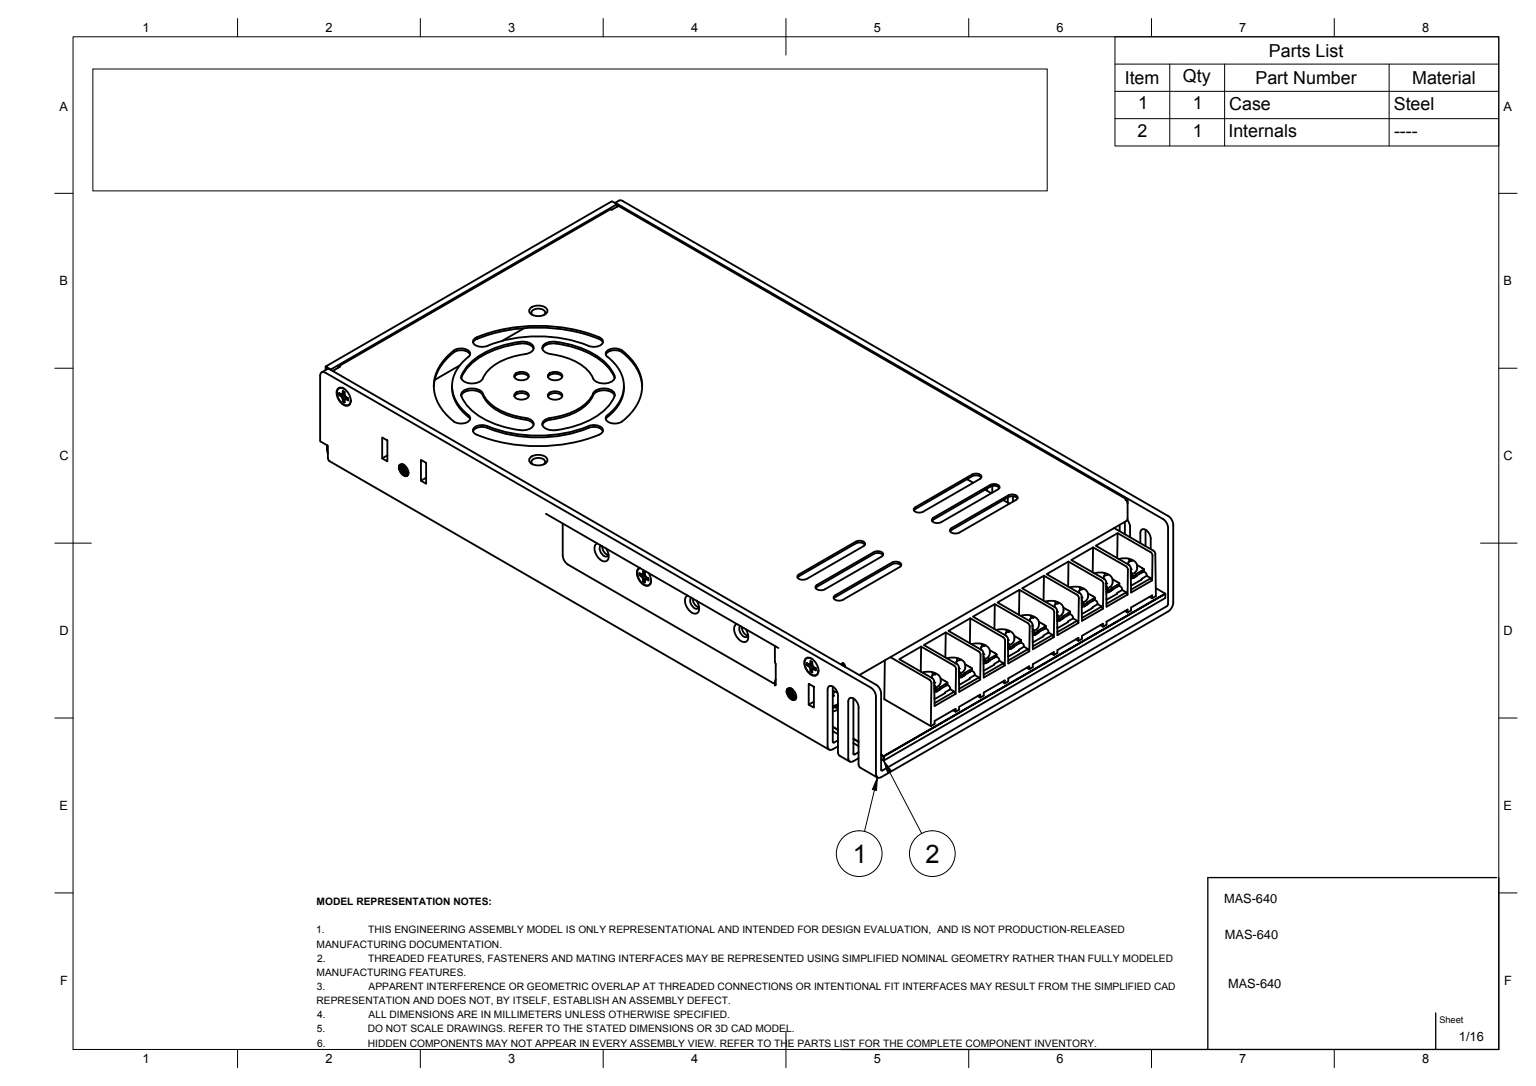
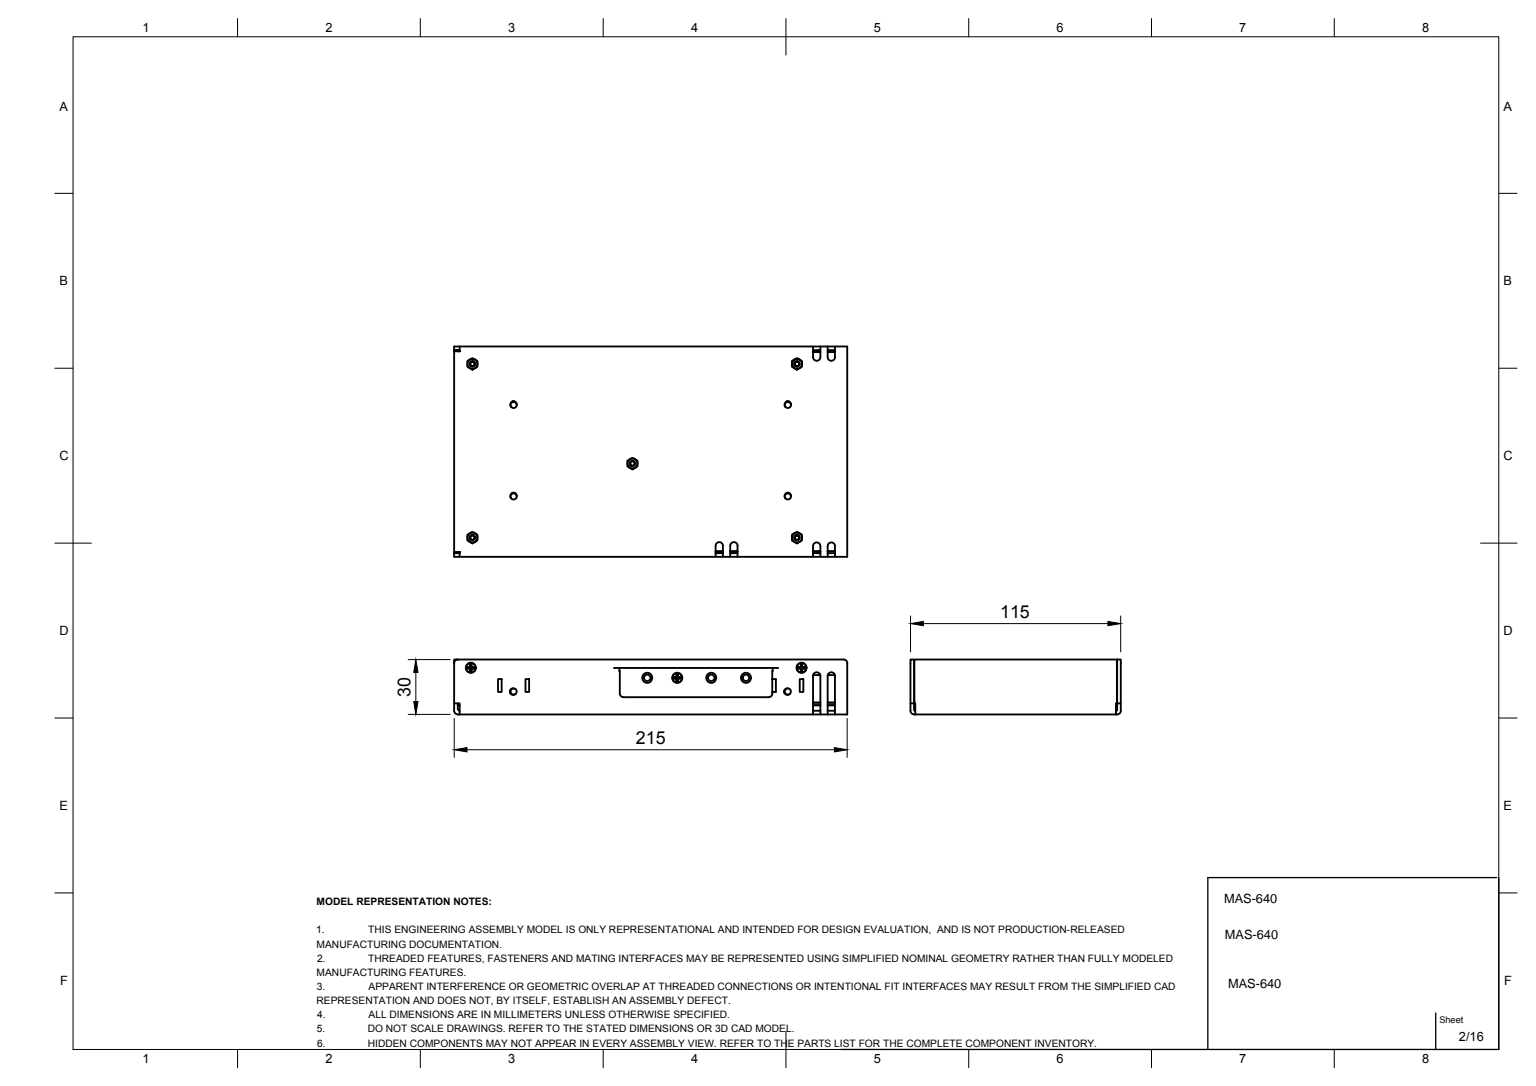
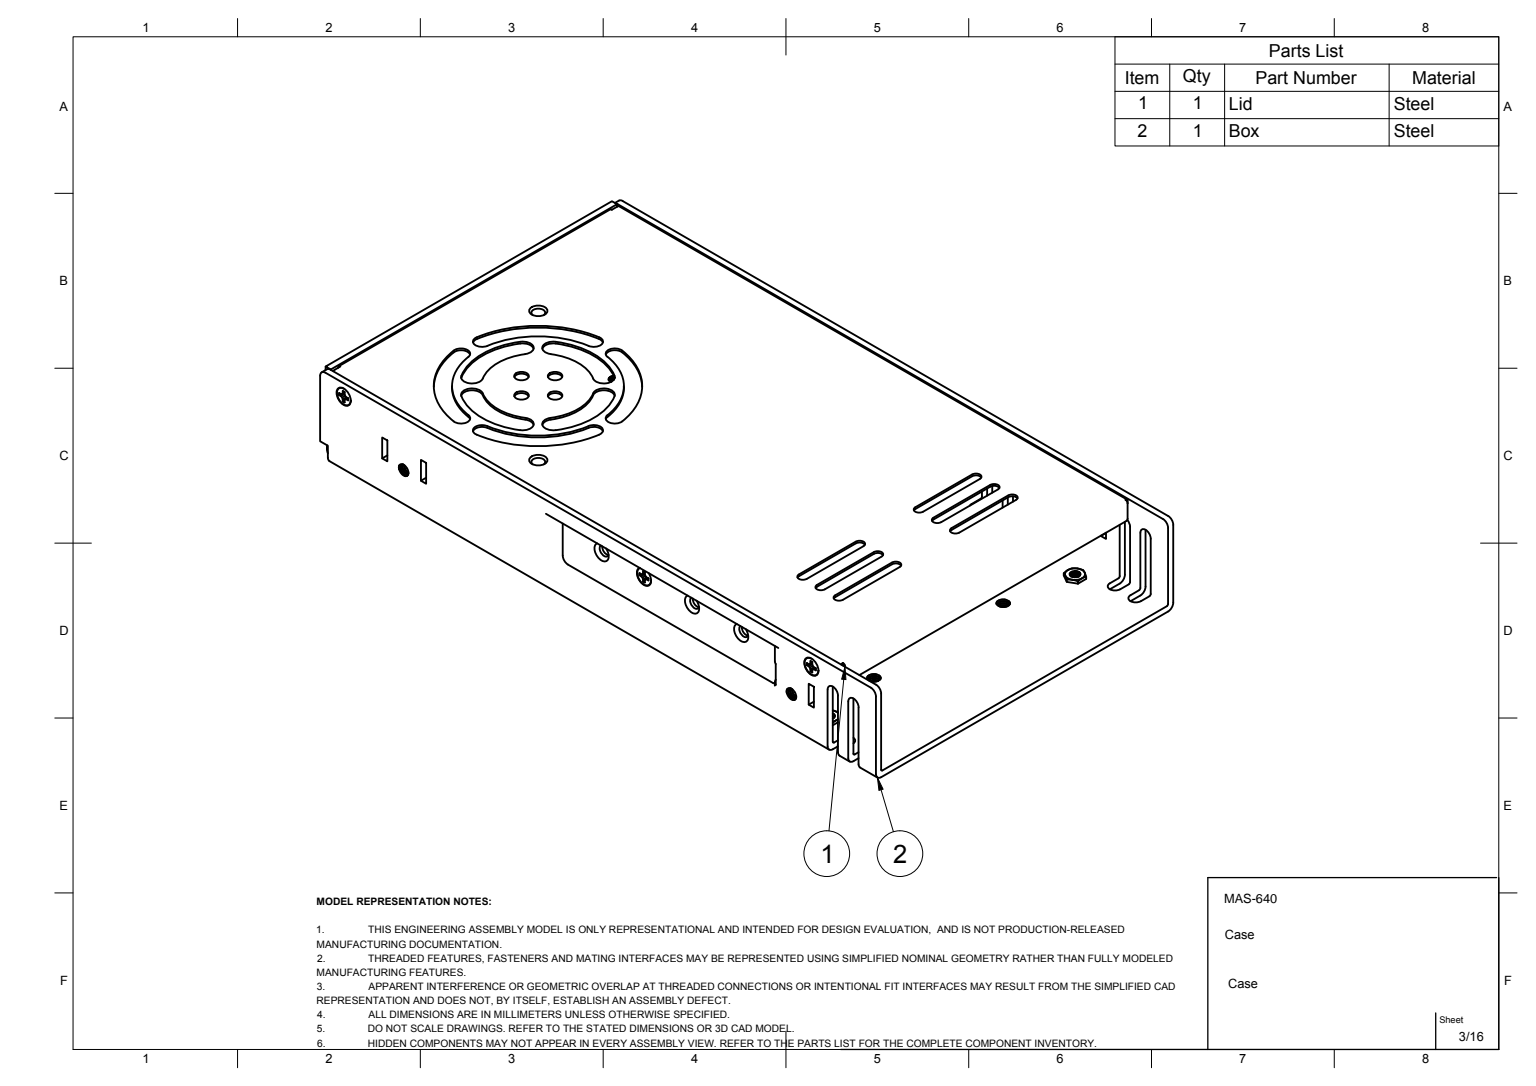
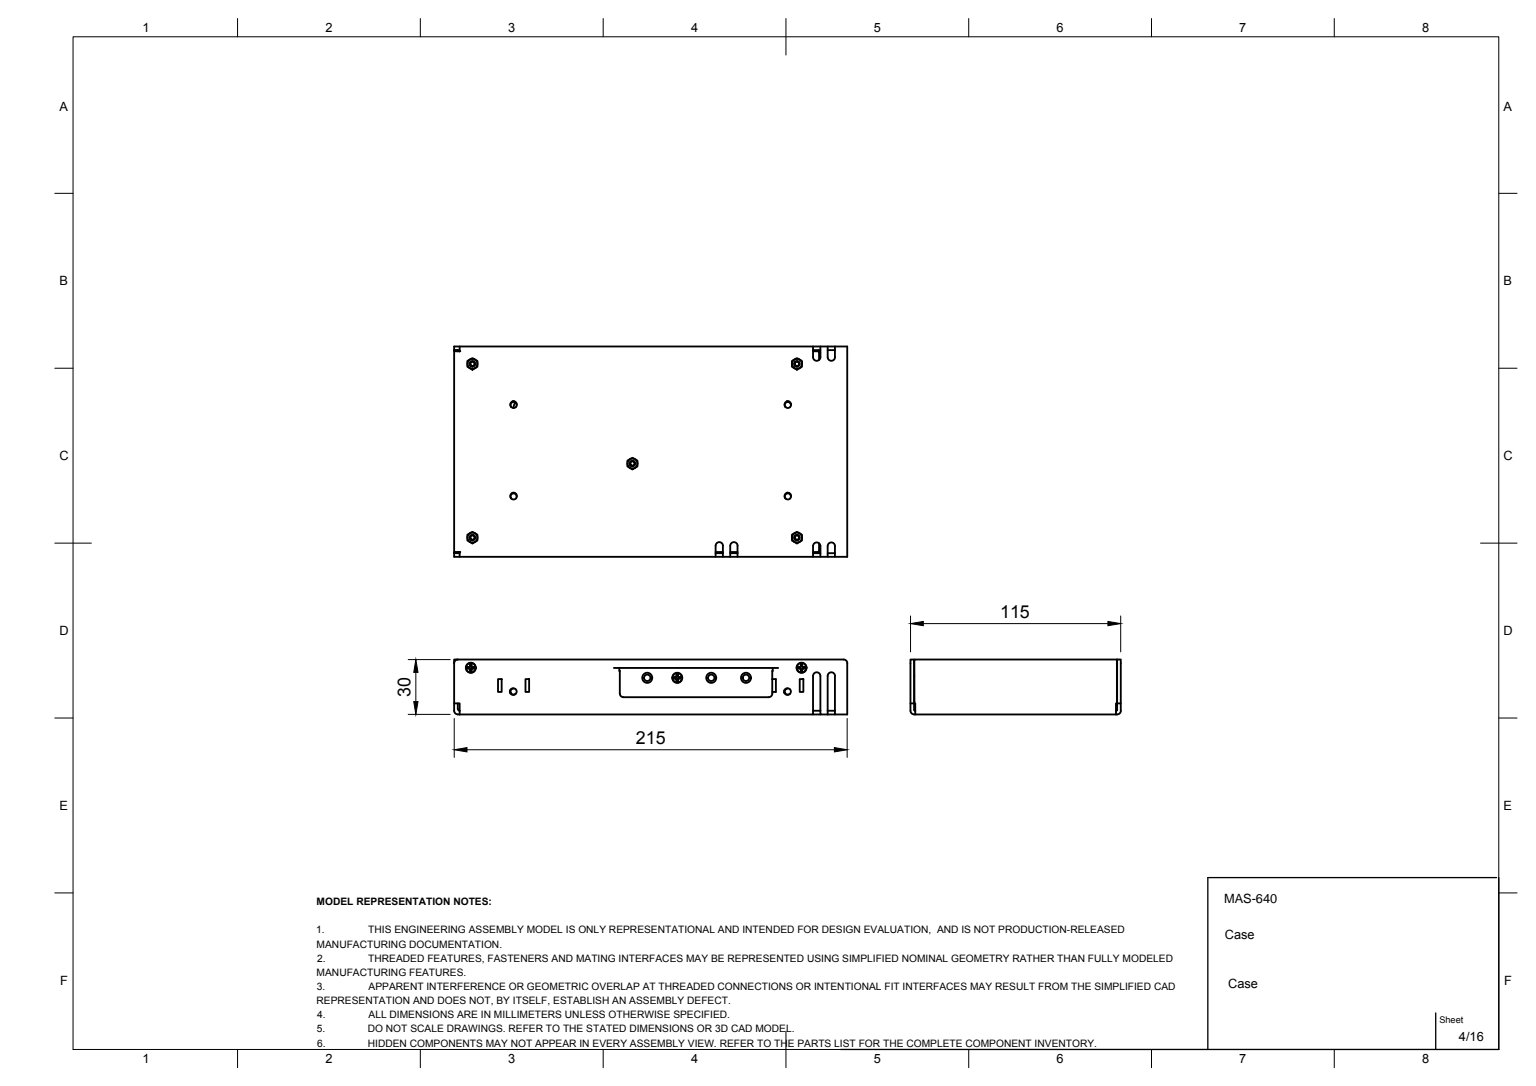
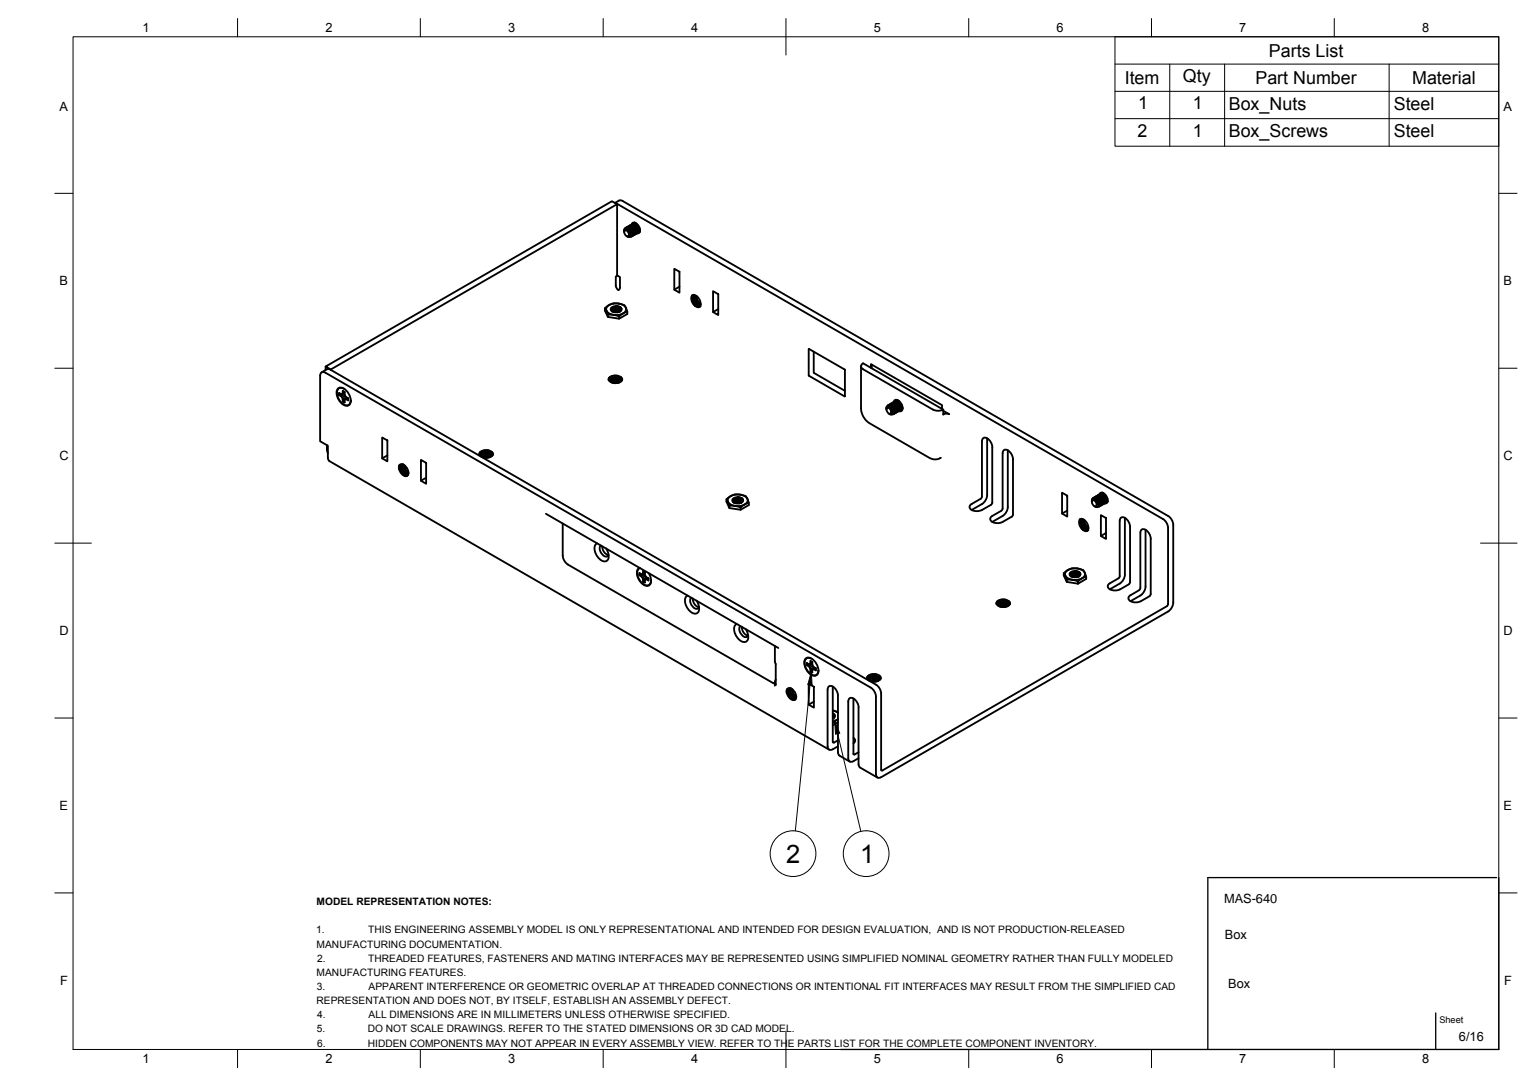
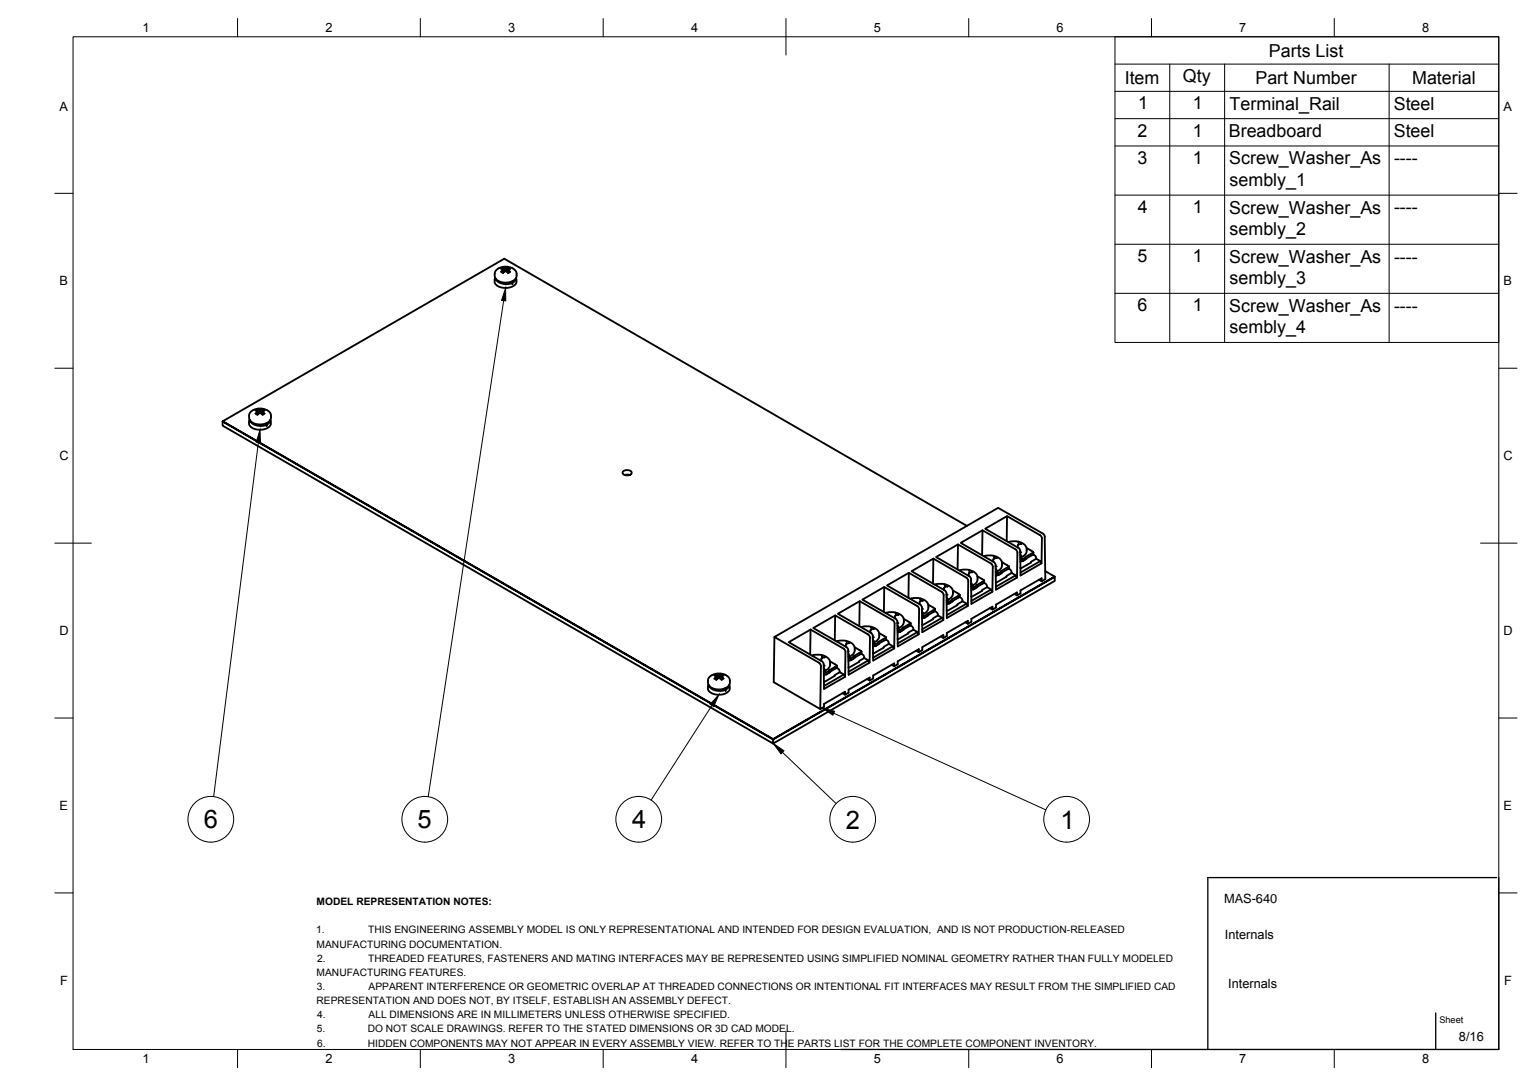
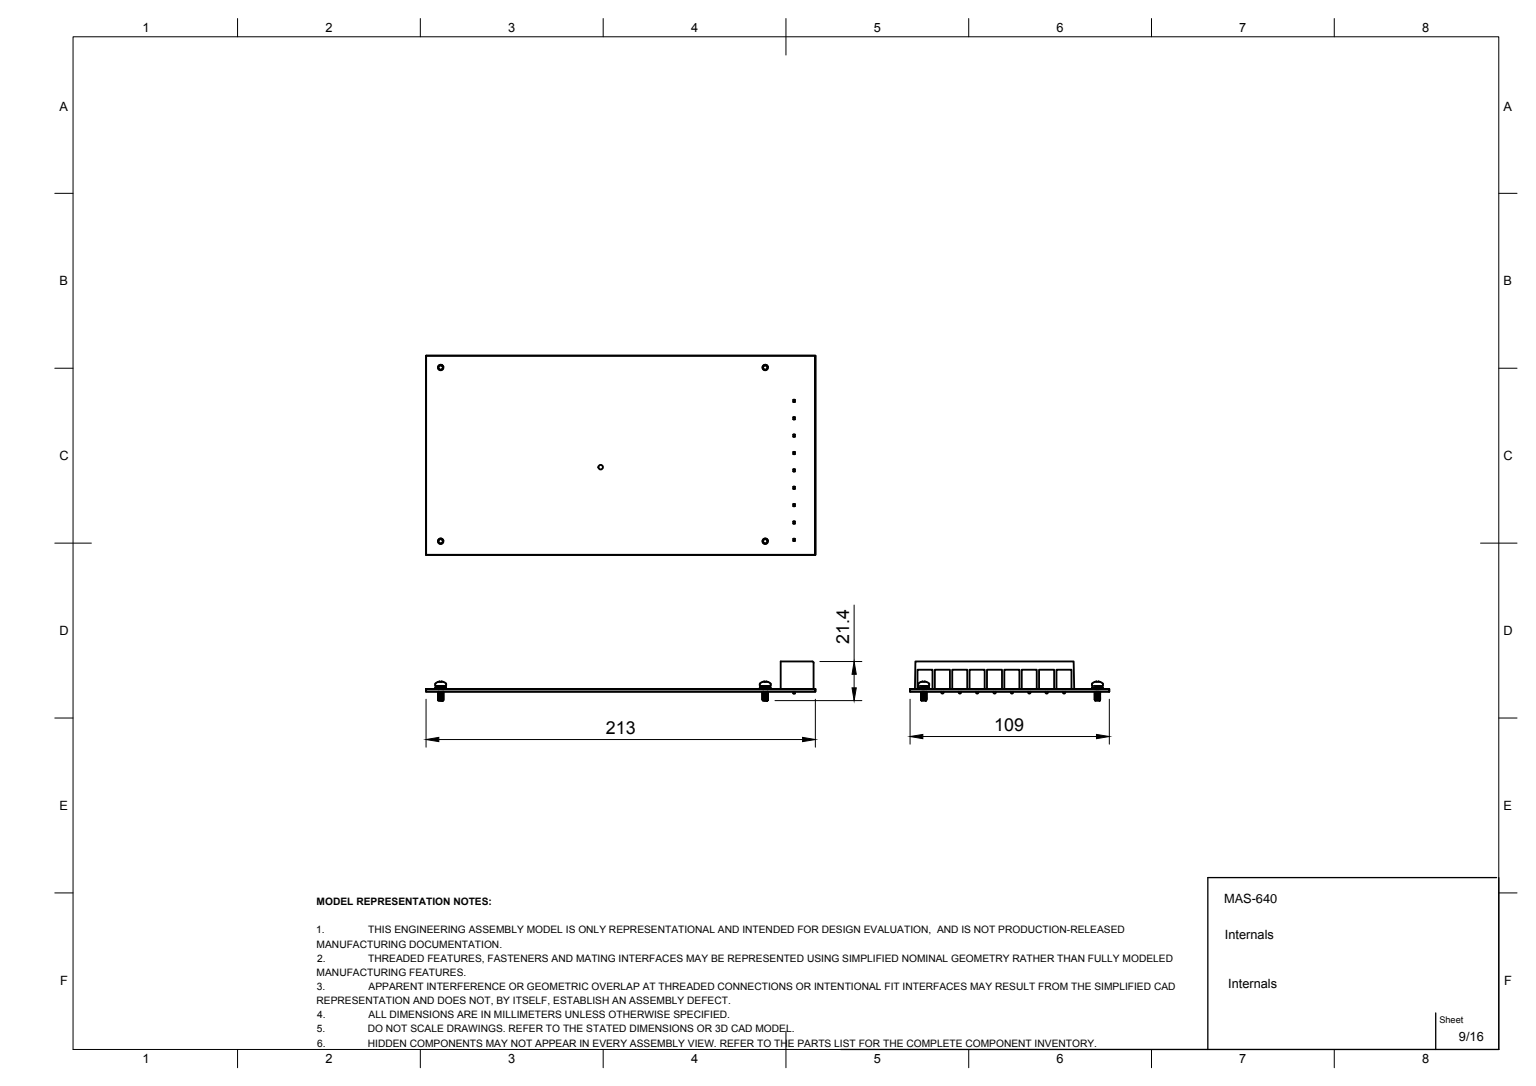
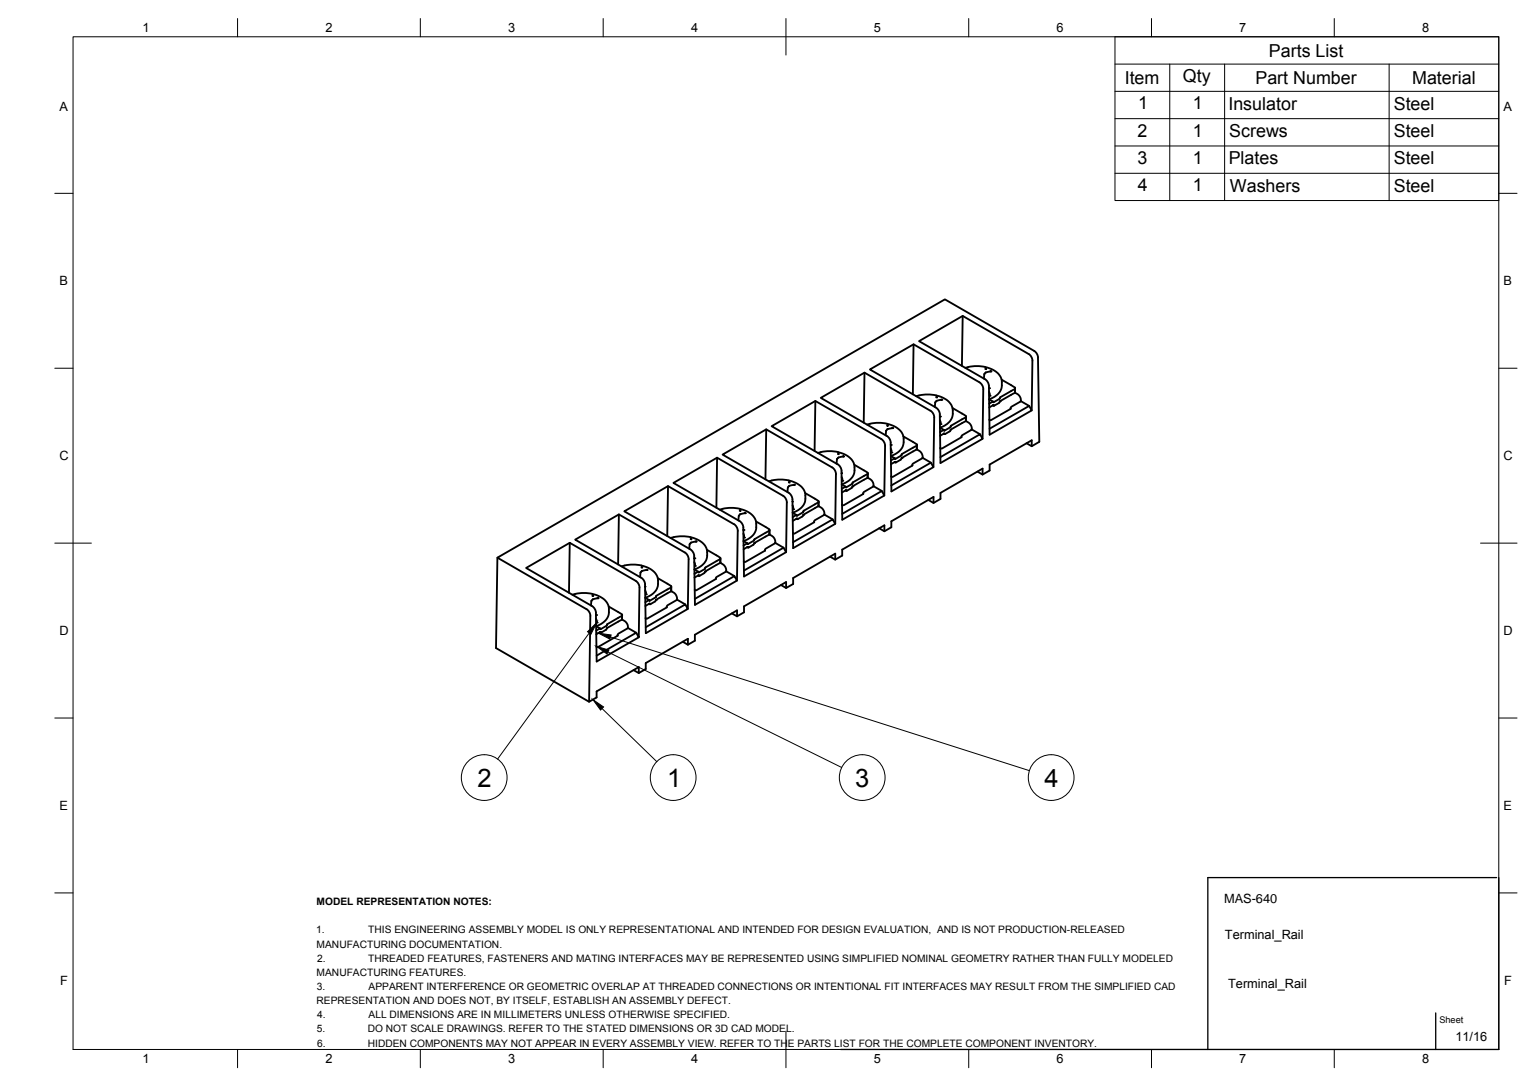
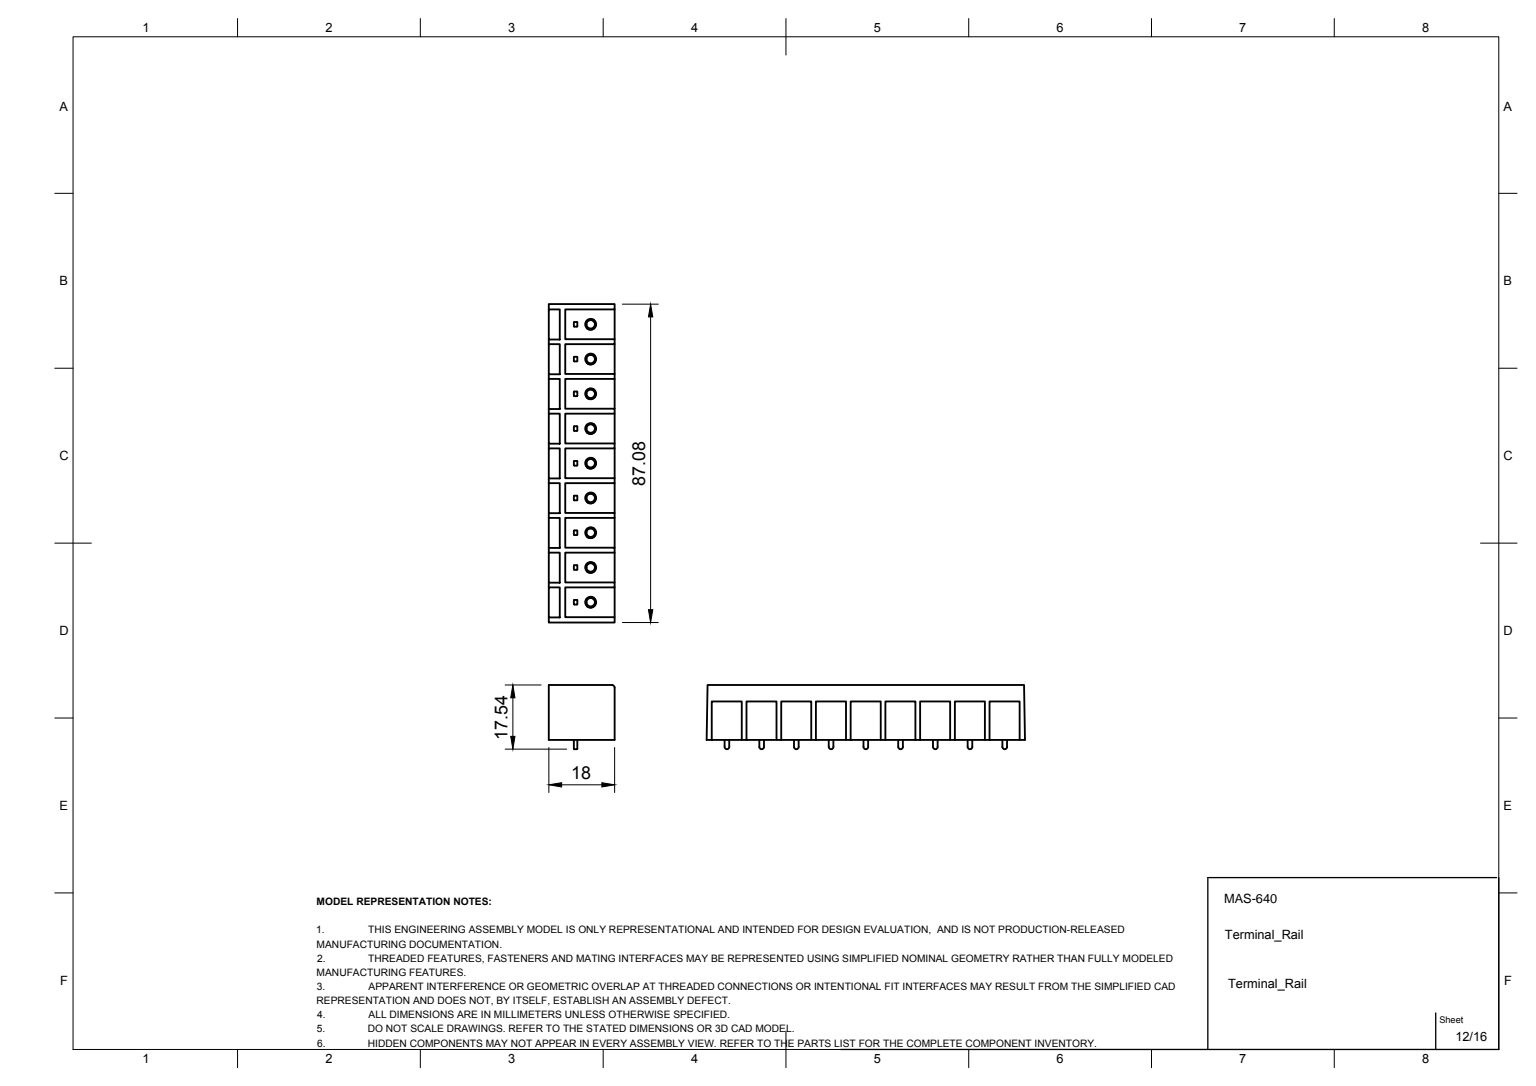
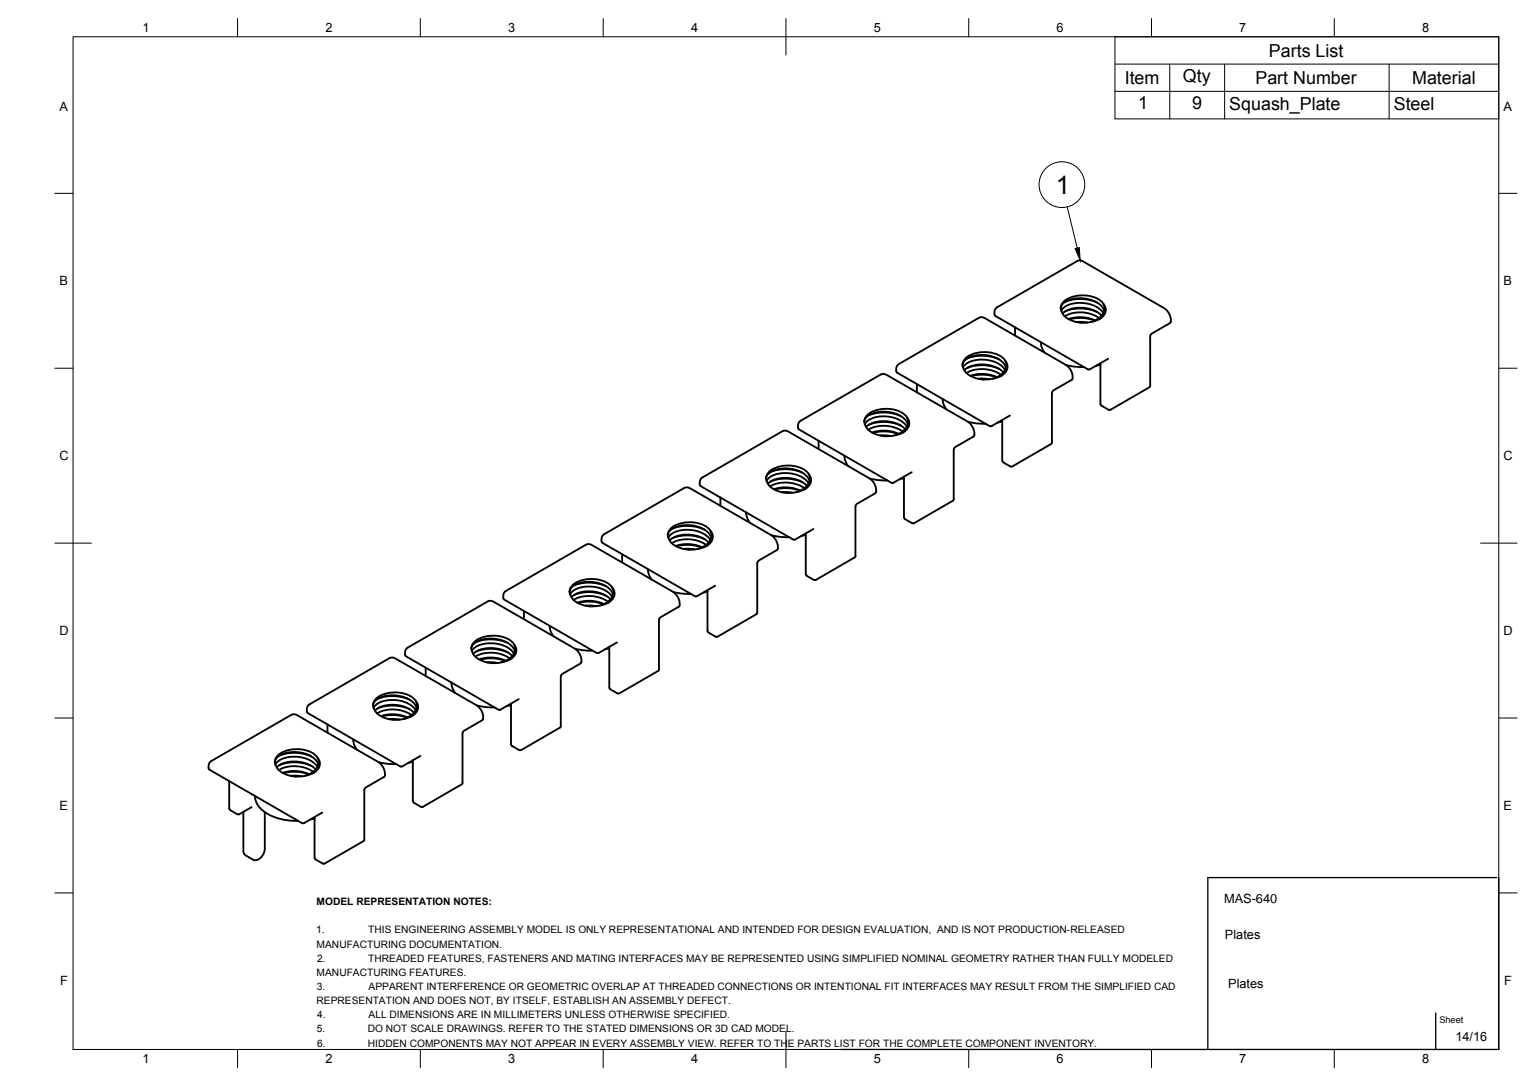
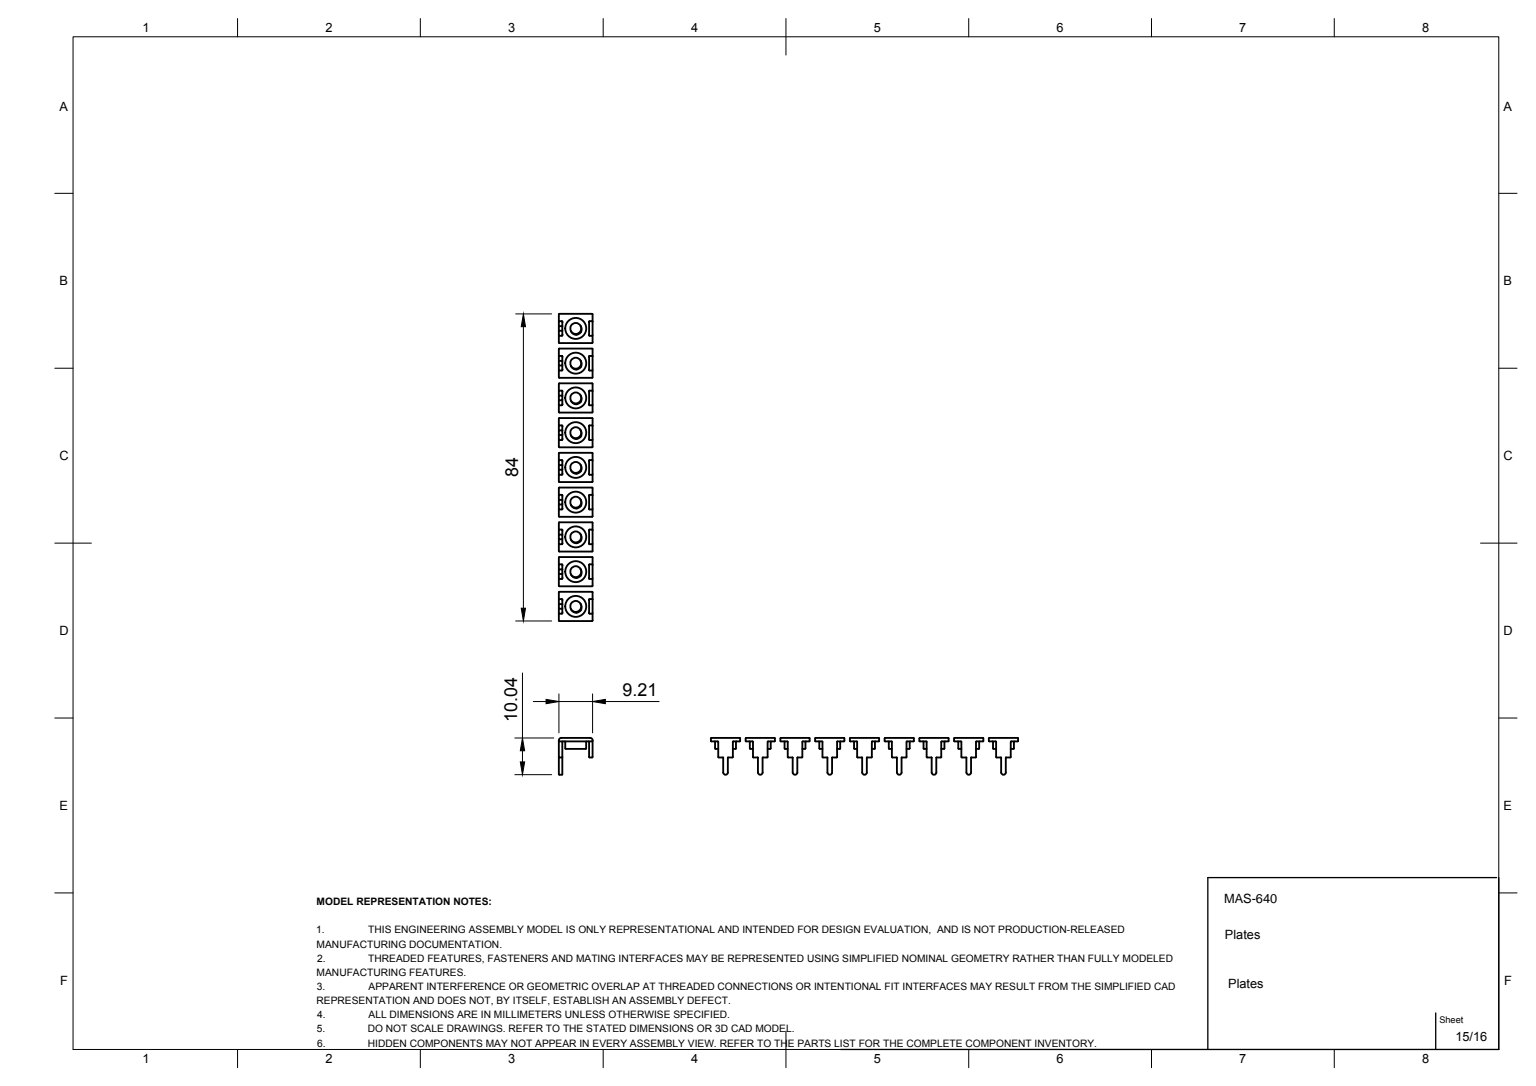
ISO-10303-21;
HEADER;
FILE_DESCRIPTION((''),'2;1');
FILE_NAME('MAS-640','2026-10-09T10:33:02-07:00',(''),(''),'','','');
FILE_SCHEMA (('AUTOMOTIVE_DESIGN { 1 0 10303 214 3 1 1 }'));
ENDSEC;
DATA;
#10 = MECHANICAL_DESIGN_GEOMETRIC_PRESENTATION_REPRESENTATION('',(#838,#839,
#840,#841,#842,#843,#844,#845,#846,#847,#848,#849),#86330) ;
#11 = SPHERICAL_SURFACE('',#34725,0.125) ;
#12 = SPHERICAL_SURFACE('',#34726,0.125) ;
#13 = SPHERICAL_SURFACE('',#34730,0.125) ;
#14 = SPHERICAL_SURFACE('',#34731,0.125) ;
#15 = SPHERICAL_SURFACE('',#34736,0.125) ;
#16 = SPHERICAL_SURFACE('',#34739,0.125) ;
#17 = SPHERICAL_SURFACE('',#34750,0.124999999999993) ;
#18 = SPHERICAL_SURFACE('',#34751,0.125000000000011) ;
#19 = SPHERICAL_SURFACE('',#34781,0.125) ;
#20 = SPHERICAL_SURFACE('',#34783,0.125) ;
#21 = SPHERICAL_SURFACE('',#34787,0.125) ;
#22 = SPHERICAL_SURFACE('',#34789,0.125) ;
#23 = SPHERICAL_SURFACE('',#34794,0.125) ;
#24 = SPHERICAL_SURFACE('',#34798,0.125) ;
#25 = SPHERICAL_SURFACE('',#34810,0.124999999999993) ;
#26 = SPHERICAL_SURFACE('',#34811,0.125000000000011) ;
#27 = SPHERICAL_SURFACE('',#34841,0.125) ;
#28 = SPHERICAL_SURFACE('',#34843,0.125) ;
#29 = SPHERICAL_SURFACE('',#34847,0.125) ;
#30 = SPHERICAL_SURFACE('',#34849,0.125) ;
#31 = SPHERICAL_SURFACE('',#34854,0.125) ;
#32 = SPHERICAL_SURFACE('',#34858,0.125) ;
#33 = SPHERICAL_SURFACE('',#34870,0.124999999999993) ;
#34 = SPHERICAL_SURFACE('',#34871,0.125000000000011) ;
#35 = SPHERICAL_SURFACE('',#34901,0.125) ;
#36 = SPHERICAL_SURFACE('',#34903,0.125) ;
#37 = SPHERICAL_SURFACE('',#34907,0.125) ;
#38 = SPHERICAL_SURFACE('',#34909,0.125) ;
#39 = SPHERICAL_SURFACE('',#34914,0.125) ;
#40 = SPHERICAL_SURFACE('',#34918,0.125) ;
#41 = SPHERICAL_SURFACE('',#34930,0.124999999999993) ;
#42 = SPHERICAL_SURFACE('',#34931,0.125000000000011) ;
#43 = SPHERICAL_SURFACE('',#34961,0.125) ;
#44 = SPHERICAL_SURFACE('',#34963,0.125) ;
#45 = SPHERICAL_SURFACE('',#34967,0.125) ;
#46 = SPHERICAL_SURFACE('',#34969,0.125) ;
#47 = SPHERICAL_SURFACE('',#34974,0.125) ;
#48 = SPHERICAL_SURFACE('',#34978,0.125) ;
#49 = SPHERICAL_SURFACE('',#34990,0.124999999999993) ;
#50 = SPHERICAL_SURFACE('',#34991,0.125000000000011) ;
#51 = SPHERICAL_SURFACE('',#35021,0.125) ;
#52 = SPHERICAL_SURFACE('',#35023,0.125) ;
#53 = SPHERICAL_SURFACE('',#35027,0.125) ;
#54 = SPHERICAL_SURFACE('',#35029,0.125) ;
#55 = SPHERICAL_SURFACE('',#35034,0.125) ;
#56 = SPHERICAL_SURFACE('',#35038,0.125) ;
#57 = SPHERICAL_SURFACE('',#35050,0.124999999999993) ;
#58 = SPHERICAL_SURFACE('',#35051,0.125000000000011) ;
#59 = SPHERICAL_SURFACE('',#35081,0.125) ;
#60 = SPHERICAL_SURFACE('',#35083,0.125) ;
#61 = SPHERICAL_SURFACE('',#35087,0.125) ;
#62 = SPHERICAL_SURFACE('',#35089,0.125) ;
#63 = SPHERICAL_SURFACE('',#35094,0.125) ;
#64 = SPHERICAL_SURFACE('',#35098,0.125) ;
#65 = SPHERICAL_SURFACE('',#35110,0.124999999999993) ;
#66 = SPHERICAL_SURFACE('',#35111,0.125000000000011) ;
#67 = SPHERICAL_SURFACE('',#35141,0.125) ;
#68 = SPHERICAL_SURFACE('',#35143,0.125) ;
#69 = SPHERICAL_SURFACE('',#35147,0.125) ;
#70 = SPHERICAL_SURFACE('',#35149,0.125) ;
#71 = SPHERICAL_SURFACE('',#35154,0.125) ;
#72 = SPHERICAL_SURFACE('',#35158,0.125) ;
#73 = SPHERICAL_SURFACE('',#35170,0.124999999999993) ;
#74 = SPHERICAL_SURFACE('',#35171,0.125000000000011) ;
#75 = SPHERICAL_SURFACE('',#35201,0.125) ;
#76 = SPHERICAL_SURFACE('',#35203,0.125) ;
#77 = SPHERICAL_SURFACE('',#35207,0.125) ;
#78 = SPHERICAL_SURFACE('',#35209,0.125) ;
#79 = SPHERICAL_SURFACE('',#35214,0.125) ;
#80 = SPHERICAL_SURFACE('',#35218,0.125) ;
#81 = SPHERICAL_SURFACE('',#35230,0.124999999999993) ;
#82 = SPHERICAL_SURFACE('',#35231,0.125000000000011) ;
#83 = SPHERICAL_SURFACE('',#35563,0.1) ;
#84 = SPHERICAL_SURFACE('',#35577,0.1) ;
#85 = SPHERICAL_SURFACE('',#35579,0.1) ;
#86 = SPHERICAL_SURFACE('',#35598,0.1) ;
#87 = SPHERICAL_SURFACE('',#35605,0.1) ;
#88 = SPHERICAL_SURFACE('',#35624,0.1) ;
#89 = SPHERICAL_SURFACE('',#35641,0.1) ;
#90 = SPHERICAL_SURFACE('',#35652,0.1) ;
#91 = SPHERICAL_SURFACE('',#35677,0.1) ;
#92 = SPHERICAL_SURFACE('',#35686,0.1) ;
#93 = SPHERICAL_SURFACE('',#35710,0.1) ;
#94 = SPHERICAL_SURFACE('',#35713,0.1) ;
#95 = SPHERICAL_SURFACE('',#35719,0.1) ;
#96 = SPHERICAL_SURFACE('',#35730,0.1) ;
#97 = SPHERICAL_SURFACE('',#35737,0.1) ;
#98 = SPHERICAL_SURFACE('',#35749,0.1) ;
#99 = SPHERICAL_SURFACE('',#35772,0.1) ;
#100 = SPHERICAL_SURFACE('',#35781,0.1) ;
#101 = SPHERICAL_SURFACE('',#35806,0.1) ;
#102 = SPHERICAL_SURFACE('',#35809,0.1) ;
#103 = SPHERICAL_SURFACE('',#35816,0.1) ;
#104 = SPHERICAL_SURFACE('',#35828,0.1) ;
#105 = SPHERICAL_SURFACE('',#35835,0.1) ;
#106 = SPHERICAL_SURFACE('',#35845,0.1) ;
#107 = SPHERICAL_SURFACE('',#35878,5.38826958762885) ;
#108 = SPHERICAL_SURFACE('',#35892,5.38826958762885) ;
#109 = SPHERICAL_SURFACE('',#35974,0.125) ;
#110 = SPHERICAL_SURFACE('',#35976,0.125) ;
#111 = SPHERICAL_SURFACE('',#35981,0.125) ;
#112 = SPHERICAL_SURFACE('',#35983,0.125) ;
#113 = SPHERICAL_SURFACE('',#36041,0.125) ;
#114 = SPHERICAL_SURFACE('',#36047,0.125) ;
#115 = SPHERICAL_SURFACE('',#36104,0.124999999999993) ;
#116 = SPHERICAL_SURFACE('',#36105,0.125000000000011) ;
#117 = SPHERICAL_SURFACE('',#36116,0.124999999999993) ;
#118 = SPHERICAL_SURFACE('',#36117,0.124999999999993) ;
#119 = SPHERICAL_SURFACE('',#36118,0.124999999999993) ;
#120 = SPHERICAL_SURFACE('',#36119,0.124999999999993) ;
#121 = SPHERICAL_SURFACE('',#36434,4.225) ;
#122 = ELLIPSE('',#33166,20.5459783090209,1.7907) ;
#123 = ELLIPSE('',#33167,20.545978309021,1.7907) ;
#124 = ELLIPSE('',#33169,20.545978309021,1.7907) ;
#125 = ELLIPSE('',#33170,20.5459783090209,1.7907) ;
#126 = ELLIPSE('',#33172,20.545978309021,1.7907) ;
#127 = ELLIPSE('',#33173,20.545978309021,1.7907) ;
#128 = ELLIPSE('',#33185,20.545978309021,1.7907) ;
#129 = ELLIPSE('',#33187,20.545978309021,1.7907) ;
#130 = ELLIPSE('',#35261,0.75011424965518,0.750000004857936) ;
#131 = ELLIPSE('',#35262,0.750114249654022,0.750000004857117) ;
#132 = ELLIPSE('',#35265,0.750114249653564,0.750000004856577) ;
#133 = ELLIPSE('',#35266,0.75011424965434,0.750000004857177) ;
#134 = ELLIPSE('',#35268,0.750114249655181,0.750000004857937) ;
#135 = ELLIPSE('',#35269,0.750114249654116,0.750000004857023) ;
#136 = ELLIPSE('',#35271,0.75011424965372,0.750000004856674) ;
#137 = ELLIPSE('',#35272,0.75011424965532,0.750000004858217) ;
#138 = ELLIPSE('',#35274,0.750114249654022,0.750000004857117) ;
#139 = ELLIPSE('',#35275,0.750114249656223,0.750000004858968) ;
#140 = ELLIPSE('',#35277,0.750114249654019,0.750000004856718) ;
#141 = ELLIPSE('',#35278,0.750114249655222,0.750000004857992) ;
#142 = ELLIPSE('',#35280,0.750114249654021,0.750000004856918) ;
#143 = ELLIPSE('',#35281,0.750114249656024,0.750000004858698) ;
#144 = ELLIPSE('',#35283,0.750114249655273,0.75000000485804) ;
#145 = ELLIPSE('',#35284,0.750114249653565,0.75000000485638) ;
#146 = ELLIPSE('',#35286,0.750114249654481,0.750000004857962) ;
#147 = ELLIPSE('',#35287,0.750114249650677,0.750000004854032) ;
#148 = ELLIPSE('',#35289,0.750114249654021,0.750000004856918) ;
#149 = ELLIPSE('',#35291,0.750114249654338,0.750000004857176) ;
#150 = ELLIPSE('',#35501,0.0961348525953907,0.0789674582653757) ;
#151 = ELLIPSE('',#35502,0.181135134462203,0.157351167100413) ;
#152 = ELLIPSE('',#35506,0.179452491476591,0.152051329111869) ;
#153 = ELLIPSE('',#35509,0.17945249124005,0.152051328979059) ;
#154 = ELLIPSE('',#35511,0.173242568385421,0.148461954688806) ;
#155 = ELLIPSE('',#35514,0.173242568255686,0.148461954613973) ;
#156 = ELLIPSE('',#35520,0.0961348009085155,0.0789673736338199) ;
#157 = ELLIPSE('',#35526,0.18113516065876,0.157351212612531) ;
#158 = ELLIPSE('',#35537,0.0961347917913063,0.0789673586439759) ;
#159 = ELLIPSE('',#35538,0.181135145593687,0.157351186447307) ;
#160 = ELLIPSE('',#35544,0.0961348054140246,0.0789673810185351) ;
#161 = ELLIPSE('',#35550,0.18113516065876,0.157351212612531) ;
#162 = ELLIPSE('',#35557,0.301518169878764,0.257262372521227) ;
#163 = ELLIPSE('',#35559,0.107622698330153,0.1) ;
#164 = ELLIPSE('',#35560,0.107622698330153,0.1) ;
#165 = ELLIPSE('',#35570,0.170365066914478,0.147415894551294) ;
#166 = ELLIPSE('',#35575,0.0854022854049574,0.0779713270951896) ;
#167 = ELLIPSE('',#35585,0.085402285745328,0.0779713277049084) ;
#168 = ELLIPSE('',#35586,0.170365066783361,0.147415894323676) ;
#169 = ELLIPSE('',#35593,0.107622698330153,0.1) ;
#170 = ELLIPSE('',#35595,0.107622698330153,0.1) ;
#171 = ELLIPSE('',#35601,0.217305352531138,0.2) ;
#172 = ELLIPSE('',#35604,0.129857287089145,0.1) ;
#173 = ELLIPSE('',#35610,0.0854022855711418,0.0779713273931643) ;
#174 = ELLIPSE('',#35612,0.170365066781204,0.147415894320068) ;
#175 = ELLIPSE('',#35615,0.0854022856622134,0.0779713275582352) ;
#176 = ELLIPSE('',#35623,0.107622698330153,0.1) ;
#177 = ELLIPSE('',#35629,0.17036506667425,0.147415894132821) ;
#178 = ELLIPSE('',#35636,0.107622698330153,0.1) ;
#179 = ELLIPSE('',#35638,0.107622698330153,0.1) ;
#180 = ELLIPSE('',#35644,0.217305352531139,0.2) ;
#181 = ELLIPSE('',#35647,0.129857287089145,0.1) ;
#182 = ELLIPSE('',#35649,0.107622698330153,0.1) ;
#183 = ELLIPSE('',#35658,0.129857287089145,0.1) ;
#184 = ELLIPSE('',#35659,1.80295526461806,1.74359985651392) ;
#185 = ELLIPSE('',#35663,1.44368220806618,1.24694668207658) ;
#186 = ELLIPSE('',#35667,0.325215841526545,0.1384674618534) ;
#187 = ELLIPSE('',#35668,0.179960384676197,0.0842561394706778) ;
#188 = ELLIPSE('',#35669,0.143757456365121,0.0572377473682424) ;
#189 = ELLIPSE('',#35670,0.178426613998649,0.0895872224985392) ;
#190 = ELLIPSE('',#35671,0.180280902012032,0.0868949646061415) ;
#191 = ELLIPSE('',#35672,0.318318659412206,0.139006967439323) ;
#192 = ELLIPSE('',#35674,0.181500403086132,0.1649478028119) ;
#193 = ELLIPSE('',#35675,0.0992598259423044,0.0779564848832496) ;
#194 = ELLIPSE('',#35691,0.0992598257926529,0.0779564846898224) ;
#195 = ELLIPSE('',#35693,0.181500403012281,0.164947802681056) ;
#196 = ELLIPSE('',#35698,0.107622698330153,0.1) ;
#197 = ELLIPSE('',#35701,0.129857287089145,0.1) ;
#198 = ELLIPSE('',#35705,0.21730535253114,0.2) ;
#199 = ELLIPSE('',#35707,0.13123115574696,0.0999999999999999) ;
#200 = ELLIPSE('',#35716,0.107622698330153,0.1) ;
#201 = ELLIPSE('',#35727,0.131231155746957,0.1) ;
#202 = ELLIPSE('',#35736,0.129857287089145,0.1) ;
#203 = ELLIPSE('',#35746,0.301519549160911,0.257265094389927) ;
#204 = ELLIPSE('',#35755,0.107622698330153,0.1) ;
#205 = ELLIPSE('',#35756,0.107622698330153,0.1) ;
#206 = ELLIPSE('',#35760,0.131231155746959,0.1) ;
#207 = ELLIPSE('',#35762,0.325215841518844,0.138467461839436) ;
#208 = ELLIPSE('',#35763,0.179960384640109,0.084256139441645) ;
#209 = ELLIPSE('',#35764,0.143757456333512,0.0572377473425655) ;
#210 = ELLIPSE('',#35765,0.178426614167312,0.0895872226348807) ;
#211 = ELLIPSE('',#35766,0.180280902020227,0.086894964614583) ;
#212 = ELLIPSE('',#35767,0.318318659448403,0.139006967461565) ;
#213 = ELLIPSE('',#35769,0.181500403028042,0.164947802708139) ;
#214 = ELLIPSE('',#35770,0.0992598259984378,0.0779564849579177) ;
#215 = ELLIPSE('',#35786,0.0992598258762505,0.0779564847990513) ;
#216 = ELLIPSE('',#35788,0.181500403117952,0.164947802867497) ;
#217 = ELLIPSE('',#35793,0.107622698330153,0.1) ;
#218 = ELLIPSE('',#35798,0.129857287089145,0.1) ;
#219 = ELLIPSE('',#35799,0.129857287089145,0.1) ;
#220 = ELLIPSE('',#35801,0.217305352531139,0.2) ;
#221 = ELLIPSE('',#35803,0.131231155746959,0.1) ;
#222 = ELLIPSE('',#35813,0.107622698330153,0.1) ;
#223 = ELLIPSE('',#35834,0.129857287089145,0.1) ;
#224 = ELLIPSE('',#35851,0.107622698330153,0.1) ;
#225 = ELLIPSE('',#35852,0.107622698330153,0.1) ;
#226 = TOROIDAL_SURFACE('',#33146,2.55525626680218,0.0625) ;
#227 = TOROIDAL_SURFACE('',#33403,5.,1.) ;
#228 = TOROIDAL_SURFACE('',#33408,5.,1.) ;
#229 = TOROIDAL_SURFACE('',#33423,5.,1.) ;
#230 = TOROIDAL_SURFACE('',#33428,5.,1.) ;
#231 = TOROIDAL_SURFACE('',#33506,5.25,3.25) ;
#232 = TOROIDAL_SURFACE('',#33549,5.25,3.25) ;
#233 = TOROIDAL_SURFACE('',#33614,5.25,3.25) ;
#234 = TOROIDAL_SURFACE('',#33619,5.25,3.25) ;
#235 = TOROIDAL_SURFACE('',#33657,0.250000000000004,0.124999999999957) ;
#236 = TOROIDAL_SURFACE('',#33661,0.250000000000004,0.125000000000002) ;
#237 = TOROIDAL_SURFACE('',#33662,0.250000000000004,0.125000000000002) ;
#238 = TOROIDAL_SURFACE('',#33663,0.250000000000004,0.125000000000011) ;
#239 = TOROIDAL_SURFACE('',#33756,1.625,0.125) ;
#240 = TOROIDAL_SURFACE('',#33767,1.625,0.125) ;
#241 = TOROIDAL_SURFACE('',#33778,1.625,0.125) ;
#242 = TOROIDAL_SURFACE('',#33789,1.625,0.125) ;
#243 = TOROIDAL_SURFACE('',#33800,1.625,0.125) ;
#244 = TOROIDAL_SURFACE('',#33811,1.625,0.125) ;
#245 = TOROIDAL_SURFACE('',#33822,1.625,0.125) ;
#246 = TOROIDAL_SURFACE('',#33833,1.625,0.125) ;
#247 = TOROIDAL_SURFACE('',#33844,1.625,0.125) ;
#248 = TOROIDAL_SURFACE('',#33874,0.375,0.25) ;
#249 = TOROIDAL_SURFACE('',#33879,0.375,0.25) ;
#250 = TOROIDAL_SURFACE('',#33884,0.375,0.25) ;
#251 = TOROIDAL_SURFACE('',#33889,0.375,0.25) ;
#252 = TOROIDAL_SURFACE('',#33902,0.375,0.25) ;
#253 = TOROIDAL_SURFACE('',#33907,0.375,0.25) ;
#254 = TOROIDAL_SURFACE('',#33912,0.375,0.25) ;
#255 = TOROIDAL_SURFACE('',#33917,0.375,0.25) ;
#256 = TOROIDAL_SURFACE('',#33930,0.375,0.25) ;
#257 = TOROIDAL_SURFACE('',#33935,0.375,0.25) ;
#258 = TOROIDAL_SURFACE('',#33940,0.375,0.25) ;
#259 = TOROIDAL_SURFACE('',#33945,0.375,0.25) ;
#260 = TOROIDAL_SURFACE('',#33958,0.375,0.25) ;
#261 = TOROIDAL_SURFACE('',#33963,0.375,0.25) ;
#262 = TOROIDAL_SURFACE('',#33968,0.375,0.25) ;
#263 = TOROIDAL_SURFACE('',#33973,0.375,0.25) ;
#264 = TOROIDAL_SURFACE('',#33986,0.375,0.25) ;
#265 = TOROIDAL_SURFACE('',#33991,0.375,0.25) ;
#266 = TOROIDAL_SURFACE('',#33996,0.375,0.25) ;
#267 = TOROIDAL_SURFACE('',#34001,0.375,0.25) ;
#268 = TOROIDAL_SURFACE('',#34014,0.375,0.25) ;
#269 = TOROIDAL_SURFACE('',#34019,0.375,0.25) ;
#270 = TOROIDAL_SURFACE('',#34024,0.375,0.25) ;
#271 = TOROIDAL_SURFACE('',#34029,0.375,0.25) ;
#272 = TOROIDAL_SURFACE('',#34042,0.375,0.25) ;
#273 = TOROIDAL_SURFACE('',#34047,0.375,0.25) ;
#274 = TOROIDAL_SURFACE('',#34052,0.375,0.25) ;
#275 = TOROIDAL_SURFACE('',#34057,0.375,0.25) ;
#276 = TOROIDAL_SURFACE('',#34070,0.375,0.25) ;
#277 = TOROIDAL_SURFACE('',#34075,0.375,0.25) ;
#278 = TOROIDAL_SURFACE('',#34080,0.375,0.25) ;
#279 = TOROIDAL_SURFACE('',#34085,0.375,0.25) ;
#280 = TOROIDAL_SURFACE('',#34098,0.375,0.25) ;
#281 = TOROIDAL_SURFACE('',#34103,0.375,0.25) ;
#282 = TOROIDAL_SURFACE('',#34108,0.375,0.25) ;
#283 = TOROIDAL_SURFACE('',#34113,0.375,0.25) ;
#284 = TOROIDAL_SURFACE('',#34126,0.375,0.25) ;
#285 = TOROIDAL_SURFACE('',#34132,0.375,0.25) ;
#286 = TOROIDAL_SURFACE('',#34138,0.375,0.25) ;
#287 = TOROIDAL_SURFACE('',#34144,0.375,0.25) ;
#288 = TOROIDAL_SURFACE('',#34156,0.375,0.25) ;
#289 = TOROIDAL_SURFACE('',#34162,0.375,0.25) ;
#290 = TOROIDAL_SURFACE('',#34168,0.375,0.25) ;
#291 = TOROIDAL_SURFACE('',#34174,0.375,0.25) ;
#292 = TOROIDAL_SURFACE('',#34186,0.375,0.25) ;
#293 = TOROIDAL_SURFACE('',#34192,0.375,0.25) ;
#294 = TOROIDAL_SURFACE('',#34198,0.375,0.25) ;
#295 = TOROIDAL_SURFACE('',#34204,0.375,0.25) ;
#296 = TOROIDAL_SURFACE('',#34216,0.375,0.25) ;
#297 = TOROIDAL_SURFACE('',#34222,0.375,0.25) ;
#298 = TOROIDAL_SURFACE('',#34228,0.375,0.25) ;
#299 = TOROIDAL_SURFACE('',#34234,0.375,0.25) ;
#300 = TOROIDAL_SURFACE('',#34246,0.375,0.25) ;
#301 = TOROIDAL_SURFACE('',#34252,0.375,0.25) ;
#302 = TOROIDAL_SURFACE('',#34258,0.375,0.25) ;
#303 = TOROIDAL_SURFACE('',#34264,0.375,0.25) ;
#304 = TOROIDAL_SURFACE('',#34276,0.375,0.25) ;
#305 = TOROIDAL_SURFACE('',#34282,0.375,0.25) ;
#306 = TOROIDAL_SURFACE('',#34288,0.375,0.25) ;
#307 = TOROIDAL_SURFACE('',#34294,0.375,0.25) ;
#308 = TOROIDAL_SURFACE('',#34306,0.375,0.25) ;
#309 = TOROIDAL_SURFACE('',#34312,0.375,0.25) ;
#310 = TOROIDAL_SURFACE('',#34318,0.375,0.25) ;
#311 = TOROIDAL_SURFACE('',#34324,0.375,0.25) ;
#312 = TOROIDAL_SURFACE('',#34336,0.375,0.25) ;
#313 = TOROIDAL_SURFACE('',#34342,0.375,0.25) ;
#314 = TOROIDAL_SURFACE('',#34348,0.375,0.25) ;
#315 = TOROIDAL_SURFACE('',#34354,0.375,0.25) ;
#316 = TOROIDAL_SURFACE('',#34366,0.375,0.25) ;
#317 = TOROIDAL_SURFACE('',#34372,0.375,0.25) ;
#318 = TOROIDAL_SURFACE('',#34378,0.375,0.25) ;
#319 = TOROIDAL_SURFACE('',#34384,0.375,0.25) ;
#320 = TOROIDAL_SURFACE('',#34398,0.375,0.25) ;
#321 = TOROIDAL_SURFACE('',#34404,0.375,0.25) ;
#322 = TOROIDAL_SURFACE('',#34410,0.375,0.25) ;
#323 = TOROIDAL_SURFACE('',#34416,0.375,0.25) ;
#324 = TOROIDAL_SURFACE('',#34430,0.375,0.25) ;
#325 = TOROIDAL_SURFACE('',#34436,0.375,0.25) ;
#326 = TOROIDAL_SURFACE('',#34442,0.375,0.25) ;
#327 = TOROIDAL_SURFACE('',#34448,0.375,0.25) ;
#328 = TOROIDAL_SURFACE('',#34462,0.375,0.25) ;
#329 = TOROIDAL_SURFACE('',#34468,0.375,0.25) ;
#330 = TOROIDAL_SURFACE('',#34474,0.375,0.25) ;
#331 = TOROIDAL_SURFACE('',#34480,0.375,0.25) ;
#332 = TOROIDAL_SURFACE('',#34494,0.375,0.25) ;
#333 = TOROIDAL_SURFACE('',#34500,0.375,0.25) ;
#334 = TOROIDAL_SURFACE('',#34506,0.375,0.25) ;
#335 = TOROIDAL_SURFACE('',#34512,0.375,0.25) ;
#336 = TOROIDAL_SURFACE('',#34526,0.375,0.25) ;
#337 = TOROIDAL_SURFACE('',#34532,0.375,0.25) ;
#338 = TOROIDAL_SURFACE('',#34538,0.375,0.25) ;
#339 = TOROIDAL_SURFACE('',#34544,0.375,0.25) ;
#340 = TOROIDAL_SURFACE('',#34558,0.375,0.25) ;
#341 = TOROIDAL_SURFACE('',#34564,0.375,0.25) ;
#342 = TOROIDAL_SURFACE('',#34570,0.375,0.25) ;
#343 = TOROIDAL_SURFACE('',#34576,0.375,0.25) ;
#344 = TOROIDAL_SURFACE('',#34590,0.375,0.25) ;
#345 = TOROIDAL_SURFACE('',#34596,0.375,0.25) ;
#346 = TOROIDAL_SURFACE('',#34602,0.375,0.25) ;
#347 = TOROIDAL_SURFACE('',#34608,0.375,0.25) ;
#348 = TOROIDAL_SURFACE('',#34622,0.375,0.25) ;
#349 = TOROIDAL_SURFACE('',#34628,0.375,0.25) ;
#350 = TOROIDAL_SURFACE('',#34634,0.375,0.25) ;
#351 = TOROIDAL_SURFACE('',#34640,0.375,0.25) ;
#352 = TOROIDAL_SURFACE('',#34658,0.375,0.25) ;
#353 = TOROIDAL_SURFACE('',#34663,0.375,0.25) ;
#354 = TOROIDAL_SURFACE('',#34668,0.375,0.25) ;
#355 = TOROIDAL_SURFACE('',#34673,0.375,0.25) ;
#356 = TOROIDAL_SURFACE('',#34701,0.188499999999969,0.124999999999993) ;
#357 = TOROIDAL_SURFACE('',#34706,0.188499999999987,0.124999999999993) ;
#358 = TOROIDAL_SURFACE('',#34709,0.188499999999987,0.124999999999993) ;
#359 = TOROIDAL_SURFACE('',#34716,0.188499999999987,0.124999999999993) ;
#360 = TOROIDAL_SURFACE('',#34757,0.188499999999969,0.124999999999993) ;
#361 = TOROIDAL_SURFACE('',#34762,0.188499999999987,0.124999999999993) ;
#362 = TOROIDAL_SURFACE('',#34765,0.188499999999987,0.124999999999993) ;
#363 = TOROIDAL_SURFACE('',#34772,0.188499999999987,0.124999999999993) ;
#364 = TOROIDAL_SURFACE('',#34817,0.188499999999969,0.124999999999993) ;
#365 = TOROIDAL_SURFACE('',#34822,0.188499999999987,0.124999999999993) ;
#366 = TOROIDAL_SURFACE('',#34825,0.188499999999987,0.124999999999993) ;
#367 = TOROIDAL_SURFACE('',#34832,0.188499999999987,0.124999999999993) ;
#368 = TOROIDAL_SURFACE('',#34877,0.188499999999969,0.124999999999993) ;
#369 = TOROIDAL_SURFACE('',#34882,0.188499999999987,0.124999999999993) ;
#370 = TOROIDAL_SURFACE('',#34885,0.188499999999987,0.124999999999993) ;
#371 = TOROIDAL_SURFACE('',#34892,0.188499999999987,0.124999999999993) ;
#372 = TOROIDAL_SURFACE('',#34937,0.188499999999969,0.124999999999993) ;
#373 = TOROIDAL_SURFACE('',#34942,0.188499999999987,0.124999999999993) ;
#374 = TOROIDAL_SURFACE('',#34945,0.188499999999987,0.124999999999993) ;
#375 = TOROIDAL_SURFACE('',#34952,0.188499999999987,0.124999999999993) ;
#376 = TOROIDAL_SURFACE('',#34997,0.188499999999969,0.124999999999993) ;
#377 = TOROIDAL_SURFACE('',#35002,0.188499999999987,0.124999999999993) ;
#378 = TOROIDAL_SURFACE('',#35005,0.188499999999987,0.124999999999993) ;
#379 = TOROIDAL_SURFACE('',#35012,0.188499999999987,0.124999999999993) ;
#380 = TOROIDAL_SURFACE('',#35057,0.188499999999969,0.124999999999993) ;
#381 = TOROIDAL_SURFACE('',#35062,0.188499999999987,0.124999999999993) ;
#382 = TOROIDAL_SURFACE('',#35065,0.188499999999987,0.124999999999993) ;
#383 = TOROIDAL_SURFACE('',#35072,0.188499999999987,0.124999999999993) ;
#384 = TOROIDAL_SURFACE('',#35117,0.188499999999969,0.124999999999993) ;
#385 = TOROIDAL_SURFACE('',#35122,0.188499999999987,0.124999999999993) ;
#386 = TOROIDAL_SURFACE('',#35125,0.188499999999987,0.124999999999993) ;
#387 = TOROIDAL_SURFACE('',#35132,0.188499999999987,0.124999999999993) ;
#388 = TOROIDAL_SURFACE('',#35177,0.188499999999969,0.124999999999993) ;
#389 = TOROIDAL_SURFACE('',#35182,0.188499999999987,0.124999999999993) ;
#390 = TOROIDAL_SURFACE('',#35185,0.188499999999987,0.124999999999993) ;
#391 = TOROIDAL_SURFACE('',#35192,0.188499999999987,0.124999999999993) ;
#392 = TOROIDAL_SURFACE('',#35330,2.9825,0.125) ;
#393 = TOROIDAL_SURFACE('',#35336,2.7325,0.125) ;
#394 = TOROIDAL_SURFACE('',#35342,2.9825,0.125) ;
#395 = TOROIDAL_SURFACE('',#35348,2.7325,0.125) ;
#396 = TOROIDAL_SURFACE('',#35354,2.9825,0.125) ;
#397 = TOROIDAL_SURFACE('',#35360,2.7325,0.125) ;
#398 = TOROIDAL_SURFACE('',#35366,2.9825,0.125) ;
#399 = TOROIDAL_SURFACE('',#35372,2.7325,0.125) ;
#400 = TOROIDAL_SURFACE('',#35378,2.9825,0.125) ;
#401 = TOROIDAL_SURFACE('',#35384,2.7325,0.125) ;
#402 = TOROIDAL_SURFACE('',#35390,2.9825,0.125) ;
#403 = TOROIDAL_SURFACE('',#35396,2.7325,0.125) ;
#404 = TOROIDAL_SURFACE('',#35402,2.9825,0.125) ;
#405 = TOROIDAL_SURFACE('',#35408,2.7325,0.125) ;
#406 = TOROIDAL_SURFACE('',#35414,2.9825,0.125) ;
#407 = TOROIDAL_SURFACE('',#35420,2.7325,0.125) ;
#408 = TOROIDAL_SURFACE('',#35424,2.9825,0.125) ;
#409 = TOROIDAL_SURFACE('',#35430,2.7325,0.125) ;
#410 = TOROIDAL_SURFACE('',#35507,2.985516,0.443484) ;
#411 = TOROIDAL_SURFACE('',#35518,3.2727760605723,0.1) ;
#412 = TOROIDAL_SURFACE('',#35542,3.2727760605723,0.1) ;
#413 = TOROIDAL_SURFACE('',#35566,5.28650897109211,0.1) ;
#414 = TOROIDAL_SURFACE('',#35587,5.28650897109211,0.1) ;
#415 = TOROIDAL_SURFACE('',#35613,2.31499663839041,0.1) ;
#416 = TOROIDAL_SURFACE('',#35619,1.74337006393707,0.1) ;
#417 = TOROIDAL_SURFACE('',#35630,5.28650897109211,0.1) ;
#418 = TOROIDAL_SURFACE('',#35661,1.8526,0.1) ;
#419 = TOROIDAL_SURFACE('',#35683,1.99389469750719,0.1) ;
#420 = TOROIDAL_SURFACE('',#35739,5.25939963812285,0.1) ;
#421 = TOROIDAL_SURFACE('',#35741,5.21754264299203,0.1) ;
#422 = TOROIDAL_SURFACE('',#35778,1.99389469750719,0.1) ;
#423 = TOROIDAL_SURFACE('',#35837,5.25939963812284,0.1) ;
#424 = TOROIDAL_SURFACE('',#35839,5.21754264299203,0.1) ;
#425 = TOROIDAL_SURFACE('',#35855,1.74337006393707,0.1) ;
#426 = TOROIDAL_SURFACE('',#35858,1.74337006393707,0.1) ;
#427 = TOROIDAL_SURFACE('',#35861,1.74337006393707,0.1) ;
#428 = TOROIDAL_SURFACE('',#35868,5.21754264299203,0.1) ;
#429 = TOROIDAL_SURFACE('',#35871,5.25939963812284,0.1) ;
#430 = TOROIDAL_SURFACE('',#35873,2.31499663839041,0.1) ;
#431 = TOROIDAL_SURFACE('',#35880,2.985516,0.443484) ;
#432 = TOROIDAL_SURFACE('',#35884,5.21754264299203,0.1) ;
#433 = TOROIDAL_SURFACE('',#35886,5.25939963812284,0.1) ;
#434 = TOROIDAL_SURFACE('',#35888,5.28650897109211,0.1) ;
#435 = TOROIDAL_SURFACE('',#35894,2.985516,0.443484) ;
#436 = TOROIDAL_SURFACE('',#35930,0.188499999999969,0.124999999999993) ;
#437 = TOROIDAL_SURFACE('',#35937,0.188499999999987,0.124999999999993) ;
#438 = TOROIDAL_SURFACE('',#35942,0.188499999999987,0.124999999999993) ;
#439 = TOROIDAL_SURFACE('',#35949,0.509999999999996,0.125) ;
#440 = TOROIDAL_SURFACE('',#35956,0.188499999999987,0.124999999999993) ;
#441 = TOROIDAL_SURFACE('',#35965,0.509999999999996,0.125) ;
#442 = TOROIDAL_SURFACE('',#36032,0.25,0.125) ;
#443 = TOROIDAL_SURFACE('',#36035,0.25,0.125) ;
#444 = TOROIDAL_SURFACE('',#36038,0.25,0.125) ;
#445 = TOROIDAL_SURFACE('',#36044,0.25,0.125) ;
#446 = TOROIDAL_SURFACE('',#36064,0.573499999999999,0.125) ;
#447 = TOROIDAL_SURFACE('',#36068,0.573500000000001,0.125) ;
#448 = TOROIDAL_SURFACE('',#36081,0.573500000000001,0.125) ;
#449 = TOROIDAL_SURFACE('',#36085,0.573499999999999,0.125) ;
#450 = TOROIDAL_SURFACE('',#36111,0.249999999999986,0.124999999999993) ;
#451 = TOROIDAL_SURFACE('',#36115,0.250000000000004,0.124999999999993) ;
#452 = TOROIDAL_SURFACE('',#36120,0.249999999999968,0.124999999999993) ;
#453 = TOROIDAL_SURFACE('',#36121,0.249999999999986,0.124999999999993) ;
#454 = TOROIDAL_SURFACE('',#36122,2.7325,0.125) ;
#455 = TOROIDAL_SURFACE('',#36131,2.9825,0.125) ;
#456 = TOROIDAL_SURFACE('',#36171,0.730250002805488,0.0952500026781452) ;
#457 = TOROIDAL_SURFACE('',#36179,0.730250002805489,0.0952500026781457) ;
#458 = TOROIDAL_SURFACE('',#36187,0.730250002805489,0.0952500026781457) ;
#459 = TOROIDAL_SURFACE('',#36205,0.571500002095673,0.0634999979994503) ;
#460 = TOROIDAL_SURFACE('',#36208,0.571500002095676,0.0634999979994492) ;
#461 = TOROIDAL_SURFACE('',#36220,0.571500002095676,0.0634999979994491) ;
#462 = TOROIDAL_SURFACE('',#36237,0.571500002095674,0.0634999979994503) ;
#463 = TOROIDAL_SURFACE('',#36240,0.730250002805489,0.0952500026781457) ;
#464 = TOROIDAL_SURFACE('',#36260,0.445134999999998,0.189865000000001) ;
#465 = TOROIDAL_SURFACE('',#36274,0.445134999999997,0.189865000000001) ;
#466 = TOROIDAL_SURFACE('',#36288,0.445134999999999,0.189865) ;
#467 = TOROIDAL_SURFACE('',#36302,0.445134999999993,0.189865000000003) ;
#468 = TOROIDAL_SURFACE('',#36429,2.55,0.449999999999999) ;
#469 = TOROIDAL_SURFACE('',#36456,2.55,0.45) ;
#470 = TOROIDAL_SURFACE('',#36487,2.9375,0.0625) ;
#471 = TOROIDAL_SURFACE('',#36497,2.9375,0.0625) ;
#472 = ITEM_DEFINED_TRANSFORMATION($,$,#33062,#33118) ;
#473 = ITEM_DEFINED_TRANSFORMATION($,$,#33062,#33119) ;
#474 = ITEM_DEFINED_TRANSFORMATION($,$,#33062,#33120) ;
#475 = ITEM_DEFINED_TRANSFORMATION($,$,#33062,#33121) ;
#476 = ITEM_DEFINED_TRANSFORMATION($,$,#33062,#33122) ;
#477 = ITEM_DEFINED_TRANSFORMATION($,$,#33124,#33195) ;
#478 = ITEM_DEFINED_TRANSFORMATION($,$,#33124,#33196) ;
#479 = ITEM_DEFINED_TRANSFORMATION($,$,#33124,#33197) ;
#480 = ITEM_DEFINED_TRANSFORMATION($,$,#33124,#33198) ;
#481 = ITEM_DEFINED_TRANSFORMATION($,$,#33124,#33199) ;
#482 = ITEM_DEFINED_TRANSFORMATION($,$,#33124,#33200) ;
#483 = ITEM_DEFINED_TRANSFORMATION($,$,#33061,#33712) ;
#484 = ITEM_DEFINED_TRANSFORMATION($,$,#33123,#33713) ;
#485 = ITEM_DEFINED_TRANSFORMATION($,$,#32773,#33714) ;
#486 = ITEM_DEFINED_TRANSFORMATION($,$,#33060,#33715) ;
#487 = ITEM_DEFINED_TRANSFORMATION($,$,#35475,#35902) ;
#488 = ITEM_DEFINED_TRANSFORMATION($,$,#35475,#35903) ;
#489 = ITEM_DEFINED_TRANSFORMATION($,$,#35475,#35904) ;
#490 = ITEM_DEFINED_TRANSFORMATION($,$,#35475,#35905) ;
#491 = ITEM_DEFINED_TRANSFORMATION($,$,#35475,#35906) ;
#492 = ITEM_DEFINED_TRANSFORMATION($,$,#35475,#35907) ;
#493 = ITEM_DEFINED_TRANSFORMATION($,$,#35475,#35908) ;
#494 = ITEM_DEFINED_TRANSFORMATION($,$,#35475,#35909) ;
#495 = ITEM_DEFINED_TRANSFORMATION($,$,#35475,#35910) ;
#496 = ITEM_DEFINED_TRANSFORMATION($,$,#35912,#36134) ;
#497 = ITEM_DEFINED_TRANSFORMATION($,$,#35912,#36135) ;
#498 = ITEM_DEFINED_TRANSFORMATION($,$,#35912,#36136) ;
#499 = ITEM_DEFINED_TRANSFORMATION($,$,#35912,#36137) ;
#500 = ITEM_DEFINED_TRANSFORMATION($,$,#35912,#36138) ;
#501 = ITEM_DEFINED_TRANSFORMATION($,$,#35912,#36139) ;
#502 = ITEM_DEFINED_TRANSFORMATION($,$,#35912,#36140) ;
#503 = ITEM_DEFINED_TRANSFORMATION($,$,#35912,#36141) ;
#504 = ITEM_DEFINED_TRANSFORMATION($,$,#35912,#36142) ;
#505 = ITEM_DEFINED_TRANSFORMATION($,$,#36144,#36330) ;
#506 = ITEM_DEFINED_TRANSFORMATION($,$,#36144,#36331) ;
#507 = ITEM_DEFINED_TRANSFORMATION($,$,#36144,#36332) ;
#508 = ITEM_DEFINED_TRANSFORMATION($,$,#36144,#36333) ;
#509 = ITEM_DEFINED_TRANSFORMATION($,$,#36144,#36334) ;
#510 = ITEM_DEFINED_TRANSFORMATION($,$,#36144,#36335) ;
#511 = ITEM_DEFINED_TRANSFORMATION($,$,#36144,#36336) ;
#512 = ITEM_DEFINED_TRANSFORMATION($,$,#36144,#36337) ;
#513 = ITEM_DEFINED_TRANSFORMATION($,$,#36144,#36338) ;
#514 = ITEM_DEFINED_TRANSFORMATION($,$,#33718,#36339) ;
#515 = ITEM_DEFINED_TRANSFORMATION($,$,#35474,#36340) ;
#516 = ITEM_DEFINED_TRANSFORMATION($,$,#35911,#36341) ;
#517 = ITEM_DEFINED_TRANSFORMATION($,$,#36143,#36342) ;
#518 = ITEM_DEFINED_TRANSFORMATION($,$,#36381,#36503) ;
#519 = ITEM_DEFINED_TRANSFORMATION($,$,#36482,#36504) ;
#520 = ITEM_DEFINED_TRANSFORMATION($,$,#36486,#36505) ;
#521 = ITEM_DEFINED_TRANSFORMATION($,$,#36381,#36506) ;
#522 = ITEM_DEFINED_TRANSFORMATION($,$,#36482,#36507) ;
#523 = ITEM_DEFINED_TRANSFORMATION($,$,#36486,#36508) ;
#524 = ITEM_DEFINED_TRANSFORMATION($,$,#36381,#36509) ;
#525 = ITEM_DEFINED_TRANSFORMATION($,$,#36482,#36510) ;
#526 = ITEM_DEFINED_TRANSFORMATION($,$,#36486,#36511) ;
#527 = ITEM_DEFINED_TRANSFORMATION($,$,#36381,#36512) ;
#528 = ITEM_DEFINED_TRANSFORMATION($,$,#36482,#36513) ;
#529 = ITEM_DEFINED_TRANSFORMATION($,$,#36486,#36514) ;
#530 = ITEM_DEFINED_TRANSFORMATION($,$,#33717,#36515) ;
#531 = ITEM_DEFINED_TRANSFORMATION($,$,#36343,#36516) ;
#532 = ITEM_DEFINED_TRANSFORMATION($,$,#36377,#36517) ;
#533 = ITEM_DEFINED_TRANSFORMATION($,$,#36378,#36518) ;
#534 = ITEM_DEFINED_TRANSFORMATION($,$,#36379,#36519) ;
#535 = ITEM_DEFINED_TRANSFORMATION($,$,#36380,#36520) ;
#536 = ITEM_DEFINED_TRANSFORMATION($,$,#32772,#36521) ;
#537 = ITEM_DEFINED_TRANSFORMATION($,$,#33716,#36522) ;
#538 = (
REPRESENTATION_RELATIONSHIP($,$,#86456,#86455)
REPRESENTATION_RELATIONSHIP_WITH_TRANSFORMATION(#472)
SHAPE_REPRESENTATION_RELATIONSHIP()
) ;
#539 = (
REPRESENTATION_RELATIONSHIP($,$,#86456,#86455)
REPRESENTATION_RELATIONSHIP_WITH_TRANSFORMATION(#473)
SHAPE_REPRESENTATION_RELATIONSHIP()
) ;
#540 = (
REPRESENTATION_RELATIONSHIP($,$,#86456,#86455)
REPRESENTATION_RELATIONSHIP_WITH_TRANSFORMATION(#474)
SHAPE_REPRESENTATION_RELATIONSHIP()
) ;
#541 = (
REPRESENTATION_RELATIONSHIP($,$,#86456,#86455)
REPRESENTATION_RELATIONSHIP_WITH_TRANSFORMATION(#475)
SHAPE_REPRESENTATION_RELATIONSHIP()
) ;
#542 = (
REPRESENTATION_RELATIONSHIP($,$,#86456,#86455)
REPRESENTATION_RELATIONSHIP_WITH_TRANSFORMATION(#476)
SHAPE_REPRESENTATION_RELATIONSHIP()
) ;
#543 = (
REPRESENTATION_RELATIONSHIP($,$,#86458,#86457)
REPRESENTATION_RELATIONSHIP_WITH_TRANSFORMATION(#477)
SHAPE_REPRESENTATION_RELATIONSHIP()
) ;
#544 = (
REPRESENTATION_RELATIONSHIP($,$,#86458,#86457)
REPRESENTATION_RELATIONSHIP_WITH_TRANSFORMATION(#478)
SHAPE_REPRESENTATION_RELATIONSHIP()
) ;
#545 = (
REPRESENTATION_RELATIONSHIP($,$,#86458,#86457)
REPRESENTATION_RELATIONSHIP_WITH_TRANSFORMATION(#479)
SHAPE_REPRESENTATION_RELATIONSHIP()
) ;
#546 = (
REPRESENTATION_RELATIONSHIP($,$,#86458,#86457)
REPRESENTATION_RELATIONSHIP_WITH_TRANSFORMATION(#480)
SHAPE_REPRESENTATION_RELATIONSHIP()
) ;
#547 = (
REPRESENTATION_RELATIONSHIP($,$,#86458,#86457)
REPRESENTATION_RELATIONSHIP_WITH_TRANSFORMATION(#481)
SHAPE_REPRESENTATION_RELATIONSHIP()
) ;
#548 = (
REPRESENTATION_RELATIONSHIP($,$,#86458,#86457)
REPRESENTATION_RELATIONSHIP_WITH_TRANSFORMATION(#482)
SHAPE_REPRESENTATION_RELATIONSHIP()
) ;
#549 = (
REPRESENTATION_RELATIONSHIP($,$,#86455,#86454)
REPRESENTATION_RELATIONSHIP_WITH_TRANSFORMATION(#483)
SHAPE_REPRESENTATION_RELATIONSHIP()
) ;
#550 = (
REPRESENTATION_RELATIONSHIP($,$,#86457,#86454)
REPRESENTATION_RELATIONSHIP_WITH_TRANSFORMATION(#484)
SHAPE_REPRESENTATION_RELATIONSHIP()
) ;
#551 = (
REPRESENTATION_RELATIONSHIP($,$,#86453,#86452)
REPRESENTATION_RELATIONSHIP_WITH_TRANSFORMATION(#485)
SHAPE_REPRESENTATION_RELATIONSHIP()
) ;
#552 = (
REPRESENTATION_RELATIONSHIP($,$,#86454,#86452)
REPRESENTATION_RELATIONSHIP_WITH_TRANSFORMATION(#486)
SHAPE_REPRESENTATION_RELATIONSHIP()
) ;
#553 = (
REPRESENTATION_RELATIONSHIP($,$,#86463,#86462)
REPRESENTATION_RELATIONSHIP_WITH_TRANSFORMATION(#487)
SHAPE_REPRESENTATION_RELATIONSHIP()
) ;
#554 = (
REPRESENTATION_RELATIONSHIP($,$,#86463,#86462)
REPRESENTATION_RELATIONSHIP_WITH_TRANSFORMATION(#488)
SHAPE_REPRESENTATION_RELATIONSHIP()
) ;
#555 = (
REPRESENTATION_RELATIONSHIP($,$,#86463,#86462)
REPRESENTATION_RELATIONSHIP_WITH_TRANSFORMATION(#489)
SHAPE_REPRESENTATION_RELATIONSHIP()
) ;
#556 = (
REPRESENTATION_RELATIONSHIP($,$,#86463,#86462)
REPRESENTATION_RELATIONSHIP_WITH_TRANSFORMATION(#490)
SHAPE_REPRESENTATION_RELATIONSHIP()
) ;
#557 = (
REPRESENTATION_RELATIONSHIP($,$,#86463,#86462)
REPRESENTATION_RELATIONSHIP_WITH_TRANSFORMATION(#491)
SHAPE_REPRESENTATION_RELATIONSHIP()
) ;
#558 = (
REPRESENTATION_RELATIONSHIP($,$,#86463,#86462)
REPRESENTATION_RELATIONSHIP_WITH_TRANSFORMATION(#492)
SHAPE_REPRESENTATION_RELATIONSHIP()
) ;
#559 = (
REPRESENTATION_RELATIONSHIP($,$,#86463,#86462)
REPRESENTATION_RELATIONSHIP_WITH_TRANSFORMATION(#493)
SHAPE_REPRESENTATION_RELATIONSHIP()
) ;
#560 = (
REPRESENTATION_RELATIONSHIP($,$,#86463,#86462)
REPRESENTATION_RELATIONSHIP_WITH_TRANSFORMATION(#494)
SHAPE_REPRESENTATION_RELATIONSHIP()
) ;
#561 = (
REPRESENTATION_RELATIONSHIP($,$,#86463,#86462)
REPRESENTATION_RELATIONSHIP_WITH_TRANSFORMATION(#495)
SHAPE_REPRESENTATION_RELATIONSHIP()
) ;
#562 = (
REPRESENTATION_RELATIONSHIP($,$,#86465,#86464)
REPRESENTATION_RELATIONSHIP_WITH_TRANSFORMATION(#496)
SHAPE_REPRESENTATION_RELATIONSHIP()
) ;
#563 = (
REPRESENTATION_RELATIONSHIP($,$,#86465,#86464)
REPRESENTATION_RELATIONSHIP_WITH_TRANSFORMATION(#497)
SHAPE_REPRESENTATION_RELATIONSHIP()
) ;
#564 = (
REPRESENTATION_RELATIONSHIP($,$,#86465,#86464)
REPRESENTATION_RELATIONSHIP_WITH_TRANSFORMATION(#498)
SHAPE_REPRESENTATION_RELATIONSHIP()
) ;
#565 = (
REPRESENTATION_RELATIONSHIP($,$,#86465,#86464)
REPRESENTATION_RELATIONSHIP_WITH_TRANSFORMATION(#499)
SHAPE_REPRESENTATION_RELATIONSHIP()
) ;
#566 = (
REPRESENTATION_RELATIONSHIP($,$,#86465,#86464)
REPRESENTATION_RELATIONSHIP_WITH_TRANSFORMATION(#500)
SHAPE_REPRESENTATION_RELATIONSHIP()
) ;
#567 = (
REPRESENTATION_RELATIONSHIP($,$,#86465,#86464)
REPRESENTATION_RELATIONSHIP_WITH_TRANSFORMATION(#501)
SHAPE_REPRESENTATION_RELATIONSHIP()
) ;
#568 = (
REPRESENTATION_RELATIONSHIP($,$,#86465,#86464)
REPRESENTATION_RELATIONSHIP_WITH_TRANSFORMATION(#502)
SHAPE_REPRESENTATION_RELATIONSHIP()
) ;
#569 = (
REPRESENTATION_RELATIONSHIP($,$,#86465,#86464)
REPRESENTATION_RELATIONSHIP_WITH_TRANSFORMATION(#503)
SHAPE_REPRESENTATION_RELATIONSHIP()
) ;
#570 = (
REPRESENTATION_RELATIONSHIP($,$,#86465,#86464)
REPRESENTATION_RELATIONSHIP_WITH_TRANSFORMATION(#504)
SHAPE_REPRESENTATION_RELATIONSHIP()
) ;
#571 = (
REPRESENTATION_RELATIONSHIP($,$,#86467,#86466)
REPRESENTATION_RELATIONSHIP_WITH_TRANSFORMATION(#505)
SHAPE_REPRESENTATION_RELATIONSHIP()
) ;
#572 = (
REPRESENTATION_RELATIONSHIP($,$,#86467,#86466)
REPRESENTATION_RELATIONSHIP_WITH_TRANSFORMATION(#506)
SHAPE_REPRESENTATION_RELATIONSHIP()
) ;
#573 = (
REPRESENTATION_RELATIONSHIP($,$,#86467,#86466)
REPRESENTATION_RELATIONSHIP_WITH_TRANSFORMATION(#507)
SHAPE_REPRESENTATION_RELATIONSHIP()
) ;
#574 = (
REPRESENTATION_RELATIONSHIP($,$,#86467,#86466)
REPRESENTATION_RELATIONSHIP_WITH_TRANSFORMATION(#508)
SHAPE_REPRESENTATION_RELATIONSHIP()
) ;
#575 = (
REPRESENTATION_RELATIONSHIP($,$,#86467,#86466)
REPRESENTATION_RELATIONSHIP_WITH_TRANSFORMATION(#509)
SHAPE_REPRESENTATION_RELATIONSHIP()
) ;
#576 = (
REPRESENTATION_RELATIONSHIP($,$,#86467,#86466)
REPRESENTATION_RELATIONSHIP_WITH_TRANSFORMATION(#510)
SHAPE_REPRESENTATION_RELATIONSHIP()
) ;
#577 = (
REPRESENTATION_RELATIONSHIP($,$,#86467,#86466)
REPRESENTATION_RELATIONSHIP_WITH_TRANSFORMATION(#511)
SHAPE_REPRESENTATION_RELATIONSHIP()
) ;
#578 = (
REPRESENTATION_RELATIONSHIP($,$,#86467,#86466)
REPRESENTATION_RELATIONSHIP_WITH_TRANSFORMATION(#512)
SHAPE_REPRESENTATION_RELATIONSHIP()
) ;
#579 = (
REPRESENTATION_RELATIONSHIP($,$,#86467,#86466)
REPRESENTATION_RELATIONSHIP_WITH_TRANSFORMATION(#513)
SHAPE_REPRESENTATION_RELATIONSHIP()
) ;
#580 = (
REPRESENTATION_RELATIONSHIP($,$,#86461,#86460)
REPRESENTATION_RELATIONSHIP_WITH_TRANSFORMATION(#514)
SHAPE_REPRESENTATION_RELATIONSHIP()
) ;
#581 = (
REPRESENTATION_RELATIONSHIP($,$,#86462,#86460)
REPRESENTATION_RELATIONSHIP_WITH_TRANSFORMATION(#515)
SHAPE_REPRESENTATION_RELATIONSHIP()
) ;
#582 = (
REPRESENTATION_RELATIONSHIP($,$,#86464,#86460)
REPRESENTATION_RELATIONSHIP_WITH_TRANSFORMATION(#516)
SHAPE_REPRESENTATION_RELATIONSHIP()
) ;
#583 = (
REPRESENTATION_RELATIONSHIP($,$,#86466,#86460)
REPRESENTATION_RELATIONSHIP_WITH_TRANSFORMATION(#517)
SHAPE_REPRESENTATION_RELATIONSHIP()
) ;
#584 = (
REPRESENTATION_RELATIONSHIP($,$,#86473,#86469)
REPRESENTATION_RELATIONSHIP_WITH_TRANSFORMATION(#518)
SHAPE_REPRESENTATION_RELATIONSHIP()
) ;
#585 = (
REPRESENTATION_RELATIONSHIP($,$,#86474,#86469)
REPRESENTATION_RELATIONSHIP_WITH_TRANSFORMATION(#519)
SHAPE_REPRESENTATION_RELATIONSHIP()
) ;
#586 = (
REPRESENTATION_RELATIONSHIP($,$,#86475,#86469)
REPRESENTATION_RELATIONSHIP_WITH_TRANSFORMATION(#520)
SHAPE_REPRESENTATION_RELATIONSHIP()
) ;
#587 = (
REPRESENTATION_RELATIONSHIP($,$,#86473,#86470)
REPRESENTATION_RELATIONSHIP_WITH_TRANSFORMATION(#521)
SHAPE_REPRESENTATION_RELATIONSHIP()
) ;
#588 = (
REPRESENTATION_RELATIONSHIP($,$,#86474,#86470)
REPRESENTATION_RELATIONSHIP_WITH_TRANSFORMATION(#522)
SHAPE_REPRESENTATION_RELATIONSHIP()
) ;
#589 = (
REPRESENTATION_RELATIONSHIP($,$,#86475,#86470)
REPRESENTATION_RELATIONSHIP_WITH_TRANSFORMATION(#523)
SHAPE_REPRESENTATION_RELATIONSHIP()
) ;
#590 = (
REPRESENTATION_RELATIONSHIP($,$,#86473,#86471)
REPRESENTATION_RELATIONSHIP_WITH_TRANSFORMATION(#524)
SHAPE_REPRESENTATION_RELATIONSHIP()
) ;
#591 = (
REPRESENTATION_RELATIONSHIP($,$,#86474,#86471)
REPRESENTATION_RELATIONSHIP_WITH_TRANSFORMATION(#525)
SHAPE_REPRESENTATION_RELATIONSHIP()
) ;
#592 = (
REPRESENTATION_RELATIONSHIP($,$,#86475,#86471)
REPRESENTATION_RELATIONSHIP_WITH_TRANSFORMATION(#526)
SHAPE_REPRESENTATION_RELATIONSHIP()
) ;
#593 = (
REPRESENTATION_RELATIONSHIP($,$,#86473,#86472)
REPRESENTATION_RELATIONSHIP_WITH_TRANSFORMATION(#527)
SHAPE_REPRESENTATION_RELATIONSHIP()
) ;
#594 = (
REPRESENTATION_RELATIONSHIP($,$,#86474,#86472)
REPRESENTATION_RELATIONSHIP_WITH_TRANSFORMATION(#528)
SHAPE_REPRESENTATION_RELATIONSHIP()
) ;
#595 = (
REPRESENTATION_RELATIONSHIP($,$,#86475,#86472)
REPRESENTATION_RELATIONSHIP_WITH_TRANSFORMATION(#529)
SHAPE_REPRESENTATION_RELATIONSHIP()
) ;
#596 = (
REPRESENTATION_RELATIONSHIP($,$,#86460,#86459)
REPRESENTATION_RELATIONSHIP_WITH_TRANSFORMATION(#530)
SHAPE_REPRESENTATION_RELATIONSHIP()
) ;
#597 = (
REPRESENTATION_RELATIONSHIP($,$,#86468,#86459)
REPRESENTATION_RELATIONSHIP_WITH_TRANSFORMATION(#531)
SHAPE_REPRESENTATION_RELATIONSHIP()
) ;
#598 = (
REPRESENTATION_RELATIONSHIP($,$,#86469,#86459)
REPRESENTATION_RELATIONSHIP_WITH_TRANSFORMATION(#532)
SHAPE_REPRESENTATION_RELATIONSHIP()
) ;
#599 = (
REPRESENTATION_RELATIONSHIP($,$,#86470,#86459)
REPRESENTATION_RELATIONSHIP_WITH_TRANSFORMATION(#533)
SHAPE_REPRESENTATION_RELATIONSHIP()
) ;
#600 = (
REPRESENTATION_RELATIONSHIP($,$,#86471,#86459)
REPRESENTATION_RELATIONSHIP_WITH_TRANSFORMATION(#534)
SHAPE_REPRESENTATION_RELATIONSHIP()
) ;
#601 = (
REPRESENTATION_RELATIONSHIP($,$,#86472,#86459)
REPRESENTATION_RELATIONSHIP_WITH_TRANSFORMATION(#535)
SHAPE_REPRESENTATION_RELATIONSHIP()
) ;
#602 = (
REPRESENTATION_RELATIONSHIP($,$,#86452,#86451)
REPRESENTATION_RELATIONSHIP_WITH_TRANSFORMATION(#536)
SHAPE_REPRESENTATION_RELATIONSHIP()
) ;
#603 = (
REPRESENTATION_RELATIONSHIP($,$,#86459,#86451)
REPRESENTATION_RELATIONSHIP_WITH_TRANSFORMATION(#537)
SHAPE_REPRESENTATION_RELATIONSHIP()
) ;
#604 = CONTEXT_DEPENDENT_SHAPE_REPRESENTATION(#538,#86366) ;
#605 = CONTEXT_DEPENDENT_SHAPE_REPRESENTATION(#539,#86367) ;
#606 = CONTEXT_DEPENDENT_SHAPE_REPRESENTATION(#540,#86368) ;
#607 = CONTEXT_DEPENDENT_SHAPE_REPRESENTATION(#541,#86369) ;
#608 = CONTEXT_DEPENDENT_SHAPE_REPRESENTATION(#542,#86370) ;
#609 = CONTEXT_DEPENDENT_SHAPE_REPRESENTATION(#543,#86373) ;
#610 = CONTEXT_DEPENDENT_SHAPE_REPRESENTATION(#544,#86374) ;
#611 = CONTEXT_DEPENDENT_SHAPE_REPRESENTATION(#545,#86375) ;
#612 = CONTEXT_DEPENDENT_SHAPE_REPRESENTATION(#546,#86376) ;
#613 = CONTEXT_DEPENDENT_SHAPE_REPRESENTATION(#547,#86377) ;
#614 = CONTEXT_DEPENDENT_SHAPE_REPRESENTATION(#548,#86378) ;
#615 = CONTEXT_DEPENDENT_SHAPE_REPRESENTATION(#549,#86379) ;
#616 = CONTEXT_DEPENDENT_SHAPE_REPRESENTATION(#550,#86380) ;
#617 = CONTEXT_DEPENDENT_SHAPE_REPRESENTATION(#551,#86381) ;
#618 = CONTEXT_DEPENDENT_SHAPE_REPRESENTATION(#552,#86382) ;
#619 = CONTEXT_DEPENDENT_SHAPE_REPRESENTATION(#553,#86388) ;
#620 = CONTEXT_DEPENDENT_SHAPE_REPRESENTATION(#554,#86389) ;
#621 = CONTEXT_DEPENDENT_SHAPE_REPRESENTATION(#555,#86390) ;
#622 = CONTEXT_DEPENDENT_SHAPE_REPRESENTATION(#556,#86391) ;
#623 = CONTEXT_DEPENDENT_SHAPE_REPRESENTATION(#557,#86392) ;
#624 = CONTEXT_DEPENDENT_SHAPE_REPRESENTATION(#558,#86393) ;
#625 = CONTEXT_DEPENDENT_SHAPE_REPRESENTATION(#559,#86394) ;
#626 = CONTEXT_DEPENDENT_SHAPE_REPRESENTATION(#560,#86395) ;
#627 = CONTEXT_DEPENDENT_SHAPE_REPRESENTATION(#561,#86396) ;
#628 = CONTEXT_DEPENDENT_SHAPE_REPRESENTATION(#562,#86399) ;
#629 = CONTEXT_DEPENDENT_SHAPE_REPRESENTATION(#563,#86400) ;
#630 = CONTEXT_DEPENDENT_SHAPE_REPRESENTATION(#564,#86401) ;
#631 = CONTEXT_DEPENDENT_SHAPE_REPRESENTATION(#565,#86402) ;
#632 = CONTEXT_DEPENDENT_SHAPE_REPRESENTATION(#566,#86403) ;
#633 = CONTEXT_DEPENDENT_SHAPE_REPRESENTATION(#567,#86404) ;
#634 = CONTEXT_DEPENDENT_SHAPE_REPRESENTATION(#568,#86405) ;
#635 = CONTEXT_DEPENDENT_SHAPE_REPRESENTATION(#569,#86406) ;
#636 = CONTEXT_DEPENDENT_SHAPE_REPRESENTATION(#570,#86407) ;
#637 = CONTEXT_DEPENDENT_SHAPE_REPRESENTATION(#571,#86410) ;
#638 = CONTEXT_DEPENDENT_SHAPE_REPRESENTATION(#572,#86411) ;
#639 = CONTEXT_DEPENDENT_SHAPE_REPRESENTATION(#573,#86412) ;
#640 = CONTEXT_DEPENDENT_SHAPE_REPRESENTATION(#574,#86413) ;
#641 = CONTEXT_DEPENDENT_SHAPE_REPRESENTATION(#575,#86414) ;
#642 = CONTEXT_DEPENDENT_SHAPE_REPRESENTATION(#576,#86415) ;
#643 = CONTEXT_DEPENDENT_SHAPE_REPRESENTATION(#577,#86416) ;
#644 = CONTEXT_DEPENDENT_SHAPE_REPRESENTATION(#578,#86417) ;
#645 = CONTEXT_DEPENDENT_SHAPE_REPRESENTATION(#579,#86418) ;
#646 = CONTEXT_DEPENDENT_SHAPE_REPRESENTATION(#580,#86419) ;
#647 = CONTEXT_DEPENDENT_SHAPE_REPRESENTATION(#581,#86420) ;
#648 = CONTEXT_DEPENDENT_SHAPE_REPRESENTATION(#582,#86421) ;
#649 = CONTEXT_DEPENDENT_SHAPE_REPRESENTATION(#583,#86422) ;
#650 = CONTEXT_DEPENDENT_SHAPE_REPRESENTATION(#584,#86431) ;
#651 = CONTEXT_DEPENDENT_SHAPE_REPRESENTATION(#585,#86432) ;
#652 = CONTEXT_DEPENDENT_SHAPE_REPRESENTATION(#586,#86433) ;
#653 = CONTEXT_DEPENDENT_SHAPE_REPRESENTATION(#587,#86434) ;
#654 = CONTEXT_DEPENDENT_SHAPE_REPRESENTATION(#588,#86435) ;
#655 = CONTEXT_DEPENDENT_SHAPE_REPRESENTATION(#589,#86436) ;
#656 = CONTEXT_DEPENDENT_SHAPE_REPRESENTATION(#590,#86437) ;
#657 = CONTEXT_DEPENDENT_SHAPE_REPRESENTATION(#591,#86438) ;
#658 = CONTEXT_DEPENDENT_SHAPE_REPRESENTATION(#592,#86439) ;
#659 = CONTEXT_DEPENDENT_SHAPE_REPRESENTATION(#593,#86440) ;
#660 = CONTEXT_DEPENDENT_SHAPE_REPRESENTATION(#594,#86441) ;
#661 = CONTEXT_DEPENDENT_SHAPE_REPRESENTATION(#595,#86442) ;
#662 = CONTEXT_DEPENDENT_SHAPE_REPRESENTATION(#596,#86443) ;
#663 = CONTEXT_DEPENDENT_SHAPE_REPRESENTATION(#597,#86444) ;
#664 = CONTEXT_DEPENDENT_SHAPE_REPRESENTATION(#598,#86445) ;
#665 = CONTEXT_DEPENDENT_SHAPE_REPRESENTATION(#599,#86446) ;
#666 = CONTEXT_DEPENDENT_SHAPE_REPRESENTATION(#600,#86447) ;
#667 = CONTEXT_DEPENDENT_SHAPE_REPRESENTATION(#601,#86448) ;
#668 = CONTEXT_DEPENDENT_SHAPE_REPRESENTATION(#602,#86449) ;
#669 = CONTEXT_DEPENDENT_SHAPE_REPRESENTATION(#603,#86450) ;
#670 = NEXT_ASSEMBLY_USAGE_OCCURRENCE('Hex_Nut:1','Hex_Nut:1','Hex_Nut:1',
#86481,#86482,'Hex_Nut:1') ;
#671 = NEXT_ASSEMBLY_USAGE_OCCURRENCE('Hex_Nut:2','Hex_Nut:2','Hex_Nut:2',
#86481,#86482,'Hex_Nut:2') ;
#672 = NEXT_ASSEMBLY_USAGE_OCCURRENCE('Hex_Nut:3','Hex_Nut:3','Hex_Nut:3',
#86481,#86482,'Hex_Nut:3') ;
#673 = NEXT_ASSEMBLY_USAGE_OCCURRENCE('Hex_Nut:4','Hex_Nut:4','Hex_Nut:4',
#86481,#86482,'Hex_Nut:4') ;
#674 = NEXT_ASSEMBLY_USAGE_OCCURRENCE('Hex_Nut:5','Hex_Nut:5','Hex_Nut:5',
#86481,#86482,'Hex_Nut:5') ;
#675 = NEXT_ASSEMBLY_USAGE_OCCURRENCE('Flat_Head_Screw:1',
'Flat_Head_Screw:1','Flat_Head_Screw:1',#86483,#86484,
'Flat_Head_Screw:1') ;
#676 = NEXT_ASSEMBLY_USAGE_OCCURRENCE('Flat_Head_Screw:2',
'Flat_Head_Screw:2','Flat_Head_Screw:2',#86483,#86484,
'Flat_Head_Screw:2') ;
#677 = NEXT_ASSEMBLY_USAGE_OCCURRENCE('Flat_Head_Screw:3',
'Flat_Head_Screw:3','Flat_Head_Screw:3',#86483,#86484,
'Flat_Head_Screw:3') ;
#678 = NEXT_ASSEMBLY_USAGE_OCCURRENCE('Flat_Head_Screw:4',
'Flat_Head_Screw:4','Flat_Head_Screw:4',#86483,#86484,
'Flat_Head_Screw:4') ;
#679 = NEXT_ASSEMBLY_USAGE_OCCURRENCE('Flat_Head_Screw:5',
'Flat_Head_Screw:5','Flat_Head_Screw:5',#86483,#86484,
'Flat_Head_Screw:5') ;
#680 = NEXT_ASSEMBLY_USAGE_OCCURRENCE('Flat_Head_Screw:6',
'Flat_Head_Screw:6','Flat_Head_Screw:6',#86483,#86484,
'Flat_Head_Screw:6') ;
#681 = NEXT_ASSEMBLY_USAGE_OCCURRENCE('Box_Nuts:1','Box_Nuts:1',
'Box_Nuts:1',#86480,#86481,'Box_Nuts:1') ;
#682 = NEXT_ASSEMBLY_USAGE_OCCURRENCE('Box_Screws:1','Box_Screws:1',
'Box_Screws:1',#86480,#86483,'Box_Screws:1') ;
#683 = NEXT_ASSEMBLY_USAGE_OCCURRENCE('Lid:1','Lid:1','Lid:1',#86478,#86479,
'Lid:1') ;
#684 = NEXT_ASSEMBLY_USAGE_OCCURRENCE('Box:1','Box:1','Box:1',#86478,#86480,
'Box:1') ;
#685 = NEXT_ASSEMBLY_USAGE_OCCURRENCE('Pan_Head_Screw:1',
'Pan_Head_Screw:1','Pan_Head_Screw:1',#86488,#86489,'Pan_Head_Screw:1') ;
#686 = NEXT_ASSEMBLY_USAGE_OCCURRENCE('Pan_Head_Screw:2',
'Pan_Head_Screw:2','Pan_Head_Screw:2',#86488,#86489,'Pan_Head_Screw:2') ;
#687 = NEXT_ASSEMBLY_USAGE_OCCURRENCE('Pan_Head_Screw:3',
'Pan_Head_Screw:3','Pan_Head_Screw:3',#86488,#86489,'Pan_Head_Screw:3') ;
#688 = NEXT_ASSEMBLY_USAGE_OCCURRENCE('Pan_Head_Screw:4',
'Pan_Head_Screw:4','Pan_Head_Screw:4',#86488,#86489,'Pan_Head_Screw:4') ;
#689 = NEXT_ASSEMBLY_USAGE_OCCURRENCE('Pan_Head_Screw:5',
'Pan_Head_Screw:5','Pan_Head_Screw:5',#86488,#86489,'Pan_Head_Screw:5') ;
#690 = NEXT_ASSEMBLY_USAGE_OCCURRENCE('Pan_Head_Screw:6',
'Pan_Head_Screw:6','Pan_Head_Screw:6',#86488,#86489,'Pan_Head_Screw:6') ;
#691 = NEXT_ASSEMBLY_USAGE_OCCURRENCE('Pan_Head_Screw:7',
'Pan_Head_Screw:7','Pan_Head_Screw:7',#86488,#86489,'Pan_Head_Screw:7') ;
#692 = NEXT_ASSEMBLY_USAGE_OCCURRENCE('Pan_Head_Screw:8',
'Pan_Head_Screw:8','Pan_Head_Screw:8',#86488,#86489,'Pan_Head_Screw:8') ;
#693 = NEXT_ASSEMBLY_USAGE_OCCURRENCE('Pan_Head_Screw:9',
'Pan_Head_Screw:9','Pan_Head_Screw:9',#86488,#86489,'Pan_Head_Screw:9') ;
#694 = NEXT_ASSEMBLY_USAGE_OCCURRENCE('Squash_Plate:1','Squash_Plate:1',
'Squash_Plate:1',#86490,#86491,'Squash_Plate:1') ;
#695 = NEXT_ASSEMBLY_USAGE_OCCURRENCE('Squash_Plate:2','Squash_Plate:2',
'Squash_Plate:2',#86490,#86491,'Squash_Plate:2') ;
#696 = NEXT_ASSEMBLY_USAGE_OCCURRENCE('Squash_Plate:3','Squash_Plate:3',
'Squash_Plate:3',#86490,#86491,'Squash_Plate:3') ;
#697 = NEXT_ASSEMBLY_USAGE_OCCURRENCE('Squash_Plate:4','Squash_Plate:4',
'Squash_Plate:4',#86490,#86491,'Squash_Plate:4') ;
#698 = NEXT_ASSEMBLY_USAGE_OCCURRENCE('Squash_Plate:5','Squash_Plate:5',
'Squash_Plate:5',#86490,#86491,'Squash_Plate:5') ;
#699 = NEXT_ASSEMBLY_USAGE_OCCURRENCE('Squash_Plate:6','Squash_Plate:6',
'Squash_Plate:6',#86490,#86491,'Squash_Plate:6') ;
#700 = NEXT_ASSEMBLY_USAGE_OCCURRENCE('Squash_Plate:7','Squash_Plate:7',
'Squash_Plate:7',#86490,#86491,'Squash_Plate:7') ;
#701 = NEXT_ASSEMBLY_USAGE_OCCURRENCE('Squash_Plate:8','Squash_Plate:8',
'Squash_Plate:8',#86490,#86491,'Squash_Plate:8') ;
#702 = NEXT_ASSEMBLY_USAGE_OCCURRENCE('Squash_Plate:9','Squash_Plate:9',
'Squash_Plate:9',#86490,#86491,'Squash_Plate:9') ;
#703 = NEXT_ASSEMBLY_USAGE_OCCURRENCE('Flat_Washer_Large:1',
'Flat_Washer_Large:1','Flat_Washer_Large:1',#86492,#86493,
'Flat_Washer_Large:1') ;
#704 = NEXT_ASSEMBLY_USAGE_OCCURRENCE('Flat_Washer_Large:2',
'Flat_Washer_Large:2','Flat_Washer_Large:2',#86492,#86493,
'Flat_Washer_Large:2') ;
#705 = NEXT_ASSEMBLY_USAGE_OCCURRENCE('Flat_Washer_Large:3',
'Flat_Washer_Large:3','Flat_Washer_Large:3',#86492,#86493,
'Flat_Washer_Large:3') ;
#706 = NEXT_ASSEMBLY_USAGE_OCCURRENCE('Flat_Washer_Large:4',
'Flat_Washer_Large:4','Flat_Washer_Large:4',#86492,#86493,
'Flat_Washer_Large:4') ;
#707 = NEXT_ASSEMBLY_USAGE_OCCURRENCE('Flat_Washer_Large:5',
'Flat_Washer_Large:5','Flat_Washer_Large:5',#86492,#86493,
'Flat_Washer_Large:5') ;
#708 = NEXT_ASSEMBLY_USAGE_OCCURRENCE('Flat_Washer_Large:6',
'Flat_Washer_Large:6','Flat_Washer_Large:6',#86492,#86493,
'Flat_Washer_Large:6') ;
#709 = NEXT_ASSEMBLY_USAGE_OCCURRENCE('Flat_Washer_Large:7',
'Flat_Washer_Large:7','Flat_Washer_Large:7',#86492,#86493,
'Flat_Washer_Large:7') ;
#710 = NEXT_ASSEMBLY_USAGE_OCCURRENCE('Flat_Washer_Large:8',
'Flat_Washer_Large:8','Flat_Washer_Large:8',#86492,#86493,
'Flat_Washer_Large:8') ;
#711 = NEXT_ASSEMBLY_USAGE_OCCURRENCE('Flat_Washer_Large:9',
'Flat_Washer_Large:9','Flat_Washer_Large:9',#86492,#86493,
'Flat_Washer_Large:9') ;
#712 = NEXT_ASSEMBLY_USAGE_OCCURRENCE('Insulator:1','Insulator:1',
'Insulator:1',#86486,#86487,'Insulator:1') ;
#713 = NEXT_ASSEMBLY_USAGE_OCCURRENCE('Screws:1','Screws:1','Screws:1',#86486,
#86488,'Screws:1') ;
#714 = NEXT_ASSEMBLY_USAGE_OCCURRENCE('Plates:1','Plates:1','Plates:1',#86486,
#86490,'Plates:1') ;
#715 = NEXT_ASSEMBLY_USAGE_OCCURRENCE('Washers:1','Washers:1','Washers:1',
#86486,#86492,'Washers:1') ;
#716 = NEXT_ASSEMBLY_USAGE_OCCURRENCE('Pan_Head_Phillips_Screw:1',
'Pan_Head_Phillips_Screw:1','Pan_Head_Phillips_Screw:1',#86495,#86499,
'Pan_Head_Phillips_Screw:1') ;
#717 = NEXT_ASSEMBLY_USAGE_OCCURRENCE('Lock_Washer:1','Lock_Washer:1',
'Lock_Washer:1',#86495,#86500,'Lock_Washer:1') ;
#718 = NEXT_ASSEMBLY_USAGE_OCCURRENCE('Flat_Washer_Small:1',
'Flat_Washer_Small:1','Flat_Washer_Small:1',#86495,#86501,
'Flat_Washer_Small:1') ;
#719 = NEXT_ASSEMBLY_USAGE_OCCURRENCE('Pan_Head_Phillips_Screw:1',
'Pan_Head_Phillips_Screw:1','Pan_Head_Phillips_Screw:1',#86496,#86499,
'Pan_Head_Phillips_Screw:1') ;
#720 = NEXT_ASSEMBLY_USAGE_OCCURRENCE('Lock_Washer:1','Lock_Washer:1',
'Lock_Washer:1',#86496,#86500,'Lock_Washer:1') ;
#721 = NEXT_ASSEMBLY_USAGE_OCCURRENCE('Flat_Washer_Small:1',
'Flat_Washer_Small:1','Flat_Washer_Small:1',#86496,#86501,
'Flat_Washer_Small:1') ;
#722 = NEXT_ASSEMBLY_USAGE_OCCURRENCE('Pan_Head_Phillips_Screw:1',
'Pan_Head_Phillips_Screw:1','Pan_Head_Phillips_Screw:1',#86497,#86499,
'Pan_Head_Phillips_Screw:1') ;
#723 = NEXT_ASSEMBLY_USAGE_OCCURRENCE('Lock_Washer:1','Lock_Washer:1',
'Lock_Washer:1',#86497,#86500,'Lock_Washer:1') ;
#724 = NEXT_ASSEMBLY_USAGE_OCCURRENCE('Flat_Washer_Small:1',
'Flat_Washer_Small:1','Flat_Washer_Small:1',#86497,#86501,
'Flat_Washer_Small:1') ;
#725 = NEXT_ASSEMBLY_USAGE_OCCURRENCE('Pan_Head_Phillips_Screw:1',
'Pan_Head_Phillips_Screw:1','Pan_Head_Phillips_Screw:1',#86498,#86499,
'Pan_Head_Phillips_Screw:1') ;
#726 = NEXT_ASSEMBLY_USAGE_OCCURRENCE('Lock_Washer:1','Lock_Washer:1',
'Lock_Washer:1',#86498,#86500,'Lock_Washer:1') ;
#727 = NEXT_ASSEMBLY_USAGE_OCCURRENCE('Flat_Washer_Small:1',
'Flat_Washer_Small:1','Flat_Washer_Small:1',#86498,#86501,
'Flat_Washer_Small:1') ;
#728 = NEXT_ASSEMBLY_USAGE_OCCURRENCE('Terminal_Rail:1','Terminal_Rail:1',
'Terminal_Rail:1',#86485,#86486,'Terminal_Rail:1') ;
#729 = NEXT_ASSEMBLY_USAGE_OCCURRENCE('Breadboard:1','Breadboard:1',
'Breadboard:1',#86485,#86494,'Breadboard:1') ;
#730 = NEXT_ASSEMBLY_USAGE_OCCURRENCE('Screw_Washer_Assembly_1:1',
'Screw_Washer_Assembly_1:1','Screw_Washer_Assembly_1:1',#86485,#86495,
'Screw_Washer_Assembly_1:1') ;
#731 = NEXT_ASSEMBLY_USAGE_OCCURRENCE('Screw_Washer_Assembly_2:1',
'Screw_Washer_Assembly_2:1','Screw_Washer_Assembly_2:1',#86485,#86496,
'Screw_Washer_Assembly_2:1') ;
#732 = NEXT_ASSEMBLY_USAGE_OCCURRENCE('Screw_Washer_Assembly_3:1',
'Screw_Washer_Assembly_3:1','Screw_Washer_Assembly_3:1',#86485,#86497,
'Screw_Washer_Assembly_3:1') ;
#733 = NEXT_ASSEMBLY_USAGE_OCCURRENCE('Screw_Washer_Assembly_4:1',
'Screw_Washer_Assembly_4:1','Screw_Washer_Assembly_4:1',#86485,#86498,
'Screw_Washer_Assembly_4:1') ;
#734 = NEXT_ASSEMBLY_USAGE_OCCURRENCE('Case:1','Case:1','Case:1',#86477,#86478,
'Case:1') ;
#735 = NEXT_ASSEMBLY_USAGE_OCCURRENCE('Internals:1','Internals:1',
'Internals:1',#86477,#86485,'Internals:1') ;
#736 = (
BOUNDED_SURFACE()
B_SPLINE_SURFACE(1,2,((#48177,#48178,#48179,#48180,#48181,#48182,#48183,
#48184,#48185,#48186,#48187,#48188,#48189,#48190,#48191,#48192,#48193,#48194,
#48195,#48196,#48197,#48198,#48199,#48200,#48201,#48202,#48203,#48204,#48205,
#48206,#48207,#48208,#48209,#48210,#48211,#48212,#48213,#48214,#48215,#48216,
#48217,#48218,#48219,#48220,#48221,#48222,#48223,#48224,#48225,#48226,#48227,
#48228,#48229,#48230,#48231,#48232,#48233,#48234,#48235,#48236,#48237,#48238,
#48239,#48240,#48241,#48242,#48243,#48244,#48245,#48246,#48247,#48248,#48249,
#48250,#48251,#48252,#48253,#48254,#48255,#48256,#48257,#48258,#48259,#48260,
#48261),(#48262,#48263,#48264,#48265,#48266,#48267,#48268,#48269,#48270,
#48271,#48272,#48273,#48274,#48275,#48276,#48277,#48278,#48279,#48280,#48281,
#48282,#48283,#48284,#48285,#48286,#48287,#48288,#48289,#48290,#48291,#48292,
#48293,#48294,#48295,#48296,#48297,#48298,#48299,#48300,#48301,#48302,#48303,
#48304,#48305,#48306,#48307,#48308,#48309,#48310,#48311,#48312,#48313,#48314,
#48315,#48316,#48317,#48318,#48319,#48320,#48321,#48322,#48323,#48324,#48325,
#48326,#48327,#48328,#48329,#48330,#48331,#48332,#48333,#48334,#48335,#48336,
#48337,#48338,#48339,#48340,#48341,#48342,#48343,#48344,#48345,#48346)),
 .UNSPECIFIED.,.F.,.F.,.F.)
B_SPLINE_SURFACE_WITH_KNOTS((2,2),(3,2,2,2,2,2,2,2,2,2,2,2,2,2,2,2,2,2,
2,2,2,2,2,2,2,2,2,2,2,2,2,2,2,2,2,2,2,2,2,2,2,2,3),(-0.000109059520856525,
1.00010905952086),(-9.68976095313223E-5,0.0238095238095238,0.0476190476190476,
0.0714285714285714,0.0952380952380952,0.119047619047619,0.142857142857143,
0.166666666666667,0.19047619047619,0.214285714285714,0.238095238095238,
0.261904761904762,0.285714285714286,0.30952380952381,0.333333333333333,
0.357142857142857,0.380952380952381,0.404761904761905,0.428571428571429,
0.452380952380952,0.476190476190476,0.5,0.523809523809524,0.547619047619048,
0.571428571428571,0.595238095238095,0.619047619047619,0.642857142857143,
0.666666666666667,0.69047619047619,0.714285714285714,0.738095238095238,
0.761904761904762,0.785714285714286,0.80952380952381,0.833333333333333,
0.857142857142857,0.880952380952381,0.904761904761905,0.928571428571429,
0.952380952380952,0.976190476190476,1.),.UNSPECIFIED.)
GEOMETRIC_REPRESENTATION_ITEM()
RATIONAL_B_SPLINE_SURFACE(((1.00109491061774,0.865480167423768,1.,0.866025403784439,
1.,0.866025403784439,1.,0.866025403784439,1.,0.866025403784439,1.,0.866025403784439,
1.,0.866025403784439,1.,0.866025403784439,1.,0.866025403784439,1.,0.866025403784439,
1.,0.866025403784439,1.,0.866025403784439,1.,0.866025403784439,1.,0.866025403784439,
1.,0.866025403784439,1.,0.866025403784439,1.,0.866025403784439,1.,0.866025403784439,
1.,0.866025403784439,1.,0.866025403784439,1.,0.866025403784439,1.,0.866025403784439,
1.,0.866025403784439,1.,0.866025403784439,1.,0.866025403784439,1.,0.866025403784439,
1.,0.866025403784439,1.,0.866025403784439,1.,0.866025403784439,1.,0.866025403784439,
1.,0.866025403784439,1.,0.866025403784439,1.,0.866025403784439,1.,0.866025403784439,
1.,0.866025403784439,1.,0.866025403784439,1.,0.866025403784439,1.,0.866025403784439,
1.,0.866025403784439,1.,0.866025403784439,1.,0.866025403784439,1.,0.866025403784439,
1.),(1.00109491061774,0.865480167423768,1.,0.866025403784439,1.,0.866025403784439,
1.,0.866025403784439,1.,0.866025403784439,1.,0.866025403784439,1.,0.866025403784439,
1.,0.866025403784439,1.,0.866025403784439,1.,0.866025403784439,1.,0.866025403784439,
1.,0.866025403784439,1.,0.866025403784439,1.,0.866025403784439,1.,0.866025403784439,
1.,0.866025403784439,1.,0.866025403784439,1.,0.866025403784439,1.,0.866025403784439,
1.,0.866025403784439,1.,0.866025403784439,1.,0.866025403784439,1.,0.866025403784439,
1.,0.866025403784439,1.,0.866025403784439,1.,0.866025403784439,1.,0.866025403784439,
1.,0.866025403784439,1.,0.866025403784439,1.,0.866025403784439,1.,0.866025403784439,
1.,0.866025403784439,1.,0.866025403784439,1.,0.866025403784439,1.,0.866025403784439,
1.,0.866025403784439,1.,0.866025403784439,1.,0.866025403784439,1.,0.866025403784439,
1.,0.866025403784439,1.,0.866025403784439,1.,0.866025403784439,1.)))
REPRESENTATION_ITEM('')
SURFACE()
) ;
#737 = (
BOUNDED_SURFACE()
B_SPLINE_SURFACE(1,2,((#48347,#48348,#48349,#48350,#48351,#48352,#48353,
#48354,#48355,#48356,#48357,#48358,#48359,#48360,#48361,#48362,#48363,#48364,
#48365,#48366,#48367,#48368,#48369,#48370,#48371,#48372,#48373,#48374,#48375,
#48376,#48377,#48378,#48379,#48380,#48381,#48382,#48383,#48384,#48385,#48386,
#48387,#48388,#48389,#48390,#48391,#48392,#48393,#48394,#48395,#48396,#48397,
#48398,#48399,#48400,#48401,#48402,#48403,#48404,#48405,#48406,#48407,#48408,
#48409,#48410,#48411,#48412,#48413,#48414,#48415,#48416,#48417,#48418,#48419,
#48420,#48421,#48422,#48423,#48424,#48425,#48426,#48427,#48428,#48429,#48430,
#48431),(#48432,#48433,#48434,#48435,#48436,#48437,#48438,#48439,#48440,
#48441,#48442,#48443,#48444,#48445,#48446,#48447,#48448,#48449,#48450,#48451,
#48452,#48453,#48454,#48455,#48456,#48457,#48458,#48459,#48460,#48461,#48462,
#48463,#48464,#48465,#48466,#48467,#48468,#48469,#48470,#48471,#48472,#48473,
#48474,#48475,#48476,#48477,#48478,#48479,#48480,#48481,#48482,#48483,#48484,
#48485,#48486,#48487,#48488,#48489,#48490,#48491,#48492,#48493,#48494,#48495,
#48496,#48497,#48498,#48499,#48500,#48501,#48502,#48503,#48504,#48505,#48506,
#48507,#48508,#48509,#48510,#48511,#48512,#48513,#48514,#48515,#48516)),
 .UNSPECIFIED.,.F.,.F.,.F.)
B_SPLINE_SURFACE_WITH_KNOTS((2,2),(3,2,2,2,2,2,2,2,2,2,2,2,2,2,2,2,2,2,
2,2,2,2,2,2,2,2,2,2,2,2,2,2,2,2,2,2,2,2,2,2,2,2,3),(-9.75032520683202E-5,
1.),(0.,0.0238095238095238,0.0476190476190476,0.0714285714285714,0.0952380952380952,
0.119047619047619,0.142857142857143,0.166666666666667,0.19047619047619,
0.214285714285714,0.238095238095238,0.261904761904762,0.285714285714286,
0.30952380952381,0.333333333333333,0.357142857142857,0.380952380952381,
0.404761904761905,0.428571428571429,0.452380952380952,0.476190476190476,
0.5,0.523809523809524,0.547619047619048,0.571428571428571,0.595238095238095,
0.619047619047619,0.642857142857143,0.666666666666667,0.69047619047619,
0.714285714285714,0.738095238095238,0.761904761904762,0.785714285714286,
0.80952380952381,0.833333333333333,0.857142857142857,0.880952380952381,
0.904761904761905,0.928571428571429,0.952380952380952,0.976190476190476,
1.),.UNSPECIFIED.)
GEOMETRIC_REPRESENTATION_ITEM()
RATIONAL_B_SPLINE_SURFACE(((1.,0.866025403784439,1.,0.866025403784439,1.,
0.866025403784439,1.,0.866025403784439,1.,0.866025403784439,1.,0.866025403784439,
1.,0.866025403784439,1.,0.866025403784439,1.,0.866025403784439,1.,0.866025403784439,
1.,0.866025403784439,1.,0.866025403784439,1.,0.866025403784439,1.,0.866025403784439,
1.,0.866025403784439,1.,0.866025403784439,1.,0.866025403784439,1.,0.866025403784439,
1.,0.866025403784439,1.,0.866025403784439,1.,0.866025403784439,1.,0.866025403784439,
1.,0.866025403784439,1.,0.866025403784439,1.,0.866025403784439,1.,0.866025403784439,
1.,0.866025403784439,1.,0.866025403784439,1.,0.866025403784439,1.,0.866025403784439,
1.,0.866025403784439,1.,0.866025403784439,1.,0.866025403784439,1.,0.866025403784439,
1.,0.866025403784439,1.,0.866025403784439,1.,0.866025403784439,1.,0.866025403784439,
1.,0.866025403784439,1.,0.866025403784439,1.,0.866025403784439,1.,0.866025403784439,
1.),(1.,0.866025403784439,1.,0.866025403784439,1.,0.866025403784439,1.,
0.866025403784439,1.,0.866025403784439,1.,0.866025403784439,1.,0.866025403784439,
1.,0.866025403784439,1.,0.866025403784439,1.,0.866025403784439,1.,0.866025403784439,
1.,0.866025403784439,1.,0.866025403784439,1.,0.866025403784439,1.,0.866025403784439,
1.,0.866025403784439,1.,0.866025403784439,1.,0.866025403784439,1.,0.866025403784439,
1.,0.866025403784439,1.,0.866025403784439,1.,0.866025403784439,1.,0.866025403784439,
1.,0.866025403784439,1.,0.866025403784439,1.,0.866025403784439,1.,0.866025403784439,
1.,0.866025403784439,1.,0.866025403784439,1.,0.866025403784439,1.,0.866025403784439,
1.,0.866025403784439,1.,0.866025403784439,1.,0.866025403784439,1.,0.866025403784439,
1.,0.866025403784439,1.,0.866025403784439,1.,0.866025403784439,1.,0.866025403784439,
1.,0.866025403784439,1.,0.866025403784439,1.,0.866025403784439,1.)))
REPRESENTATION_ITEM('')
SURFACE()
) ;
#738 = (
BOUNDED_SURFACE()
B_SPLINE_SURFACE(1,2,((#49791,#49792,#49793,#49794,#49795,#49796,#49797,
#49798,#49799,#49800,#49801,#49802,#49803,#49804,#49805,#49806,#49807,#49808,
#49809,#49810,#49811,#49812,#49813,#49814,#49815,#49816,#49817,#49818,#49819,
#49820,#49821,#49822,#49823,#49824,#49825,#49826,#49827,#49828,#49829,#49830,
#49831,#49832,#49833,#49834,#49835,#49836,#49837,#49838,#49839,#49840,#49841,
#49842,#49843,#49844,#49845,#49846,#49847,#49848,#49849,#49850,#49851,#49852,
#49853,#49854,#49855,#49856,#49857,#49858,#49859,#49860,#49861,#49862,#49863,
#49864,#49865,#49866,#49867,#49868,#49869,#49870,#49871,#49872,#49873,#49874,
#49875,#49876,#49877,#49878,#49879,#49880,#49881,#49882,#49883,#49884,#49885,
#49886,#49887,#49888,#49889,#49890,#49891,#49892,#49893,#49894,#49895,#49896,
#49897),(#49898,#49899,#49900,#49901,#49902,#49903,#49904,#49905,#49906,
#49907,#49908,#49909,#49910,#49911,#49912,#49913,#49914,#49915,#49916,#49917,
#49918,#49919,#49920,#49921,#49922,#49923,#49924,#49925,#49926,#49927,#49928,
#49929,#49930,#49931,#49932,#49933,#49934,#49935,#49936,#49937,#49938,#49939,
#49940,#49941,#49942,#49943,#49944,#49945,#49946,#49947,#49948,#49949,#49950,
#49951,#49952,#49953,#49954,#49955,#49956,#49957,#49958,#49959,#49960,#49961,
#49962,#49963,#49964,#49965,#49966,#49967,#49968,#49969,#49970,#49971,#49972,
#49973,#49974,#49975,#49976,#49977,#49978,#49979,#49980,#49981,#49982,#49983,
#49984,#49985,#49986,#49987,#49988,#49989,#49990,#49991,#49992,#49993,#49994,
#49995,#49996,#49997,#49998,#49999,#50000,#50001,#50002,#50003,#50004)),
 .UNSPECIFIED.,.F.,.F.,.F.)
B_SPLINE_SURFACE_WITH_KNOTS((2,2),(3,2,2,2,2,2,2,2,2,2,2,2,2,2,2,2,2,2,
2,2,2,2,2,2,2,2,2,2,2,2,2,2,2,2,2,2,2,2,2,2,2,2,2,2,2,2,2,2,2,2,2,2,2,3),
(0.,1.),(0.,0.0185185185185185,0.037037037037037,0.0555555555555556,0.0740740740740741,
0.0925925925925926,0.111111111111111,0.12962962962963,0.148148148148148,
0.166666666666667,0.185185185185185,0.203703703703704,0.222222222222222,
0.240740740740741,0.259259259259259,0.277777777777778,0.296296296296296,
0.314814814814815,0.333333333333333,0.351851851851852,0.37037037037037,
0.388888888888889,0.407407407407407,0.425925925925926,0.444444444444444,
0.462962962962963,0.481481481481481,0.5,0.518518518518518,0.537037037037037,
0.555555555555556,0.574074074074074,0.592592592592593,0.611111111111111,
0.62962962962963,0.648148148148148,0.666666666666667,0.685185185185185,
0.703703703703704,0.722222222222222,0.740740740740741,0.759259259259259,
0.777777777777778,0.796296296296296,0.814814814814815,0.833333333333333,
0.851851851851852,0.87037037037037,0.888888888888889,0.907407407407407,
0.925925925925926,0.944444444444444,0.962962962962963,0.972222222222224),
 .UNSPECIFIED.)
GEOMETRIC_REPRESENTATION_ITEM()
RATIONAL_B_SPLINE_SURFACE(((1.,0.866025403784439,1.,0.866025403784439,1.,
0.866025403784439,1.,0.866025403784439,1.,0.866025403784439,1.,0.866025403784439,
1.,0.866025403784439,1.,0.866025403784439,1.,0.866025403784439,1.,0.866025403784439,
1.,0.866025403784439,1.,0.866025403784439,1.,0.866025403784439,1.,0.866025403784439,
1.,0.866025403784439,1.,0.866025403784439,1.,0.866025403784439,1.,0.866025403784439,
1.,0.866025403784439,1.,0.866025403784439,1.,0.866025403784439,1.,0.866025403784439,
1.,0.866025403784439,1.,0.866025403784439,1.,0.866025403784439,1.,0.866025403784439,
1.,0.866025403784439,1.,0.866025403784439,1.,0.866025403784439,1.,0.866025403784439,
1.,0.866025403784439,1.,0.866025403784439,1.,0.866025403784439,1.,0.866025403784439,
1.,0.866025403784439,1.,0.866025403784439,1.,0.866025403784439,1.,0.866025403784439,
1.,0.866025403784439,1.,0.866025403784439,1.,0.866025403784439,1.,0.866025403784439,
1.,0.866025403784439,1.,0.866025403784439,1.,0.866025403784439,1.,0.866025403784439,
1.,0.866025403784439,1.,0.866025403784439,1.,0.866025403784439,1.,0.866025403784439,
1.,0.866025403784439,1.,0.866025403784439,1.,0.933012701892203,0.933012701892219),
(1.,0.866025403784439,1.,0.866025403784439,1.,0.866025403784439,1.,0.866025403784439,
1.,0.866025403784439,1.,0.866025403784439,1.,0.866025403784439,1.,0.866025403784439,
1.,0.866025403784439,1.,0.866025403784439,1.,0.866025403784439,1.,0.866025403784439,
1.,0.866025403784439,1.,0.866025403784439,1.,0.866025403784439,1.,0.866025403784439,
1.,0.866025403784439,1.,0.866025403784439,1.,0.866025403784439,1.,0.866025403784439,
1.,0.866025403784439,1.,0.866025403784439,1.,0.866025403784439,1.,0.866025403784439,
1.,0.866025403784439,1.,0.866025403784439,1.,0.866025403784439,1.,0.866025403784439,
1.,0.866025403784439,1.,0.866025403784439,1.,0.866025403784439,1.,0.866025403784439,
1.,0.866025403784439,1.,0.866025403784439,1.,0.866025403784439,1.,0.866025403784439,
1.,0.866025403784439,1.,0.866025403784439,1.,0.866025403784439,1.,0.866025403784439,
1.,0.866025403784439,1.,0.866025403784439,1.,0.866025403784439,1.,0.866025403784439,
1.,0.866025403784439,1.,0.866025403784439,1.,0.866025403784439,1.,0.866025403784439,
1.,0.866025403784439,1.,0.866025403784439,1.,0.866025403784439,1.,0.866025403784439,
1.,0.933012701892203,0.933012701892219)))
REPRESENTATION_ITEM('')
SURFACE()
) ;
#739 = (
BOUNDED_SURFACE()
B_SPLINE_SURFACE(1,2,((#50005,#50006,#50007,#50008,#50009,#50010,#50011,
#50012,#50013,#50014,#50015,#50016,#50017,#50018,#50019,#50020,#50021,#50022,
#50023,#50024,#50025,#50026,#50027,#50028,#50029,#50030,#50031,#50032,#50033,
#50034,#50035,#50036,#50037,#50038,#50039,#50040,#50041,#50042,#50043,#50044,
#50045,#50046,#50047,#50048,#50049,#50050,#50051,#50052,#50053,#50054,#50055,
#50056,#50057,#50058,#50059,#50060,#50061,#50062,#50063,#50064,#50065,#50066,
#50067,#50068,#50069,#50070,#50071,#50072,#50073,#50074,#50075,#50076,#50077,
#50078,#50079,#50080,#50081,#50082,#50083,#50084,#50085,#50086,#50087,#50088,
#50089,#50090,#50091,#50092,#50093,#50094,#50095,#50096,#50097,#50098,#50099,
#50100,#50101,#50102,#50103,#50104,#50105,#50106,#50107,#50108,#50109,#50110,
#50111),(#50112,#50113,#50114,#50115,#50116,#50117,#50118,#50119,#50120,
#50121,#50122,#50123,#50124,#50125,#50126,#50127,#50128,#50129,#50130,#50131,
#50132,#50133,#50134,#50135,#50136,#50137,#50138,#50139,#50140,#50141,#50142,
#50143,#50144,#50145,#50146,#50147,#50148,#50149,#50150,#50151,#50152,#50153,
#50154,#50155,#50156,#50157,#50158,#50159,#50160,#50161,#50162,#50163,#50164,
#50165,#50166,#50167,#50168,#50169,#50170,#50171,#50172,#50173,#50174,#50175,
#50176,#50177,#50178,#50179,#50180,#50181,#50182,#50183,#50184,#50185,#50186,
#50187,#50188,#50189,#50190,#50191,#50192,#50193,#50194,#50195,#50196,#50197,
#50198,#50199,#50200,#50201,#50202,#50203,#50204,#50205,#50206,#50207,#50208,
#50209,#50210,#50211,#50212,#50213,#50214,#50215,#50216,#50217,#50218)),
 .UNSPECIFIED.,.F.,.F.,.F.)
B_SPLINE_SURFACE_WITH_KNOTS((2,2),(3,2,2,2,2,2,2,2,2,2,2,2,2,2,2,2,2,2,
2,2,2,2,2,2,2,2,2,2,2,2,2,2,2,2,2,2,2,2,2,2,2,2,2,2,2,2,2,2,2,2,2,2,2,3),
(0.,1.),(0.,0.0185185185185185,0.037037037037037,0.0555555555555556,0.0740740740740741,
0.0925925925925926,0.111111111111111,0.12962962962963,0.148148148148148,
0.166666666666667,0.185185185185185,0.203703703703704,0.222222222222222,
0.240740740740741,0.259259259259259,0.277777777777778,0.296296296296296,
0.314814814814815,0.333333333333333,0.351851851851852,0.37037037037037,
0.388888888888889,0.407407407407407,0.425925925925926,0.444444444444444,
0.462962962962963,0.481481481481481,0.5,0.518518518518518,0.537037037037037,
0.555555555555556,0.574074074074074,0.592592592592593,0.611111111111111,
0.62962962962963,0.648148148148148,0.666666666666667,0.685185185185185,
0.703703703703704,0.722222222222222,0.740740740740741,0.759259259259259,
0.777777777777778,0.796296296296296,0.814814814814815,0.833333333333333,
0.851851851851852,0.87037037037037,0.888888888888889,0.907407407407407,
0.925925925925926,0.944444444444444,0.962962962962963,0.972222222222225),
 .UNSPECIFIED.)
GEOMETRIC_REPRESENTATION_ITEM()
RATIONAL_B_SPLINE_SURFACE(((1.,0.866025403784439,1.,0.866025403784439,1.,
0.866025403784439,1.,0.866025403784439,1.,0.866025403784439,1.,0.866025403784439,
1.,0.866025403784439,1.,0.866025403784439,1.,0.866025403784439,1.,0.866025403784439,
1.,0.866025403784439,1.,0.866025403784439,1.,0.866025403784439,1.,0.866025403784439,
1.,0.866025403784439,1.,0.866025403784439,1.,0.866025403784439,1.,0.866025403784439,
1.,0.866025403784439,1.,0.866025403784439,1.,0.866025403784439,1.,0.866025403784439,
1.,0.866025403784439,1.,0.866025403784439,1.,0.866025403784439,1.,0.866025403784439,
1.,0.866025403784439,1.,0.866025403784439,1.,0.866025403784439,1.,0.866025403784439,
1.,0.866025403784439,1.,0.866025403784439,1.,0.866025403784439,1.,0.866025403784439,
1.,0.866025403784439,1.,0.866025403784439,1.,0.866025403784439,1.,0.866025403784439,
1.,0.866025403784439,1.,0.866025403784439,1.,0.866025403784439,1.,0.866025403784439,
1.,0.866025403784439,1.,0.866025403784439,1.,0.866025403784439,1.,0.866025403784439,
1.,0.866025403784439,1.,0.866025403784439,1.,0.866025403784439,1.,0.866025403784439,
1.,0.866025403784439,1.,0.866025403784439,1.,0.933012701892203,0.933012701892219),
(1.,0.866025403784439,1.,0.866025403784439,1.,0.866025403784439,1.,0.866025403784439,
1.,0.866025403784439,1.,0.866025403784439,1.,0.866025403784439,1.,0.866025403784439,
1.,0.866025403784439,1.,0.866025403784439,1.,0.866025403784439,1.,0.866025403784439,
1.,0.866025403784439,1.,0.866025403784439,1.,0.866025403784439,1.,0.866025403784439,
1.,0.866025403784439,1.,0.866025403784439,1.,0.866025403784439,1.,0.866025403784439,
1.,0.866025403784439,1.,0.866025403784439,1.,0.866025403784439,1.,0.866025403784439,
1.,0.866025403784439,1.,0.866025403784439,1.,0.866025403784439,1.,0.866025403784439,
1.,0.866025403784439,1.,0.866025403784439,1.,0.866025403784439,1.,0.866025403784439,
1.,0.866025403784439,1.,0.866025403784439,1.,0.866025403784439,1.,0.866025403784439,
1.,0.866025403784439,1.,0.866025403784439,1.,0.866025403784439,1.,0.866025403784439,
1.,0.866025403784439,1.,0.866025403784439,1.,0.866025403784439,1.,0.866025403784439,
1.,0.866025403784439,1.,0.866025403784439,1.,0.866025403784439,1.,0.866025403784439,
1.,0.866025403784439,1.,0.866025403784439,1.,0.866025403784439,1.,0.866025403784439,
1.,0.933012701892203,0.933012701892219)))
REPRESENTATION_ITEM('')
SURFACE()
) ;
#740 = (
BOUNDED_SURFACE()
B_SPLINE_SURFACE(2,2,((#67035,#67036,#67037),(#67038,#67039,#67040),(#67041,
#67042,#67043)),.UNSPECIFIED.,.F.,.F.,.F.)
B_SPLINE_SURFACE_WITH_KNOTS((3,3),(3,3),(-1.5707963267962,1.31181440870059E-14),
(-1.57079632679766,2.95313754417746E-12),.UNSPECIFIED.)
GEOMETRIC_REPRESENTATION_ITEM()
RATIONAL_B_SPLINE_SURFACE(((1.,0.707106781184525,1.),(0.707106781186029,
0.499999999998204,0.707106781186029),(1.,0.707106781184525,1.)))
REPRESENTATION_ITEM('')
SURFACE()
) ;
#741 = (
BOUNDED_SURFACE()
B_SPLINE_SURFACE(2,2,((#67047,#67048,#67049),(#67050,#67051,#67052),(#67053,
#67054,#67055)),.UNSPECIFIED.,.F.,.F.,.F.)
B_SPLINE_SURFACE_WITH_KNOTS((3,3),(3,3),(-1.38839876682605E-15,1.57079632679588),
(1.57079632679424,3.14159265359081),.UNSPECIFIED.)
GEOMETRIC_REPRESENTATION_ITEM()
RATIONAL_B_SPLINE_SURFACE(((1.,0.707106781185957,1.),(0.707106781186211,
0.499999999999345,0.707106781186211),(1.,0.707106781185957,1.)))
REPRESENTATION_ITEM('')
SURFACE()
) ;
#742 = (
BOUNDED_SURFACE()
B_SPLINE_SURFACE(2,2,((#67066,#67067,#67068),(#67069,#67070,#67071),(#67072,
#67073,#67074)),.UNSPECIFIED.,.F.,.F.,.F.)
B_SPLINE_SURFACE_WITH_KNOTS((3,3),(3,3),(-3.21499456677232E-13,1.57079632679539),
(-7.36310365920222E-13,1.57079632679562),.UNSPECIFIED.)
GEOMETRIC_REPRESENTATION_ITEM()
RATIONAL_B_SPLINE_SURFACE(((1.,0.707106781186032,1.),(0.707106781186293,
0.499999999999455,0.707106781186293),(1.,0.707106781186032,1.)))
REPRESENTATION_ITEM('')
SURFACE()
) ;
#743 = (
BOUNDED_SURFACE()
B_SPLINE_SURFACE(2,2,((#67078,#67079,#67080),(#67081,#67082,#67083),(#67084,
#67085,#67086)),.UNSPECIFIED.,.F.,.F.,.F.)
B_SPLINE_SURFACE_WITH_KNOTS((3,3),(3,3),(-1.57079632679451,6.78283756875461E-13),
(-3.14159265358933,-1.57079632679533),.UNSPECIFIED.)
GEOMETRIC_REPRESENTATION_ITEM()
RATIONAL_B_SPLINE_SURFACE(((1.,0.707106781186867,1.),(0.70710678118647,
0.500000000000171,0.70710678118647),(1.,0.707106781186867,1.)))
REPRESENTATION_ITEM('')
SURFACE()
) ;
#744 = (
BOUNDED_SURFACE()
B_SPLINE_SURFACE(1,2,((#76706,#76707,#76708,#76709,#76710,#76711,#76712,
#76713,#76714,#76715,#76716,#76717,#76718,#76719,#76720,#76721,#76722,#76723,
#76724,#76725,#76726,#76727,#76728,#76729,#76730,#76731,#76732,#76733,#76734,
#76735,#76736,#76737,#76738,#76739,#76740,#76741,#76742,#76743,#76744,#76745,
#76746,#76747,#76748,#76749,#76750,#76751,#76752,#76753,#76754,#76755,#76756,
#76757,#76758,#76759,#76760,#76761,#76762,#76763,#76764,#76765,#76766,#76767,
#76768,#76769,#76770,#76771,#76772,#76773,#76774,#76775,#76776,#76777,#76778,
#76779,#76780,#76781,#76782,#76783,#76784,#76785,#76786,#76787,#76788,#76789,
#76790,#76791,#76792,#76793,#76794,#76795,#76796,#76797,#76798,#76799,#76800,
#76801,#76802,#76803,#76804,#76805,#76806,#76807,#76808,#76809,#76810,#76811,
#76812,#76813,#76814,#76815,#76816,#76817,#76818,#76819,#76820,#76821,#76822,
#76823,#76824,#76825,#76826,#76827,#76828,#76829,#76830,#76831,#76832,#76833,
#76834,#76835,#76836,#76837,#76838,#76839,#76840,#76841,#76842,#76843,#76844,
#76845,#76846,#76847,#76848,#76849,#76850),(#76851,#76852,#76853,#76854,
#76855,#76856,#76857,#76858,#76859,#76860,#76861,#76862,#76863,#76864,#76865,
#76866,#76867,#76868,#76869,#76870,#76871,#76872,#76873,#76874,#76875,#76876,
#76877,#76878,#76879,#76880,#76881,#76882,#76883,#76884,#76885,#76886,#76887,
#76888,#76889,#76890,#76891,#76892,#76893,#76894,#76895,#76896,#76897,#76898,
#76899,#76900,#76901,#76902,#76903,#76904,#76905,#76906,#76907,#76908,#76909,
#76910,#76911,#76912,#76913,#76914,#76915,#76916,#76917,#76918,#76919,#76920,
#76921,#76922,#76923,#76924,#76925,#76926,#76927,#76928,#76929,#76930,#76931,
#76932,#76933,#76934,#76935,#76936,#76937,#76938,#76939,#76940,#76941,#76942,
#76943,#76944,#76945,#76946,#76947,#76948,#76949,#76950,#76951,#76952,#76953,
#76954,#76955,#76956,#76957,#76958,#76959,#76960,#76961,#76962,#76963,#76964,
#76965,#76966,#76967,#76968,#76969,#76970,#76971,#76972,#76973,#76974,#76975,
#76976,#76977,#76978,#76979,#76980,#76981,#76982,#76983,#76984,#76985,#76986,
#76987,#76988,#76989,#76990,#76991,#76992,#76993,#76994,#76995),(#76996,
#76997,#76998,#76999,#77000,#77001,#77002,#77003,#77004,#77005,#77006,#77007,
#77008,#77009,#77010,#77011,#77012,#77013,#77014,#77015,#77016,#77017,#77018,
#77019,#77020,#77021,#77022,#77023,#77024,#77025,#77026,#77027,#77028,#77029,
#77030,#77031,#77032,#77033,#77034,#77035,#77036,#77037,#77038,#77039,#77040,
#77041,#77042,#77043,#77044,#77045,#77046,#77047,#77048,#77049,#77050,#77051,
#77052,#77053,#77054,#77055,#77056,#77057,#77058,#77059,#77060,#77061,#77062,
#77063,#77064,#77065,#77066,#77067,#77068,#77069,#77070,#77071,#77072,#77073,
#77074,#77075,#77076,#77077,#77078,#77079,#77080,#77081,#77082,#77083,#77084,
#77085,#77086,#77087,#77088,#77089,#77090,#77091,#77092,#77093,#77094,#77095,
#77096,#77097,#77098,#77099,#77100,#77101,#77102,#77103,#77104,#77105,#77106,
#77107,#77108,#77109,#77110,#77111,#77112,#77113,#77114,#77115,#77116,#77117,
#77118,#77119,#77120,#77121,#77122,#77123,#77124,#77125,#77126,#77127,#77128,
#77129,#77130,#77131,#77132,#77133,#77134,#77135,#77136,#77137,#77138,#77139,
#77140),(#77141,#77142,#77143,#77144,#77145,#77146,#77147,#77148,#77149,
#77150,#77151,#77152,#77153,#77154,#77155,#77156,#77157,#77158,#77159,#77160,
#77161,#77162,#77163,#77164,#77165,#77166,#77167,#77168,#77169,#77170,#77171,
#77172,#77173,#77174,#77175,#77176,#77177,#77178,#77179,#77180,#77181,#77182,
#77183,#77184,#77185,#77186,#77187,#77188,#77189,#77190,#77191,#77192,#77193,
#77194,#77195,#77196,#77197,#77198,#77199,#77200,#77201,#77202,#77203,#77204,
#77205,#77206,#77207,#77208,#77209,#77210,#77211,#77212,#77213,#77214,#77215,
#77216,#77217,#77218,#77219,#77220,#77221,#77222,#77223,#77224,#77225,#77226,
#77227,#77228,#77229,#77230,#77231,#77232,#77233,#77234,#77235,#77236,#77237,
#77238,#77239,#77240,#77241,#77242,#77243,#77244,#77245,#77246,#77247,#77248,
#77249,#77250,#77251,#77252,#77253,#77254,#77255,#77256,#77257,#77258,#77259,
#77260,#77261,#77262,#77263,#77264,#77265,#77266,#77267,#77268,#77269,#77270,
#77271,#77272,#77273,#77274,#77275,#77276,#77277,#77278,#77279,#77280,#77281,
#77282,#77283,#77284,#77285)),.UNSPECIFIED.,.F.,.F.,.F.)
B_SPLINE_SURFACE_WITH_KNOTS((2,1,1,2),(3,2,2,2,2,2,2,2,2,2,2,2,2,2,2,2,
2,2,2,2,2,2,2,2,2,2,2,2,2,2,2,2,2,2,2,2,2,2,2,2,2,2,2,2,2,2,2,2,2,2,2,2,
2,2,2,2,2,2,2,2,2,2,2,2,2,2,2,2,2,2,2,2,3),(-5.32860868657006,0.,1.,2.58924025826637),
(0.,0.0138888888888889,0.0277777777777778,0.0416666666666667,0.0555555555555556,
0.0694444444444444,0.0833333333333333,0.0972222222222222,0.111111111111111,
0.125,0.138888888888889,0.152777777777778,0.166666666666667,0.180555555555556,
0.194444444444444,0.208333333333333,0.222222222222222,0.236111111111111,
0.25,0.263888888888889,0.277777777777778,0.291666666666667,0.305555555555556,
0.319444444444444,0.333333333333333,0.347222222222222,0.361111111111111,
0.375,0.388888888888889,0.402777777777778,0.416666666666667,0.430555555555556,
0.444444444444444,0.458333333333333,0.472222222222222,0.486111111111111,
0.5,0.513888888888889,0.527777777777778,0.541666666666667,0.555555555555556,
0.569444444444444,0.583333333333333,0.597222222222222,0.611111111111111,
0.625,0.638888888888889,0.652777777777778,0.666666666666667,0.680555555555556,
0.694444444444444,0.708333333333333,0.722222222222222,0.736111111111111,
0.75,0.763888888888889,0.777777777777778,0.791666666666667,0.805555555555556,
0.819444444444444,0.833333333333333,0.847222222222222,0.861111111111111,
0.875,0.888888888888889,0.902777777777778,0.916666666666667,0.930555555555556,
0.944444444444444,0.958333333333333,0.972222222222222,0.986111111111111,
1.),.UNSPECIFIED.)
GEOMETRIC_REPRESENTATION_ITEM()
RATIONAL_B_SPLINE_SURFACE(((1.,0.923879532511287,1.,0.923879532511287,1.,
0.923879532511287,1.,0.923879532511287,1.,0.923879532511287,1.,0.923879532511287,
1.,0.923879532511287,1.,0.923879532511287,1.,0.923879532511287,1.,0.923879532511287,
1.,0.923879532511287,1.,0.923879532511287,1.,0.923879532511287,1.,0.923879532511287,
1.,0.923879532511287,1.,0.923879532511287,1.,0.923879532511287,1.,0.923879532511287,
1.,0.923879532511287,1.,0.923879532511287,1.,0.923879532511287,1.,0.923879532511287,
1.,0.923879532511287,1.,0.923879532511287,1.,0.923879532511287,1.,0.923879532511287,
1.,0.923879532511287,1.,0.923879532511287,1.,0.923879532511287,1.,0.923879532511287,
1.,0.923879532511287,1.,0.923879532511287,1.,0.923879532511287,1.,0.923879532511287,
1.,0.923879532511287,1.,0.923879532511287,1.,0.923879532511287,1.,0.923879532511287,
1.,0.923879532511287,1.,0.923879532511287,1.,0.923879532511287,1.,0.923879532511287,
1.,0.923879532511287,1.,0.923879532511287,1.,0.923879532511287,1.,0.923879532511287,
1.,0.923879532511287,1.,0.923879532511287,1.,0.923879532511287,1.,0.923879532511287,
1.,0.923879532511287,1.,0.923879532511287,1.,0.923879532511287,1.,0.923879532511287,
1.,0.923879532511287,1.,0.923879532511287,1.,0.923879532511287,1.,0.923879532511287,
1.,0.923879532511287,1.,0.923879532511287,1.,0.923879532511287,1.,0.923879532511287,
1.,0.923879532511287,1.,0.923879532511287,1.,0.923879532511287,1.,0.923879532511287,
1.,0.923879532511287,1.,0.923879532511287,1.,0.923879532511287,1.,0.923879532511287,
1.,0.923879532511287,1.,0.923879532511287,1.),(1.,0.923879532511287,1.,
0.923879532511287,1.,0.923879532511287,1.,0.923879532511287,1.,0.923879532511287,
1.,0.923879532511287,1.,0.923879532511287,1.,0.923879532511287,1.,0.923879532511287,
1.,0.923879532511287,1.,0.923879532511287,1.,0.923879532511287,1.,0.923879532511287,
1.,0.923879532511287,1.,0.923879532511287,1.,0.923879532511287,1.,0.923879532511287,
1.,0.923879532511287,1.,0.923879532511287,1.,0.923879532511287,1.,0.923879532511287,
1.,0.923879532511287,1.,0.923879532511287,1.,0.923879532511287,1.,0.923879532511287,
1.,0.923879532511287,1.,0.923879532511287,1.,0.923879532511287,1.,0.923879532511287,
1.,0.923879532511287,1.,0.923879532511287,1.,0.923879532511287,1.,0.923879532511287,
1.,0.923879532511287,1.,0.923879532511287,1.,0.923879532511287,1.,0.923879532511287,
1.,0.923879532511287,1.,0.923879532511287,1.,0.923879532511287,1.,0.923879532511287,
1.,0.923879532511287,1.,0.923879532511287,1.,0.923879532511287,1.,0.923879532511287,
1.,0.923879532511287,1.,0.923879532511287,1.,0.923879532511287,1.,0.923879532511287,
1.,0.923879532511287,1.,0.923879532511287,1.,0.923879532511287,1.,0.923879532511287,
1.,0.923879532511287,1.,0.923879532511287,1.,0.923879532511287,1.,0.923879532511287,
1.,0.923879532511287,1.,0.923879532511287,1.,0.923879532511287,1.,0.923879532511287,
1.,0.923879532511287,1.,0.923879532511287,1.,0.923879532511287,1.,0.923879532511287,
1.,0.923879532511287,1.,0.923879532511287,1.,0.923879532511287,1.,0.923879532511287,
1.,0.923879532511287,1.,0.923879532511287,1.,0.923879532511287,1.),(1.,
0.923879532511287,1.,0.923879532511287,1.,0.923879532511287,1.,0.923879532511287,
1.,0.923879532511287,1.,0.923879532511287,1.,0.923879532511287,1.,0.923879532511287,
1.,0.923879532511287,1.,0.923879532511287,1.,0.923879532511287,1.,0.923879532511287,
1.,0.923879532511287,1.,0.923879532511287,1.,0.923879532511287,1.,0.923879532511287,
1.,0.923879532511287,1.,0.923879532511287,1.,0.923879532511287,1.,0.923879532511287,
1.,0.923879532511287,1.,0.923879532511287,1.,0.923879532511287,1.,0.923879532511287,
1.,0.923879532511287,1.,0.923879532511287,1.,0.923879532511287,1.,0.923879532511287,
1.,0.923879532511287,1.,0.923879532511287,1.,0.923879532511287,1.,0.923879532511287,
1.,0.923879532511287,1.,0.923879532511287,1.,0.923879532511287,1.,0.923879532511287,
1.,0.923879532511287,1.,0.923879532511287,1.,0.923879532511287,1.,0.923879532511287,
1.,0.923879532511287,1.,0.923879532511287,1.,0.923879532511287,1.,0.923879532511287,
1.,0.923879532511287,1.,0.923879532511287,1.,0.923879532511287,1.,0.923879532511287,
1.,0.923879532511287,1.,0.923879532511287,1.,0.923879532511287,1.,0.923879532511287,
1.,0.923879532511287,1.,0.923879532511287,1.,0.923879532511287,1.,0.923879532511287,
1.,0.923879532511287,1.,0.923879532511287,1.,0.923879532511287,1.,0.923879532511287,
1.,0.923879532511287,1.,0.923879532511287,1.,0.923879532511287,1.,0.923879532511287,
1.,0.923879532511287,1.,0.923879532511287,1.,0.923879532511287,1.,0.923879532511287,
1.,0.923879532511287,1.,0.923879532511287,1.,0.923879532511287,1.,0.923879532511287,
1.),(1.,0.923879532511287,1.,0.923879532511287,1.,0.923879532511287,1.,
0.923879532511287,1.,0.923879532511287,1.,0.923879532511287,1.,0.923879532511287,
1.,0.923879532511287,1.,0.923879532511287,1.,0.923879532511287,1.,0.923879532511287,
1.,0.923879532511287,1.,0.923879532511287,1.,0.923879532511287,1.,0.923879532511287,
1.,0.923879532511287,1.,0.923879532511287,1.,0.923879532511287,1.,0.923879532511287,
1.,0.923879532511287,1.,0.923879532511287,1.,0.923879532511287,1.,0.923879532511287,
1.,0.923879532511287,1.,0.923879532511287,1.,0.923879532511287,1.,0.923879532511287,
1.,0.923879532511287,1.,0.923879532511287,1.,0.923879532511287,1.,0.923879532511287,
1.,0.923879532511287,1.,0.923879532511287,1.,0.923879532511287,1.,0.923879532511287,
1.,0.923879532511287,1.,0.923879532511287,1.,0.923879532511287,1.,0.923879532511287,
1.,0.923879532511287,1.,0.923879532511287,1.,0.923879532511287,1.,0.923879532511287,
1.,0.923879532511287,1.,0.923879532511287,1.,0.923879532511287,1.,0.923879532511287,
1.,0.923879532511287,1.,0.923879532511287,1.,0.923879532511287,1.,0.923879532511287,
1.,0.923879532511287,1.,0.923879532511287,1.,0.923879532511287,1.,0.923879532511287,
1.,0.923879532511287,1.,0.923879532511287,1.,0.923879532511287,1.,0.923879532511287,
1.,0.923879532511287,1.,0.923879532511287,1.,0.923879532511287,1.,0.923879532511287,
1.,0.923879532511287,1.,0.923879532511287,1.,0.923879532511287,1.,0.923879532511287,
1.,0.923879532511287,1.,0.923879532511287,1.,0.923879532511287,1.,0.923879532511287,
1.,0.923879532511287,1.)))
REPRESENTATION_ITEM('')
SURFACE()
) ;
#745 = (
BOUNDED_SURFACE()
B_SPLINE_SURFACE(1,2,((#78487,#78488,#78489,#78490,#78491,#78492,#78493,
#78494,#78495,#78496,#78497,#78498,#78499,#78500,#78501,#78502,#78503,#78504,
#78505,#78506,#78507,#78508,#78509,#78510,#78511,#78512,#78513,#78514,#78515,
#78516,#78517,#78518,#78519,#78520,#78521,#78522,#78523,#78524,#78525,#78526,
#78527,#78528,#78529,#78530,#78531,#78532,#78533,#78534,#78535,#78536,#78537,
#78538,#78539,#78540,#78541,#78542,#78543,#78544,#78545,#78546,#78547,#78548,
#78549,#78550,#78551,#78552,#78553,#78554,#78555,#78556,#78557,#78558,#78559,
#78560,#78561,#78562,#78563,#78564,#78565,#78566,#78567,#78568,#78569,#78570,
#78571,#78572,#78573,#78574,#78575,#78576,#78577,#78578,#78579,#78580,#78581,
#78582,#78583,#78584,#78585,#78586,#78587,#78588,#78589,#78590,#78591,#78592,
#78593,#78594,#78595,#78596,#78597,#78598,#78599,#78600,#78601,#78602,#78603,
#78604,#78605,#78606,#78607,#78608,#78609,#78610,#78611,#78612,#78613,#78614,
#78615,#78616,#78617,#78618,#78619,#78620,#78621,#78622,#78623,#78624,#78625,
#78626,#78627,#78628,#78629,#78630,#78631),(#78632,#78633,#78634,#78635,
#78636,#78637,#78638,#78639,#78640,#78641,#78642,#78643,#78644,#78645,#78646,
#78647,#78648,#78649,#78650,#78651,#78652,#78653,#78654,#78655,#78656,#78657,
#78658,#78659,#78660,#78661,#78662,#78663,#78664,#78665,#78666,#78667,#78668,
#78669,#78670,#78671,#78672,#78673,#78674,#78675,#78676,#78677,#78678,#78679,
#78680,#78681,#78682,#78683,#78684,#78685,#78686,#78687,#78688,#78689,#78690,
#78691,#78692,#78693,#78694,#78695,#78696,#78697,#78698,#78699,#78700,#78701,
#78702,#78703,#78704,#78705,#78706,#78707,#78708,#78709,#78710,#78711,#78712,
#78713,#78714,#78715,#78716,#78717,#78718,#78719,#78720,#78721,#78722,#78723,
#78724,#78725,#78726,#78727,#78728,#78729,#78730,#78731,#78732,#78733,#78734,
#78735,#78736,#78737,#78738,#78739,#78740,#78741,#78742,#78743,#78744,#78745,
#78746,#78747,#78748,#78749,#78750,#78751,#78752,#78753,#78754,#78755,#78756,
#78757,#78758,#78759,#78760,#78761,#78762,#78763,#78764,#78765,#78766,#78767,
#78768,#78769,#78770,#78771,#78772,#78773,#78774,#78775,#78776)),
 .UNSPECIFIED.,.F.,.F.,.F.)
B_SPLINE_SURFACE_WITH_KNOTS((2,2),(3,2,2,2,2,2,2,2,2,2,2,2,2,2,2,2,2,2,
2,2,2,2,2,2,2,2,2,2,2,2,2,2,2,2,2,2,2,2,2,2,2,2,2,2,2,2,2,2,2,2,2,2,2,2,
2,2,2,2,2,2,2,2,2,2,2,2,2,2,2,2,2,2,3),(0.,1.00005636984077),(0.,0.0138888888888889,
0.0277777777777778,0.0416666666666667,0.0555555555555556,0.0694444444444444,
0.0833333333333333,0.0972222222222222,0.111111111111111,0.125,0.138888888888889,
0.152777777777778,0.166666666666667,0.180555555555556,0.194444444444444,
0.208333333333333,0.222222222222222,0.236111111111111,0.25,0.263888888888889,
0.277777777777778,0.291666666666667,0.305555555555556,0.319444444444444,
0.333333333333333,0.347222222222222,0.361111111111111,0.375,0.388888888888889,
0.402777777777778,0.416666666666667,0.430555555555556,0.444444444444444,
0.458333333333333,0.472222222222222,0.486111111111111,0.5,0.513888888888889,
0.527777777777778,0.541666666666667,0.555555555555556,0.569444444444444,
0.583333333333333,0.597222222222222,0.611111111111111,0.625,0.638888888888889,
0.652777777777778,0.666666666666667,0.680555555555556,0.694444444444444,
0.708333333333333,0.722222222222222,0.736111111111111,0.75,0.763888888888889,
0.777777777777778,0.791666666666667,0.805555555555556,0.819444444444444,
0.833333333333333,0.847222222222222,0.861111111111111,0.875,0.888888888888889,
0.902777777777778,0.916666666666667,0.930555555555556,0.944444444444444,
0.958333333333333,0.972222222222222,0.986111111111111,1.),.UNSPECIFIED.)
GEOMETRIC_REPRESENTATION_ITEM()
RATIONAL_B_SPLINE_SURFACE(((1.,0.923879532511287,1.,0.923879532511287,1.,
0.923879532511287,1.,0.923879532511287,1.,0.923879532511287,1.,0.923879532511287,
1.,0.923879532511287,1.,0.923879532511287,1.,0.923879532511287,1.,0.923879532511287,
1.,0.923879532511287,1.,0.923879532511287,1.,0.923879532511287,1.,0.923879532511287,
1.,0.923879532511287,1.,0.923879532511287,1.,0.923879532511287,1.,0.923879532511287,
1.,0.923879532511287,1.,0.923879532511287,1.,0.923879532511287,1.,0.923879532511287,
1.,0.923879532511287,1.,0.923879532511287,1.,0.923879532511287,1.,0.923879532511287,
1.,0.923879532511287,1.,0.923879532511287,1.,0.923879532511287,1.,0.923879532511287,
1.,0.923879532511287,1.,0.923879532511287,1.,0.923879532511287,1.,0.923879532511287,
1.,0.923879532511287,1.,0.923879532511287,1.,0.923879532511287,1.,0.923879532511287,
1.,0.923879532511287,1.,0.923879532511287,1.,0.923879532511287,1.,0.923879532511287,
1.,0.923879532511287,1.,0.923879532511287,1.,0.923879532511287,1.,0.923879532511287,
1.,0.923879532511287,1.,0.923879532511287,1.,0.923879532511287,1.,0.923879532511287,
1.,0.923879532511287,1.,0.923879532511287,1.,0.923879532511287,1.,0.923879532511287,
1.,0.923879532511287,1.,0.923879532511287,1.,0.923879532511287,1.,0.923879532511287,
1.,0.923879532511287,1.,0.923879532511287,1.,0.923879532511287,1.,0.923879532511287,
1.,0.923879532511287,1.,0.923879532511287,1.,0.923879532511287,1.,0.923879532511287,
1.,0.923879532511287,1.,0.923879532511287,1.,0.923879532511287,1.,0.923879532511287,
1.,0.923879532511287,1.,0.923879532511287,1.),(1.,0.923879532511287,1.,
0.923879532511287,1.,0.923879532511287,1.,0.923879532511287,1.,0.923879532511287,
1.,0.923879532511287,1.,0.923879532511287,1.,0.923879532511287,1.,0.923879532511287,
1.,0.923879532511287,1.,0.923879532511287,1.,0.923879532511287,1.,0.923879532511287,
1.,0.923879532511287,1.,0.923879532511287,1.,0.923879532511287,1.,0.923879532511287,
1.,0.923879532511287,1.,0.923879532511287,1.,0.923879532511287,1.,0.923879532511287,
1.,0.923879532511287,1.,0.923879532511287,1.,0.923879532511287,1.,0.923879532511287,
1.,0.923879532511287,1.,0.923879532511287,1.,0.923879532511287,1.,0.923879532511287,
1.,0.923879532511287,1.,0.923879532511287,1.,0.923879532511287,1.,0.923879532511287,
1.,0.923879532511287,1.,0.923879532511287,1.,0.923879532511287,1.,0.923879532511287,
1.,0.923879532511287,1.,0.923879532511287,1.,0.923879532511287,1.,0.923879532511287,
1.,0.923879532511287,1.,0.923879532511287,1.,0.923879532511287,1.,0.923879532511287,
1.,0.923879532511287,1.,0.923879532511287,1.,0.923879532511287,1.,0.923879532511287,
1.,0.923879532511287,1.,0.923879532511287,1.,0.923879532511287,1.,0.923879532511287,
1.,0.923879532511287,1.,0.923879532511287,1.,0.923879532511287,1.,0.923879532511287,
1.,0.923879532511287,1.,0.923879532511287,1.,0.923879532511287,1.,0.923879532511287,
1.,0.923879532511287,1.,0.923879532511287,1.,0.923879532511287,1.,0.923879532511287,
1.,0.923879532511287,1.,0.923879532511287,1.,0.923879532511287,1.,0.923879532511287,
1.,0.923879532511287,1.,0.923879532511287,1.,0.923879532511287,1.)))
REPRESENTATION_ITEM('')
SURFACE()
) ;
#746 = (
BOUNDED_SURFACE()
B_SPLINE_SURFACE(1,2,((#79923,#79924,#79925,#79926,#79927,#79928,#79929,
#79930,#79931,#79932,#79933,#79934,#79935,#79936,#79937,#79938,#79939,#79940,
#79941,#79942,#79943,#79944,#79945,#79946,#79947,#79948,#79949,#79950,#79951,
#79952,#79953,#79954,#79955,#79956,#79957,#79958,#79959,#79960,#79961,#79962,
#79963,#79964,#79965,#79966,#79967,#79968,#79969,#79970,#79971,#79972,#79973,
#79974,#79975,#79976,#79977,#79978,#79979,#79980,#79981,#79982,#79983,#79984,
#79985,#79986,#79987,#79988,#79989,#79990,#79991,#79992,#79993,#79994,#79995,
#79996,#79997,#79998,#79999,#80000,#80001,#80002,#80003,#80004,#80005,#80006,
#80007,#80008,#80009,#80010,#80011,#80012,#80013,#80014,#80015,#80016,#80017,
#80018,#80019,#80020,#80021,#80022,#80023,#80024,#80025,#80026,#80027,#80028,
#80029,#80030,#80031,#80032,#80033,#80034,#80035,#80036,#80037,#80038,#80039,
#80040,#80041,#80042,#80043,#80044,#80045,#80046,#80047,#80048,#80049,#80050,
#80051,#80052,#80053,#80054,#80055,#80056,#80057,#80058,#80059,#80060,#80061,
#80062,#80063,#80064,#80065,#80066,#80067),(#80068,#80069,#80070,#80071,
#80072,#80073,#80074,#80075,#80076,#80077,#80078,#80079,#80080,#80081,#80082,
#80083,#80084,#80085,#80086,#80087,#80088,#80089,#80090,#80091,#80092,#80093,
#80094,#80095,#80096,#80097,#80098,#80099,#80100,#80101,#80102,#80103,#80104,
#80105,#80106,#80107,#80108,#80109,#80110,#80111,#80112,#80113,#80114,#80115,
#80116,#80117,#80118,#80119,#80120,#80121,#80122,#80123,#80124,#80125,#80126,
#80127,#80128,#80129,#80130,#80131,#80132,#80133,#80134,#80135,#80136,#80137,
#80138,#80139,#80140,#80141,#80142,#80143,#80144,#80145,#80146,#80147,#80148,
#80149,#80150,#80151,#80152,#80153,#80154,#80155,#80156,#80157,#80158,#80159,
#80160,#80161,#80162,#80163,#80164,#80165,#80166,#80167,#80168,#80169,#80170,
#80171,#80172,#80173,#80174,#80175,#80176,#80177,#80178,#80179,#80180,#80181,
#80182,#80183,#80184,#80185,#80186,#80187,#80188,#80189,#80190,#80191,#80192,
#80193,#80194,#80195,#80196,#80197,#80198,#80199,#80200,#80201,#80202,#80203,
#80204,#80205,#80206,#80207,#80208,#80209,#80210,#80211,#80212),(#80213,
#80214,#80215,#80216,#80217,#80218,#80219,#80220,#80221,#80222,#80223,#80224,
#80225,#80226,#80227,#80228,#80229,#80230,#80231,#80232,#80233,#80234,#80235,
#80236,#80237,#80238,#80239,#80240,#80241,#80242,#80243,#80244,#80245,#80246,
#80247,#80248,#80249,#80250,#80251,#80252,#80253,#80254,#80255,#80256,#80257,
#80258,#80259,#80260,#80261,#80262,#80263,#80264,#80265,#80266,#80267,#80268,
#80269,#80270,#80271,#80272,#80273,#80274,#80275,#80276,#80277,#80278,#80279,
#80280,#80281,#80282,#80283,#80284,#80285,#80286,#80287,#80288,#80289,#80290,
#80291,#80292,#80293,#80294,#80295,#80296,#80297,#80298,#80299,#80300,#80301,
#80302,#80303,#80304,#80305,#80306,#80307,#80308,#80309,#80310,#80311,#80312,
#80313,#80314,#80315,#80316,#80317,#80318,#80319,#80320,#80321,#80322,#80323,
#80324,#80325,#80326,#80327,#80328,#80329,#80330,#80331,#80332,#80333,#80334,
#80335,#80336,#80337,#80338,#80339,#80340,#80341,#80342,#80343,#80344,#80345,
#80346,#80347,#80348,#80349,#80350,#80351,#80352,#80353,#80354,#80355,#80356,
#80357),(#80358,#80359,#80360,#80361,#80362,#80363,#80364,#80365,#80366,
#80367,#80368,#80369,#80370,#80371,#80372,#80373,#80374,#80375,#80376,#80377,
#80378,#80379,#80380,#80381,#80382,#80383,#80384,#80385,#80386,#80387,#80388,
#80389,#80390,#80391,#80392,#80393,#80394,#80395,#80396,#80397,#80398,#80399,
#80400,#80401,#80402,#80403,#80404,#80405,#80406,#80407,#80408,#80409,#80410,
#80411,#80412,#80413,#80414,#80415,#80416,#80417,#80418,#80419,#80420,#80421,
#80422,#80423,#80424,#80425,#80426,#80427,#80428,#80429,#80430,#80431,#80432,
#80433,#80434,#80435,#80436,#80437,#80438,#80439,#80440,#80441,#80442,#80443,
#80444,#80445,#80446,#80447,#80448,#80449,#80450,#80451,#80452,#80453,#80454,
#80455,#80456,#80457,#80458,#80459,#80460,#80461,#80462,#80463,#80464,#80465,
#80466,#80467,#80468,#80469,#80470,#80471,#80472,#80473,#80474,#80475,#80476,
#80477,#80478,#80479,#80480,#80481,#80482,#80483,#80484,#80485,#80486,#80487,
#80488,#80489,#80490,#80491,#80492,#80493,#80494,#80495,#80496,#80497,#80498,
#80499,#80500,#80501,#80502)),.UNSPECIFIED.,.F.,.F.,.F.)
B_SPLINE_SURFACE_WITH_KNOTS((2,1,1,2),(3,2,2,2,2,2,2,2,2,2,2,2,2,2,2,2,
2,2,2,2,2,2,2,2,2,2,2,2,2,2,2,2,2,2,2,2,2,2,2,2,2,2,2,2,2,2,2,2,2,2,2,2,
2,2,2,2,2,2,2,2,2,2,2,2,2,2,2,2,2,2,2,2,3),(-5.32860868657006,0.,1.,2.58924025826637),
(0.,0.0138888888888889,0.0277777777777778,0.0416666666666667,0.0555555555555556,
0.0694444444444444,0.0833333333333333,0.0972222222222222,0.111111111111111,
0.125,0.138888888888889,0.152777777777778,0.166666666666667,0.180555555555556,
0.194444444444444,0.208333333333333,0.222222222222222,0.236111111111111,
0.25,0.263888888888889,0.277777777777778,0.291666666666667,0.305555555555556,
0.319444444444444,0.333333333333333,0.347222222222222,0.361111111111111,
0.375,0.388888888888889,0.402777777777778,0.416666666666667,0.430555555555556,
0.444444444444444,0.458333333333333,0.472222222222222,0.486111111111111,
0.5,0.513888888888889,0.527777777777778,0.541666666666667,0.555555555555556,
0.569444444444444,0.583333333333333,0.597222222222222,0.611111111111111,
0.625,0.638888888888889,0.652777777777778,0.666666666666667,0.680555555555556,
0.694444444444444,0.708333333333333,0.722222222222222,0.736111111111111,
0.75,0.763888888888889,0.777777777777778,0.791666666666667,0.805555555555556,
0.819444444444444,0.833333333333333,0.847222222222222,0.861111111111111,
0.875,0.888888888888889,0.902777777777778,0.916666666666667,0.930555555555556,
0.944444444444444,0.958333333333333,0.972222222222222,0.986111111111111,
1.),.UNSPECIFIED.)
GEOMETRIC_REPRESENTATION_ITEM()
RATIONAL_B_SPLINE_SURFACE(((1.,0.923879532511287,1.,0.923879532511287,1.,
0.923879532511287,1.,0.923879532511287,1.,0.923879532511287,1.,0.923879532511287,
1.,0.923879532511287,1.,0.923879532511287,1.,0.923879532511287,1.,0.923879532511287,
1.,0.923879532511287,1.,0.923879532511287,1.,0.923879532511287,1.,0.923879532511287,
1.,0.923879532511287,1.,0.923879532511287,1.,0.923879532511287,1.,0.923879532511287,
1.,0.923879532511287,1.,0.923879532511287,1.,0.923879532511287,1.,0.923879532511287,
1.,0.923879532511287,1.,0.923879532511287,1.,0.923879532511287,1.,0.923879532511287,
1.,0.923879532511287,1.,0.923879532511287,1.,0.923879532511287,1.,0.923879532511287,
1.,0.923879532511287,1.,0.923879532511287,1.,0.923879532511287,1.,0.923879532511287,
1.,0.923879532511287,1.,0.923879532511287,1.,0.923879532511287,1.,0.923879532511287,
1.,0.923879532511287,1.,0.923879532511287,1.,0.923879532511287,1.,0.923879532511287,
1.,0.923879532511287,1.,0.923879532511287,1.,0.923879532511287,1.,0.923879532511287,
1.,0.923879532511287,1.,0.923879532511287,1.,0.923879532511287,1.,0.923879532511287,
1.,0.923879532511287,1.,0.923879532511287,1.,0.923879532511287,1.,0.923879532511287,
1.,0.923879532511287,1.,0.923879532511287,1.,0.923879532511287,1.,0.923879532511287,
1.,0.923879532511287,1.,0.923879532511287,1.,0.923879532511287,1.,0.923879532511287,
1.,0.923879532511287,1.,0.923879532511287,1.,0.923879532511287,1.,0.923879532511287,
1.,0.923879532511287,1.,0.923879532511287,1.,0.923879532511287,1.,0.923879532511287,
1.,0.923879532511287,1.,0.923879532511287,1.),(1.,0.923879532511287,1.,
0.923879532511287,1.,0.923879532511287,1.,0.923879532511287,1.,0.923879532511287,
1.,0.923879532511287,1.,0.923879532511287,1.,0.923879532511287,1.,0.923879532511287,
1.,0.923879532511287,1.,0.923879532511287,1.,0.923879532511287,1.,0.923879532511287,
1.,0.923879532511287,1.,0.923879532511287,1.,0.923879532511287,1.,0.923879532511287,
1.,0.923879532511287,1.,0.923879532511287,1.,0.923879532511287,1.,0.923879532511287,
1.,0.923879532511287,1.,0.923879532511287,1.,0.923879532511287,1.,0.923879532511287,
1.,0.923879532511287,1.,0.923879532511287,1.,0.923879532511287,1.,0.923879532511287,
1.,0.923879532511287,1.,0.923879532511287,1.,0.923879532511287,1.,0.923879532511287,
1.,0.923879532511287,1.,0.923879532511287,1.,0.923879532511287,1.,0.923879532511287,
1.,0.923879532511287,1.,0.923879532511287,1.,0.923879532511287,1.,0.923879532511287,
1.,0.923879532511287,1.,0.923879532511287,1.,0.923879532511287,1.,0.923879532511287,
1.,0.923879532511287,1.,0.923879532511287,1.,0.923879532511287,1.,0.923879532511287,
1.,0.923879532511287,1.,0.923879532511287,1.,0.923879532511287,1.,0.923879532511287,
1.,0.923879532511287,1.,0.923879532511287,1.,0.923879532511287,1.,0.923879532511287,
1.,0.923879532511287,1.,0.923879532511287,1.,0.923879532511287,1.,0.923879532511287,
1.,0.923879532511287,1.,0.923879532511287,1.,0.923879532511287,1.,0.923879532511287,
1.,0.923879532511287,1.,0.923879532511287,1.,0.923879532511287,1.,0.923879532511287,
1.,0.923879532511287,1.,0.923879532511287,1.,0.923879532511287,1.),(1.,
0.923879532511287,1.,0.923879532511287,1.,0.923879532511287,1.,0.923879532511287,
1.,0.923879532511287,1.,0.923879532511287,1.,0.923879532511287,1.,0.923879532511287,
1.,0.923879532511287,1.,0.923879532511287,1.,0.923879532511287,1.,0.923879532511287,
1.,0.923879532511287,1.,0.923879532511287,1.,0.923879532511287,1.,0.923879532511287,
1.,0.923879532511287,1.,0.923879532511287,1.,0.923879532511287,1.,0.923879532511287,
1.,0.923879532511287,1.,0.923879532511287,1.,0.923879532511287,1.,0.923879532511287,
1.,0.923879532511287,1.,0.923879532511287,1.,0.923879532511287,1.,0.923879532511287,
1.,0.923879532511287,1.,0.923879532511287,1.,0.923879532511287,1.,0.923879532511287,
1.,0.923879532511287,1.,0.923879532511287,1.,0.923879532511287,1.,0.923879532511287,
1.,0.923879532511287,1.,0.923879532511287,1.,0.923879532511287,1.,0.923879532511287,
1.,0.923879532511287,1.,0.923879532511287,1.,0.923879532511287,1.,0.923879532511287,
1.,0.923879532511287,1.,0.923879532511287,1.,0.923879532511287,1.,0.923879532511287,
1.,0.923879532511287,1.,0.923879532511287,1.,0.923879532511287,1.,0.923879532511287,
1.,0.923879532511287,1.,0.923879532511287,1.,0.923879532511287,1.,0.923879532511287,
1.,0.923879532511287,1.,0.923879532511287,1.,0.923879532511287,1.,0.923879532511287,
1.,0.923879532511287,1.,0.923879532511287,1.,0.923879532511287,1.,0.923879532511287,
1.,0.923879532511287,1.,0.923879532511287,1.,0.923879532511287,1.,0.923879532511287,
1.,0.923879532511287,1.,0.923879532511287,1.,0.923879532511287,1.,0.923879532511287,
1.),(1.,0.923879532511287,1.,0.923879532511287,1.,0.923879532511287,1.,
0.923879532511287,1.,0.923879532511287,1.,0.923879532511287,1.,0.923879532511287,
1.,0.923879532511287,1.,0.923879532511287,1.,0.923879532511287,1.,0.923879532511287,
1.,0.923879532511287,1.,0.923879532511287,1.,0.923879532511287,1.,0.923879532511287,
1.,0.923879532511287,1.,0.923879532511287,1.,0.923879532511287,1.,0.923879532511287,
1.,0.923879532511287,1.,0.923879532511287,1.,0.923879532511287,1.,0.923879532511287,
1.,0.923879532511287,1.,0.923879532511287,1.,0.923879532511287,1.,0.923879532511287,
1.,0.923879532511287,1.,0.923879532511287,1.,0.923879532511287,1.,0.923879532511287,
1.,0.923879532511287,1.,0.923879532511287,1.,0.923879532511287,1.,0.923879532511287,
1.,0.923879532511287,1.,0.923879532511287,1.,0.923879532511287,1.,0.923879532511287,
1.,0.923879532511287,1.,0.923879532511287,1.,0.923879532511287,1.,0.923879532511287,
1.,0.923879532511287,1.,0.923879532511287,1.,0.923879532511287,1.,0.923879532511287,
1.,0.923879532511287,1.,0.923879532511287,1.,0.923879532511287,1.,0.923879532511287,
1.,0.923879532511287,1.,0.923879532511287,1.,0.923879532511287,1.,0.923879532511287,
1.,0.923879532511287,1.,0.923879532511287,1.,0.923879532511287,1.,0.923879532511287,
1.,0.923879532511287,1.,0.923879532511287,1.,0.923879532511287,1.,0.923879532511287,
1.,0.923879532511287,1.,0.923879532511287,1.,0.923879532511287,1.,0.923879532511287,
1.,0.923879532511287,1.,0.923879532511287,1.,0.923879532511287,1.,0.923879532511287,
1.,0.923879532511287,1.)))
REPRESENTATION_ITEM('')
SURFACE()
) ;
#747 = (
BOUNDED_SURFACE()
B_SPLINE_SURFACE(1,2,((#80503,#80504,#80505,#80506,#80507,#80508,#80509,
#80510,#80511,#80512,#80513,#80514,#80515,#80516,#80517,#80518,#80519,#80520,
#80521,#80522,#80523,#80524,#80525,#80526,#80527,#80528,#80529,#80530,#80531,
#80532,#80533,#80534,#80535,#80536,#80537,#80538,#80539,#80540,#80541,#80542,
#80543,#80544,#80545,#80546,#80547,#80548,#80549,#80550,#80551,#80552,#80553,
#80554,#80555,#80556,#80557,#80558,#80559,#80560,#80561,#80562,#80563,#80564,
#80565,#80566,#80567,#80568,#80569,#80570,#80571,#80572,#80573,#80574,#80575,
#80576,#80577,#80578,#80579,#80580,#80581,#80582,#80583,#80584,#80585,#80586,
#80587,#80588,#80589,#80590,#80591,#80592,#80593,#80594,#80595,#80596,#80597,
#80598,#80599,#80600,#80601,#80602,#80603,#80604,#80605,#80606,#80607,#80608,
#80609,#80610,#80611,#80612,#80613,#80614,#80615,#80616,#80617,#80618,#80619,
#80620,#80621,#80622,#80623,#80624,#80625,#80626,#80627,#80628,#80629,#80630,
#80631,#80632,#80633,#80634,#80635,#80636,#80637,#80638,#80639,#80640,#80641,
#80642,#80643,#80644,#80645,#80646,#80647),(#80648,#80649,#80650,#80651,
#80652,#80653,#80654,#80655,#80656,#80657,#80658,#80659,#80660,#80661,#80662,
#80663,#80664,#80665,#80666,#80667,#80668,#80669,#80670,#80671,#80672,#80673,
#80674,#80675,#80676,#80677,#80678,#80679,#80680,#80681,#80682,#80683,#80684,
#80685,#80686,#80687,#80688,#80689,#80690,#80691,#80692,#80693,#80694,#80695,
#80696,#80697,#80698,#80699,#80700,#80701,#80702,#80703,#80704,#80705,#80706,
#80707,#80708,#80709,#80710,#80711,#80712,#80713,#80714,#80715,#80716,#80717,
#80718,#80719,#80720,#80721,#80722,#80723,#80724,#80725,#80726,#80727,#80728,
#80729,#80730,#80731,#80732,#80733,#80734,#80735,#80736,#80737,#80738,#80739,
#80740,#80741,#80742,#80743,#80744,#80745,#80746,#80747,#80748,#80749,#80750,
#80751,#80752,#80753,#80754,#80755,#80756,#80757,#80758,#80759,#80760,#80761,
#80762,#80763,#80764,#80765,#80766,#80767,#80768,#80769,#80770,#80771,#80772,
#80773,#80774,#80775,#80776,#80777,#80778,#80779,#80780,#80781,#80782,#80783,
#80784,#80785,#80786,#80787,#80788,#80789,#80790,#80791,#80792)),
 .UNSPECIFIED.,.F.,.F.,.F.)
B_SPLINE_SURFACE_WITH_KNOTS((2,2),(3,2,2,2,2,2,2,2,2,2,2,2,2,2,2,2,2,2,
2,2,2,2,2,2,2,2,2,2,2,2,2,2,2,2,2,2,2,2,2,2,2,2,2,2,2,2,2,2,2,2,2,2,2,2,
2,2,2,2,2,2,2,2,2,2,2,2,2,2,2,2,2,2,3),(0.,1.00004424589271),(0.,0.0138888888888889,
0.0277777777777778,0.0416666666666667,0.0555555555555556,0.0694444444444444,
0.0833333333333333,0.0972222222222222,0.111111111111111,0.125,0.138888888888889,
0.152777777777778,0.166666666666667,0.180555555555556,0.194444444444444,
0.208333333333333,0.222222222222222,0.236111111111111,0.25,0.263888888888889,
0.277777777777778,0.291666666666667,0.305555555555556,0.319444444444444,
0.333333333333333,0.347222222222222,0.361111111111111,0.375,0.388888888888889,
0.402777777777778,0.416666666666667,0.430555555555556,0.444444444444444,
0.458333333333333,0.472222222222222,0.486111111111111,0.5,0.513888888888889,
0.527777777777778,0.541666666666667,0.555555555555556,0.569444444444444,
0.583333333333333,0.597222222222222,0.611111111111111,0.625,0.638888888888889,
0.652777777777778,0.666666666666667,0.680555555555556,0.694444444444444,
0.708333333333333,0.722222222222222,0.736111111111111,0.75,0.763888888888889,
0.777777777777778,0.791666666666667,0.805555555555556,0.819444444444444,
0.833333333333333,0.847222222222222,0.861111111111111,0.875,0.888888888888889,
0.902777777777778,0.916666666666667,0.930555555555556,0.944444444444444,
0.958333333333333,0.972222222222222,0.986111111111111,1.),.UNSPECIFIED.)
GEOMETRIC_REPRESENTATION_ITEM()
RATIONAL_B_SPLINE_SURFACE(((1.,0.923879532511287,1.,0.923879532511287,1.,
0.923879532511287,1.,0.923879532511287,1.,0.923879532511287,1.,0.923879532511287,
1.,0.923879532511287,1.,0.923879532511287,1.,0.923879532511287,1.,0.923879532511287,
1.,0.923879532511287,1.,0.923879532511287,1.,0.923879532511287,1.,0.923879532511287,
1.,0.923879532511287,1.,0.923879532511287,1.,0.923879532511287,1.,0.923879532511287,
1.,0.923879532511287,1.,0.923879532511287,1.,0.923879532511287,1.,0.923879532511287,
1.,0.923879532511287,1.,0.923879532511287,1.,0.923879532511287,1.,0.923879532511287,
1.,0.923879532511287,1.,0.923879532511287,1.,0.923879532511287,1.,0.923879532511287,
1.,0.923879532511287,1.,0.923879532511287,1.,0.923879532511287,1.,0.923879532511287,
1.,0.923879532511287,1.,0.923879532511287,1.,0.923879532511287,1.,0.923879532511287,
1.,0.923879532511287,1.,0.923879532511287,1.,0.923879532511287,1.,0.923879532511287,
1.,0.923879532511287,1.,0.923879532511287,1.,0.923879532511287,1.,0.923879532511287,
1.,0.923879532511287,1.,0.923879532511287,1.,0.923879532511287,1.,0.923879532511287,
1.,0.923879532511287,1.,0.923879532511287,1.,0.923879532511287,1.,0.923879532511287,
1.,0.923879532511287,1.,0.923879532511287,1.,0.923879532511287,1.,0.923879532511287,
1.,0.923879532511287,1.,0.923879532511287,1.,0.923879532511287,1.,0.923879532511287,
1.,0.923879532511287,1.,0.923879532511287,1.,0.923879532511287,1.,0.923879532511287,
1.,0.923879532511287,1.,0.923879532511287,1.,0.923879532511287,1.,0.923879532511287,
1.,0.923879532511287,1.,0.923879532511287,1.),(1.,0.923879532511287,1.,
0.923879532511287,1.,0.923879532511287,1.,0.923879532511287,1.,0.923879532511287,
1.,0.923879532511287,1.,0.923879532511287,1.,0.923879532511287,1.,0.923879532511287,
1.,0.923879532511287,1.,0.923879532511287,1.,0.923879532511287,1.,0.923879532511287,
1.,0.923879532511287,1.,0.923879532511287,1.,0.923879532511287,1.,0.923879532511287,
1.,0.923879532511287,1.,0.923879532511287,1.,0.923879532511287,1.,0.923879532511287,
1.,0.923879532511287,1.,0.923879532511287,1.,0.923879532511287,1.,0.923879532511287,
1.,0.923879532511287,1.,0.923879532511287,1.,0.923879532511287,1.,0.923879532511287,
1.,0.923879532511287,1.,0.923879532511287,1.,0.923879532511287,1.,0.923879532511287,
1.,0.923879532511287,1.,0.923879532511287,1.,0.923879532511287,1.,0.923879532511287,
1.,0.923879532511287,1.,0.923879532511287,1.,0.923879532511287,1.,0.923879532511287,
1.,0.923879532511287,1.,0.923879532511287,1.,0.923879532511287,1.,0.923879532511287,
1.,0.923879532511287,1.,0.923879532511287,1.,0.923879532511287,1.,0.923879532511287,
1.,0.923879532511287,1.,0.923879532511287,1.,0.923879532511287,1.,0.923879532511287,
1.,0.923879532511287,1.,0.923879532511287,1.,0.923879532511287,1.,0.923879532511287,
1.,0.923879532511287,1.,0.923879532511287,1.,0.923879532511287,1.,0.923879532511287,
1.,0.923879532511287,1.,0.923879532511287,1.,0.923879532511287,1.,0.923879532511287,
1.,0.923879532511287,1.,0.923879532511287,1.,0.923879532511287,1.,0.923879532511287,
1.,0.923879532511287,1.,0.923879532511287,1.,0.923879532511287,1.)))
REPRESENTATION_ITEM('')
SURFACE()
) ;
#748 = (
BOUNDED_SURFACE()
B_SPLINE_SURFACE(2,2,((#80804,#80805,#80806,#80807,#80808,#80809,#80810,
#80811,#80812),(#80813,#80814,#80815,#80816,#80817,#80818,#80819,#80820,
#80821),(#80822,#80823,#80824,#80825,#80826,#80827,#80828,#80829,#80830)),
 .UNSPECIFIED.,.F.,.T.,.F.)
B_SPLINE_SURFACE_WITH_KNOTS((3,3),(3,2,2,2,3),(0.,1.3),(0.,13.3286488144751,
26.6572976289502,39.9859464434253,53.3145952579004),.UNSPECIFIED.)
GEOMETRIC_REPRESENTATION_ITEM()
RATIONAL_B_SPLINE_SURFACE(((1.,0.707106781186548,1.,0.707106781186548,1.,
0.707106781186548,1.,0.707106781186548,1.),(1.,0.707106781186548,1.,0.707106781186548,
1.,0.707106781186548,1.,0.707106781186548,1.),(1.,0.707106781186548,1.,
0.707106781186548,1.,0.707106781186548,1.,0.707106781186548,1.)))
REPRESENTATION_ITEM('')
SURFACE()
) ;
#749 = (
BOUNDED_SURFACE()
B_SPLINE_SURFACE(2,2,((#80847,#80848,#80849,#80850,#80851,#80852,#80853,
#80854,#80855),(#80856,#80857,#80858,#80859,#80860,#80861,#80862,#80863,
#80864),(#80865,#80866,#80867,#80868,#80869,#80870,#80871,#80872,#80873)),
 .UNSPECIFIED.,.F.,.T.,.F.)
B_SPLINE_SURFACE_WITH_KNOTS((3,3),(3,2,2,2,3),(0.,1.3),(0.,13.3286488144751,
26.6572976289502,39.9859464434253,53.3145952579004),.UNSPECIFIED.)
GEOMETRIC_REPRESENTATION_ITEM()
RATIONAL_B_SPLINE_SURFACE(((1.,0.707106781186548,1.,0.707106781186548,1.,
0.707106781186548,1.,0.707106781186548,1.),(1.,0.707106781186548,1.,0.707106781186548,
1.,0.707106781186548,1.,0.707106781186548,1.),(1.,0.707106781186548,1.,
0.707106781186548,1.,0.707106781186548,1.,0.707106781186548,1.)))
REPRESENTATION_ITEM('')
SURFACE()
) ;
#750 = (
BOUNDED_SURFACE()
B_SPLINE_SURFACE(2,2,((#80892,#80893,#80894,#80895,#80896,#80897,#80898,
#80899,#80900),(#80901,#80902,#80903,#80904,#80905,#80906,#80907,#80908,
#80909),(#80910,#80911,#80912,#80913,#80914,#80915,#80916,#80917,#80918)),
 .UNSPECIFIED.,.F.,.T.,.F.)
B_SPLINE_SURFACE_WITH_KNOTS((3,3),(3,2,2,2,3),(0.,1.3),(0.,13.3286488144751,
26.6572976289502,39.9859464434253,53.3145952579004),.UNSPECIFIED.)
GEOMETRIC_REPRESENTATION_ITEM()
RATIONAL_B_SPLINE_SURFACE(((1.,0.707106781186548,1.,0.707106781186548,1.,
0.707106781186548,1.,0.707106781186548,1.),(1.,0.707106781186548,1.,0.707106781186548,
1.,0.707106781186548,1.,0.707106781186548,1.),(1.,0.707106781186548,1.,
0.707106781186548,1.,0.707106781186548,1.,0.707106781186548,1.)))
REPRESENTATION_ITEM('')
SURFACE()
) ;
#751 = (
BOUNDED_SURFACE()
B_SPLINE_SURFACE(2,2,((#80929,#80930,#80931,#80932,#80933,#80934,#80935,
#80936,#80937),(#80938,#80939,#80940,#80941,#80942,#80943,#80944,#80945,
#80946),(#80947,#80948,#80949,#80950,#80951,#80952,#80953,#80954,#80955)),
 .UNSPECIFIED.,.F.,.T.,.F.)
B_SPLINE_SURFACE_WITH_KNOTS((3,3),(3,2,2,2,3),(0.,1.3),(0.,13.3286488144751,
26.6572976289502,39.9859464434253,53.3145952579004),.UNSPECIFIED.)
GEOMETRIC_REPRESENTATION_ITEM()
RATIONAL_B_SPLINE_SURFACE(((1.,0.707106781186548,1.,0.707106781186548,1.,
0.707106781186548,1.,0.707106781186548,1.),(1.,0.707106781186548,1.,0.707106781186548,
1.,0.707106781186548,1.,0.707106781186548,1.),(1.,0.707106781186548,1.,
0.707106781186548,1.,0.707106781186548,1.,0.707106781186548,1.)))
REPRESENTATION_ITEM('')
SURFACE()
) ;
#752 = (
BOUNDED_SURFACE()
B_SPLINE_SURFACE(2,2,((#80974,#80975,#80976,#80977,#80978,#80979,#80980,
#80981,#80982),(#80983,#80984,#80985,#80986,#80987,#80988,#80989,#80990,
#80991),(#80992,#80993,#80994,#80995,#80996,#80997,#80998,#80999,#81000)),
 .UNSPECIFIED.,.F.,.T.,.F.)
B_SPLINE_SURFACE_WITH_KNOTS((3,3),(3,2,2,2,3),(0.,1.3),(0.,13.3286488144751,
26.6572976289502,39.9859464434253,53.3145952579004),.UNSPECIFIED.)
GEOMETRIC_REPRESENTATION_ITEM()
RATIONAL_B_SPLINE_SURFACE(((1.,0.707106781186548,1.,0.707106781186548,1.,
0.707106781186548,1.,0.707106781186548,1.),(1.,0.707106781186548,1.,0.707106781186548,
1.,0.707106781186548,1.,0.707106781186548,1.),(1.,0.707106781186548,1.,
0.707106781186548,1.,0.707106781186548,1.,0.707106781186548,1.)))
REPRESENTATION_ITEM('')
SURFACE()
) ;
#753 = (
BOUNDED_SURFACE()
B_SPLINE_SURFACE(2,2,((#81429,#81430,#81431),(#81432,#81433,#81434),(#81435,
#81436,#81437),(#81438,#81439,#81440),(#81441,#81442,#81443),(#81444,#81445,
#81446),(#81447,#81448,#81449),(#81450,#81451,#81452),(#81453,#81454,#81455)),
 .UNSPECIFIED.,.T.,.F.,.F.)
B_SPLINE_SURFACE_WITH_KNOTS((3,2,2,2,3),(3,3),(0.,13.3286488144751,26.6572976289502,
39.9859464434253,53.3145952579004),(0.,1.3),.UNSPECIFIED.)
GEOMETRIC_REPRESENTATION_ITEM()
RATIONAL_B_SPLINE_SURFACE(((1.,1.,1.),(0.707106781186548,0.707106781186548,
0.707106781186548),(1.,1.,1.),(0.707106781186548,0.707106781186548,0.707106781186548),
(1.,1.,1.),(0.707106781186548,0.707106781186548,0.707106781186548),(1.,
1.,1.),(0.707106781186548,0.707106781186548,0.707106781186548),(1.,1.,1.)))
REPRESENTATION_ITEM('')
SURFACE()
) ;
#754 = (
BOUNDED_SURFACE()
B_SPLINE_SURFACE(2,2,((#81475,#81476,#81477),(#81478,#81479,#81480),(#81481,
#81482,#81483),(#81484,#81485,#81486),(#81487,#81488,#81489),(#81490,#81491,
#81492),(#81493,#81494,#81495),(#81496,#81497,#81498),(#81499,#81500,#81501)),
 .UNSPECIFIED.,.T.,.F.,.F.)
B_SPLINE_SURFACE_WITH_KNOTS((3,2,2,2,3),(3,3),(0.,13.3286488144751,26.6572976289502,
39.9859464434253,53.3145952579004),(0.,1.3),.UNSPECIFIED.)
GEOMETRIC_REPRESENTATION_ITEM()
RATIONAL_B_SPLINE_SURFACE(((1.,1.,1.),(0.707106781186548,0.707106781186548,
0.707106781186548),(1.,1.,1.),(0.707106781186548,0.707106781186548,0.707106781186548),
(1.,1.,1.),(0.707106781186548,0.707106781186548,0.707106781186548),(1.,
1.,1.),(0.707106781186548,0.707106781186548,0.707106781186548),(1.,1.,1.)))
REPRESENTATION_ITEM('')
SURFACE()
) ;
#755 = (
BOUNDED_SURFACE()
B_SPLINE_SURFACE(2,2,((#81521,#81522,#81523),(#81524,#81525,#81526),(#81527,
#81528,#81529),(#81530,#81531,#81532),(#81533,#81534,#81535),(#81536,#81537,
#81538),(#81539,#81540,#81541),(#81542,#81543,#81544),(#81545,#81546,#81547)),
 .UNSPECIFIED.,.T.,.F.,.F.)
B_SPLINE_SURFACE_WITH_KNOTS((3,2,2,2,3),(3,3),(0.,13.3286488144751,26.6572976289502,
39.9859464434253,53.3145952579004),(0.,1.3),.UNSPECIFIED.)
GEOMETRIC_REPRESENTATION_ITEM()
RATIONAL_B_SPLINE_SURFACE(((1.,1.,1.),(0.707106781186548,0.707106781186548,
0.707106781186548),(1.,1.,1.),(0.707106781186548,0.707106781186548,0.707106781186548),
(1.,1.,1.),(0.707106781186548,0.707106781186548,0.707106781186548),(1.,
1.,1.),(0.707106781186548,0.707106781186548,0.707106781186548),(1.,1.,1.)))
REPRESENTATION_ITEM('')
SURFACE()
) ;
#756 = (
BOUNDED_SURFACE()
B_SPLINE_SURFACE(2,2,((#81561,#81562,#81563),(#81564,#81565,#81566),(#81567,
#81568,#81569),(#81570,#81571,#81572),(#81573,#81574,#81575),(#81576,#81577,
#81578),(#81579,#81580,#81581),(#81582,#81583,#81584),(#81585,#81586,#81587)),
 .UNSPECIFIED.,.T.,.F.,.F.)
B_SPLINE_SURFACE_WITH_KNOTS((3,2,2,2,3),(3,3),(0.,13.3286488144751,26.6572976289502,
39.9859464434253,53.3145952579004),(0.,1.3),.UNSPECIFIED.)
GEOMETRIC_REPRESENTATION_ITEM()
RATIONAL_B_SPLINE_SURFACE(((1.,1.,1.),(0.707106781186548,0.707106781186548,
0.707106781186548),(1.,1.,1.),(0.707106781186548,0.707106781186548,0.707106781186548),
(1.,1.,1.),(0.707106781186548,0.707106781186548,0.707106781186548),(1.,
1.,1.),(0.707106781186548,0.707106781186548,0.707106781186548),(1.,1.,1.)))
REPRESENTATION_ITEM('')
SURFACE()
) ;
#757 = (
BOUNDED_SURFACE()
B_SPLINE_SURFACE(2,2,((#81600,#81601,#81602),(#81603,#81604,#81605),(#81606,
#81607,#81608),(#81609,#81610,#81611),(#81612,#81613,#81614),(#81615,#81616,
#81617),(#81618,#81619,#81620),(#81621,#81622,#81623),(#81624,#81625,#81626)),
 .UNSPECIFIED.,.T.,.F.,.F.)
B_SPLINE_SURFACE_WITH_KNOTS((3,2,2,2,3),(3,3),(0.,13.3286488144751,26.6572976289502,
39.9859464434253,53.3145952579004),(0.,1.3),.UNSPECIFIED.)
GEOMETRIC_REPRESENTATION_ITEM()
RATIONAL_B_SPLINE_SURFACE(((1.,1.,1.),(0.707106781186548,0.707106781186548,
0.707106781186548),(1.,1.,1.),(0.707106781186548,0.707106781186548,0.707106781186548),
(1.,1.,1.),(0.707106781186548,0.707106781186548,0.707106781186548),(1.,
1.,1.),(0.707106781186548,0.707106781186548,0.707106781186548),(1.,1.,1.)))
REPRESENTATION_ITEM('')
SURFACE()
) ;
#758 = (
BOUNDED_SURFACE()
B_SPLINE_SURFACE(1,2,((#84487,#84488,#84489,#84490,#84491,#84492,#84493,
#84494,#84495,#84496,#84497,#84498,#84499,#84500,#84501,#84502,#84503,#84504,
#84505,#84506,#84507,#84508,#84509,#84510,#84511,#84512,#84513,#84514,#84515,
#84516,#84517,#84518,#84519,#84520,#84521,#84522,#84523,#84524,#84525,#84526,
#84527,#84528,#84529,#84530,#84531,#84532,#84533,#84534,#84535,#84536,#84537,
#84538,#84539,#84540,#84541,#84542,#84543,#84544,#84545,#84546,#84547,#84548,
#84549,#84550,#84551,#84552,#84553,#84554,#84555,#84556,#84557,#84558,#84559,
#84560,#84561,#84562,#84563,#84564,#84565,#84566,#84567,#84568,#84569,#84570,
#84571,#84572,#84573,#84574,#84575,#84576,#84577,#84578,#84579,#84580,#84581,
#84582,#84583,#84584,#84585,#84586,#84587,#84588,#84589,#84590,#84591,#84592,
#84593,#84594,#84595,#84596,#84597,#84598,#84599,#84600,#84601,#84602,#84603,
#84604,#84605,#84606,#84607,#84608,#84609,#84610,#84611,#84612,#84613,#84614,
#84615,#84616,#84617,#84618,#84619,#84620,#84621,#84622,#84623,#84624,#84625,
#84626,#84627,#84628,#84629,#84630,#84631,#84632,#84633,#84634,#84635,#84636,
#84637,#84638,#84639,#84640,#84641,#84642,#84643,#84644,#84645,#84646,#84647,
#84648,#84649,#84650,#84651,#84652,#84653,#84654,#84655,#84656,#84657,#84658,
#84659,#84660,#84661,#84662,#84663,#84664,#84665,#84666,#84667,#84668,#84669,
#84670,#84671,#84672,#84673,#84674,#84675,#84676,#84677,#84678,#84679,#84680,
#84681,#84682,#84683,#84684,#84685,#84686,#84687,#84688,#84689,#84690,#84691,
#84692,#84693,#84694,#84695,#84696,#84697,#84698,#84699,#84700,#84701,#84702,
#84703),(#84704,#84705,#84706,#84707,#84708,#84709,#84710,#84711,#84712,
#84713,#84714,#84715,#84716,#84717,#84718,#84719,#84720,#84721,#84722,#84723,
#84724,#84725,#84726,#84727,#84728,#84729,#84730,#84731,#84732,#84733,#84734,
#84735,#84736,#84737,#84738,#84739,#84740,#84741,#84742,#84743,#84744,#84745,
#84746,#84747,#84748,#84749,#84750,#84751,#84752,#84753,#84754,#84755,#84756,
#84757,#84758,#84759,#84760,#84761,#84762,#84763,#84764,#84765,#84766,#84767,
#84768,#84769,#84770,#84771,#84772,#84773,#84774,#84775,#84776,#84777,#84778,
#84779,#84780,#84781,#84782,#84783,#84784,#84785,#84786,#84787,#84788,#84789,
#84790,#84791,#84792,#84793,#84794,#84795,#84796,#84797,#84798,#84799,#84800,
#84801,#84802,#84803,#84804,#84805,#84806,#84807,#84808,#84809,#84810,#84811,
#84812,#84813,#84814,#84815,#84816,#84817,#84818,#84819,#84820,#84821,#84822,
#84823,#84824,#84825,#84826,#84827,#84828,#84829,#84830,#84831,#84832,#84833,
#84834,#84835,#84836,#84837,#84838,#84839,#84840,#84841,#84842,#84843,#84844,
#84845,#84846,#84847,#84848,#84849,#84850,#84851,#84852,#84853,#84854,#84855,
#84856,#84857,#84858,#84859,#84860,#84861,#84862,#84863,#84864,#84865,#84866,
#84867,#84868,#84869,#84870,#84871,#84872,#84873,#84874,#84875,#84876,#84877,
#84878,#84879,#84880,#84881,#84882,#84883,#84884,#84885,#84886,#84887,#84888,
#84889,#84890,#84891,#84892,#84893,#84894,#84895,#84896,#84897,#84898,#84899,
#84900,#84901,#84902,#84903,#84904,#84905,#84906,#84907,#84908,#84909,#84910,
#84911,#84912,#84913,#84914,#84915,#84916,#84917,#84918,#84919,#84920)),
 .UNSPECIFIED.,.F.,.F.,.F.)
B_SPLINE_SURFACE_WITH_KNOTS((2,2),(3,2,2,2,2,2,2,2,2,2,2,2,2,2,2,2,2,2,
2,2,2,2,2,2,2,2,2,2,2,2,2,2,2,2,2,2,2,2,2,2,2,2,2,2,2,2,2,2,2,2,2,2,2,2,
2,2,2,2,2,2,2,2,2,2,2,2,2,2,2,2,2,2,2,2,2,2,2,2,2,2,2,2,2,2,2,2,2,2,2,2,
2,2,2,2,2,2,2,2,2,2,2,2,2,2,2,2,2,2,3),(-3.28672302357595E-5,1.),(-2.52038739293362E-5,
0.00925925925925926,0.0185185185185185,0.0277777777777778,0.037037037037037,
0.0462962962962963,0.0555555555555556,0.0648148148148148,0.0740740740740741,
0.0833333333333333,0.0925925925925926,0.101851851851852,0.111111111111111,
0.12037037037037,0.12962962962963,0.138888888888889,0.148148148148148,0.157407407407407,
0.166666666666667,0.175925925925926,0.185185185185185,0.194444444444444,
0.203703703703704,0.212962962962963,0.222222222222222,0.231481481481481,
0.240740740740741,0.25,0.259259259259259,0.268518518518519,0.277777777777778,
0.287037037037037,0.296296296296296,0.305555555555556,0.314814814814815,
0.324074074074074,0.333333333333333,0.342592592592593,0.351851851851852,
0.361111111111111,0.37037037037037,0.37962962962963,0.388888888888889,0.398148148148148,
0.407407407407407,0.416666666666667,0.425925925925926,0.435185185185185,
0.444444444444444,0.453703703703704,0.462962962962963,0.472222222222222,
0.481481481481481,0.490740740740741,0.5,0.509259259259259,0.518518518518518,
0.527777777777778,0.537037037037037,0.546296296296296,0.555555555555556,
0.564814814814815,0.574074074074074,0.583333333333333,0.592592592592593,
0.601851851851852,0.611111111111111,0.62037037037037,0.62962962962963,0.638888888888889,
0.648148148148148,0.657407407407407,0.666666666666667,0.675925925925926,
0.685185185185185,0.694444444444444,0.703703703703704,0.712962962962963,
0.722222222222222,0.731481481481482,0.740740740740741,0.75,0.759259259259259,
0.768518518518518,0.777777777777778,0.787037037037037,0.796296296296296,
0.805555555555556,0.814814814814815,0.824074074074074,0.833333333333333,
0.842592592592593,0.851851851851852,0.861111111111111,0.87037037037037,
0.87962962962963,0.888888888888889,0.898148148148148,0.907407407407407,
0.916666666666667,0.925925925925926,0.935185185185185,0.944444444444444,
0.953703703703704,0.962962962962963,0.972222222222222,0.981481481481482,
0.990740740740741,1.),.UNSPECIFIED.)
GEOMETRIC_REPRESENTATION_ITEM()
RATIONAL_B_SPLINE_SURFACE(((1.00073134796636,0.865660722470502,1.,0.866025403784439,
1.,0.866025403784439,1.,0.866025403784439,1.,0.866025403784439,1.,0.866025403784439,
1.,0.866025403784439,1.,0.866025403784439,1.,0.866025403784439,1.,0.866025403784439,
1.,0.866025403784439,1.,0.866025403784439,1.,0.866025403784439,1.,0.866025403784439,
1.,0.866025403784439,1.,0.866025403784439,1.,0.866025403784439,1.,0.866025403784439,
1.,0.866025403784439,1.,0.866025403784439,1.,0.866025403784439,1.,0.866025403784439,
1.,0.866025403784439,1.,0.866025403784439,1.,0.866025403784439,1.,0.866025403784439,
1.,0.866025403784439,1.,0.866025403784439,1.,0.866025403784439,1.,0.866025403784439,
1.,0.866025403784439,1.,0.866025403784439,1.,0.866025403784439,1.,0.866025403784439,
1.,0.866025403784439,1.,0.866025403784439,1.,0.866025403784439,1.,0.866025403784439,
1.,0.866025403784439,1.,0.866025403784439,1.,0.866025403784439,1.,0.866025403784439,
1.,0.866025403784439,1.,0.866025403784439,1.,0.866025403784439,1.,0.866025403784439,
1.,0.866025403784439,1.,0.866025403784439,1.,0.866025403784439,1.,0.866025403784439,
1.,0.866025403784439,1.,0.866025403784439,1.,0.866025403784439,1.,0.866025403784439,
1.,0.866025403784439,1.,0.866025403784439,1.,0.866025403784439,1.,0.866025403784439,
1.,0.866025403784439,1.,0.866025403784439,1.,0.866025403784439,1.,0.866025403784439,
1.,0.866025403784439,1.,0.866025403784439,1.,0.866025403784439,1.,0.866025403784439,
1.,0.866025403784439,1.,0.866025403784439,1.,0.866025403784439,1.,0.866025403784439,
1.,0.866025403784439,1.,0.866025403784439,1.,0.866025403784439,1.,0.866025403784439,
1.,0.866025403784439,1.,0.866025403784439,1.,0.866025403784439,1.,0.866025403784439,
1.,0.866025403784439,1.,0.866025403784439,1.,0.866025403784439,1.,0.866025403784439,
1.,0.866025403784439,1.,0.866025403784439,1.,0.866025403784439,1.,0.866025403784439,
1.,0.866025403784439,1.,0.866025403784439,1.,0.866025403784439,1.,0.866025403784439,
1.,0.866025403784439,1.,0.866025403784439,1.,0.866025403784439,1.,0.866025403784439,
1.,0.866025403784439,1.,0.866025403784439,1.,0.866025403784439,1.,0.866025403784439,
1.,0.866025403784439,1.,0.866025403784439,1.,0.866025403784439,1.,0.866025403784439,
1.,0.866025403784439,1.,0.866025403784439,1.,0.866025403784439,1.,0.866025403784439,
1.,0.866025403784439,1.,0.866025403784439,1.),(1.00073134796636,0.865660722470502,
1.,0.866025403784439,1.,0.866025403784439,1.,0.866025403784439,1.,0.866025403784439,
1.,0.866025403784439,1.,0.866025403784439,1.,0.866025403784439,1.,0.866025403784439,
1.,0.866025403784439,1.,0.866025403784439,1.,0.866025403784439,1.,0.866025403784439,
1.,0.866025403784439,1.,0.866025403784439,1.,0.866025403784439,1.,0.866025403784439,
1.,0.866025403784439,1.,0.866025403784439,1.,0.866025403784439,1.,0.866025403784439,
1.,0.866025403784439,1.,0.866025403784439,1.,0.866025403784439,1.,0.866025403784439,
1.,0.866025403784439,1.,0.866025403784439,1.,0.866025403784439,1.,0.866025403784439,
1.,0.866025403784439,1.,0.866025403784439,1.,0.866025403784439,1.,0.866025403784439,
1.,0.866025403784439,1.,0.866025403784439,1.,0.866025403784439,1.,0.866025403784439,
1.,0.866025403784439,1.,0.866025403784439,1.,0.866025403784439,1.,0.866025403784439,
1.,0.866025403784439,1.,0.866025403784439,1.,0.866025403784439,1.,0.866025403784439,
1.,0.866025403784439,1.,0.866025403784439,1.,0.866025403784439,1.,0.866025403784439,
1.,0.866025403784439,1.,0.866025403784439,1.,0.866025403784439,1.,0.866025403784439,
1.,0.866025403784439,1.,0.866025403784439,1.,0.866025403784439,1.,0.866025403784439,
1.,0.866025403784439,1.,0.866025403784439,1.,0.866025403784439,1.,0.866025403784439,
1.,0.866025403784439,1.,0.866025403784439,1.,0.866025403784439,1.,0.866025403784439,
1.,0.866025403784439,1.,0.866025403784439,1.,0.866025403784439,1.,0.866025403784439,
1.,0.866025403784439,1.,0.866025403784439,1.,0.866025403784439,1.,0.866025403784439,
1.,0.866025403784439,1.,0.866025403784439,1.,0.866025403784439,1.,0.866025403784439,
1.,0.866025403784439,1.,0.866025403784439,1.,0.866025403784439,1.,0.866025403784439,
1.,0.866025403784439,1.,0.866025403784439,1.,0.866025403784439,1.,0.866025403784439,
1.,0.866025403784439,1.,0.866025403784439,1.,0.866025403784439,1.,0.866025403784439,
1.,0.866025403784439,1.,0.866025403784439,1.,0.866025403784439,1.,0.866025403784439,
1.,0.866025403784439,1.,0.866025403784439,1.,0.866025403784439,1.,0.866025403784439,
1.,0.866025403784439,1.,0.866025403784439,1.,0.866025403784439,1.,0.866025403784439,
1.,0.866025403784439,1.,0.866025403784439,1.,0.866025403784439,1.,0.866025403784439,
1.,0.866025403784439,1.,0.866025403784439,1.,0.866025403784439,1.)))
REPRESENTATION_ITEM('')
SURFACE()
) ;
#759 = (
BOUNDED_SURFACE()
B_SPLINE_SURFACE(1,2,((#84922,#84923,#84924,#84925,#84926,#84927,#84928,
#84929,#84930,#84931,#84932,#84933,#84934,#84935,#84936,#84937,#84938,#84939,
#84940,#84941,#84942,#84943,#84944,#84945,#84946,#84947,#84948,#84949,#84950,
#84951,#84952,#84953,#84954,#84955,#84956,#84957,#84958,#84959,#84960,#84961,
#84962,#84963,#84964,#84965,#84966,#84967,#84968,#84969,#84970,#84971,#84972,
#84973,#84974,#84975,#84976,#84977,#84978,#84979,#84980,#84981,#84982,#84983,
#84984,#84985,#84986,#84987,#84988,#84989,#84990,#84991,#84992,#84993,#84994,
#84995,#84996,#84997,#84998,#84999,#85000,#85001,#85002,#85003,#85004,#85005,
#85006,#85007,#85008,#85009,#85010,#85011,#85012,#85013,#85014,#85015,#85016,
#85017,#85018,#85019,#85020,#85021,#85022,#85023,#85024,#85025,#85026,#85027,
#85028,#85029,#85030,#85031,#85032,#85033,#85034,#85035,#85036,#85037,#85038,
#85039,#85040,#85041,#85042,#85043,#85044,#85045,#85046,#85047,#85048,#85049,
#85050,#85051,#85052,#85053,#85054,#85055,#85056,#85057,#85058,#85059,#85060,
#85061,#85062,#85063,#85064,#85065,#85066,#85067,#85068,#85069,#85070,#85071,
#85072,#85073,#85074,#85075,#85076,#85077,#85078,#85079,#85080,#85081,#85082,
#85083,#85084,#85085,#85086,#85087,#85088,#85089,#85090,#85091,#85092,#85093,
#85094,#85095,#85096,#85097,#85098,#85099,#85100,#85101,#85102,#85103,#85104,
#85105,#85106,#85107,#85108,#85109,#85110,#85111,#85112,#85113,#85114,#85115,
#85116,#85117,#85118,#85119,#85120,#85121,#85122,#85123,#85124,#85125,#85126,
#85127,#85128,#85129,#85130,#85131,#85132,#85133,#85134,#85135,#85136,#85137,
#85138),(#85139,#85140,#85141,#85142,#85143,#85144,#85145,#85146,#85147,
#85148,#85149,#85150,#85151,#85152,#85153,#85154,#85155,#85156,#85157,#85158,
#85159,#85160,#85161,#85162,#85163,#85164,#85165,#85166,#85167,#85168,#85169,
#85170,#85171,#85172,#85173,#85174,#85175,#85176,#85177,#85178,#85179,#85180,
#85181,#85182,#85183,#85184,#85185,#85186,#85187,#85188,#85189,#85190,#85191,
#85192,#85193,#85194,#85195,#85196,#85197,#85198,#85199,#85200,#85201,#85202,
#85203,#85204,#85205,#85206,#85207,#85208,#85209,#85210,#85211,#85212,#85213,
#85214,#85215,#85216,#85217,#85218,#85219,#85220,#85221,#85222,#85223,#85224,
#85225,#85226,#85227,#85228,#85229,#85230,#85231,#85232,#85233,#85234,#85235,
#85236,#85237,#85238,#85239,#85240,#85241,#85242,#85243,#85244,#85245,#85246,
#85247,#85248,#85249,#85250,#85251,#85252,#85253,#85254,#85255,#85256,#85257,
#85258,#85259,#85260,#85261,#85262,#85263,#85264,#85265,#85266,#85267,#85268,
#85269,#85270,#85271,#85272,#85273,#85274,#85275,#85276,#85277,#85278,#85279,
#85280,#85281,#85282,#85283,#85284,#85285,#85286,#85287,#85288,#85289,#85290,
#85291,#85292,#85293,#85294,#85295,#85296,#85297,#85298,#85299,#85300,#85301,
#85302,#85303,#85304,#85305,#85306,#85307,#85308,#85309,#85310,#85311,#85312,
#85313,#85314,#85315,#85316,#85317,#85318,#85319,#85320,#85321,#85322,#85323,
#85324,#85325,#85326,#85327,#85328,#85329,#85330,#85331,#85332,#85333,#85334,
#85335,#85336,#85337,#85338,#85339,#85340,#85341,#85342,#85343,#85344,#85345,
#85346,#85347,#85348,#85349,#85350,#85351,#85352,#85353,#85354,#85355)),
 .UNSPECIFIED.,.F.,.F.,.F.)
B_SPLINE_SURFACE_WITH_KNOTS((2,2),(3,2,2,2,2,2,2,2,2,2,2,2,2,2,2,2,2,2,
2,2,2,2,2,2,2,2,2,2,2,2,2,2,2,2,2,2,2,2,2,2,2,2,2,2,2,2,2,2,2,2,2,2,2,2,
2,2,2,2,2,2,2,2,2,2,2,2,2,2,2,2,2,2,2,2,2,2,2,2,2,2,2,2,2,2,2,2,2,2,2,2,
2,2,2,2,2,2,2,2,2,2,2,2,2,2,2,2,2,2,3),(0.,1.),(0.,0.00925925925925926,
0.0185185185185185,0.0277777777777778,0.037037037037037,0.0462962962962963,
0.0555555555555556,0.0648148148148148,0.0740740740740741,0.0833333333333333,
0.0925925925925926,0.101851851851852,0.111111111111111,0.12037037037037,
0.12962962962963,0.138888888888889,0.148148148148148,0.157407407407407,
0.166666666666667,0.175925925925926,0.185185185185185,0.194444444444444,
0.203703703703704,0.212962962962963,0.222222222222222,0.231481481481481,
0.240740740740741,0.25,0.259259259259259,0.268518518518519,0.277777777777778,
0.287037037037037,0.296296296296296,0.305555555555556,0.314814814814815,
0.324074074074074,0.333333333333333,0.342592592592593,0.351851851851852,
0.361111111111111,0.37037037037037,0.37962962962963,0.388888888888889,0.398148148148148,
0.407407407407407,0.416666666666667,0.425925925925926,0.435185185185185,
0.444444444444444,0.453703703703704,0.462962962962963,0.472222222222222,
0.481481481481481,0.490740740740741,0.5,0.509259259259259,0.518518518518518,
0.527777777777778,0.537037037037037,0.546296296296296,0.555555555555556,
0.564814814814815,0.574074074074074,0.583333333333333,0.592592592592593,
0.601851851851852,0.611111111111111,0.62037037037037,0.62962962962963,0.638888888888889,
0.648148148148148,0.657407407407407,0.666666666666667,0.675925925925926,
0.685185185185185,0.694444444444444,0.703703703703704,0.712962962962963,
0.722222222222222,0.731481481481482,0.740740740740741,0.75,0.759259259259259,
0.768518518518518,0.777777777777778,0.787037037037037,0.796296296296296,
0.805555555555556,0.814814814814815,0.824074074074074,0.833333333333333,
0.842592592592593,0.851851851851852,0.861111111111111,0.87037037037037,
0.87962962962963,0.888888888888889,0.898148148148148,0.907407407407407,
0.916666666666667,0.925925925925926,0.935185185185185,0.944444444444444,
0.953703703703704,0.962962962962963,0.972222222222222,0.981481481481482,
0.990740740740741,1.),.UNSPECIFIED.)
GEOMETRIC_REPRESENTATION_ITEM()
RATIONAL_B_SPLINE_SURFACE(((1.,0.866025403784439,1.,0.866025403784439,1.,
0.866025403784439,1.,0.866025403784439,1.,0.866025403784439,1.,0.866025403784439,
1.,0.866025403784439,1.,0.866025403784439,1.,0.866025403784439,1.,0.866025403784439,
1.,0.866025403784439,1.,0.866025403784439,1.,0.866025403784439,1.,0.866025403784439,
1.,0.866025403784439,1.,0.866025403784439,1.,0.866025403784439,1.,0.866025403784439,
1.,0.866025403784439,1.,0.866025403784439,1.,0.866025403784439,1.,0.866025403784439,
1.,0.866025403784439,1.,0.866025403784439,1.,0.866025403784439,1.,0.866025403784439,
1.,0.866025403784439,1.,0.866025403784439,1.,0.866025403784439,1.,0.866025403784439,
1.,0.866025403784439,1.,0.866025403784439,1.,0.866025403784439,1.,0.866025403784439,
1.,0.866025403784439,1.,0.866025403784439,1.,0.866025403784439,1.,0.866025403784439,
1.,0.866025403784439,1.,0.866025403784439,1.,0.866025403784439,1.,0.866025403784439,
1.,0.866025403784439,1.,0.866025403784439,1.,0.866025403784439,1.,0.866025403784439,
1.,0.866025403784439,1.,0.866025403784439,1.,0.866025403784439,1.,0.866025403784439,
1.,0.866025403784439,1.,0.866025403784439,1.,0.866025403784439,1.,0.866025403784439,
1.,0.866025403784439,1.,0.866025403784439,1.,0.866025403784439,1.,0.866025403784439,
1.,0.866025403784439,1.,0.866025403784439,1.,0.866025403784439,1.,0.866025403784439,
1.,0.866025403784439,1.,0.866025403784439,1.,0.866025403784439,1.,0.866025403784439,
1.,0.866025403784439,1.,0.866025403784439,1.,0.866025403784439,1.,0.866025403784439,
1.,0.866025403784439,1.,0.866025403784439,1.,0.866025403784439,1.,0.866025403784439,
1.,0.866025403784439,1.,0.866025403784439,1.,0.866025403784439,1.,0.866025403784439,
1.,0.866025403784439,1.,0.866025403784439,1.,0.866025403784439,1.,0.866025403784439,
1.,0.866025403784439,1.,0.866025403784439,1.,0.866025403784439,1.,0.866025403784439,
1.,0.866025403784439,1.,0.866025403784439,1.,0.866025403784439,1.,0.866025403784439,
1.,0.866025403784439,1.,0.866025403784439,1.,0.866025403784439,1.,0.866025403784439,
1.,0.866025403784439,1.,0.866025403784439,1.,0.866025403784439,1.,0.866025403784439,
1.,0.866025403784439,1.,0.866025403784439,1.,0.866025403784439,1.,0.866025403784439,
1.,0.866025403784439,1.,0.866025403784439,1.,0.866025403784439,1.,0.866025403784439,
1.,0.866025403784439,1.,0.866025403784439,1.),(1.,0.866025403784439,1.,
0.866025403784439,1.,0.866025403784439,1.,0.866025403784439,1.,0.866025403784439,
1.,0.866025403784439,1.,0.866025403784439,1.,0.866025403784439,1.,0.866025403784439,
1.,0.866025403784439,1.,0.866025403784439,1.,0.866025403784439,1.,0.866025403784439,
1.,0.866025403784439,1.,0.866025403784439,1.,0.866025403784439,1.,0.866025403784439,
1.,0.866025403784439,1.,0.866025403784439,1.,0.866025403784439,1.,0.866025403784439,
1.,0.866025403784439,1.,0.866025403784439,1.,0.866025403784439,1.,0.866025403784439,
1.,0.866025403784439,1.,0.866025403784439,1.,0.866025403784439,1.,0.866025403784439,
1.,0.866025403784439,1.,0.866025403784439,1.,0.866025403784439,1.,0.866025403784439,
1.,0.866025403784439,1.,0.866025403784439,1.,0.866025403784439,1.,0.866025403784439,
1.,0.866025403784439,1.,0.866025403784439,1.,0.866025403784439,1.,0.866025403784439,
1.,0.866025403784439,1.,0.866025403784439,1.,0.866025403784439,1.,0.866025403784439,
1.,0.866025403784439,1.,0.866025403784439,1.,0.866025403784439,1.,0.866025403784439,
1.,0.866025403784439,1.,0.866025403784439,1.,0.866025403784439,1.,0.866025403784439,
1.,0.866025403784439,1.,0.866025403784439,1.,0.866025403784439,1.,0.866025403784439,
1.,0.866025403784439,1.,0.866025403784439,1.,0.866025403784439,1.,0.866025403784439,
1.,0.866025403784439,1.,0.866025403784439,1.,0.866025403784439,1.,0.866025403784439,
1.,0.866025403784439,1.,0.866025403784439,1.,0.866025403784439,1.,0.866025403784439,
1.,0.866025403784439,1.,0.866025403784439,1.,0.866025403784439,1.,0.866025403784439,
1.,0.866025403784439,1.,0.866025403784439,1.,0.866025403784439,1.,0.866025403784439,
1.,0.866025403784439,1.,0.866025403784439,1.,0.866025403784439,1.,0.866025403784439,
1.,0.866025403784439,1.,0.866025403784439,1.,0.866025403784439,1.,0.866025403784439,
1.,0.866025403784439,1.,0.866025403784439,1.,0.866025403784439,1.,0.866025403784439,
1.,0.866025403784439,1.,0.866025403784439,1.,0.866025403784439,1.,0.866025403784439,
1.,0.866025403784439,1.,0.866025403784439,1.,0.866025403784439,1.,0.866025403784439,
1.,0.866025403784439,1.,0.866025403784439,1.,0.866025403784439,1.,0.866025403784439,
1.,0.866025403784439,1.,0.866025403784439,1.,0.866025403784439,1.,0.866025403784439,
1.,0.866025403784439,1.,0.866025403784439,1.,0.866025403784439,1.)))
REPRESENTATION_ITEM('')
SURFACE()
) ;
#760 = (
BOUNDED_SURFACE()
B_SPLINE_SURFACE(1,2,((#85356,#85357,#85358,#85359,#85360,#85361,#85362,
#85363,#85364,#85365,#85366,#85367,#85368),(#85369,#85370,#85371,#85372,
#85373,#85374,#85375,#85376,#85377,#85378,#85379,#85380,#85381)),
 .UNSPECIFIED.,.F.,.F.,.F.)
B_SPLINE_SURFACE_WITH_KNOTS((2,2),(3,2,2,2,2,2,3),(0.,1.),(-2.070897694853E-5,
0.166666666666667,0.333333333333333,0.5,0.666666666666667,0.833333333333333,
1.),.UNSPECIFIED.)
GEOMETRIC_REPRESENTATION_ITEM()
RATIONAL_B_SPLINE_SURFACE(((1.00003329785877,0.866008756923491,1.,0.866025403784439,
1.,0.866025403784439,1.,0.866025403784439,1.,0.866025403784439,1.,0.866025403784439,
1.),(1.00003329785877,0.866008756923491,1.,0.866025403784439,1.,0.866025403784439,
1.,0.866025403784439,1.,0.866025403784439,1.,0.866025403784439,1.)))
REPRESENTATION_ITEM('')
SURFACE()
) ;
#761 = (
BOUNDED_SURFACE()
B_SPLINE_SURFACE(1,2,((#85479,#85480,#85481,#85482,#85483,#85484,#85485,
#85486,#85487,#85488,#85489,#85490,#85491,#85492,#85493,#85494,#85495),
(#85496,#85497,#85498,#85499,#85500,#85501,#85502,#85503,#85504,#85505,
#85506,#85507,#85508,#85509,#85510,#85511,#85512)),.UNSPECIFIED.,.F.,.F.,
 .F.)
B_SPLINE_SURFACE_WITH_KNOTS((2,2),(3,2,2,2,2,2,2,2,3),(0.,1.00000000011731),
(0.,0.125,0.25,0.375,0.5,0.625,0.75,0.875,0.989797394114478),
 .UNSPECIFIED.)
GEOMETRIC_REPRESENTATION_ITEM()
RATIONAL_B_SPLINE_SURFACE(((1.,0.923879532511287,1.,0.923879532511287,1.,
0.923879532511287,1.,0.923879532511287,1.,0.923879532511287,1.,0.923879532511287,
1.,0.923879532511287,1.,0.930092549548159,0.988588189353252),(1.,0.923879532511287,
1.,0.923879532511287,1.,0.923879532511287,1.,0.923879532511287,1.,0.923879532511287,
1.,0.923879532511287,1.,0.923879532511287,1.,0.930092549548159,0.988588189353252)))
REPRESENTATION_ITEM('')
SURFACE()
) ;
#762 = (
BOUNDED_SURFACE()
B_SPLINE_SURFACE(1,2,((#86143,#86144,#86145,#86146,#86147,#86148,#86149,
#86150,#86151,#86152,#86153,#86154,#86155,#86156,#86157,#86158,#86159),
(#86160,#86161,#86162,#86163,#86164,#86165,#86166,#86167,#86168,#86169,
#86170,#86171,#86172,#86173,#86174,#86175,#86176)),.UNSPECIFIED.,.F.,.F.,
 .F.)
B_SPLINE_SURFACE_WITH_KNOTS((2,2),(3,2,2,2,2,2,2,2,3),(0.,1.),(0.,0.125,
0.25,0.375,0.5,0.625,0.75,0.875,0.989795524002031),.UNSPECIFIED.)
GEOMETRIC_REPRESENTATION_ITEM()
RATIONAL_B_SPLINE_SURFACE(((1.,0.923879532511287,1.,0.923879532511287,1.,
0.923879532511287,1.,0.923879532511287,1.,0.923879532511287,1.,0.923879532511287,
1.,0.923879532511287,1.,0.930093688378829,0.988586283535283),(1.,0.923879532511287,
1.,0.923879532511287,1.,0.923879532511287,1.,0.923879532511287,1.,0.923879532511287,
1.,0.923879532511287,1.,0.923879532511287,1.,0.930093688378829,0.988586283535283)))
REPRESENTATION_ITEM('')
SURFACE()
) ;
#763 = (
BOUNDED_SURFACE()
B_SPLINE_SURFACE(1,2,((#86194,#86195,#86196,#86197,#86198,#86199,#86200,
#86201,#86202,#86203,#86204,#86205,#86206,#86207,#86208,#86209,#86210,#86211,
#86212),(#86213,#86214,#86215,#86216,#86217,#86218,#86219,#86220,#86221,
#86222,#86223,#86224,#86225,#86226,#86227,#86228,#86229,#86230,#86231)),
 .UNSPECIFIED.,.F.,.F.,.F.)
B_SPLINE_SURFACE_WITH_KNOTS((2,2),(3,2,2,2,2,2,2,2,2,3),(0.,1.),(0.,0.125,
0.25,0.375,0.5,0.625,0.75,0.875,0.989795225942127,0.999693178201548),
 .UNSPECIFIED.)
GEOMETRIC_REPRESENTATION_ITEM()
RATIONAL_B_SPLINE_SURFACE(((1.,0.923879532511287,1.,0.923879532511287,1.,
0.923879532511287,1.,0.923879532511287,1.,0.923879532511287,1.,0.923879532511287,
1.,0.923879532511287,1.,0.930093869886503,0.988585979790904,0.988585979790904,
0.988585979790904),(1.,0.923879532511287,1.,0.923879532511287,1.,0.923879532511287,
1.,0.923879532511287,1.,0.923879532511287,1.,0.923879532511287,1.,0.923879532511287,
1.,0.930093869886503,0.988585979790904,0.988585979790904,0.988585979790904)))
REPRESENTATION_ITEM('')
SURFACE()
) ;
#764 = (
BOUNDED_CURVE()
B_SPLINE_CURVE(2,(#48160,#48161,#48162),.UNSPECIFIED.,.F.,.F.)
B_SPLINE_CURVE_WITH_KNOTS((3,3),(-1.37310606553565,-1.01047077031707),
 .UNSPECIFIED.)
CURVE()
GEOMETRIC_REPRESENTATION_ITEM()
RATIONAL_B_SPLINE_CURVE((2.09743606996414,2.25967331459556,2.25967331459556))
REPRESENTATION_ITEM('')
) ;
#765 = (
BOUNDED_CURVE()
B_SPLINE_CURVE(2,(#48163,#48164,#48165),.UNSPECIFIED.,.F.,.F.)
B_SPLINE_CURVE_WITH_KNOTS((3,3),(1.01047077031706,1.37310606553565),
 .UNSPECIFIED.)
CURVE()
GEOMETRIC_REPRESENTATION_ITEM()
RATIONAL_B_SPLINE_CURVE((2.25967331459555,2.25967331459556,2.09743606996414))
REPRESENTATION_ITEM('')
) ;
#766 = (
BOUNDED_CURVE()
B_SPLINE_CURVE(2,(#48171,#48172,#48173),.UNSPECIFIED.,.F.,.F.)
B_SPLINE_CURVE_WITH_KNOTS((3,3),(1.01047077031707,1.37310606553565),
 .UNSPECIFIED.)
CURVE()
GEOMETRIC_REPRESENTATION_ITEM()
RATIONAL_B_SPLINE_CURVE((2.25967331459556,2.25967331459556,2.09743606996414))
REPRESENTATION_ITEM('')
) ;
#767 = (
BOUNDED_CURVE()
B_SPLINE_CURVE(2,(#48174,#48175,#48176),.UNSPECIFIED.,.F.,.F.)
B_SPLINE_CURVE_WITH_KNOTS((3,3),(-1.37310606553565,-1.01047077031707),
 .UNSPECIFIED.)
CURVE()
GEOMETRIC_REPRESENTATION_ITEM()
RATIONAL_B_SPLINE_CURVE((2.09743606996414,2.25967331459556,2.25967331459556))
REPRESENTATION_ITEM('')
) ;
#768 = (
BOUNDED_CURVE()
B_SPLINE_CURVE(2,(#48532,#48533,#48534),.UNSPECIFIED.,.F.,.F.)
B_SPLINE_CURVE_WITH_KNOTS((3,3),(-1.37310606553565,-1.01047077031706),
 .UNSPECIFIED.)
CURVE()
GEOMETRIC_REPRESENTATION_ITEM()
RATIONAL_B_SPLINE_CURVE((2.09743606996414,2.25967331459555,2.25967331459555))
REPRESENTATION_ITEM('')
) ;
#769 = (
BOUNDED_CURVE()
B_SPLINE_CURVE(2,(#48536,#48537,#48538),.UNSPECIFIED.,.F.,.F.)
B_SPLINE_CURVE_WITH_KNOTS((3,3),(-1.01047077031706,-0.647835475111481),
 .UNSPECIFIED.)
CURVE()
GEOMETRIC_REPRESENTATION_ITEM()
RATIONAL_B_SPLINE_CURVE((2.25967331459555,2.25967331459555,2.09743606997577))
REPRESENTATION_ITEM('')
) ;
#770 = (
BOUNDED_CURVE()
B_SPLINE_CURVE(2,(#48541,#48542,#48543),.UNSPECIFIED.,.F.,.F.)
B_SPLINE_CURVE_WITH_KNOTS((3,3),(1.01047077031706,1.37310606553561),
 .UNSPECIFIED.)
CURVE()
GEOMETRIC_REPRESENTATION_ITEM()
RATIONAL_B_SPLINE_CURVE((2.25967331459555,2.25967331459555,2.09743606996417))
REPRESENTATION_ITEM('')
) ;
#771 = (
BOUNDED_CURVE()
B_SPLINE_CURVE(2,(#48544,#48545,#48546),.UNSPECIFIED.,.F.,.F.)
B_SPLINE_CURVE_WITH_KNOTS((3,3),(0.647835475111436,1.01047077031706),
 .UNSPECIFIED.)
CURVE()
GEOMETRIC_REPRESENTATION_ITEM()
RATIONAL_B_SPLINE_CURVE((2.09743606997573,2.25967331459555,2.25967331459555))
REPRESENTATION_ITEM('')
) ;
#772 = (
BOUNDED_CURVE()
B_SPLINE_CURVE(2,(#48549,#48550,#48551),.UNSPECIFIED.,.F.,.F.)
B_SPLINE_CURVE_WITH_KNOTS((3,3),(-1.3731060655357,-1.01047077031707),
 .UNSPECIFIED.)
CURVE()
GEOMETRIC_REPRESENTATION_ITEM()
RATIONAL_B_SPLINE_CURVE((2.09743606996409,2.25967331459555,2.25967331459555))
REPRESENTATION_ITEM('')
) ;
#773 = (
BOUNDED_CURVE()
B_SPLINE_CURVE(2,(#48553,#48554,#48555),.UNSPECIFIED.,.F.,.F.)
B_SPLINE_CURVE_WITH_KNOTS((3,3),(-1.01047077031707,-0.647835475111438),
 .UNSPECIFIED.)
CURVE()
GEOMETRIC_REPRESENTATION_ITEM()
RATIONAL_B_SPLINE_CURVE((2.25967331459555,2.25967331459555,2.09743606997573))
REPRESENTATION_ITEM('')
) ;
#774 = (
BOUNDED_CURVE()
B_SPLINE_CURVE(2,(#48558,#48559,#48560),.UNSPECIFIED.,.F.,.F.)
B_SPLINE_CURVE_WITH_KNOTS((3,3),(1.01047077031707,1.37310606553565),
 .UNSPECIFIED.)
CURVE()
GEOMETRIC_REPRESENTATION_ITEM()
RATIONAL_B_SPLINE_CURVE((2.25967331459555,2.25967331459555,2.09743606996414))
REPRESENTATION_ITEM('')
) ;
#775 = (
BOUNDED_CURVE()
B_SPLINE_CURVE(2,(#48561,#48562,#48563),.UNSPECIFIED.,.F.,.F.)
B_SPLINE_CURVE_WITH_KNOTS((3,3),(0.647835475111388,1.01047077031707),
 .UNSPECIFIED.)
CURVE()
GEOMETRIC_REPRESENTATION_ITEM()
RATIONAL_B_SPLINE_CURVE((2.09743606997569,2.25967331459555,2.25967331459555))
REPRESENTATION_ITEM('')
) ;
#776 = (
BOUNDED_CURVE()
B_SPLINE_CURVE(2,(#48565,#48566,#48567),.UNSPECIFIED.,.F.,.F.)
B_SPLINE_CURVE_WITH_KNOTS((3,3),(-1.37310606553565,-1.01047077031707),
 .UNSPECIFIED.)
CURVE()
GEOMETRIC_REPRESENTATION_ITEM()
RATIONAL_B_SPLINE_CURVE((2.09743606996414,2.25967331459555,2.25967331459555))
REPRESENTATION_ITEM('')
) ;
#777 = (
BOUNDED_CURVE()
B_SPLINE_CURVE(2,(#48569,#48570,#48571),.UNSPECIFIED.,.F.,.F.)
B_SPLINE_CURVE_WITH_KNOTS((3,3),(0.647835475111436,1.01047077031707),
 .UNSPECIFIED.)
CURVE()
GEOMETRIC_REPRESENTATION_ITEM()
RATIONAL_B_SPLINE_CURVE((2.09743606997573,2.25967331459556,2.25967331459556))
REPRESENTATION_ITEM('')
) ;
#778 = (
BOUNDED_CURVE()
B_SPLINE_CURVE(2,(#48574,#48575,#48576),.UNSPECIFIED.,.F.,.F.)
B_SPLINE_CURVE_WITH_KNOTS((3,3),(-1.01047077031707,-0.647835475111437),
 .UNSPECIFIED.)
CURVE()
GEOMETRIC_REPRESENTATION_ITEM()
RATIONAL_B_SPLINE_CURVE((2.25967331459556,2.25967331459556,2.09743606997574))
REPRESENTATION_ITEM('')
) ;
#779 = (
BOUNDED_CURVE()
B_SPLINE_CURVE(2,(#48579,#48580,#48581),.UNSPECIFIED.,.F.,.F.)
B_SPLINE_CURVE_WITH_KNOTS((3,3),(1.01047077031707,1.37310606553565),
 .UNSPECIFIED.)
CURVE()
GEOMETRIC_REPRESENTATION_ITEM()
RATIONAL_B_SPLINE_CURVE((2.25967331459556,2.25967331459556,2.09743606996414))
REPRESENTATION_ITEM('')
) ;
#780 = (
BOUNDED_CURVE()
B_SPLINE_CURVE(2,(#48584,#48585,#48586),.UNSPECIFIED.,.F.,.F.)
B_SPLINE_CURVE_WITH_KNOTS((3,3),(-1.37310606553565,-1.01047077031707),
 .UNSPECIFIED.)
CURVE()
GEOMETRIC_REPRESENTATION_ITEM()
RATIONAL_B_SPLINE_CURVE((2.09743606996414,2.25967331459555,2.25967331459555))
REPRESENTATION_ITEM('')
) ;
#781 = (
BOUNDED_CURVE()
B_SPLINE_CURVE(2,(#48588,#48589,#48590),.UNSPECIFIED.,.F.,.F.)
B_SPLINE_CURVE_WITH_KNOTS((3,3),(-1.01047077031707,-0.647835475111435),
 .UNSPECIFIED.)
CURVE()
GEOMETRIC_REPRESENTATION_ITEM()
RATIONAL_B_SPLINE_CURVE((2.25967331459555,2.25967331459555,2.09743606997573))
REPRESENTATION_ITEM('')
) ;
#782 = (
BOUNDED_CURVE()
B_SPLINE_CURVE(2,(#48593,#48594,#48595),.UNSPECIFIED.,.F.,.F.)
B_SPLINE_CURVE_WITH_KNOTS((3,3),(1.01047077031706,1.37310606553565),
 .UNSPECIFIED.)
CURVE()
GEOMETRIC_REPRESENTATION_ITEM()
RATIONAL_B_SPLINE_CURVE((2.25967331459556,2.25967331459556,2.09743606996414))
REPRESENTATION_ITEM('')
) ;
#783 = (
BOUNDED_CURVE()
B_SPLINE_CURVE(2,(#48596,#48597,#48598),.UNSPECIFIED.,.F.,.F.)
B_SPLINE_CURVE_WITH_KNOTS((3,3),(0.647835475111437,1.01047077031706),
 .UNSPECIFIED.)
CURVE()
GEOMETRIC_REPRESENTATION_ITEM()
RATIONAL_B_SPLINE_CURVE((2.09743606997574,2.25967331459556,2.25967331459556))
REPRESENTATION_ITEM('')
) ;
#784 = (
BOUNDED_CURVE()
B_SPLINE_CURVE(2,(#48601,#48602,#48603),.UNSPECIFIED.,.F.,.F.)
B_SPLINE_CURVE_WITH_KNOTS((3,3),(-1.37310606553565,-1.01047077031706),
 .UNSPECIFIED.)
CURVE()
GEOMETRIC_REPRESENTATION_ITEM()
RATIONAL_B_SPLINE_CURVE((2.09743606996413,2.25967331459555,2.25967331459555))
REPRESENTATION_ITEM('')
) ;
#785 = (
BOUNDED_CURVE()
B_SPLINE_CURVE(2,(#48604,#48605,#48606),.UNSPECIFIED.,.F.,.F.)
B_SPLINE_CURVE_WITH_KNOTS((3,3),(-1.01047077031706,-0.647835475111436),
 .UNSPECIFIED.)
CURVE()
GEOMETRIC_REPRESENTATION_ITEM()
RATIONAL_B_SPLINE_CURVE((2.25967331459555,2.25967331459555,2.09743606997573))
REPRESENTATION_ITEM('')
) ;
#786 = (
BOUNDED_CURVE()
B_SPLINE_CURVE(2,(#48607,#48608,#48609),.UNSPECIFIED.,.F.,.F.)
B_SPLINE_CURVE_WITH_KNOTS((3,3),(1.01047077031706,1.37310606553565),
 .UNSPECIFIED.)
CURVE()
GEOMETRIC_REPRESENTATION_ITEM()
RATIONAL_B_SPLINE_CURVE((2.25967331459555,2.25967331459555,2.09743606996413))
REPRESENTATION_ITEM('')
) ;
#787 = (
BOUNDED_CURVE()
B_SPLINE_CURVE(2,(#48610,#48611,#48612),.UNSPECIFIED.,.F.,.F.)
B_SPLINE_CURVE_WITH_KNOTS((3,3),(0.647835475111436,1.01047077031706),
 .UNSPECIFIED.)
CURVE()
GEOMETRIC_REPRESENTATION_ITEM()
RATIONAL_B_SPLINE_CURVE((2.09743606997573,2.25967331459555,2.25967331459555))
REPRESENTATION_ITEM('')
) ;
#788 = (
BOUNDED_CURVE()
B_SPLINE_CURVE(2,(#49643,#49644,#49645),.UNSPECIFIED.,.F.,.F.)
B_SPLINE_CURVE_WITH_KNOTS((3,3),(-0.0377785531909541,-0.0133078155412431),
 .UNSPECIFIED.)
CURVE()
GEOMETRIC_REPRESENTATION_ITEM()
RATIONAL_B_SPLINE_CURVE((2.38177903497838,1.9561989176297,1.50219886598083))
REPRESENTATION_ITEM('')
) ;
#789 = (
BOUNDED_CURVE()
B_SPLINE_CURVE(2,(#49647,#49648,#49649),.UNSPECIFIED.,.F.,.F.)
B_SPLINE_CURVE_WITH_KNOTS((3,3),(0.118635872970107,0.265338602965705),
 .UNSPECIFIED.)
CURVE()
GEOMETRIC_REPRESENTATION_ITEM()
RATIONAL_B_SPLINE_CURVE((2.07975074185157,2.61715986238987,2.83258860692592))
REPRESENTATION_ITEM('')
) ;
#790 = (
BOUNDED_CURVE()
B_SPLINE_CURVE(2,(#49651,#49652,#49653),.UNSPECIFIED.,.F.,.F.)
B_SPLINE_CURVE_WITH_KNOTS((3,3),(0.461648610024908,0.608351340026347),
 .UNSPECIFIED.)
CURVE()
GEOMETRIC_REPRESENTATION_ITEM()
RATIONAL_B_SPLINE_CURVE((2.83258860692592,2.61715986238129,2.07975074180877))
REPRESENTATION_ITEM('')
) ;
#791 = (
BOUNDED_CURVE()
B_SPLINE_CURVE(2,(#49655,#49656,#49657),.UNSPECIFIED.,.F.,.F.)
B_SPLINE_CURVE_WITH_KNOTS((3,3),(0.770662682377589,0.795133420027306),
 .UNSPECIFIED.)
CURVE()
GEOMETRIC_REPRESENTATION_ITEM()
RATIONAL_B_SPLINE_CURVE((2.38177903497838,1.9561989176296,1.50219886598061))
REPRESENTATION_ITEM('')
) ;
#792 = (
BOUNDED_CURVE()
B_SPLINE_CURVE(2,(#49661,#49662,#49663),.UNSPECIFIED.,.F.,.F.)
B_SPLINE_CURVE_WITH_KNOTS((3,3),(-0.037778553190954,-0.0133078155412431),
 .UNSPECIFIED.)
CURVE()
GEOMETRIC_REPRESENTATION_ITEM()
RATIONAL_B_SPLINE_CURVE((2.38177903497838,1.9561989176297,1.50219886598083))
REPRESENTATION_ITEM('')
) ;
#793 = (
BOUNDED_CURVE()
B_SPLINE_CURVE(2,(#49665,#49666,#49667),.UNSPECIFIED.,.F.,.F.)
B_SPLINE_CURVE_WITH_KNOTS((3,3),(0.118635872970107,0.265338602965705),
 .UNSPECIFIED.)
CURVE()
GEOMETRIC_REPRESENTATION_ITEM()
RATIONAL_B_SPLINE_CURVE((2.07975074185157,2.61715986238987,2.83258860692592))
REPRESENTATION_ITEM('')
) ;
#794 = (
BOUNDED_CURVE()
B_SPLINE_CURVE(2,(#49669,#49670,#49671),.UNSPECIFIED.,.F.,.F.)
B_SPLINE_CURVE_WITH_KNOTS((3,3),(0.461648610024907,0.608351340026346),
 .UNSPECIFIED.)
CURVE()
GEOMETRIC_REPRESENTATION_ITEM()
RATIONAL_B_SPLINE_CURVE((2.83258860692591,2.61715986238129,2.07975074180877))
REPRESENTATION_ITEM('')
) ;
#795 = (
BOUNDED_CURVE()
B_SPLINE_CURVE(2,(#49673,#49674,#49675),.UNSPECIFIED.,.F.,.F.)
B_SPLINE_CURVE_WITH_KNOTS((3,3),(0.770662682377589,0.795133420027306),
 .UNSPECIFIED.)
CURVE()
GEOMETRIC_REPRESENTATION_ITEM()
RATIONAL_B_SPLINE_CURVE((2.38177903497839,1.95619891762961,1.50219886598062))
REPRESENTATION_ITEM('')
) ;
#796 = (
BOUNDED_CURVE()
B_SPLINE_CURVE(2,(#49679,#49680,#49681),.UNSPECIFIED.,.F.,.F.)
B_SPLINE_CURVE_WITH_KNOTS((3,3),(0.77066268237759,0.795133420027307),
 .UNSPECIFIED.)
CURVE()
GEOMETRIC_REPRESENTATION_ITEM()
RATIONAL_B_SPLINE_CURVE((2.38177903497836,1.95619891762959,1.5021988659806))
REPRESENTATION_ITEM('')
) ;
#797 = (
BOUNDED_CURVE()
B_SPLINE_CURVE(2,(#49683,#49684,#49685),.UNSPECIFIED.,.F.,.F.)
B_SPLINE_CURVE_WITH_KNOTS((3,3),(-0.608351340026346,-0.461648610024908),
 .UNSPECIFIED.)
CURVE()
GEOMETRIC_REPRESENTATION_ITEM()
RATIONAL_B_SPLINE_CURVE((2.07975074180878,2.61715986238129,2.83258860692592))
REPRESENTATION_ITEM('')
) ;
#798 = (
BOUNDED_CURVE()
B_SPLINE_CURVE(2,(#49687,#49688,#49689),.UNSPECIFIED.,.F.,.F.)
B_SPLINE_CURVE_WITH_KNOTS((3,3),(-0.265338602965705,-0.118635872970107),
 .UNSPECIFIED.)
CURVE()
GEOMETRIC_REPRESENTATION_ITEM()
RATIONAL_B_SPLINE_CURVE((2.83258860692592,2.61715986238987,2.07975074185157))
REPRESENTATION_ITEM('')
) ;
#799 = (
BOUNDED_CURVE()
B_SPLINE_CURVE(2,(#49691,#49692,#49693),.UNSPECIFIED.,.F.,.F.)
B_SPLINE_CURVE_WITH_KNOTS((3,3),(-0.0377785531909541,-0.0133078155412431),
 .UNSPECIFIED.)
CURVE()
GEOMETRIC_REPRESENTATION_ITEM()
RATIONAL_B_SPLINE_CURVE((2.38177903497838,1.9561989176297,1.50219886598083))
REPRESENTATION_ITEM('')
) ;
#800 = (
BOUNDED_CURVE()
B_SPLINE_CURVE(2,(#49697,#49698,#49699),.UNSPECIFIED.,.F.,.F.)
B_SPLINE_CURVE_WITH_KNOTS((3,3),(0.770662682377589,0.795133420027306),
 .UNSPECIFIED.)
CURVE()
GEOMETRIC_REPRESENTATION_ITEM()
RATIONAL_B_SPLINE_CURVE((2.38177903497838,1.9561989176296,1.50219886598061))
REPRESENTATION_ITEM('')
) ;
#801 = (
BOUNDED_CURVE()
B_SPLINE_CURVE(2,(#49701,#49702,#49703),.UNSPECIFIED.,.F.,.F.)
B_SPLINE_CURVE_WITH_KNOTS((3,3),(-0.608351340026346,-0.461648610024906),
 .UNSPECIFIED.)
CURVE()
GEOMETRIC_REPRESENTATION_ITEM()
RATIONAL_B_SPLINE_CURVE((2.07975074180877,2.61715986238129,2.83258860692592))
REPRESENTATION_ITEM('')
) ;
#802 = (
BOUNDED_CURVE()
B_SPLINE_CURVE(2,(#49705,#49706,#49707),.UNSPECIFIED.,.F.,.F.)
B_SPLINE_CURVE_WITH_KNOTS((3,3),(-0.265338602965706,-0.118635872970107),
 .UNSPECIFIED.)
CURVE()
GEOMETRIC_REPRESENTATION_ITEM()
RATIONAL_B_SPLINE_CURVE((2.83258860692592,2.61715986238987,2.07975074185157))
REPRESENTATION_ITEM('')
) ;
#803 = (
BOUNDED_CURVE()
B_SPLINE_CURVE(2,(#49709,#49710,#49711),.UNSPECIFIED.,.F.,.F.)
B_SPLINE_CURVE_WITH_KNOTS((3,3),(-0.0377785531909542,-0.0133078155412432),
 .UNSPECIFIED.)
CURVE()
GEOMETRIC_REPRESENTATION_ITEM()
RATIONAL_B_SPLINE_CURVE((2.38177903497838,1.95619891762971,1.50219886598083))
REPRESENTATION_ITEM('')
) ;
#804 = (
BOUNDED_CURVE()
B_SPLINE_CURVE(2,(#73318,#73319,#73320,#73321,#73322,#73323,#73324,#73325,
#73326,#73327,#73328,#73329,#73330,#73331,#73332),.UNSPECIFIED.,.F.,.F.)
B_SPLINE_CURVE_WITH_KNOTS((3,2,2,2,2,2,2,3),(0.833333333333333,0.847222222222222,
0.861111111111111,0.875,0.888888888888889,0.902777777777778,0.916666666666667,
0.921887868180636),.UNSPECIFIED.)
CURVE()
GEOMETRIC_REPRESENTATION_ITEM()
RATIONAL_B_SPLINE_CURVE((1.,0.923879532511287,1.,0.923879532511287,1.,0.923879532511287,
1.,0.923879532511287,1.,0.923879532511287,1.,0.923879532511287,1.,0.971384298393079,
0.964283398401841))
REPRESENTATION_ITEM('')
) ;
#805 = (
BOUNDED_CURVE()
B_SPLINE_CURVE(2,(#84380,#84381,#84382),.UNSPECIFIED.,.F.,.F.)
B_SPLINE_CURVE_WITH_KNOTS((3,3),(0.144622167450292,0.333975502520127),
 .UNSPECIFIED.)
CURVE()
GEOMETRIC_REPRESENTATION_ITEM()
RATIONAL_B_SPLINE_CURVE((1.05123113411618,1.06704736773796,1.03645650657006))
REPRESENTATION_ITEM('')
) ;
#806 = (
BOUNDED_CURVE()
B_SPLINE_CURVE(2,(#84385,#84386,#84387),.UNSPECIFIED.,.F.,.F.)
B_SPLINE_CURVE_WITH_KNOTS((3,3),(-0.273691078067528,-0.0843377429954669),
 .UNSPECIFIED.)
CURVE()
GEOMETRIC_REPRESENTATION_ITEM()
RATIONAL_B_SPLINE_CURVE((1.05123113407425,1.06704736768547,1.03645650654287))
REPRESENTATION_ITEM('')
) ;
#807 = (
BOUNDED_CURVE()
B_SPLINE_CURVE(2,(#84393,#84394,#84395),.UNSPECIFIED.,.F.,.F.)
B_SPLINE_CURVE_WITH_KNOTS((3,3),(0.14462216745017,0.333975502519992),
 .UNSPECIFIED.)
CURVE()
GEOMETRIC_REPRESENTATION_ITEM()
RATIONAL_B_SPLINE_CURVE((1.05123113411541,1.06704736773698,1.03645650656957))
REPRESENTATION_ITEM('')
) ;
#808 = (
BOUNDED_CURVE()
B_SPLINE_CURVE(2,(#84398,#84399,#84400),.UNSPECIFIED.,.F.,.F.)
B_SPLINE_CURVE_WITH_KNOTS((3,3),(-0.273691078054969,-0.0843377429828408),
 .UNSPECIFIED.)
CURVE()
GEOMETRIC_REPRESENTATION_ITEM()
RATIONAL_B_SPLINE_CURVE((1.0512311341411,1.06704736776924,1.03645650658487))
REPRESENTATION_ITEM('')
) ;
#809 = (
BOUNDED_CURVE()
B_SPLINE_CURVE(2,(#85385,#85386,#85387),.UNSPECIFIED.,.F.,.F.)
B_SPLINE_CURVE_WITH_KNOTS((3,3),(-0.273691078066784,-0.0843377429945845),
 .UNSPECIFIED.)
CURVE()
GEOMETRIC_REPRESENTATION_ITEM()
RATIONAL_B_SPLINE_CURVE((1.05123113407905,1.06704736769164,1.03645650654597))
REPRESENTATION_ITEM('')
) ;
#810 = (
BOUNDED_CURVE()
B_SPLINE_CURVE(2,(#85390,#85391,#85392),.UNSPECIFIED.,.F.,.F.)
B_SPLINE_CURVE_WITH_KNOTS((3,3),(0.144622167447006,0.333975502516735),
 .UNSPECIFIED.)
CURVE()
GEOMETRIC_REPRESENTATION_ITEM()
RATIONAL_B_SPLINE_CURVE((1.05123113409603,1.06704736771258,1.03645650655733))
REPRESENTATION_ITEM('')
) ;
#811 = (
BOUNDED_CURVE()
B_SPLINE_CURVE(2,(#85446,#85447,#85448),.UNSPECIFIED.,.F.,.F.)
B_SPLINE_CURVE_WITH_KNOTS((3,3),(0.144622167449308,0.333975502519229),
 .UNSPECIFIED.)
CURVE()
GEOMETRIC_REPRESENTATION_ITEM()
RATIONAL_B_SPLINE_CURVE((1.05123113411181,1.06704736773254,1.03645650656736))
REPRESENTATION_ITEM('')
) ;
#812 = (
BOUNDED_CURVE()
B_SPLINE_CURVE(2,(#85450,#85451,#85452),.UNSPECIFIED.,.F.,.F.)
B_SPLINE_CURVE_WITH_KNOTS((3,3),(0.14462216745368,0.333975502523465),
 .UNSPECIFIED.)
CURVE()
GEOMETRIC_REPRESENTATION_ITEM()
RATIONAL_B_SPLINE_CURVE((1.05123113413176,1.06704736775736,1.03645650657979))
REPRESENTATION_ITEM('')
) ;
#813 = (
BOUNDED_CURVE()
B_SPLINE_CURVE(2,(#86177,#86178,#86179,#86180,#86181,#86182,#86183,#86184,
#86185,#86186,#86187,#86188,#86189,#86190,#86191,#86192,#86193),
 .UNSPECIFIED.,.F.,.F.)
B_SPLINE_CURVE_WITH_KNOTS((3,2,2,2,2,2,2,2,3),(0.,0.125,0.25,0.375,0.5,
0.625,0.75,0.875,0.989794503291371),.UNSPECIFIED.)
CURVE()
GEOMETRIC_REPRESENTATION_ITEM()
RATIONAL_B_SPLINE_CURVE((1.,0.923879532511287,1.,0.923879532511287,1.,0.923879532511287,
1.,0.923879532511287,1.,0.923879532511287,1.,0.923879532511287,1.,0.923879532511287,
1.,0.93009430995461,0.988585243365237))
REPRESENTATION_ITEM('')
) ;
#814 = SHAPE_REPRESENTATION_RELATIONSHIP('SRR','None',#86453,#826) ;
#815 = SHAPE_REPRESENTATION_RELATIONSHIP('SRR','None',#86456,#827) ;
#816 = SHAPE_REPRESENTATION_RELATIONSHIP('SRR','None',#86458,#828) ;
#817 = SHAPE_REPRESENTATION_RELATIONSHIP('SRR','None',#86454,#829) ;
#818 = SHAPE_REPRESENTATION_RELATIONSHIP('SRR','None',#86461,#830) ;
#819 = SHAPE_REPRESENTATION_RELATIONSHIP('SRR','None',#86463,#831) ;
#820 = SHAPE_REPRESENTATION_RELATIONSHIP('SRR','None',#86465,#832) ;
#821 = SHAPE_REPRESENTATION_RELATIONSHIP('SRR','None',#86467,#833) ;
#822 = SHAPE_REPRESENTATION_RELATIONSHIP('SRR','None',#86468,#834) ;
#823 = SHAPE_REPRESENTATION_RELATIONSHIP('SRR','None',#86473,#835) ;
#824 = SHAPE_REPRESENTATION_RELATIONSHIP('SRR','None',#86474,#836) ;
#825 = SHAPE_REPRESENTATION_RELATIONSHIP('SRR','None',#86475,#837) ;
#826 = ADVANCED_BREP_SHAPE_REPRESENTATION('',(#850),#86307) ;
#827 = ADVANCED_BREP_SHAPE_REPRESENTATION('',(#851),#86310) ;
#828 = ADVANCED_BREP_SHAPE_REPRESENTATION('',(#852),#86312) ;
#829 = ADVANCED_BREP_SHAPE_REPRESENTATION('',(#853),#86308) ;
#830 = ADVANCED_BREP_SHAPE_REPRESENTATION('',(#854),#86315) ;
#831 = ADVANCED_BREP_SHAPE_REPRESENTATION('',(#855),#86317) ;
#832 = ADVANCED_BREP_SHAPE_REPRESENTATION('',(#856),#86319) ;
#833 = ADVANCED_BREP_SHAPE_REPRESENTATION('',(#857),#86321) ;
#834 = ADVANCED_BREP_SHAPE_REPRESENTATION('',(#858),#86322) ;
#835 = ADVANCED_BREP_SHAPE_REPRESENTATION('',(#859),#86327) ;
#836 = ADVANCED_BREP_SHAPE_REPRESENTATION('',(#860),#86328) ;
#837 = ADVANCED_BREP_SHAPE_REPRESENTATION('',(#861),#86329) ;
#838 = STYLED_ITEM('',(#86581),#850) ;
#839 = STYLED_ITEM('',(#86582),#851) ;
#840 = STYLED_ITEM('',(#86582),#852) ;
#841 = STYLED_ITEM('',(#86581),#853) ;
#842 = STYLED_ITEM('',(#86583),#854) ;
#843 = STYLED_ITEM('',(#86582),#855) ;
#844 = STYLED_ITEM('',(#86582),#856) ;
#845 = STYLED_ITEM('',(#86582),#857) ;
#846 = STYLED_ITEM('',(#86584),#858) ;
#847 = STYLED_ITEM('',(#86582),#859) ;
#848 = STYLED_ITEM('',(#86582),#860) ;
#849 = STYLED_ITEM('',(#86582),#861) ;
#850 = MANIFOLD_SOLID_BREP('Body1',#32637) ;
#851 = MANIFOLD_SOLID_BREP('Body1',#32638) ;
#852 = MANIFOLD_SOLID_BREP('Body1',#32639) ;
#853 = MANIFOLD_SOLID_BREP('Body1',#32640) ;
#854 = MANIFOLD_SOLID_BREP('Body1',#32641) ;
#855 = MANIFOLD_SOLID_BREP('Body1',#32642) ;
#856 = MANIFOLD_SOLID_BREP('Body1',#32643) ;
#857 = MANIFOLD_SOLID_BREP('Body1',#32644) ;
#858 = MANIFOLD_SOLID_BREP('Body1',#32645) ;
#859 = MANIFOLD_SOLID_BREP('Body1',#32646) ;
#860 = MANIFOLD_SOLID_BREP('Body1',#32647) ;
#861 = MANIFOLD_SOLID_BREP('Body1',#32648) ;
#862 = CONICAL_SURFACE('',#33010,2.390165042945,0.785398163397448) ;
#863 = CONICAL_SURFACE('',#33011,2.390165042945,0.785398163397448) ;
#864 = CONICAL_SURFACE('',#33078,1.5,0.78539816339745) ;
#865 = CONICAL_SURFACE('',#33079,1.5,0.78539816339745) ;
#866 = CONICAL_SURFACE('',#33080,1.5,0.78539816339745) ;
#867 = CONICAL_SURFACE('',#33082,1.5,0.78539816339745) ;
#868 = CONICAL_SURFACE('',#33086,2.75,1.0471975511966) ;
#869 = CONICAL_SURFACE('',#33088,2.75,1.0471975511966) ;
#870 = CONICAL_SURFACE('',#33108,2.75,1.0471975511966) ;
#871 = CONICAL_SURFACE('',#33109,2.75,1.0471975511966) ;
#872 = CONICAL_SURFACE('',#33110,2.75,1.0471975511966) ;
#873 = CONICAL_SURFACE('',#33111,2.75,1.0471975511966) ;
#874 = CONICAL_SURFACE('',#33112,2.75,1.0471975511966) ;
#875 = CONICAL_SURFACE('',#33113,2.75,1.0471975511966) ;
#876 = CONICAL_SURFACE('',#33114,2.75,1.0471975511966) ;
#877 = CONICAL_SURFACE('',#33115,2.75,1.0471975511966) ;
#878 = CONICAL_SURFACE('',#33116,2.75,1.0471975511966) ;
#879 = CONICAL_SURFACE('',#33117,2.75,1.0471975511966) ;
#880 = CONICAL_SURFACE('',#33151,1.4224,0.715584993317677) ;
#881 = CONICAL_SURFACE('',#33157,0.92075,0.78539816339745) ;
#882 = CONICAL_SURFACE('',#33159,0.968718914342085,0.715584993317677) ;
#883 = CONICAL_SURFACE('',#33469,2.20000000000002,0.785398163397472) ;
#884 = CONICAL_SURFACE('',#33472,2.2,0.78539816339745) ;
#885 = CONICAL_SURFACE('',#33475,2.2,0.785398163397451) ;
#886 = CONICAL_SURFACE('',#33486,2.25,0.785398163397448) ;
#887 = CONICAL_SURFACE('',#33571,2.25,0.785398163397448) ;
#888 = CONICAL_SURFACE('',#33576,2.25,0.785398163397448) ;
#889 = CONICAL_SURFACE('',#33581,2.25,0.785398163397448) ;
#890 = CONICAL_SURFACE('',#33586,2.25,0.785398163397448) ;
#891 = CONICAL_SURFACE('',#33635,2.2,0.78539816339745) ;
#892 = CONICAL_SURFACE('',#35617,2.38125,0.26179938779915) ;
#893 = CONICAL_SURFACE('',#35866,2.38125,0.26179938779915) ;
#894 = CONICAL_SURFACE('',#35897,1.7526,0.78539816339745) ;
#895 = CONICAL_SURFACE('',#35899,2.38125,0.26179938779915) ;
#896 = CONICAL_SURFACE('',#35900,2.38125,0.26179938779915) ;
#897 = CONICAL_SURFACE('',#36415,4.35024047358084,0.785398163397443) ;
#898 = CONICAL_SURFACE('',#36417,4.35024047358084,0.785398163397443) ;
#899 = CONICAL_SURFACE('',#36423,1.5,0.26179938779915) ;
#900 = CONICAL_SURFACE('',#36426,1.5,0.26179938779915) ;
#901 = CONICAL_SURFACE('',#36461,1.5,0.26179938779915) ;
#902 = CONICAL_SURFACE('',#36477,1.5,0.26179938779915) ;
#903 = B_SPLINE_SURFACE_WITH_KNOTS('',3,3,((#46889,#46890,#46891,#46892),
(#46893,#46894,#46895,#46896),(#46897,#46898,#46899,#46900),(#46901,#46902,
#46903,#46904),(#46905,#46906,#46907,#46908),(#46909,#46910,#46911,#46912),
(#46913,#46914,#46915,#46916)),.UNSPECIFIED.,.F.,.F.,.F.,(4,1,1,1,4),(4,
4),(0.,0.285714285714286,0.571428571428571,0.857142857142857,1.),(0.250000208289045,
0.310000208302026),.UNSPECIFIED.) ;
#904 = B_SPLINE_SURFACE_WITH_KNOTS('',3,3,((#46923,#46924,#46925,#46926),
(#46927,#46928,#46929,#46930),(#46931,#46932,#46933,#46934),(#46935,#46936,
#46937,#46938),(#46939,#46940,#46941,#46942),(#46943,#46944,#46945,#46946),
(#46947,#46948,#46949,#46950)),.UNSPECIFIED.,.F.,.F.,.F.,(4,1,1,1,4),(4,
4),(0.,0.285714285714286,0.571428571428571,0.857142857142857,1.),(-1.50824147057263E-10,
0.0600000000000031),.UNSPECIFIED.) ;
#905 = B_SPLINE_SURFACE_WITH_KNOTS('',3,1,((#65564,#65565),(#65566,#65567),
(#65568,#65569),(#65570,#65571),(#65572,#65573),(#65574,#65575),(#65576,
#65577),(#65578,#65579),(#65580,#65581),(#65582,#65583),(#65584,#65585),
(#65586,#65587),(#65588,#65589),(#65590,#65591),(#65592,#65593),(#65594,
#65595),(#65596,#65597),(#65598,#65599),(#65600,#65601),(#65602,#65603),
(#65604,#65605),(#65606,#65607)),.UNSPECIFIED.,.F.,.F.,.F.,(4,3,3,3,3,3,
3,4),(2,2),(0.136589431488165,0.1402592459748,0.143851356976514,0.2091154250925,
0.346827783328,0.4845401415634,0.990211404581674,0.997547219258416),(0.,
0.297000000002801),.UNSPECIFIED.) ;
#906 = B_SPLINE_SURFACE_WITH_KNOTS('',3,3,((#66221,#66222,#66223,#66224,#66225,
#66226,#66227,#66228,#66229,#66230,#66231,#66232,#66233,#66234,#66235,#66236,
#66237,#66238,#66239,#66240,#66241,#66242,#66243),(#66244,#66245,#66246,
#66247,#66248,#66249,#66250,#66251,#66252,#66253,#66254,#66255,#66256,#66257,
#66258,#66259,#66260,#66261,#66262,#66263,#66264,#66265,#66266),(#66267,
#66268,#66269,#66270,#66271,#66272,#66273,#66274,#66275,#66276,#66277,#66278,
#66279,#66280,#66281,#66282,#66283,#66284,#66285,#66286,#66287,#66288,#66289),
(#66290,#66291,#66292,#66293,#66294,#66295,#66296,#66297,#66298,#66299,
#66300,#66301,#66302,#66303,#66304,#66305,#66306,#66307,#66308,#66309,#66310,
#66311,#66312)),.UNSPECIFIED.,.F.,.F.,.F.,(4,4),(4,1,1,1,1,1,1,1,1,1,1,
1,1,1,1,1,1,1,1,1,4),(-0.000643685928907995,0.0452738098722425),(14.3976860695295,
15.3964695570642,16.3947981013537,17.3931266456432,18.3914551899327,19.3897837342222,
20.3881122785118,21.3864408228013,22.3847693670908,23.3830979113803,24.3814264556698,
25.3797549999593,26.3780835442488,27.3764120885383,28.3747406328278,29.3730691771173,
30.3713977214068,31.3697262656963,32.3680548099858,33.3663833542754,34.3650967250075),
 .UNSPECIFIED.) ;
#907 = B_SPLINE_SURFACE_WITH_KNOTS('',3,3,((#66313,#66314,#66315,#66316,#66317,
#66318,#66319,#66320,#66321,#66322,#66323,#66324,#66325,#66326,#66327,#66328,
#66329,#66330,#66331,#66332,#66333,#66334,#66335),(#66336,#66337,#66338,
#66339,#66340,#66341,#66342,#66343,#66344,#66345,#66346,#66347,#66348,#66349,
#66350,#66351,#66352,#66353,#66354,#66355,#66356,#66357,#66358),(#66359,
#66360,#66361,#66362,#66363,#66364,#66365,#66366,#66367,#66368,#66369,#66370,
#66371,#66372,#66373,#66374,#66375,#66376,#66377,#66378,#66379,#66380,#66381),
(#66382,#66383,#66384,#66385,#66386,#66387,#66388,#66389,#66390,#66391,
#66392,#66393,#66394,#66395,#66396,#66397,#66398,#66399,#66400,#66401,#66402,
#66403,#66404)),.UNSPECIFIED.,.F.,.F.,.F.,(4,4),(4,1,1,1,1,1,1,1,1,1,1,
1,1,1,1,1,1,1,1,1,4),(-0.000384825361838686,0.0458091503480694),(11.8611951788935,
12.8599085485448,13.8582370928343,14.8565656371238,15.8548941814133,16.8532227257028,
17.8515512699923,18.8498798142818,19.8482083585713,20.8465369028608,21.8448654471503,
22.8431939914399,23.8415225357294,24.8398510800189,25.8381796243084,26.8365081685979,
27.8348367128874,28.8331652571769,29.8314938014664,30.8298223457559,31.8285783647924),
 .UNSPECIFIED.) ;
#908 = B_SPLINE_SURFACE_WITH_KNOTS('',3,3,((#66405,#66406,#66407,#66408,#66409,
#66410,#66411,#66412,#66413,#66414,#66415,#66416,#66417,#66418,#66419,#66420,
#66421,#66422,#66423,#66424,#66425,#66426,#66427),(#66428,#66429,#66430,
#66431,#66432,#66433,#66434,#66435,#66436,#66437,#66438,#66439,#66440,#66441,
#66442,#66443,#66444,#66445,#66446,#66447,#66448,#66449,#66450),(#66451,
#66452,#66453,#66454,#66455,#66456,#66457,#66458,#66459,#66460,#66461,#66462,
#66463,#66464,#66465,#66466,#66467,#66468,#66469,#66470,#66471,#66472,#66473),
(#66474,#66475,#66476,#66477,#66478,#66479,#66480,#66481,#66482,#66483,
#66484,#66485,#66486,#66487,#66488,#66489,#66490,#66491,#66492,#66493,#66494,
#66495,#66496)),.UNSPECIFIED.,.F.,.F.,.F.,(4,4),(4,1,1,1,1,1,1,1,1,1,1,
1,1,1,1,1,1,1,1,1,4),(-0.000647263935840991,0.0452759437895929),(14.3976836084423,
15.3964695570666,16.394798101356,17.3931266456453,18.3914551899347,19.389783734224,
20.3881122785134,21.3864408228027,22.384769367092,23.3830979113814,24.3814264556707,
25.3797549999601,26.3780835442494,27.3764120885388,28.3747406328281,29.3730691771175,
30.3713977214068,31.3697262656962,32.3680548099855,33.3663833542749,34.3650988589243),
 .UNSPECIFIED.) ;
#909 = B_SPLINE_SURFACE_WITH_KNOTS('',3,3,((#66497,#66498,#66499,#66500,#66501,
#66502,#66503,#66504,#66505,#66506,#66507,#66508,#66509,#66510,#66511,#66512,
#66513,#66514,#66515,#66516,#66517,#66518,#66519),(#66520,#66521,#66522,
#66523,#66524,#66525,#66526,#66527,#66528,#66529,#66530,#66531,#66532,#66533,
#66534,#66535,#66536,#66537,#66538,#66539,#66540,#66541,#66542),(#66543,
#66544,#66545,#66546,#66547,#66548,#66549,#66550,#66551,#66552,#66553,#66554,
#66555,#66556,#66557,#66558,#66559,#66560,#66561,#66562,#66563,#66564,#66565),
(#66566,#66567,#66568,#66569,#66570,#66571,#66572,#66573,#66574,#66575,
#66576,#66577,#66578,#66579,#66580,#66581,#66582,#66583,#66584,#66585,#66586,
#66587,#66588)),.UNSPECIFIED.,.F.,.F.,.F.,(4,4),(4,1,1,1,1,1,1,1,1,1,1,
1,1,1,1,1,1,1,1,1,4),(-0.00038695950106726,0.0458188085461498),(11.8611930447567,
12.8599085485472,13.8582370928365,14.8565656371259,15.8548941814152,16.8532227257046,
17.8515512699939,18.8498798142833,19.8482083585726,20.846536902862,21.8448654471513,
22.8431939914407,23.84152253573,24.8398510800194,25.8381796243087,26.8365081685981,
27.8348367128874,28.8331652571768,29.8314938014661,30.8298223457555,31.8285876047897),
 .UNSPECIFIED.) ;
#910 = B_SPLINE_SURFACE_WITH_KNOTS('',3,3,((#66589,#66590,#66591,#66592,#66593,
#66594,#66595,#66596,#66597,#66598,#66599,#66600,#66601,#66602,#66603,#66604,
#66605,#66606,#66607,#66608,#66609,#66610,#66611),(#66612,#66613,#66614,
#66615,#66616,#66617,#66618,#66619,#66620,#66621,#66622,#66623,#66624,#66625,
#66626,#66627,#66628,#66629,#66630,#66631,#66632,#66633,#66634),(#66635,
#66636,#66637,#66638,#66639,#66640,#66641,#66642,#66643,#66644,#66645,#66646,
#66647,#66648,#66649,#66650,#66651,#66652,#66653,#66654,#66655,#66656,#66657),
(#66658,#66659,#66660,#66661,#66662,#66663,#66664,#66665,#66666,#66667,
#66668,#66669,#66670,#66671,#66672,#66673,#66674,#66675,#66676,#66677,#66678,
#66679,#66680)),.UNSPECIFIED.,.F.,.F.,.F.,(4,4),(4,1,1,1,1,1,1,1,1,1,1,
1,1,1,1,1,1,1,1,1,4),(-0.000640464694106941,0.0452718121575805),(14.3976883946163,
15.3964695570665,16.394798101356,17.3931266456454,18.3914551899348,19.3897837342242,
20.3881122785137,21.3864408228031,22.3847693670925,23.3830979113819,24.3814264556714,
25.3797549999608,26.3780835442502,27.3764120885396,28.3747406328291,29.3730691771185,
30.3713977214079,31.3697262656973,32.3680548099868,33.3663833542762,34.3650947272934),
 .UNSPECIFIED.) ;
#911 = B_SPLINE_SURFACE_WITH_KNOTS('',3,3,((#66681,#66682,#66683,#66684,#66685,
#66686,#66687,#66688,#66689,#66690,#66691,#66692,#66693,#66694,#66695,#66696,
#66697,#66698,#66699,#66700,#66701,#66702,#66703),(#66704,#66705,#66706,
#66707,#66708,#66709,#66710,#66711,#66712,#66713,#66714,#66715,#66716,#66717,
#66718,#66719,#66720,#66721,#66722,#66723,#66724,#66725,#66726),(#66727,
#66728,#66729,#66730,#66731,#66732,#66733,#66734,#66735,#66736,#66737,#66738,
#66739,#66740,#66741,#66742,#66743,#66744,#66745,#66746,#66747,#66748,#66749),
(#66750,#66751,#66752,#66753,#66754,#66755,#66756,#66757,#66758,#66759,
#66760,#66761,#66762,#66763,#66764,#66765,#66766,#66767,#66768,#66769,#66770,
#66771,#66772)),.UNSPECIFIED.,.F.,.F.,.F.,(4,4),(4,1,1,1,1,1,1,1,1,1,1,
1,1,1,1,1,1,1,1,1,4),(-0.000382830284004954,0.0458008767222032),(11.8611971739735,
12.8599085485469,13.8582370928364,14.8565656371258,15.8548941814152,16.8532227257047,
17.8515512699941,18.8498798142835,19.848208358573,20.8465369028624,21.8448654471518,
22.8431939914413,23.8415225357307,24.8398510800201,25.8381796243096,26.836508168599,
27.8348367128884,28.8331652571779,29.8314938014673,30.8298223457568,31.8285705594706),
 .UNSPECIFIED.) ;
#912 = B_SPLINE_SURFACE_WITH_KNOTS('',3,3,((#66773,#66774,#66775,#66776,#66777,
#66778,#66779,#66780,#66781,#66782,#66783,#66784,#66785,#66786,#66787,#66788,
#66789,#66790,#66791,#66792,#66793,#66794,#66795),(#66796,#66797,#66798,
#66799,#66800,#66801,#66802,#66803,#66804,#66805,#66806,#66807,#66808,#66809,
#66810,#66811,#66812,#66813,#66814,#66815,#66816,#66817,#66818),(#66819,
#66820,#66821,#66822,#66823,#66824,#66825,#66826,#66827,#66828,#66829,#66830,
#66831,#66832,#66833,#66834,#66835,#66836,#66837,#66838,#66839,#66840,#66841),
(#66842,#66843,#66844,#66845,#66846,#66847,#66848,#66849,#66850,#66851,
#66852,#66853,#66854,#66855,#66856,#66857,#66858,#66859,#66860,#66861,#66862,
#66863,#66864)),.UNSPECIFIED.,.F.,.F.,.F.,(4,4),(4,1,1,1,1,1,1,1,1,1,1,
1,1,1,1,1,1,1,1,1,4),(-0.000644632360233455,0.0452743831442753),(14.3976854059706,
15.3964695570646,16.394798101354,17.3931266456435,18.3914551899329,19.3897837342223,
20.3881122785117,21.3864408228012,22.3847693670906,23.38309791138,24.3814264556694,
25.3797549999589,26.3780835442483,27.3764120885377,28.3747406328271,29.3730691771166,
30.371397721406,31.3697262656954,32.3680548099849,33.3663833542743,34.3650972982779),
 .UNSPECIFIED.) ;
#913 = B_SPLINE_SURFACE_WITH_KNOTS('',3,3,((#66865,#66866,#66867,#66868,#66869,
#66870,#66871,#66872,#66873,#66874,#66875,#66876,#66877,#66878,#66879,#66880,
#66881,#66882,#66883,#66884,#66885,#66886,#66887),(#66888,#66889,#66890,
#66891,#66892,#66893,#66894,#66895,#66896,#66897,#66898,#66899,#66900,#66901,
#66902,#66903,#66904,#66905,#66906,#66907,#66908,#66909,#66910),(#66911,
#66912,#66913,#66914,#66915,#66916,#66917,#66918,#66919,#66920,#66921,#66922,
#66923,#66924,#66925,#66926,#66927,#66928,#66929,#66930,#66931,#66932,#66933),
(#66934,#66935,#66936,#66937,#66938,#66939,#66940,#66941,#66942,#66943,
#66944,#66945,#66946,#66947,#66948,#66949,#66950,#66951,#66952,#66953,#66954,
#66955,#66956)),.UNSPECIFIED.,.F.,.F.,.F.,(4,4),(4,1,1,1,1,1,1,1,1,1,1,
1,1,1,1,1,1,1,1,1,4),(-0.000385400908840022,0.045811671314961),(11.8611946033468,
12.859908548545,13.8582370928345,14.8565656371239,15.8548941814133,16.8532227257028,
17.8515512699922,18.8498798142816,19.8482083585711,20.8465369028605,21.8448654471499,
22.8431939914394,23.8415225357288,24.8398510800182,25.8381796243077,26.8365081685971,
27.8348367128865,28.833165257176,29.8314938014654,30.8298223457548,31.8285807653119),
 .UNSPECIFIED.) ;
#914 = B_SPLINE_SURFACE_WITH_KNOTS('',3,3,((#67087,#67088,#67089,#67090,#67091,
#67092,#67093,#67094,#67095,#67096,#67097,#67098,#67099,#67100,#67101,#67102,
#67103,#67104,#67105,#67106,#67107,#67108,#67109),(#67110,#67111,#67112,
#67113,#67114,#67115,#67116,#67117,#67118,#67119,#67120,#67121,#67122,#67123,
#67124,#67125,#67126,#67127,#67128,#67129,#67130,#67131,#67132),(#67133,
#67134,#67135,#67136,#67137,#67138,#67139,#67140,#67141,#67142,#67143,#67144,
#67145,#67146,#67147,#67148,#67149,#67150,#67151,#67152,#67153,#67154,#67155),
(#67156,#67157,#67158,#67159,#67160,#67161,#67162,#67163,#67164,#67165,
#67166,#67167,#67168,#67169,#67170,#67171,#67172,#67173,#67174,#67175,#67176,
#67177,#67178)),.UNSPECIFIED.,.F.,.F.,.F.,(4,4),(4,1,1,1,1,1,1,1,1,1,1,
1,1,1,1,1,1,1,1,1,4),(-0.000645665255431383,0.0452750015650409),(14.3976846920928,
15.3964695570661,16.3947981013555,17.3931266456449,18.3914551899343,19.3897837342237,
20.3881122785131,21.3864408228024,22.3847693670918,23.3830979113812,24.3814264556706,
25.37975499996,26.3780835442494,27.3764120885388,28.3747406328282,29.3730691771176,
30.3713977214069,31.3697262656963,32.3680548099857,33.3663833542751,34.3650979167),
 .UNSPECIFIED.) ;
#915 = B_SPLINE_SURFACE_WITH_KNOTS('',3,3,((#67354,#67355,#67356,#67357,#67358,
#67359,#67360,#67361,#67362,#67363,#67364,#67365,#67366,#67367,#67368,#67369,
#67370,#67371,#67372,#67373,#67374,#67375,#67376),(#67377,#67378,#67379,
#67380,#67381,#67382,#67383,#67384,#67385,#67386,#67387,#67388,#67389,#67390,
#67391,#67392,#67393,#67394,#67395,#67396,#67397,#67398,#67399),(#67400,
#67401,#67402,#67403,#67404,#67405,#67406,#67407,#67408,#67409,#67410,#67411,
#67412,#67413,#67414,#67415,#67416,#67417,#67418,#67419,#67420,#67421,#67422),
(#67423,#67424,#67425,#67426,#67427,#67428,#67429,#67430,#67431,#67432,
#67433,#67434,#67435,#67436,#67437,#67438,#67439,#67440,#67441,#67442,#67443,
#67444,#67445)),.UNSPECIFIED.,.F.,.F.,.F.,(4,4),(4,1,1,1,1,1,1,1,1,1,1,
1,1,1,1,1,1,1,1,1,4),(-0.000386017183284365,0.0458144387691291),(11.8611939870731,
12.8599085485457,13.8582370928351,14.8565656371245,15.8548941814139,16.8532227257033,
17.8515512699927,18.8498798142821,19.8482083585714,20.8465369028608,21.8448654471502,
22.8431939914396,23.841522535729,24.8398510800184,25.8381796243078,26.8365081685971,
27.8348367128865,28.8331652571759,29.8314938014653,30.8298223457547,31.8285834103066),
 .UNSPECIFIED.) ;
#916 = B_SPLINE_SURFACE_WITH_KNOTS('',3,3,((#67621,#67622,#67623,#67624,#67625,
#67626,#67627,#67628,#67629,#67630,#67631,#67632,#67633,#67634,#67635,#67636,
#67637,#67638,#67639,#67640,#67641,#67642,#67643),(#67644,#67645,#67646,
#67647,#67648,#67649,#67650,#67651,#67652,#67653,#67654,#67655,#67656,#67657,
#67658,#67659,#67660,#67661,#67662,#67663,#67664,#67665,#67666),(#67667,
#67668,#67669,#67670,#67671,#67672,#67673,#67674,#67675,#67676,#67677,#67678,
#67679,#67680,#67681,#67682,#67683,#67684,#67685,#67686,#67687,#67688,#67689),
(#67690,#67691,#67692,#67693,#67694,#67695,#67696,#67697,#67698,#67699,
#67700,#67701,#67702,#67703,#67704,#67705,#67706,#67707,#67708,#67709,#67710,
#67711,#67712)),.UNSPECIFIED.,.F.,.F.,.F.,(4,4),(4,1,1,1,1,1,1,1,1,1,1,
1,1,1,1,1,1,1,1,1,4),(-0.000641741025930388,0.0452726121833519),(14.3976874611935,
15.3964695570662,16.3947981013556,17.393126645645,18.3914551899344,19.3897837342237,
20.3881122785131,21.3864408228025,22.3847693670919,23.3830979113813,24.3814264556707,
25.37975499996,26.3780835442494,27.3764120885388,28.3747406328282,29.3730691771176,
30.371397721407,31.3697262656963,32.3680548099857,33.3663833542751,34.3650955273184),
 .UNSPECIFIED.) ;
#917 = B_SPLINE_SURFACE_WITH_KNOTS('',3,3,((#67888,#67889,#67890,#67891,#67892,
#67893,#67894,#67895,#67896,#67897,#67898,#67899,#67900,#67901,#67902,#67903,
#67904,#67905,#67906,#67907,#67908,#67909,#67910),(#67911,#67912,#67913,
#67914,#67915,#67916,#67917,#67918,#67919,#67920,#67921,#67922,#67923,#67924,
#67925,#67926,#67927,#67928,#67929,#67930,#67931,#67932,#67933),(#67934,
#67935,#67936,#67937,#67938,#67939,#67940,#67941,#67942,#67943,#67944,#67945,
#67946,#67947,#67948,#67949,#67950,#67951,#67952,#67953,#67954,#67955,#67956),
(#67957,#67958,#67959,#67960,#67961,#67962,#67963,#67964,#67965,#67966,
#67967,#67968,#67969,#67970,#67971,#67972,#67973,#67974,#67975,#67976,#67977,
#67978,#67979)),.UNSPECIFIED.,.F.,.F.,.F.,(4,4),(4,1,1,1,1,1,1,1,1,1,1,
1,1,1,1,1,1,1,1,1,4),(-0.000383627530710749,0.0458040974015815),(11.8611963767258,
12.8599085485459,13.8582370928353,14.8565656371247,15.8548941814141,16.8532227257035,
17.8515512699929,18.8498798142822,19.8482083585716,20.846536902861,21.8448654471504,
22.8431939914398,23.8415225357292,24.8398510800186,25.8381796243079,26.8365081685973,
27.8348367128867,28.8331652571761,29.8314938014655,30.8298223457549,31.8285735830159),
 .UNSPECIFIED.) ;
#918 = B_SPLINE_SURFACE_WITH_KNOTS('',3,3,((#68155,#68156,#68157,#68158,#68159,
#68160,#68161,#68162,#68163,#68164,#68165,#68166,#68167,#68168,#68169,#68170,
#68171,#68172,#68173,#68174,#68175,#68176,#68177),(#68178,#68179,#68180,
#68181,#68182,#68183,#68184,#68185,#68186,#68187,#68188,#68189,#68190,#68191,
#68192,#68193,#68194,#68195,#68196,#68197,#68198,#68199,#68200),(#68201,
#68202,#68203,#68204,#68205,#68206,#68207,#68208,#68209,#68210,#68211,#68212,
#68213,#68214,#68215,#68216,#68217,#68218,#68219,#68220,#68221,#68222,#68223),
(#68224,#68225,#68226,#68227,#68228,#68229,#68230,#68231,#68232,#68233,
#68234,#68235,#68236,#68237,#68238,#68239,#68240,#68241,#68242,#68243,#68244,
#68245,#68246)),.UNSPECIFIED.,.F.,.F.,.F.,(4,4),(4,1,1,1,1,1,1,1,1,1,1,
1,1,1,1,1,1,1,1,1,4),(-0.000643140498361754,0.0452734766386899),(14.3976864560211,
15.3964695570662,16.3947981013556,17.3931266456449,18.3914551899343,19.3897837342237,
20.3881122785131,21.3864408228024,22.3847693670918,23.3830979113812,24.3814264556706,
25.3797549999599,26.3780835442493,27.3764120885387,28.3747406328281,29.3730691771174,
30.3713977214068,31.3697262656962,32.3680548099856,33.3663833542749,34.3650963917735),
 .UNSPECIFIED.) ;
#919 = B_SPLINE_SURFACE_WITH_KNOTS('',3,3,((#68422,#68423,#68424,#68425,#68426,
#68427,#68428,#68429,#68430,#68431,#68432,#68433,#68434,#68435,#68436,#68437,
#68438,#68439,#68440,#68441,#68442,#68443,#68444),(#68445,#68446,#68447,
#68448,#68449,#68450,#68451,#68452,#68453,#68454,#68455,#68456,#68457,#68458,
#68459,#68460,#68461,#68462,#68463,#68464,#68465,#68466,#68467),(#68468,
#68469,#68470,#68471,#68472,#68473,#68474,#68475,#68476,#68477,#68478,#68479,
#68480,#68481,#68482,#68483,#68484,#68485,#68486,#68487,#68488,#68489,#68490),
(#68491,#68492,#68493,#68494,#68495,#68496,#68497,#68498,#68499,#68500,
#68501,#68502,#68503,#68504,#68505,#68506,#68507,#68508,#68509,#68510,#68511,
#68512,#68513)),.UNSPECIFIED.,.F.,.F.,.F.,(4,4),(4,1,1,1,1,1,1,1,1,1,1,
1,1,1,1,1,1,1,1,1,4),(-0.000384492090036841,0.0458077183624923),(11.8611955121666,
12.859908548546,13.8582370928354,14.8565656371247,15.8548941814141,16.8532227257035,
17.8515512699929,18.8498798142823,19.8482083585716,20.846536902861,21.8448654471504,
22.8431939914398,23.8415225357292,24.8398510800185,25.8381796243079,26.8365081685973,
27.8348367128867,28.833165257176,29.8314938014654,30.8298223457548,31.8285770053882),
 .UNSPECIFIED.) ;
#920 = B_SPLINE_SURFACE_WITH_KNOTS('',3,3,((#68901,#68902,#68903,#68904,#68905,
#68906,#68907,#68908,#68909,#68910,#68911,#68912,#68913,#68914,#68915,#68916,
#68917,#68918,#68919,#68920,#68921,#68922,#68923),(#68924,#68925,#68926,
#68927,#68928,#68929,#68930,#68931,#68932,#68933,#68934,#68935,#68936,#68937,
#68938,#68939,#68940,#68941,#68942,#68943,#68944,#68945,#68946),(#68947,
#68948,#68949,#68950,#68951,#68952,#68953,#68954,#68955,#68956,#68957,#68958,
#68959,#68960,#68961,#68962,#68963,#68964,#68965,#68966,#68967,#68968,#68969),
(#68970,#68971,#68972,#68973,#68974,#68975,#68976,#68977,#68978,#68979,
#68980,#68981,#68982,#68983,#68984,#68985,#68986,#68987,#68988,#68989,#68990,
#68991,#68992)),.UNSPECIFIED.,.F.,.F.,.F.,(4,4),(4,1,1,1,1,1,1,1,1,1,1,
1,1,1,1,1,1,1,1,1,4),(-0.000646812714374105,0.0452756796923178),(14.3976839116802,
15.3964695570661,16.3947981013555,17.3931266456449,18.3914551899343,19.3897837342237,
20.3881122785131,21.3864408228024,22.3847693670918,23.3830979113812,24.3814264556706,
25.37975499996,26.3780835442494,27.3764120885387,28.3747406328281,29.3730691771175,
30.3713977214069,31.3697262656963,32.3680548099857,33.3663833542751,34.3650985948273),
 .UNSPECIFIED.) ;
#921 = B_SPLINE_SURFACE_WITH_KNOTS('',3,3,((#69075,#69076,#69077,#69078,#69079,
#69080,#69081,#69082,#69083,#69084,#69085,#69086,#69087,#69088,#69089,#69090,
#69091,#69092,#69093,#69094,#69095,#69096,#69097),(#69098,#69099,#69100,
#69101,#69102,#69103,#69104,#69105,#69106,#69107,#69108,#69109,#69110,#69111,
#69112,#69113,#69114,#69115,#69116,#69117,#69118,#69119,#69120),(#69121,
#69122,#69123,#69124,#69125,#69126,#69127,#69128,#69129,#69130,#69131,#69132,
#69133,#69134,#69135,#69136,#69137,#69138,#69139,#69140,#69141,#69142,#69143),
(#69144,#69145,#69146,#69147,#69148,#69149,#69150,#69151,#69152,#69153,
#69154,#69155,#69156,#69157,#69158,#69159,#69160,#69161,#69162,#69163,#69164,
#69165,#69166)),.UNSPECIFIED.,.F.,.F.,.F.,(4,4),(4,1,1,1,1,1,1,1,1,1,1,
1,1,1,1,1,1,1,1,1,4),(-0.000386695378374584,0.0458175667348162),(11.861193308878,
12.8599085485458,13.8582370928352,14.8565656371246,15.854894181414,16.8532227257034,
17.8515512699928,18.8498798142822,19.8482083585716,20.846536902861,21.8448654471503,
22.8431939914397,23.8415225357291,24.8398510800185,25.8381796243079,26.8365081685973,
27.8348367128867,28.8331652571761,29.8314938014655,30.8298223457549,31.8285864107338),
 .UNSPECIFIED.) ;
#922 = B_SPLINE_SURFACE_WITH_KNOTS('',3,3,((#74438,#74439,#74440,#74441,#74442,
#74443),(#74444,#74445,#74446,#74447,#74448,#74449),(#74450,#74451,#74452,
#74453,#74454,#74455),(#74456,#74457,#74458,#74459,#74460,#74461)),
 .UNSPECIFIED.,.F.,.F.,.F.,(4,4),(4,2,4),(0.,1.),(-0.0362588513985796,-0.0343987133118532,
0.),.UNSPECIFIED.) ;
#923 = B_SPLINE_SURFACE_WITH_KNOTS('',3,3,((#74478,#74479,#74480,#74481),
(#74482,#74483,#74484,#74485),(#74486,#74487,#74488,#74489),(#74490,#74491,
#74492,#74493),(#74494,#74495,#74496,#74497)),.UNSPECIFIED.,.F.,.F.,.F.,
(4,1,4),(4,4),(0.,0.571428571428571,1.),(0.,0.00945665398132608),
 .UNSPECIFIED.) ;
#924 = B_SPLINE_SURFACE_WITH_KNOTS('',3,3,((#74513,#74514,#74515,#74516,#74517),
(#74518,#74519,#74520,#74521,#74522),(#74523,#74524,#74525,#74526,#74527),
(#74528,#74529,#74530,#74531,#74532),(#74533,#74534,#74535,#74536,#74537)),
 .UNSPECIFIED.,.F.,.F.,.F.,(4,1,4),(4,1,4),(0.,0.571428571428571,1.),(0.,
0.0040902611621181,0.00954394271160891),.UNSPECIFIED.) ;
#925 = B_SPLINE_SURFACE_WITH_KNOTS('',3,3,((#74551,#74552,#74553,#74554),
(#74555,#74556,#74557,#74558),(#74559,#74560,#74561,#74562),(#74563,#74564,
#74565,#74566),(#74567,#74568,#74569,#74570)),.UNSPECIFIED.,.F.,.F.,.F.,
(4,1,4),(4,4),(0.,0.571428571428571,1.),(0.126991784547804,0.128026026143509),
 .UNSPECIFIED.) ;
#926 = B_SPLINE_SURFACE_WITH_KNOTS('',3,3,((#74576,#74577,#74578,#74579,#74580,
#74581,#74582,#74583),(#74584,#74585,#74586,#74587,#74588,#74589,#74590,
#74591),(#74592,#74593,#74594,#74595,#74596,#74597,#74598,#74599),(#74600,
#74601,#74602,#74603,#74604,#74605,#74606,#74607),(#74608,#74609,#74610,
#74611,#74612,#74613,#74614,#74615),(#74616,#74617,#74618,#74619,#74620,
#74621,#74622,#74623),(#74624,#74625,#74626,#74627,#74628,#74629,#74630,
#74631),(#74632,#74633,#74634,#74635,#74636,#74637,#74638,#74639),(#74640,
#74641,#74642,#74643,#74644,#74645,#74646,#74647)),.UNSPECIFIED.,.F.,.F.,
 .F.,(4,1,1,1,1,1,4),(4,2,1,1,4),(0.,0.714285714285714,0.857142857142857,
0.928571428571429,0.964285714285714,0.982142857142857,1.00710268589528),
(-0.000154777169791509,0.,0.00161206075000591,0.00241809112500886,0.00444864477949539),
 .UNSPECIFIED.) ;
#927 = B_SPLINE_SURFACE_WITH_KNOTS('',3,3,((#74661,#74662,#74663,#74664),
(#74665,#74666,#74667,#74668),(#74669,#74670,#74671,#74672),(#74673,#74674,
#74675,#74676),(#74677,#74678,#74679,#74680)),.UNSPECIFIED.,.F.,.F.,.F.,
(4,1,4),(4,4),(0.,0.571428571428571,1.),(0.,0.00216800481456508),
 .UNSPECIFIED.) ;
#928 = B_SPLINE_SURFACE_WITH_KNOTS('',3,3,((#74689,#74690,#74691,#74692,#74693,
#74694,#74695,#74696,#74697),(#74698,#74699,#74700,#74701,#74702,#74703,
#74704,#74705,#74706),(#74707,#74708,#74709,#74710,#74711,#74712,#74713,
#74714,#74715),(#74716,#74717,#74718,#74719,#74720,#74721,#74722,#74723,
#74724),(#74725,#74726,#74727,#74728,#74729,#74730,#74731,#74732,#74733)),
 .UNSPECIFIED.,.F.,.F.,.F.,(4,1,4),(4,1,1,1,1,1,4),(0.,0.571428571428571,
1.),(1.11022302462521E-16,0.000121096313570565,0.00024219262714102,0.000363288940711474,
0.000484385254281929,0.00145315576284556,0.00339069677997283),
 .UNSPECIFIED.) ;
#929 = B_SPLINE_SURFACE_WITH_KNOTS('',3,3,((#74755,#74756,#74757,#74758),
(#74759,#74760,#74761,#74762),(#74763,#74764,#74765,#74766),(#74767,#74768,
#74769,#74770)),.UNSPECIFIED.,.F.,.F.,.F.,(4,4),(4,4),(0.,0.47085965842338),
(0.179999904671396,0.182852270042874),.UNSPECIFIED.) ;
#930 = B_SPLINE_SURFACE_WITH_KNOTS('',3,3,((#74826,#74827,#74828,#74829,#74830,
#74831),(#74832,#74833,#74834,#74835,#74836,#74837),(#74838,#74839,#74840,
#74841,#74842,#74843),(#74844,#74845,#74846,#74847,#74848,#74849)),
 .UNSPECIFIED.,.F.,.F.,.F.,(4,4),(4,2,4),(0.,1.),(-0.00186013808672659,
0.,0.0343987133118501),.UNSPECIFIED.) ;
#931 = B_SPLINE_SURFACE_WITH_KNOTS('',3,3,((#74858,#74859,#74860,#74861),
(#74862,#74863,#74864,#74865),(#74866,#74867,#74868,#74869),(#74870,#74871,
#74872,#74873),(#74874,#74875,#74876,#74877)),.UNSPECIFIED.,.F.,.F.,.F.,
(4,1,4),(4,4),(0.,0.571428571428571,1.),(7.96865975725692E-14,0.00945665401173728),
 .UNSPECIFIED.) ;
#932 = B_SPLINE_SURFACE_WITH_KNOTS('',3,3,((#74890,#74891,#74892,#74893,#74894),
(#74895,#74896,#74897,#74898,#74899),(#74900,#74901,#74902,#74903,#74904),
(#74905,#74906,#74907,#74908,#74909),(#74910,#74911,#74912,#74913,#74914)),
 .UNSPECIFIED.,.F.,.F.,.F.,(4,1,4),(4,1,4),(0.,0.571428571428571,1.),(0.,
0.00545368154943955,0.00954394271151922),.UNSPECIFIED.) ;
#933 = B_SPLINE_SURFACE_WITH_KNOTS('',3,3,((#74922,#74923,#74924,#74925),
(#74926,#74927,#74928,#74929),(#74930,#74931,#74932,#74933),(#74934,#74935,
#74936,#74937),(#74938,#74939,#74940,#74941)),.UNSPECIFIED.,.F.,.F.,.F.,
(4,1,4),(4,4),(0.,0.571428571428571,1.),(0.126991784443102,0.128026026038763),
 .UNSPECIFIED.) ;
#934 = B_SPLINE_SURFACE_WITH_KNOTS('',3,3,((#74945,#74946,#74947,#74948,#74949,
#74950,#74951,#74952,#74953),(#74954,#74955,#74956,#74957,#74958,#74959,
#74960,#74961,#74962),(#74963,#74964,#74965,#74966,#74967,#74968,#74969,
#74970,#74971),(#74972,#74973,#74974,#74975,#74976,#74977,#74978,#74979,
#74980),(#74981,#74982,#74983,#74984,#74985,#74986,#74987,#74988,#74989)),
 .UNSPECIFIED.,.F.,.F.,.F.,(4,1,4),(4,1,1,1,2,4),(0.,0.571428571428571,
1.),(0.,0.000799914108848609,0.00159982821769722,0.00239974232654583,0.00399957054424305,
0.00418497063961359),.UNSPECIFIED.) ;
#935 = B_SPLINE_SURFACE_WITH_KNOTS('',3,3,((#75017,#75018,#75019,#75020),
(#75021,#75022,#75023,#75024),(#75025,#75026,#75027,#75028),(#75029,#75030,
#75031,#75032),(#75033,#75034,#75035,#75036)),.UNSPECIFIED.,.F.,.F.,.F.,
(4,1,4),(4,4),(0.,0.571428571428571,1.),(0.,0.00216800481456542),
 .UNSPECIFIED.) ;
#936 = B_SPLINE_SURFACE_WITH_KNOTS('',3,3,((#75045,#75046,#75047,#75048,#75049,
#75050,#75051,#75052,#75053),(#75054,#75055,#75056,#75057,#75058,#75059,
#75060,#75061,#75062),(#75063,#75064,#75065,#75066,#75067,#75068,#75069,
#75070,#75071),(#75072,#75073,#75074,#75075,#75076,#75077,#75078,#75079,
#75080),(#75081,#75082,#75083,#75084,#75085,#75086,#75087,#75088,#75089)),
 .UNSPECIFIED.,.F.,.F.,.F.,(4,1,4),(4,1,1,1,1,1,4),(0.,0.571428571428571,
1.),(0.,0.000121096313570718,0.000242192627141436,0.000363288940712154,
0.000484385254282872,0.00145315576284862,0.00339069677998011),
 .UNSPECIFIED.) ;
#937 = B_SPLINE_SURFACE_WITH_KNOTS('',3,3,((#75129,#75130,#75131,#75132,#75133,
#75134),(#75135,#75136,#75137,#75138,#75139,#75140),(#75141,#75142,#75143,
#75144,#75145,#75146),(#75147,#75148,#75149,#75150,#75151,#75152)),
 .UNSPECIFIED.,.F.,.F.,.F.,(4,4),(4,2,4),(0.,1.),(-0.0362588513985796,-0.0343987133118529,
0.),.UNSPECIFIED.) ;
#938 = B_SPLINE_SURFACE_WITH_KNOTS('',3,3,((#75161,#75162,#75163,#75164),
(#75165,#75166,#75167,#75168),(#75169,#75170,#75171,#75172),(#75173,#75174,
#75175,#75176),(#75177,#75178,#75179,#75180)),.UNSPECIFIED.,.F.,.F.,.F.,
(4,1,4),(4,4),(0.,0.571428571428571,1.),(0.,0.00945665398132565),
 .UNSPECIFIED.) ;
#939 = B_SPLINE_SURFACE_WITH_KNOTS('',3,3,((#75196,#75197,#75198,#75199,#75200),
(#75201,#75202,#75203,#75204,#75205),(#75206,#75207,#75208,#75209,#75210),
(#75211,#75212,#75213,#75214,#75215),(#75216,#75217,#75218,#75219,#75220)),
 .UNSPECIFIED.,.F.,.F.,.F.,(4,1,4),(4,1,4),(0.,0.571428571428571,1.),(5.7658280050909E-17,
0.00409026116211842,0.00954394271160956),.UNSPECIFIED.) ;
#940 = B_SPLINE_SURFACE_WITH_KNOTS('',3,3,((#75234,#75235,#75236,#75237),
(#75238,#75239,#75240,#75241),(#75242,#75243,#75244,#75245),(#75246,#75247,
#75248,#75249),(#75250,#75251,#75252,#75253)),.UNSPECIFIED.,.F.,.F.,.F.,
(4,1,4),(4,4),(0.,0.571428571428571,1.),(0.253983569095608,0.255017810691314),
 .UNSPECIFIED.) ;
#941 = B_SPLINE_SURFACE_WITH_KNOTS('',3,3,((#75259,#75260,#75261,#75262,#75263,
#75264,#75265,#75266,#75267),(#75268,#75269,#75270,#75271,#75272,#75273,
#75274,#75275,#75276),(#75277,#75278,#75279,#75280,#75281,#75282,#75283,
#75284,#75285),(#75286,#75287,#75288,#75289,#75290,#75291,#75292,#75293,
#75294),(#75295,#75296,#75297,#75298,#75299,#75300,#75301,#75302,#75303)),
 .UNSPECIFIED.,.F.,.F.,.F.,(4,1,4),(4,2,1,1,1,4),(0.,0.571428571428571,
1.00181493187422),(-0.000154790814778927,0.,0.00161206074594362,0.00241809111891543,
0.00322412149188724,0.00444864613282186),.UNSPECIFIED.) ;
#942 = B_SPLINE_SURFACE_WITH_KNOTS('',3,3,((#75370,#75371,#75372,#75373),
(#75374,#75375,#75376,#75377),(#75378,#75379,#75380,#75381),(#75382,#75383,
#75384,#75385),(#75386,#75387,#75388,#75389)),.UNSPECIFIED.,.F.,.F.,.F.,
(4,1,4),(4,4),(0.,0.571428571428571,1.),(1.21699733691425E-15,0.00216800481456625),
 .UNSPECIFIED.) ;
#943 = B_SPLINE_SURFACE_WITH_KNOTS('',3,3,((#75398,#75399,#75400,#75401,#75402,
#75403,#75404,#75405,#75406),(#75407,#75408,#75409,#75410,#75411,#75412,
#75413,#75414,#75415),(#75416,#75417,#75418,#75419,#75420,#75421,#75422,
#75423,#75424),(#75425,#75426,#75427,#75428,#75429,#75430,#75431,#75432,
#75433),(#75434,#75435,#75436,#75437,#75438,#75439,#75440,#75441,#75442)),
 .UNSPECIFIED.,.F.,.F.,.F.,(4,1,4),(4,1,1,1,1,1,4),(0.,0.571428571428571,
1.),(2.74316139050604E-16,0.000121096313570731,0.000242192627141187,0.0004843852542821,
0.000968770508563926,0.00193754101712758,0.00339069677997306),
 .UNSPECIFIED.) ;
#944 = B_SPLINE_SURFACE_WITH_KNOTS('',3,3,((#75462,#75463,#75464,#75465),
(#75466,#75467,#75468,#75469),(#75470,#75471,#75472,#75473),(#75474,#75475,
#75476,#75477)),.UNSPECIFIED.,.F.,.F.,.F.,(4,4),(4,4),(0.,0.470859658423347),
(0.179999904671396,0.182852270042875),.UNSPECIFIED.) ;
#945 = B_SPLINE_SURFACE_WITH_KNOTS('',3,3,((#75491,#75492,#75493,#75494,#75495,
#75496),(#75497,#75498,#75499,#75500,#75501,#75502),(#75503,#75504,#75505,
#75506,#75507,#75508),(#75509,#75510,#75511,#75512,#75513,#75514)),
 .UNSPECIFIED.,.F.,.F.,.F.,(4,4),(4,2,4),(0.,1.),(-0.00186013808672611,
0.,0.0343987133118504),.UNSPECIFIED.) ;
#946 = B_SPLINE_SURFACE_WITH_KNOTS('',3,3,((#75523,#75524,#75525,#75526),
(#75527,#75528,#75529,#75530),(#75531,#75532,#75533,#75534),(#75535,#75536,
#75537,#75538),(#75539,#75540,#75541,#75542)),.UNSPECIFIED.,.F.,.F.,.F.,
(4,1,4),(4,4),(0.,0.571428571428571,1.),(7.97441283497418E-14,0.00945665401173742),
 .UNSPECIFIED.) ;
#947 = B_SPLINE_SURFACE_WITH_KNOTS('',3,3,((#75555,#75556,#75557,#75558,#75559),
(#75560,#75561,#75562,#75563,#75564),(#75565,#75566,#75567,#75568,#75569),
(#75570,#75571,#75572,#75573,#75574),(#75575,#75576,#75577,#75578,#75579)),
 .UNSPECIFIED.,.F.,.F.,.F.,(4,1,4),(4,1,4),(0.,0.571428571428571,1.),(0.,
0.00409026116207964,0.00954394271151917),.UNSPECIFIED.) ;
#948 = B_SPLINE_SURFACE_WITH_KNOTS('',3,3,((#75587,#75588,#75589,#75590),
(#75591,#75592,#75593,#75594),(#75595,#75596,#75597,#75598),(#75599,#75600,
#75601,#75602),(#75603,#75604,#75605,#75606)),.UNSPECIFIED.,.F.,.F.,.F.,
(4,1,4),(4,4),(0.,0.571428571428571,1.),(0.126991784443102,0.128026026038763),
 .UNSPECIFIED.) ;
#949 = B_SPLINE_SURFACE_WITH_KNOTS('',3,3,((#75610,#75611,#75612,#75613,#75614,
#75615,#75616,#75617,#75618),(#75619,#75620,#75621,#75622,#75623,#75624,
#75625,#75626,#75627),(#75628,#75629,#75630,#75631,#75632,#75633,#75634,
#75635,#75636),(#75637,#75638,#75639,#75640,#75641,#75642,#75643,#75644,
#75645),(#75646,#75647,#75648,#75649,#75650,#75651,#75652,#75653,#75654)),
 .UNSPECIFIED.,.F.,.F.,.F.,(4,1,4),(4,1,1,1,2,4),(0.,0.571428571428571,
1.),(0.,0.000799914107796385,0.00159982821559277,0.00239974232338915,0.00399957053898192,
0.00418493275019483),.UNSPECIFIED.) ;
#950 = B_SPLINE_SURFACE_WITH_KNOTS('',3,3,((#75682,#75683,#75684,#75685),
(#75686,#75687,#75688,#75689),(#75690,#75691,#75692,#75693),(#75694,#75695,
#75696,#75697),(#75698,#75699,#75700,#75701)),.UNSPECIFIED.,.F.,.F.,.F.,
(4,1,4),(4,4),(0.,0.571428571428571,1.),(0.,0.00216800481456436),
 .UNSPECIFIED.) ;
#951 = B_SPLINE_SURFACE_WITH_KNOTS('',3,3,((#75710,#75711,#75712,#75713,#75714,
#75715,#75716,#75717,#75718),(#75719,#75720,#75721,#75722,#75723,#75724,
#75725,#75726,#75727),(#75728,#75729,#75730,#75731,#75732,#75733,#75734,
#75735,#75736),(#75737,#75738,#75739,#75740,#75741,#75742,#75743,#75744,
#75745),(#75746,#75747,#75748,#75749,#75750,#75751,#75752,#75753,#75754)),
 .UNSPECIFIED.,.F.,.F.,.F.,(4,1,4),(4,1,1,1,1,1,4),(0.,0.571428571428571,
1.),(0.,0.000121096313570705,0.00024219262714141,0.000363288940712115,0.00048438525428282,
0.00145315576284846,0.00339069677997974),.UNSPECIFIED.) ;
#952 = B_SPLINE_SURFACE_WITH_KNOTS('',3,3,((#75790,#75791,#75792,#75793),
(#75794,#75795,#75796,#75797),(#75798,#75799,#75800,#75801),(#75802,#75803,
#75804,#75805)),.UNSPECIFIED.,.F.,.F.,.F.,(4,4),(4,4),(0.,1.),(-1.5707963267949,
-0.0872664625997159),.UNSPECIFIED.) ;
#953 = B_SPLINE_SURFACE_WITH_KNOTS('',3,3,((#75846,#75847,#75848,#75849,#75850,
#75851),(#75852,#75853,#75854,#75855,#75856,#75857),(#75858,#75859,#75860,
#75861,#75862,#75863),(#75864,#75865,#75866,#75867,#75868,#75869),(#75870,
#75871,#75872,#75873,#75874,#75875)),.UNSPECIFIED.,.F.,.F.,.F.,(4,1,4),
(4,2,4),(0.,0.571428571428571,1.),(0.,0.0361627499148956,0.0364117611345324),
 .UNSPECIFIED.) ;
#954 = B_SPLINE_SURFACE_WITH_KNOTS('',3,3,((#75884,#75885,#75886,#75887),
(#75888,#75889,#75890,#75891),(#75892,#75893,#75894,#75895),(#75896,#75897,
#75898,#75899),(#75900,#75901,#75902,#75903)),.UNSPECIFIED.,.F.,.F.,.F.,
(4,1,4),(4,4),(0.,0.571428571428571,1.),(2.33694858927792E-16,0.00331127956228568),
 .UNSPECIFIED.) ;
#955 = B_SPLINE_SURFACE_WITH_KNOTS('',3,3,((#75907,#75908,#75909,#75910),
(#75911,#75912,#75913,#75914),(#75915,#75916,#75917,#75918),(#75919,#75920,
#75921,#75922),(#75923,#75924,#75925,#75926)),.UNSPECIFIED.,.F.,.F.,.F.,
(4,1,4),(4,4),(0.,0.571428571428571,1.00022442227795),(-0.00022442227795638,
0.146595920707548),.UNSPECIFIED.) ;
#956 = B_SPLINE_SURFACE_WITH_KNOTS('',3,3,((#75946,#75947,#75948,#75949),
(#75950,#75951,#75952,#75953),(#75954,#75955,#75956,#75957),(#75958,#75959,
#75960,#75961),(#75962,#75963,#75964,#75965)),.UNSPECIFIED.,.F.,.F.,.F.,
(4,1,4),(4,4),(-0.000224423998443304,0.571428571428571,1.),(-0.000224423998443185,
0.146595922429139),.UNSPECIFIED.) ;
#957 = B_SPLINE_SURFACE_WITH_KNOTS('',3,3,((#75981,#75982,#75983,#75984),
(#75985,#75986,#75987,#75988),(#75989,#75990,#75991,#75992),(#75993,#75994,
#75995,#75996),(#75997,#75998,#75999,#76000)),.UNSPECIFIED.,.F.,.F.,.F.,
(4,1,4),(4,4),(0.,0.571428571428571,1.),(1.76333003250469E-16,0.00331127956228543),
 .UNSPECIFIED.) ;
#958 = B_SPLINE_SURFACE_WITH_KNOTS('',3,3,((#76006,#76007,#76008,#76009,#76010,
#76011),(#76012,#76013,#76014,#76015,#76016,#76017),(#76018,#76019,#76020,
#76021,#76022,#76023),(#76024,#76025,#76026,#76027,#76028,#76029),(#76030,
#76031,#76032,#76033,#76034,#76035)),.UNSPECIFIED.,.F.,.F.,.F.,(4,1,4),
(4,2,4),(0.,0.571428571428571,1.),(8.84614312661979E-17,0.0361913306097799,
0.0364133025372201),.UNSPECIFIED.) ;
#959 = B_SPLINE_SURFACE_WITH_KNOTS('',3,3,((#76063,#76064,#76065,#76066),
(#76067,#76068,#76069,#76070),(#76071,#76072,#76073,#76074),(#76075,#76076,
#76077,#76078)),.UNSPECIFIED.,.F.,.F.,.F.,(4,4),(4,4),(0.,1.),(-1.5707963267949,
-0.0872664625997159),.UNSPECIFIED.) ;
#960 = B_SPLINE_SURFACE_WITH_KNOTS('',3,3,((#76109,#76110,#76111,#76112),
(#76113,#76114,#76115,#76116),(#76117,#76118,#76119,#76120),(#76121,#76122,
#76123,#76124),(#76125,#76126,#76127,#76128)),.UNSPECIFIED.,.F.,.F.,.F.,
(4,1,4),(4,4),(0.,0.571428571428571,1.00022442227796),(-0.000224422277962333,
0.146595920707853),.UNSPECIFIED.) ;
#961 = B_SPLINE_SURFACE_WITH_KNOTS('',3,3,((#76144,#76145,#76146,#76147),
(#76148,#76149,#76150,#76151),(#76152,#76153,#76154,#76155),(#76156,#76157,
#76158,#76159),(#76160,#76161,#76162,#76163)),.UNSPECIFIED.,.F.,.F.,.F.,
(4,1,4),(4,4),(0.,0.571428571428571,1.),(0.,0.00331127956228537),
 .UNSPECIFIED.) ;
#962 = B_SPLINE_SURFACE_WITH_KNOTS('',3,3,((#76169,#76170,#76171,#76172,#76173,
#76174),(#76175,#76176,#76177,#76178,#76179,#76180),(#76181,#76182,#76183,
#76184,#76185,#76186),(#76187,#76188,#76189,#76190,#76191,#76192),(#76193,
#76194,#76195,#76196,#76197,#76198)),.UNSPECIFIED.,.F.,.F.,.F.,(4,1,4),
(4,2,4),(0.,0.571428571428571,1.),(0.,0.0361629958429266,0.0364117772057813),
 .UNSPECIFIED.) ;
#963 = B_SPLINE_SURFACE_WITH_KNOTS('',3,3,((#76250,#76251,#76252,#76253),
(#76254,#76255,#76256,#76257),(#76258,#76259,#76260,#76261),(#76262,#76263,
#76264,#76265),(#76266,#76267,#76268,#76269)),.UNSPECIFIED.,.F.,.F.,.F.,
(4,1,4),(4,4),(-0.000224423998441357,0.571428571428571,1.),(-0.000224423998442386,
0.146595922428333),.UNSPECIFIED.) ;
#964 = B_SPLINE_SURFACE_WITH_KNOTS('',3,3,((#76276,#76277,#76278,#76279),
(#76280,#76281,#76282,#76283),(#76284,#76285,#76286,#76287),(#76288,#76289,
#76290,#76291),(#76292,#76293,#76294,#76295)),.UNSPECIFIED.,.F.,.F.,.F.,
(4,1,4),(4,4),(0.,0.571428571428571,1.),(1.64044101459669E-16,0.00331127956228544),
 .UNSPECIFIED.) ;
#965 = B_SPLINE_SURFACE_WITH_KNOTS('',3,3,((#76299,#76300,#76301,#76302,#76303,
#76304),(#76305,#76306,#76307,#76308,#76309,#76310),(#76311,#76312,#76313,
#76314,#76315,#76316),(#76317,#76318,#76319,#76320,#76321,#76322),(#76323,
#76324,#76325,#76326,#76327,#76328)),.UNSPECIFIED.,.F.,.F.,.F.,(4,1,4),
(4,2,4),(0.,0.571428571428571,1.),(0.,0.0361913306296307,0.0364133025382447),
 .UNSPECIFIED.) ;
#966 = B_SPLINE_SURFACE_WITH_KNOTS('',3,3,((#76349,#76350,#76351,#76352),
(#76353,#76354,#76355,#76356),(#76357,#76358,#76359,#76360),(#76361,#76362,
#76363,#76364)),.UNSPECIFIED.,.F.,.F.,.F.,(4,4),(4,4),(0.,1.),(-1.5707963267949,
-0.0872664625997158),.UNSPECIFIED.) ;
#967 = B_SPLINE_SURFACE_WITH_KNOTS('',3,3,((#76388,#76389,#76390,#76391),
(#76392,#76393,#76394,#76395),(#76396,#76397,#76398,#76399),(#76400,#76401,
#76402,#76403)),.UNSPECIFIED.,.F.,.F.,.F.,(4,4),(4,4),(0.,1.),(-1.5707963267949,
-0.0872664625997159),.UNSPECIFIED.) ;
#968 = B_SPLINE_SURFACE_WITH_KNOTS('',3,3,((#76425,#76426,#76427,#76428,#76429,
#76430,#76431,#76432,#76433,#76434),(#76435,#76436,#76437,#76438,#76439,
#76440,#76441,#76442,#76443,#76444),(#76445,#76446,#76447,#76448,#76449,
#76450,#76451,#76452,#76453,#76454),(#76455,#76456,#76457,#76458,#76459,
#76460,#76461,#76462,#76463,#76464)),.UNSPECIFIED.,.F.,.F.,.F.,(4,4),(4,
2,2,2,4),(-0.0343546625814549,1.0000001624628),(-0.32865367100704,-0.273443015535847,
-0.153352882404738,-0.0199317405198332,0.0415869283876659),
 .UNSPECIFIED.) ;
#969 = B_SPLINE_SURFACE_WITH_KNOTS('',3,3,((#76599,#76600,#76601,#76602,#76603,
#76604,#76605,#76606,#76607,#76608),(#76609,#76610,#76611,#76612,#76613,
#76614,#76615,#76616,#76617,#76618),(#76619,#76620,#76621,#76622,#76623,
#76624,#76625,#76626,#76627,#76628),(#76629,#76630,#76631,#76632,#76633,
#76634,#76635,#76636,#76637,#76638),(#76639,#76640,#76641,#76642,#76643,
#76644,#76645,#76646,#76647,#76648),(#76649,#76650,#76651,#76652,#76653,
#76654,#76655,#76656,#76657,#76658),(#76659,#76660,#76661,#76662,#76663,
#76664,#76665,#76666,#76667,#76668)),.UNSPECIFIED.,.F.,.F.,.F.,(4,1,1,1,
4),(4,2,2,2,4),(-0.000134967941931711,0.285714285714286,0.571428571428571,
0.857142857142857,1.00001222043739),(-0.408276645255811,-0.349022909463275,
-0.215144182724569,-0.094503731574,3.81138728867237E-14),.UNSPECIFIED.) ;
#970 = B_SPLINE_SURFACE_WITH_KNOTS('',3,3,((#77299,#77300,#77301,#77302,#77303,
#77304),(#77305,#77306,#77307,#77308,#77309,#77310),(#77311,#77312,#77313,
#77314,#77315,#77316),(#77317,#77318,#77319,#77320,#77321,#77322)),
 .UNSPECIFIED.,.F.,.F.,.F.,(4,4),(4,2,4),(0.,1.),(-0.0308408628658576,-0.0306076340858662,
0.),.UNSPECIFIED.) ;
#971 = B_SPLINE_SURFACE_WITH_KNOTS('',3,3,((#77341,#77342,#77343,#77344),
(#77345,#77346,#77347,#77348),(#77349,#77350,#77351,#77352),(#77353,#77354,
#77355,#77356),(#77357,#77358,#77359,#77360)),.UNSPECIFIED.,.F.,.F.,.F.,
(4,1,4),(4,4),(0.,0.571428571428571,1.),(0.,0.00359123636946031),
 .UNSPECIFIED.) ;
#972 = B_SPLINE_SURFACE_WITH_KNOTS('',3,3,((#77366,#77367,#77368,#77369),
(#77370,#77371,#77372,#77373),(#77374,#77375,#77376,#77377),(#77378,#77379,
#77380,#77381),(#77382,#77383,#77384,#77385)),.UNSPECIFIED.,.F.,.F.,.F.,
(4,1,4),(4,4),(0.,0.571428571428571,1.),(0.,0.0186228334819338),
 .UNSPECIFIED.) ;
#973 = B_SPLINE_SURFACE_WITH_KNOTS('',3,3,((#77428,#77429,#77430,#77431),
(#77432,#77433,#77434,#77435),(#77436,#77437,#77438,#77439),(#77440,#77441,
#77442,#77443),(#77444,#77445,#77446,#77447)),.UNSPECIFIED.,.F.,.F.,.F.,
(4,1,4),(4,4),(0.,0.571428571428571,1.),(0.,0.0186228334823064),
 .UNSPECIFIED.) ;
#974 = B_SPLINE_SURFACE_WITH_KNOTS('',3,3,((#77453,#77454,#77455,#77456),
(#77457,#77458,#77459,#77460),(#77461,#77462,#77463,#77464),(#77465,#77466,
#77467,#77468),(#77469,#77470,#77471,#77472)),.UNSPECIFIED.,.F.,.F.,.F.,
(4,1,4),(4,4),(0.,0.571428571428571,1.),(0.,0.00359123636948427),
 .UNSPECIFIED.) ;
#975 = B_SPLINE_SURFACE_WITH_KNOTS('',3,3,((#77477,#77478,#77479,#77480,#77481,
#77482),(#77483,#77484,#77485,#77486,#77487,#77488),(#77489,#77490,#77491,
#77492,#77493,#77494),(#77495,#77496,#77497,#77498,#77499,#77500),(#77501,
#77502,#77503,#77504,#77505,#77506)),.UNSPECIFIED.,.F.,.F.,.F.,(4,1,4),
(4,2,4),(0.,0.571428571428571,1.),(-0.0306076446211308,0.,0.000233218663520837),
 .UNSPECIFIED.) ;
#976 = B_SPLINE_SURFACE_WITH_KNOTS('',3,3,((#77539,#77540,#77541,#77542),
(#77543,#77544,#77545,#77546),(#77547,#77548,#77549,#77550),(#77551,#77552,
#77553,#77554)),.UNSPECIFIED.,.F.,.F.,.F.,(4,4),(4,4),(0.,1.),(0.0872664625997159,
1.5707963267949),.UNSPECIFIED.) ;
#977 = B_SPLINE_SURFACE_WITH_KNOTS('',3,3,((#77564,#77565,#77566,#77567,#77568),
(#77569,#77570,#77571,#77572,#77573),(#77574,#77575,#77576,#77577,#77578),
(#77579,#77580,#77581,#77582,#77583),(#77584,#77585,#77586,#77587,#77588)),
 .UNSPECIFIED.,.F.,.F.,.F.,(4,1,4),(4,1,4),(-0.00252299082537574,0.571428571428571,
1.00133658399285),(-1.34809870897391,-0.448243149014699,0.227279268661048),
 .UNSPECIFIED.) ;
#978 = B_SPLINE_SURFACE_WITH_KNOTS('',3,3,((#77620,#77621,#77622,#77623),
(#77624,#77625,#77626,#77627),(#77628,#77629,#77630,#77631),(#77632,#77633,
#77634,#77635)),.UNSPECIFIED.,.F.,.F.,.F.,(4,4),(4,4),(0.,1.),(0.0872664625997158,
1.5707963267949),.UNSPECIFIED.) ;
#979 = B_SPLINE_SURFACE_WITH_KNOTS('',3,3,((#77636,#77637,#77638,#77639,#77640),
(#77641,#77642,#77643,#77644,#77645),(#77646,#77647,#77648,#77649,#77650),
(#77651,#77652,#77653,#77654,#77655),(#77656,#77657,#77658,#77659,#77660)),
 .UNSPECIFIED.,.F.,.F.,.F.,(4,1,4),(4,1,4),(-0.00252299071549198,0.571428571428571,
1.00133658396291),(-0.227279268551174,0.44824314284206,1.34809869654654),
 .UNSPECIFIED.) ;
#980 = B_SPLINE_SURFACE_WITH_KNOTS('',3,3,((#77679,#77680,#77681,#77682),
(#77683,#77684,#77685,#77686),(#77687,#77688,#77689,#77690),(#77691,#77692,
#77693,#77694)),.UNSPECIFIED.,.F.,.F.,.F.,(4,4),(4,4),(0.,1.),(0.0872664625997159,
1.5707963267949),.UNSPECIFIED.) ;
#981 = B_SPLINE_SURFACE_WITH_KNOTS('',3,3,((#77724,#77725,#77726,#77727),
(#77728,#77729,#77730,#77731),(#77732,#77733,#77734,#77735),(#77736,#77737,
#77738,#77739)),.UNSPECIFIED.,.F.,.F.,.F.,(4,4),(4,4),(0.,1.),(0.0872664625997159,
1.5707963267949),.UNSPECIFIED.) ;
#982 = B_SPLINE_SURFACE_WITH_KNOTS('',3,3,((#77747,#77748,#77749,#77750),
(#77751,#77752,#77753,#77754),(#77755,#77756,#77757,#77758),(#77759,#77760,
#77761,#77762)),.UNSPECIFIED.,.F.,.F.,.F.,(4,4),(4,4),(0.,0.470859658428145),
(0.177146934337171,0.179997619857109),.UNSPECIFIED.) ;
#983 = B_SPLINE_SURFACE_WITH_KNOTS('',3,3,((#77763,#77764,#77765,#77766),
(#77767,#77768,#77769,#77770),(#77771,#77772,#77773,#77774),(#77775,#77776,
#77777,#77778)),.UNSPECIFIED.,.F.,.F.,.F.,(4,4),(4,4),(0.,0.470859658428137),
(0.177146934337171,0.17999761985711),.UNSPECIFIED.) ;
#984 = B_SPLINE_SURFACE_WITH_KNOTS('',3,3,((#77785,#77786,#77787,#77788,#77789,
#77790),(#77791,#77792,#77793,#77794,#77795,#77796),(#77797,#77798,#77799,
#77800,#77801,#77802),(#77803,#77804,#77805,#77806,#77807,#77808)),
 .UNSPECIFIED.,.F.,.F.,.F.,(4,4),(4,2,4),(0.,1.),(-0.0308408628658596,-0.0306076340858954,
0.),.UNSPECIFIED.) ;
#985 = B_SPLINE_SURFACE_WITH_KNOTS('',3,3,((#77827,#77828,#77829,#77830),
(#77831,#77832,#77833,#77834),(#77835,#77836,#77837,#77838),(#77839,#77840,
#77841,#77842),(#77843,#77844,#77845,#77846)),.UNSPECIFIED.,.F.,.F.,.F.,
(4,1,4),(4,4),(0.,0.571428571428571,1.),(0.,0.00359123636946112),
 .UNSPECIFIED.) ;
#986 = B_SPLINE_SURFACE_WITH_KNOTS('',3,3,((#77852,#77853,#77854,#77855),
(#77856,#77857,#77858,#77859),(#77860,#77861,#77862,#77863),(#77864,#77865,
#77866,#77867),(#77868,#77869,#77870,#77871)),.UNSPECIFIED.,.F.,.F.,.F.,
(4,1,4),(4,4),(0.,0.571428571428571,1.),(0.,0.0186228334818513),
 .UNSPECIFIED.) ;
#987 = B_SPLINE_SURFACE_WITH_KNOTS('',3,3,((#77914,#77915,#77916,#77917),
(#77918,#77919,#77920,#77921),(#77922,#77923,#77924,#77925),(#77926,#77927,
#77928,#77929),(#77930,#77931,#77932,#77933)),.UNSPECIFIED.,.F.,.F.,.F.,
(4,1,4),(4,4),(0.,0.571428571428571,1.),(0.,0.0186228334823063),
 .UNSPECIFIED.) ;
#988 = B_SPLINE_SURFACE_WITH_KNOTS('',3,3,((#77939,#77940,#77941,#77942),
(#77943,#77944,#77945,#77946),(#77947,#77948,#77949,#77950),(#77951,#77952,
#77953,#77954),(#77955,#77956,#77957,#77958)),.UNSPECIFIED.,.F.,.F.,.F.,
(4,1,4),(4,4),(0.,0.571428571428571,1.),(0.,0.00359123636948379),
 .UNSPECIFIED.) ;
#989 = B_SPLINE_SURFACE_WITH_KNOTS('',3,3,((#77963,#77964,#77965,#77966,#77967,
#77968),(#77969,#77970,#77971,#77972,#77973,#77974),(#77975,#77976,#77977,
#77978,#77979,#77980),(#77981,#77982,#77983,#77984,#77985,#77986),(#77987,
#77988,#77989,#77990,#77991,#77992)),.UNSPECIFIED.,.F.,.F.,.F.,(4,1,4),
(4,2,4),(0.,0.571428571428571,1.),(-0.0306076446211596,0.,0.0002332186634917),
 .UNSPECIFIED.) ;
#990 = B_SPLINE_SURFACE_WITH_KNOTS('',3,3,((#78032,#78033,#78034,#78035),
(#78036,#78037,#78038,#78039),(#78040,#78041,#78042,#78043),(#78044,#78045,
#78046,#78047)),.UNSPECIFIED.,.F.,.F.,.F.,(4,4),(4,4),(0.,1.),(0.0872664625997158,
1.5707963267949),.UNSPECIFIED.) ;
#991 = B_SPLINE_SURFACE_WITH_KNOTS('',3,3,((#78051,#78052,#78053,#78054,#78055),
(#78056,#78057,#78058,#78059,#78060),(#78061,#78062,#78063,#78064,#78065),
(#78066,#78067,#78068,#78069,#78070),(#78071,#78072,#78073,#78074,#78075)),
 .UNSPECIFIED.,.F.,.F.,.F.,(4,1,4),(4,1,4),(-0.00218136360640586,0.571428571428571,
1.00166487948942),(-1.34775708175487,-0.672576291298116,0.226937641442087),
 .UNSPECIFIED.) ;
#992 = B_SPLINE_SURFACE_WITH_KNOTS('',3,3,((#78108,#78109,#78110,#78111),
(#78112,#78113,#78114,#78115),(#78116,#78117,#78118,#78119),(#78120,#78121,
#78122,#78123)),.UNSPECIFIED.,.F.,.F.,.F.,(4,4),(4,4),(0.,1.),(-1.5707963267949,
-0.0872664625997159),.UNSPECIFIED.) ;
#993 = B_SPLINE_SURFACE_WITH_KNOTS('',3,3,((#78128,#78129,#78130,#78131,#78132),
(#78133,#78134,#78135,#78136,#78137),(#78138,#78139,#78140,#78141,#78142),
(#78143,#78144,#78145,#78146,#78147),(#78148,#78149,#78150,#78151,#78152)),
 .UNSPECIFIED.,.F.,.F.,.F.,(4,1,4),(4,1,4),(-0.00252299071546332,0.571428571428571,
1.00133658396291),(-0.22727926855115,0.44824314284204,1.34809869654644),
 .UNSPECIFIED.) ;
#994 = B_SPLINE_SURFACE_WITH_KNOTS('',3,3,((#78169,#78170,#78171,#78172),
(#78173,#78174,#78175,#78176),(#78177,#78178,#78179,#78180),(#78181,#78182,
#78183,#78184)),.UNSPECIFIED.,.F.,.F.,.F.,(4,4),(4,4),(0.,1.),(0.0872664625997154,
1.5707963267949),.UNSPECIFIED.) ;
#995 = B_SPLINE_SURFACE_WITH_KNOTS('',3,3,((#78216,#78217,#78218,#78219),
(#78220,#78221,#78222,#78223),(#78224,#78225,#78226,#78227),(#78228,#78229,
#78230,#78231)),.UNSPECIFIED.,.F.,.F.,.F.,(4,4),(4,4),(0.,1.),(0.087266462599716,
1.5707963267949),.UNSPECIFIED.) ;
#996 = B_SPLINE_SURFACE_WITH_KNOTS('',3,3,((#78256,#78257,#78258,#78259),
(#78260,#78261,#78262,#78263),(#78264,#78265,#78266,#78267),(#78268,#78269,
#78270,#78271),(#78272,#78273,#78274,#78275),(#78276,#78277,#78278,#78279)),
 .UNSPECIFIED.,.F.,.F.,.F.,(4,1,1,4),(4,4),(0.,0.285714285714286,0.571428571428571,
1.),(0.,0.0319729496810593),.UNSPECIFIED.) ;
#997 = B_SPLINE_SURFACE_WITH_KNOTS('',3,3,((#78293,#78294,#78295,#78296),
(#78297,#78298,#78299,#78300),(#78301,#78302,#78303,#78304),(#78305,#78306,
#78307,#78308),(#78309,#78310,#78311,#78312),(#78313,#78314,#78315,#78316)),
 .UNSPECIFIED.,.F.,.F.,.F.,(4,1,1,4),(4,4),(0.,0.285714285714286,0.571428571428571,
1.),(0.,0.0319729764593517),.UNSPECIFIED.) ;
#998 = B_SPLINE_SURFACE_WITH_KNOTS('',3,3,((#78326,#78327,#78328,#78329,#78330),
(#78331,#78332,#78333,#78334,#78335),(#78336,#78337,#78338,#78339,#78340),
(#78341,#78342,#78343,#78344,#78345),(#78346,#78347,#78348,#78349,#78350),
(#78351,#78352,#78353,#78354,#78355)),.UNSPECIFIED.,.F.,.F.,.F.,(4,1,1,
4),(4,1,4),(0.,0.285714285714286,0.571428571428571,1.),(0.,0.013702704196865,
0.0319729764593517),.UNSPECIFIED.) ;
#999 = B_SPLINE_SURFACE_WITH_KNOTS('',3,3,((#78380,#78381,#78382,#78383,#78384),
(#78385,#78386,#78387,#78388,#78389),(#78390,#78391,#78392,#78393,#78394),
(#78395,#78396,#78397,#78398,#78399),(#78400,#78401,#78402,#78403,#78404),
(#78405,#78406,#78407,#78408,#78409)),.UNSPECIFIED.,.F.,.F.,.F.,(4,1,1,
4),(4,1,4),(0.,0.285714285714286,0.571428571428571,1.),(1.29610738810862E-16,
0.0182702569606054,0.0319729496810593),.UNSPECIFIED.) ;
#1000 = FACE_BOUND('',#4160,.T.) ;
#1001 = FACE_BOUND('',#4161,.T.) ;
#1002 = FACE_BOUND('',#4162,.T.) ;
#1003 = FACE_BOUND('',#4163,.T.) ;
#1004 = FACE_BOUND('',#4164,.T.) ;
#1005 = FACE_BOUND('',#4165,.T.) ;
#1006 = FACE_BOUND('',#4166,.T.) ;
#1007 = FACE_BOUND('',#4167,.T.) ;
#1008 = FACE_BOUND('',#4168,.T.) ;
#1009 = FACE_BOUND('',#4169,.T.) ;
#1010 = FACE_BOUND('',#4170,.T.) ;
#1011 = FACE_BOUND('',#4171,.T.) ;
#1012 = FACE_BOUND('',#4172,.T.) ;
#1013 = FACE_BOUND('',#4173,.T.) ;
#1014 = FACE_BOUND('',#4174,.T.) ;
#1015 = FACE_BOUND('',#4175,.T.) ;
#1016 = FACE_BOUND('',#4176,.T.) ;
#1017 = FACE_BOUND('',#4177,.T.) ;
#1018 = FACE_BOUND('',#4178,.T.) ;
#1019 = FACE_BOUND('',#4179,.T.) ;
#1020 = FACE_BOUND('',#4183,.T.) ;
#1021 = FACE_BOUND('',#4184,.T.) ;
#1022 = FACE_BOUND('',#4188,.T.) ;
#1023 = FACE_BOUND('',#4189,.T.) ;
#1024 = FACE_BOUND('',#4193,.T.) ;
#1025 = FACE_BOUND('',#4194,.T.) ;
#1026 = FACE_BOUND('',#4202,.T.) ;
#1027 = FACE_BOUND('',#4203,.T.) ;
#1028 = FACE_BOUND('',#4204,.T.) ;
#1029 = FACE_BOUND('',#4205,.T.) ;
#1030 = FACE_BOUND('',#4206,.T.) ;
#1031 = FACE_BOUND('',#4207,.T.) ;
#1032 = FACE_BOUND('',#4208,.T.) ;
#1033 = FACE_BOUND('',#4209,.T.) ;
#1034 = FACE_BOUND('',#4210,.T.) ;
#1035 = FACE_BOUND('',#4211,.T.) ;
#1036 = FACE_BOUND('',#4212,.T.) ;
#1037 = FACE_BOUND('',#4213,.T.) ;
#1038 = FACE_BOUND('',#4214,.T.) ;
#1039 = FACE_BOUND('',#4215,.T.) ;
#1040 = FACE_BOUND('',#4216,.T.) ;
#1041 = FACE_BOUND('',#4217,.T.) ;
#1042 = FACE_BOUND('',#4218,.T.) ;
#1043 = FACE_BOUND('',#4219,.T.) ;
#1044 = FACE_BOUND('',#4220,.T.) ;
#1045 = FACE_BOUND('',#4221,.T.) ;
#1046 = FACE_BOUND('',#4223,.T.) ;
#1047 = FACE_BOUND('',#4224,.T.) ;
#1048 = FACE_BOUND('',#4356,.T.) ;
#1049 = FACE_BOUND('',#4364,.T.) ;
#1050 = FACE_BOUND('',#4391,.T.) ;
#1051 = FACE_BOUND('',#4491,.T.) ;
#1052 = FACE_BOUND('',#4492,.T.) ;
#1053 = FACE_BOUND('',#4493,.T.) ;
#1054 = FACE_BOUND('',#4494,.T.) ;
#1055 = FACE_BOUND('',#4495,.T.) ;
#1056 = FACE_BOUND('',#4496,.T.) ;
#1057 = FACE_BOUND('',#4497,.T.) ;
#1058 = FACE_BOUND('',#4498,.T.) ;
#1059 = FACE_BOUND('',#4501,.T.) ;
#1060 = FACE_BOUND('',#4502,.T.) ;
#1061 = FACE_BOUND('',#4503,.T.) ;
#1062 = FACE_BOUND('',#4504,.T.) ;
#1063 = FACE_BOUND('',#4505,.T.) ;
#1064 = FACE_BOUND('',#4506,.T.) ;
#1065 = FACE_BOUND('',#4507,.T.) ;
#1066 = FACE_BOUND('',#4508,.T.) ;
#1067 = FACE_BOUND('',#4509,.T.) ;
#1068 = FACE_BOUND('',#4510,.T.) ;
#1069 = FACE_BOUND('',#4512,.T.) ;
#1070 = FACE_BOUND('',#4513,.T.) ;
#1071 = FACE_BOUND('',#4514,.T.) ;
#1072 = FACE_BOUND('',#4515,.T.) ;
#1073 = FACE_BOUND('',#4516,.T.) ;
#1074 = FACE_BOUND('',#4517,.T.) ;
#1075 = FACE_BOUND('',#4518,.T.) ;
#1076 = FACE_BOUND('',#4519,.T.) ;
#1077 = FACE_BOUND('',#4521,.T.) ;
#1078 = FACE_BOUND('',#4522,.T.) ;
#1079 = FACE_BOUND('',#4523,.T.) ;
#1080 = FACE_BOUND('',#4524,.T.) ;
#1081 = FACE_BOUND('',#4525,.T.) ;
#1082 = FACE_BOUND('',#4526,.T.) ;
#1083 = FACE_BOUND('',#4527,.T.) ;
#1084 = FACE_BOUND('',#4528,.T.) ;
#1085 = FACE_BOUND('',#4529,.T.) ;
#1086 = FACE_BOUND('',#4530,.T.) ;
#1087 = FACE_BOUND('',#4644,.T.) ;
#1088 = FACE_BOUND('',#4645,.T.) ;
#1089 = FACE_BOUND('',#4646,.T.) ;
#1090 = FACE_BOUND('',#4647,.T.) ;
#1091 = FACE_BOUND('',#4689,.T.) ;
#1092 = FACE_BOUND('',#4724,.T.) ;
#1093 = FACE_BOUND('',#4725,.T.) ;
#1094 = FACE_BOUND('',#4726,.T.) ;
#1095 = FACE_BOUND('',#4727,.T.) ;
#1096 = FACE_BOUND('',#4732,.T.) ;
#1097 = FACE_BOUND('',#4744,.T.) ;
#1098 = FACE_BOUND('',#4745,.T.) ;
#1099 = FACE_BOUND('',#4746,.T.) ;
#1100 = FACE_BOUND('',#4747,.T.) ;
#1101 = FACE_BOUND('',#4748,.T.) ;
#1102 = FACE_BOUND('',#4749,.T.) ;
#1103 = FACE_BOUND('',#4750,.T.) ;
#1104 = FACE_BOUND('',#4751,.T.) ;
#1105 = FACE_BOUND('',#4752,.T.) ;
#1106 = FACE_BOUND('',#4768,.T.) ;
#1107 = FACE_BOUND('',#4769,.T.) ;
#1108 = FACE_BOUND('',#4770,.T.) ;
#1109 = FACE_BOUND('',#4771,.T.) ;
#1110 = FACE_BOUND('',#4772,.T.) ;
#1111 = FACE_BOUND('',#4773,.T.) ;
#1112 = FACE_BOUND('',#4774,.T.) ;
#1113 = FACE_BOUND('',#4775,.T.) ;
#1114 = FACE_BOUND('',#4776,.T.) ;
#1115 = FACE_BOUND('',#4823,.T.) ;
#1116 = FACE_BOUND('',#4824,.T.) ;
#1117 = FACE_BOUND('',#4828,.T.) ;
#1118 = FACE_BOUND('',#4829,.T.) ;
#1119 = FACE_BOUND('',#4833,.T.) ;
#1120 = FACE_BOUND('',#4834,.T.) ;
#1121 = FACE_BOUND('',#4838,.T.) ;
#1122 = FACE_BOUND('',#4839,.T.) ;
#1123 = FACE_BOUND('',#4843,.T.) ;
#1124 = FACE_BOUND('',#4844,.T.) ;
#1125 = FACE_BOUND('',#4848,.T.) ;
#1126 = FACE_BOUND('',#4849,.T.) ;
#1127 = FACE_BOUND('',#4853,.T.) ;
#1128 = FACE_BOUND('',#4854,.T.) ;
#1129 = FACE_BOUND('',#4858,.T.) ;
#1130 = FACE_BOUND('',#4859,.T.) ;
#1131 = FACE_BOUND('',#4862,.T.) ;
#1132 = FACE_BOUND('',#4863,.T.) ;
#1133 = FACE_BOUND('',#4866,.T.) ;
#1134 = FACE_BOUND('',#4868,.T.) ;
#1135 = FACE_BOUND('',#4870,.T.) ;
#1136 = FACE_BOUND('',#4872,.T.) ;
#1137 = FACE_BOUND('',#4874,.T.) ;
#1138 = FACE_BOUND('',#4876,.T.) ;
#1139 = FACE_BOUND('',#4878,.T.) ;
#1140 = FACE_BOUND('',#4880,.T.) ;
#1141 = FACE_BOUND('',#5194,.T.) ;
#1142 = FACE_BOUND('',#5195,.T.) ;
#1143 = FACE_BOUND('',#5196,.T.) ;
#1144 = FACE_BOUND('',#5217,.T.) ;
#1145 = FACE_BOUND('',#5565,.T.) ;
#1146 = FACE_BOUND('',#5566,.T.) ;
#1147 = FACE_BOUND('',#5567,.T.) ;
#1148 = FACE_BOUND('',#5574,.T.) ;
#1149 = FACE_BOUND('',#5575,.T.) ;
#1150 = FACE_BOUND('',#5576,.T.) ;
#1151 = FACE_BOUND('',#5583,.T.) ;
#1152 = FACE_BOUND('',#5584,.T.) ;
#1153 = FACE_BOUND('',#5585,.T.) ;
#1154 = FACE_BOUND('',#5592,.T.) ;
#1155 = FACE_BOUND('',#5593,.T.) ;
#1156 = FACE_BOUND('',#5594,.T.) ;
#1157 = FACE_BOUND('',#5601,.T.) ;
#1158 = FACE_BOUND('',#5602,.T.) ;
#1159 = FACE_BOUND('',#5603,.T.) ;
#1160 = FACE_BOUND('',#5610,.T.) ;
#1161 = FACE_BOUND('',#5611,.T.) ;
#1162 = FACE_BOUND('',#5612,.T.) ;
#1163 = FACE_BOUND('',#5619,.T.) ;
#1164 = FACE_BOUND('',#5620,.T.) ;
#1165 = FACE_BOUND('',#5621,.T.) ;
#1166 = FACE_BOUND('',#5628,.T.) ;
#1167 = FACE_BOUND('',#5629,.T.) ;
#1168 = FACE_BOUND('',#5630,.T.) ;
#1169 = FACE_BOUND('',#5787,.T.) ;
#1170 = FACE_BOUND('',#5960,.T.) ;
#1171 = FACE_BOUND('',#6015,.T.) ;
#1172 = FACE_BOUND('',#6019,.T.) ;
#1173 = FACE_BOUND('',#6029,.T.) ;
#1174 = FACE_BOUND('',#6103,.T.) ;
#1175 = FACE_BOUND('',#6134,.T.) ;
#1176 = FACE_BOUND('',#6135,.T.) ;
#1177 = FACE_BOUND('',#6136,.T.) ;
#1178 = FACE_BOUND('',#6137,.T.) ;
#1179 = FACE_BOUND('',#6138,.T.) ;
#1180 = FACE_BOUND('',#6140,.T.) ;
#1181 = FACE_BOUND('',#6141,.T.) ;
#1182 = FACE_BOUND('',#6142,.T.) ;
#1183 = FACE_BOUND('',#6143,.T.) ;
#1184 = FACE_BOUND('',#6144,.T.) ;
#1185 = FACE_BOUND('',#6193,.T.) ;
#1186 = FACE_BOUND('',#6197,.T.) ;
#1187 = FACE_BOUND('',#6230,.T.) ;
#1188 = FACE_BOUND('',#6233,.T.) ;
#1189 = B_SPLINE_CURVE_WITH_KNOTS('',3,(#46372,#46373,#46374,#46375,#46376,
#46377,#46378),.UNSPECIFIED.,.F.,.F.,(4,1,1,1,4),(0.,0.112519573127489,
0.337558719382466,0.562597865637444,0.787637011892422),.UNSPECIFIED.) ;
#1190 = B_SPLINE_CURVE_WITH_KNOTS('',3,(#46384,#46385,#46386,#46387,#46388,
#46389,#46390),.UNSPECIFIED.,.F.,.F.,(4,1,1,1,4),(0.,0.112518191393291,
0.337554574179873,0.562590956966454,0.787627339753036),.UNSPECIFIED.) ;
#1191 = B_SPLINE_CURVE_WITH_KNOTS('',3,(#46817,#46818,#46819,#46820,#46821,
#46822,#46823),.UNSPECIFIED.,.F.,.F.,(4,1,1,1,4),(0.,0.22503638292787,0.45007276585574,
0.675109148783609,0.787627340247544),.UNSPECIFIED.) ;
#1192 = B_SPLINE_CURVE_WITH_KNOTS('',3,(#46831,#46832,#46833,#46834,#46835,
#46836,#46837),.UNSPECIFIED.,.F.,.F.,(4,1,1,1,4),(0.,0.225039146153262,
0.450078292306524,0.675117438459786,0.787637011536417),.UNSPECIFIED.) ;
#1193 = B_SPLINE_CURVE_WITH_KNOTS('',3,(#47181,#47182,#47183,#47184,#47185,
#47186,#47187,#47188,#47189,#47190),.UNSPECIFIED.,.F.,.F.,(4,2,2,2,4),(3.31842937808031,
3.35016755864468,3.396837923606,3.44175906248201,3.48648133511502),
 .UNSPECIFIED.) ;
#1194 = B_SPLINE_CURVE_WITH_KNOTS('',3,(#47193,#47194,#47195,#47196,#47197,
#47198,#47199,#47200,#47201,#47202,#47203,#47204,#47205,#47206),
 .UNSPECIFIED.,.F.,.F.,(4,2,2,2,2,2,4),(0.,0.0410648441701088,0.087038006677358,
0.133890124936013,0.178670683243025,0.225128281986789,0.260876372449635),
 .UNSPECIFIED.) ;
#1195 = B_SPLINE_CURVE_WITH_KNOTS('',3,(#47211,#47212,#47213,#47214,#47215,
#47216,#47217,#47218,#47219,#47220,#47221,#47222,#47223,#47224,#47225,#47226,
#47227,#47228,#47229,#47230,#47231,#47232,#47233,#47234,#47235,#47236,#47237,
#47238,#47239,#47240,#47241,#47242,#47243,#47244,#47245,#47246),
 .UNSPECIFIED.,.F.,.F.,(4,2,2,2,2,2,2,2,2,2,2,2,2,2,2,2,2,4),(2.57674153154878,
2.61510934153612,2.66143878579143,2.70614655228561,2.75296429564827,2.79880209242763,
2.84382702777492,2.8909179029586,2.93622526800305,2.98243368493191,3.02891741450234,
3.07371420452932,3.12056663647033,3.1665682661734,3.211499121418,3.25876850942625,
3.30424075672643,3.31842937808031),.UNSPECIFIED.) ;
#1196 = B_SPLINE_CURVE_WITH_KNOTS('',3,(#47247,#47248,#47249,#47250,#47251,
#47252,#47253,#47254,#47255,#47256,#47257,#47258,#47259,#47260,#47261,#47262,
#47263,#47264,#47265,#47266,#47267,#47268,#47269,#47270,#47271,#47272,#47273,
#47274,#47275,#47276,#47277,#47278,#47279,#47280,#47281,#47282),
 .UNSPECIFIED.,.F.,.F.,(4,2,2,2,2,2,2,2,2,2,2,2,2,2,2,2,2,4),(0.260876372449635,
0.271419194700287,0.316705310163363,0.363772652894618,0.408838431413797,
0.454655510522189,0.50148068321131,0.546189410353657,0.59250008742341,0.639168445054,
0.684332831326177,0.731267564232706,0.776520489163937,0.822218852479091,
0.869051231455086,0.913765477568226,0.959965017786808,1.00233576817236),
 .UNSPECIFIED.) ;
#1197 = B_SPLINE_CURVE_WITH_KNOTS('',3,(#47287,#47288,#47289,#47290,#47291,
#47292,#47293,#47294,#47295,#47296,#47297,#47298,#47299,#47300,#47301,#47302,
#47303,#47304,#47305,#47306,#47307,#47308,#47309,#47310,#47311,#47312,#47313,
#47314,#47315,#47316,#47317,#47318,#47319,#47320,#47321,#47322),
 .UNSPECIFIED.,.F.,.F.,(4,2,2,2,2,2,2,2,2,2,2,2,2,2,2,2,2,4),(1.83527394228767,
1.88005636343276,1.92618554035068,1.97094346323703,2.01779361772358,2.06341660574272,
2.1088504927414,2.15569904695649,2.20078442257148,2.2477789890551,2.29398931205669,
2.33868626489989,2.38550400171857,2.43121478880165,2.47641117263732,2.52336103019069,
2.56853877611464,2.57674153154878),.UNSPECIFIED.) ;
#1198 = B_SPLINE_CURVE_WITH_KNOTS('',3,(#47323,#47324,#47325,#47326,#47327,
#47328,#47329,#47330,#47331,#47332,#47333,#47334,#47335,#47336,#47337,#47338,
#47339,#47340,#47341,#47342,#47343,#47344,#47345,#47346,#47347,#47348,#47349,
#47350,#47351,#47352,#47353,#47354,#47355,#47356,#47357,#47358,#47359,#47360),
 .UNSPECIFIED.,.F.,.F.,(4,2,2,2,2,2,2,2,2,2,2,2,2,2,2,2,2,2,4),(1.00233576817236,
1.00706798297321,1.05214831718699,1.09899061505082,1.14449303921197,1.19011236551882,
1.23698396348855,1.28177341314926,1.32790037311896,1.37475812257317,1.4197708130612,
1.46653772846629,1.51240885912924,1.55796961908873,1.60533369336509,1.65027263764824,
1.69636292389366,1.7432590420322,1.74485974249583),.UNSPECIFIED.) ;
#1199 = B_SPLINE_CURVE_WITH_KNOTS('',3,(#47365,#47366,#47367,#47368,#47369,
#47370,#47371,#47372,#47373,#47374,#47375,#47376,#47377,#47378,#47379,#47380,
#47381,#47382,#47383,#47384,#47385,#47386,#47387,#47388,#47389,#47390,#47391,
#47392,#47393,#47394,#47395,#47396,#47397,#47398,#47399,#47400,#47401,#47402),
 .UNSPECIFIED.,.F.,.F.,(4,2,2,2,2,2,2,2,2,2,2,2,2,2,2,2,2,2,4),(1.09311325644766,
1.09847320345976,1.14356176541002,1.1904136830288,1.23584708927346,1.28147323113724,
1.32832534251677,1.37308461796146,1.41921690762957,1.46605634177153,1.51107118762394,
1.55784129736534,1.60362255713177,1.64918322667193,1.69654896763227,1.74143993730663,
1.78820699300995,1.83321894472862,1.83527394228767),.UNSPECIFIED.) ;
#1200 = B_SPLINE_CURVE_WITH_KNOTS('',3,(#47403,#47404,#47405,#47406,#47407,
#47408,#47409,#47410,#47411,#47412,#47413,#47414,#47415,#47416,#47417,#47418,
#47419,#47420,#47421,#47422,#47423,#47424,#47425,#47426,#47427,#47428,#47429,
#47430,#47431,#47432,#47433,#47434,#47435,#47436,#47437,#47438),
 .UNSPECIFIED.,.F.,.F.,(4,2,2,2,2,2,2,2,2,2,2,2,2,2,2,2,2,4),(1.74485974249583,
1.79012023382528,1.83625688485754,1.881046044964,1.92792078440463,1.97355010886049,
2.01904189360249,2.06589517212617,2.11098579935953,2.15806712470955,2.20427882402216,
2.24899676761857,2.29583421166923,2.34154509588437,2.38679067187208,2.43373894168524,
2.47891601834838,2.4866650924994),.UNSPECIFIED.) ;
#1201 = B_SPLINE_CURVE_WITH_KNOTS('',3,(#47444,#47445,#47446,#47447,#47448,
#47449,#47450,#47451,#47452,#47453,#47454,#47455,#47456,#47457),
 .UNSPECIFIED.,.F.,.F.,(4,2,2,2,2,2,4),(3.22852173666992,3.26076961433847,
3.30742587418507,3.3523750214278,3.39930257668415,3.44548606230632,3.48984669211956),
 .UNSPECIFIED.) ;
#1202 = B_SPLINE_CURVE_WITH_KNOTS('',3,(#47460,#47461,#47462,#47463,#47464,
#47465,#47466,#47467,#47468,#47469,#47470,#47471,#47472,#47473,#47474,#47475,
#47476,#47477),.UNSPECIFIED.,.F.,.F.,(4,2,2,2,2,2,2,2,4),(9.99999983706711E-7,
0.0438977278136496,0.0877054255663695,0.132637957456045,0.178643873404191,
0.225499231392538,0.270299674020503,0.316787599511936,0.351767081365554),
 .UNSPECIFIED.) ;
#1203 = B_SPLINE_CURVE_WITH_KNOTS('',3,(#47483,#47484,#47485,#47486,#47487,
#47488,#47489,#47490,#47491,#47492,#47493,#47494,#47495,#47496,#47497,#47498),
 .UNSPECIFIED.,.F.,.F.,(4,2,2,2,2,2,2,4),(-0.356839236286574,-0.318839138763554,
-0.259130427174361,-0.201661085069514,-0.141844076929324,-0.0829140522622169,
-0.0414114555033024,-9.99999994644174E-7),.UNSPECIFIED.) ;
#1204 = B_SPLINE_CURVE_WITH_KNOTS('',3,(#47501,#47502,#47503,#47504,#47505,
#47506,#47507,#47508,#47509,#47510,#47511,#47512,#47513,#47514,#47515,#47516,
#47517,#47518,#47519,#47520),.UNSPECIFIED.,.F.,.F.,(4,2,2,2,2,2,2,2,2,4),
(-5.6777690195579,-5.63616767911395,-5.59310905687254,-5.53347115580099,
-5.47651899265005,-5.41771065230489,-5.35758701805482,-5.30022347326295,
-5.24061901702306,-5.20527205396992),.UNSPECIFIED.) ;
#1205 = B_SPLINE_CURVE_WITH_KNOTS('',3,(#47525,#47526,#47527,#47528,#47529,
#47530,#47531,#47532,#47533,#47534,#47535,#47536,#47537,#47538,#47539,#47540,
#47541,#47542,#47543,#47544,#47545,#47546,#47547,#47548,#47549,#47550,#47551,
#47552,#47553,#47554,#47555,#47556,#47557,#47558,#47559,#47560),
 .UNSPECIFIED.,.F.,.F.,(4,2,2,2,2,2,2,2,2,2,2,2,2,2,2,2,2,4),(-1.30494350966952,
-1.25776789010065,-1.1985119263168,-1.14137951639351,-1.08158575215186,
-1.0229769527965,-0.965565001793067,-0.905333721448379,-0.847397764355833,
-0.788595538964929,-0.729125616520127,-0.671843999206589,-0.612011464665177,
-0.553186058070021,-0.495885382179051,-0.435418594272755,-0.377269758491555,
-0.356839236286574),.UNSPECIFIED.) ;
#1206 = B_SPLINE_CURVE_WITH_KNOTS('',3,(#47561,#47562,#47563,#47564,#47565,
#47566,#47567,#47568,#47569,#47570,#47571,#47572,#47573,#47574,#47575,#47576,
#47577,#47578,#47579,#47580,#47581,#47582,#47583,#47584,#47585,#47586,#47587,
#47588,#47589,#47590,#47591,#47592,#47593,#47594,#47595,#47596),
 .UNSPECIFIED.,.F.,.F.,(4,2,2,2,2,2,2,2,2,2,2,2,2,2,2,2,2,4),(-5.20527205396992,
-5.18260211509116,-5.1245647406915,-5.06488837094347,-5.00783480509734,
-4.94914569176594,-4.88949082733128,-4.8322501268223,-4.77278429618413,
-4.71425928615259,-4.65633638196459,-4.59611265214601,-4.53886176529339,
-4.48026581636814,-4.4205639465445,-4.36347931260193,-4.30423839363068,
-4.25917338249842),.UNSPECIFIED.) ;
#1207 = B_SPLINE_CURVE_WITH_KNOTS('',3,(#47601,#47602,#47603,#47604,#47605,
#47606,#47607,#47608,#47609,#47610,#47611,#47612,#47613,#47614,#47615,#47616,
#47617,#47618,#47619,#47620,#47621,#47622,#47623,#47624,#47625,#47626,#47627,
#47628,#47629,#47630,#47631,#47632,#47633,#47634,#47635,#47636),
 .UNSPECIFIED.,.F.,.F.,(4,2,2,2,2,2,2,2,2,2,2,2,2,2,2,2,2,4),(-2.25248934816888,
-2.19617623781344,-2.13725183863766,-2.08012580789218,-2.02032048864309,
-1.96204771939477,-1.904125144753,-1.84426787577856,-1.78666784944015,-1.72681573103074,
-1.66774351387222,-1.61066141331469,-1.55087592498769,-1.49245308352448,
-1.43482961561388,-1.37480327574036,-1.31705178913088,-1.30494350966952),
 .UNSPECIFIED.) ;
#1208 = B_SPLINE_CURVE_WITH_KNOTS('',3,(#47637,#47638,#47639,#47640,#47641,
#47642,#47643,#47644,#47645,#47646,#47647,#47648,#47649,#47650,#47651,#47652,
#47653,#47654,#47655,#47656,#47657,#47658,#47659,#47660,#47661,#47662,#47663,
#47664,#47665,#47666,#47667,#47668,#47669,#47670,#47671,#47672),
 .UNSPECIFIED.,.F.,.F.,(4,2,2,2,2,2,2,2,2,2,2,2,2,2,2,2,2,4),(-4.25917338249842,
-4.24527779180941,-4.18755180165972,-4.12754644710674,-4.070126508801,-4.01173002419351,
-3.95204920618323,-3.89505746671119,-3.83601367393912,-3.77651947097669,
-3.71895945267056,-3.6591389505398,-3.60145584791493,-3.54322523402684,
-3.48353646776607,-3.42654013249902,-3.36766003550048,-3.31332463994661),
 .UNSPECIFIED.) ;
#1209 = B_SPLINE_CURVE_WITH_KNOTS('',3,(#47677,#47678,#47679,#47680,#47681,
#47682,#47683,#47684,#47685,#47686,#47687,#47688,#47689,#47690,#47691,#47692,
#47693,#47694,#47695,#47696,#47697,#47698,#47699,#47700,#47701,#47702,#47703,
#47704,#47705,#47706,#47707,#47708,#47709,#47710,#47711,#47712,#47713,#47714),
 .UNSPECIFIED.,.F.,.F.,(4,2,2,2,2,2,2,2,2,2,2,2,2,2,2,2,2,2,4),(-3.20029950146654,
-3.19315660740551,-3.13560653382823,-3.07580344967673,-3.01782963552705,
-2.95960638292588,-2.89981630259394,-2.84269176491814,-2.78323065019205,
-2.72595980442964,-2.66615935009437,-2.60734191496364,-2.55008635989913,
-2.4896261022618,-2.43148541093545,-2.3731342360459,-2.31343130070289,-2.25596874753601,
-2.25248934816888),.UNSPECIFIED.) ;
#1210 = B_SPLINE_CURVE_WITH_KNOTS('',3,(#47715,#47716,#47717,#47718,#47719,
#47720,#47721,#47722,#47723,#47724,#47725,#47726,#47727,#47728,#47729,#47730,
#47731,#47732,#47733,#47734,#47735,#47736,#47737,#47738,#47739,#47740,#47741,
#47742,#47743,#47744,#47745,#47746,#47747,#47748,#47749,#47750,#47751,#47752),
 .UNSPECIFIED.,.F.,.F.,(4,2,2,2,2,2,2,2,2,2,2,2,2,2,2,2,2,2,4),(-3.31332463994661,
-3.30756374577828,-3.25013416214204,-3.19045983715782,-3.1324387157978,
-3.0743354352636,-3.01461170216103,-2.95752404946368,-2.89876880763459,
-2.83906516495525,-2.77933159023642,-2.72059832312161,-2.6633956702534,
-2.60302322859973,-2.5449655288037,-2.48664210359268,-2.42702627164252,
-2.36964659357858,-2.36659114930348),.UNSPECIFIED.) ;
#1211 = B_SPLINE_CURVE_WITH_KNOTS('',3,(#47757,#47758,#47759,#47760,#47761,
#47762,#47763,#47764,#47765,#47766,#47767,#47768,#47769,#47770,#47771,#47772,
#47773,#47774,#47775,#47776,#47777,#47778,#47779,#47780,#47781,#47782,#47783,
#47784,#47785,#47786,#47787,#47788,#47789,#47790,#47791,#47792),
 .UNSPECIFIED.,.F.,.F.,(4,2,2,2,2,2,2,2,2,2,2,2,2,2,2,2,2,4),(-4.14747208700764,
-4.13206742370891,-4.07419594267165,-4.01403463010671,-3.95660744642544,
-3.8980639186862,-3.83829740608844,-3.78120614155281,-3.72201520284988,
-3.66263824916934,-3.6049444685612,-3.54498075518231,-3.48732198039695,
-3.42895705995953,-3.36919260172769,-3.31213058552288,-3.25311607462449,
-3.20029950146654),.UNSPECIFIED.) ;
#1212 = B_SPLINE_CURVE_WITH_KNOTS('',3,(#47793,#47794,#47795,#47796,#47797,
#47798,#47799,#47800,#47801,#47802,#47803,#47804,#47805,#47806,#47807,#47808,
#47809,#47810,#47811,#47812,#47813,#47814,#47815,#47816,#47817,#47818,#47819,
#47820,#47821,#47822,#47823,#47824,#47825,#47826,#47827,#47828),
 .UNSPECIFIED.,.F.,.F.,(4,2,2,2,2,2,2,2,2,2,2,2,2,2,2,2,2,4),(-2.36659114930348,
-2.3099267325564,-2.2510883534928,-2.19402473111864,-2.1342907007857,-2.07610338007785,
-2.0182197874013,-1.95845180936089,-1.90093669275898,-1.84109983357991,
-1.78211765323279,-1.72510653073043,-1.66539497500452,-1.60706157178376,
-1.54948423504781,-1.48955121115931,-1.43188832707264,-1.42020742457329),
 .UNSPECIFIED.) ;
#1213 = B_SPLINE_CURVE_WITH_KNOTS('',3,(#47834,#47835,#47836,#47837,#47838,
#47839,#47840,#47841,#47842,#47843,#47844,#47845,#47846,#47847,#47848,#47849,
#47850,#47851,#47852,#47853),.UNSPECIFIED.,.F.,.F.,(4,2,2,2,2,2,2,2,2,4),
(-0.473361116390324,-0.434980285469829,-0.375370649937796,-0.317995768158978,
-0.258264150217988,-0.199432012735734,-0.142347766489119,-0.0826003210214793,
-0.0405758598073532,-9.99999995310308E-7),.UNSPECIFIED.) ;
#1214 = B_SPLINE_CURVE_WITH_KNOTS('',3,(#47856,#47857,#47858,#47859,#47860,
#47861,#47862,#47863,#47864,#47865,#47866,#47867,#47868,#47869,#47870,#47871,
#47872,#47873,#47874,#47875,#47876,#47877,#47878,#47879),.UNSPECIFIED.,
 .F.,.F.,(4,2,2,2,2,2,2,2,2,2,2,4),(-5.68568308835527,-5.64187567407348,
-5.59831170654822,-5.54062509920359,-5.48228578877153,-5.422526237897,-5.36546755897281,
-5.3064784656501,-5.2464513100281,-5.18892242603572,-5.12914260288557,-5.09523963172672),
 .UNSPECIFIED.) ;
#1215 = B_SPLINE_CURVE_WITH_KNOTS('',3,(#47884,#47885,#47886,#47887),
 .UNSPECIFIED.,.F.,.F.,(4,4),(-1.00218290968104,-0.991970784037339),
 .UNSPECIFIED.) ;
#1216 = B_SPLINE_CURVE_WITH_KNOTS('',3,(#47888,#47889,#47890,#47891,#47892,
#47893,#47894,#47895),.UNSPECIFIED.,.F.,.F.,(4,2,2,4),(0.,0.0435785122875659,
0.0903817076613929,0.124172560080924),.UNSPECIFIED.) ;
#1217 = B_SPLINE_CURVE_WITH_KNOTS('',3,(#47899,#47900,#47901,#47902,#47903,
#47904,#47905,#47906),.UNSPECIFIED.,.F.,.F.,(4,2,2,4),(-0.575278937572396,
-0.559414249044956,-0.544216358804097,-0.536951818658365),.UNSPECIFIED.) ;
#1218 = B_SPLINE_CURVE_WITH_KNOTS('',3,(#47907,#47908,#47909,#47910,#47911,
#47912,#47913,#47914,#47915,#47916,#47917,#47918,#47919,#47920),
 .UNSPECIFIED.,.F.,.F.,(4,2,2,2,2,2,4),(-0.166734145007444,-0.148557002683626,
-0.136251466347306,-0.113028859542707,-0.0847672793749983,-0.0413426304955296,
-1.00000017441704E-6),.UNSPECIFIED.) ;
#1219 = B_SPLINE_CURVE_WITH_KNOTS('',3,(#47923,#47924,#47925,#47926,#47927,
#47928,#47929,#47930,#47931,#47932,#47933,#47934,#47935,#47936,#47937,#47938,
#47939,#47940,#47941,#47942,#47943,#47944,#47945,#47946,#47947,#47948,#47949,
#47950,#47951,#47952,#47953,#47954,#47955,#47956,#47957,#47958),
 .UNSPECIFIED.,.F.,.F.,(4,2,2,2,2,2,2,2,2,2,2,2,2,2,2,2,2,4),(-0.536951818658365,
-0.536175700978615,-0.519496434514374,-0.503627636028881,-0.482751345818568,
-0.453972299702605,-0.427124357976038,-0.412423739643194,-0.382270815269358,
-0.353759615123692,-0.315266001158416,-0.260624023001414,-0.205656350189048,
-0.177984976990091,-0.12376571829927,-0.0654292820557721,-0.0322025263864932,
-1.00000009040091E-6),.UNSPECIFIED.) ;
#1220 = B_SPLINE_CURVE_WITH_KNOTS('',3,(#47960,#47961,#47962,#47963,#47964,
#47965,#47966,#47967),.UNSPECIFIED.,.F.,.F.,(4,2,2,4),(0.124172560080924,
0.157998858836025,0.240075000933573,0.324188312978485),.UNSPECIFIED.) ;
#1221 = B_SPLINE_CURVE_WITH_KNOTS('',3,(#47969,#47970,#47971,#47972,#47973,
#47974,#47975,#47976,#47977,#47978,#47979,#47980,#47981,#47982,#47983,#47984,
#47985,#47986,#47987,#47988,#47989,#47990,#47991,#47992,#47993,#47994,#47995,
#47996,#47997,#47998,#47999,#48000,#48001,#48002,#48003,#48004,#48005,#48006,
#48007,#48008),.UNSPECIFIED.,.F.,.F.,(4,2,2,2,2,2,2,2,2,2,2,2,2,2,2,2,2,
2,2,4),(-0.991970784037339,-0.976482169541418,-0.940511015363057,-0.898601131647801,
-0.876476528706804,-0.830559860454117,-0.786858882019556,-0.729757356509824,
-0.65196076520893,-0.579389748760059,-0.491285302902488,-0.394350008062906,
-0.294163274796139,-0.237450467655031,-0.191239556405745,-0.16841211518385,
-0.117188759032826,-0.0606892948336317,-0.0314347233699885,-1.00000009273238E-6),
 .UNSPECIFIED.) ;
#1222 = B_SPLINE_CURVE_WITH_KNOTS('',3,(#48010,#48011,#48012,#48013,#48014,
#48015,#48016,#48017,#48018,#48019,#48020,#48021,#48022,#48023,#48024,#48025,
#48026,#48027,#48028,#48029,#48030,#48031,#48032,#48033,#48034,#48035,#48036,
#48037,#48038,#48039,#48040,#48041,#48042,#48043,#48044,#48045),
 .UNSPECIFIED.,.F.,.F.,(4,2,2,2,2,2,2,2,2,2,2,2,2,2,2,2,2,4),(-5.09523963172672,
-5.07113258312941,-5.01293004439165,-4.95314154316727,-4.89601012144808,
-4.83715542661164,-4.77738423908235,-4.71998612925933,-4.6603534598268,
-4.60187538467476,-4.54379684525718,-4.48340624898908,-4.42611243528161,
-4.36735853154431,-4.30756005089831,-4.2503406903036,-4.19094189274728,
-4.14747208700764),.UNSPECIFIED.) ;
#1223 = B_SPLINE_CURVE_WITH_KNOTS('',3,(#48046,#48047,#48048,#48049,#48050,
#48051,#48052,#48053,#48054,#48055,#48056,#48057,#48058,#48059,#48060,#48061,
#48062,#48063,#48064,#48065,#48066,#48067,#48068,#48069,#48070,#48071,#48072,
#48073,#48074,#48075,#48076,#48077,#48078,#48079,#48080,#48081),
 .UNSPECIFIED.,.F.,.F.,(4,2,2,2,2,2,2,2,2,2,2,2,2,2,2,2,2,4),(-1.42020742457329,
-1.37262582777851,-1.31346342085115,-1.25641173589597,-1.19669477961086,
-1.13817895843239,-1.08082218003548,-1.02068777127858,-0.962843692323244,
-0.904072038294528,-0.844698668720221,-0.787507583204744,-0.727755034178589,
-0.669025666660467,-0.611790195274486,-0.551423357069376,-0.493369273141207,
-0.473361116390324),.UNSPECIFIED.) ;
#1224 = B_SPLINE_CURVE_WITH_KNOTS('',3,(#48083,#48084,#48085,#48086,#48087,
#48088,#48089,#48090,#48091,#48092,#48093,#48094,#48095,#48096,#48097,#48098,
#48099,#48100,#48101,#48102,#48103,#48104,#48105,#48106,#48107,#48108,#48109,
#48110,#48111,#48112,#48113,#48114,#48115,#48116,#48117,#48118),
 .UNSPECIFIED.,.F.,.F.,(4,2,2,2,2,2,2,2,2,2,2,2,2,2,2,2,2,4),(0.351767081365554,
0.362994825087978,0.408306200866931,0.45540131847049,0.500427176257259,
0.546268992971341,0.593089400650884,0.63780007653961,0.684133472260792,
0.730702175568153,0.775883529775975,0.822837200812743,0.868033712567382,
0.913748097481785,0.960568133215132,1.00526716490256,1.05148103368736,1.09311325644766),
 .UNSPECIFIED.) ;
#1225 = B_SPLINE_CURVE_WITH_KNOTS('',3,(#48119,#48120,#48121,#48122,#48123,
#48124,#48125,#48126,#48127,#48128,#48129,#48130,#48131,#48132,#48133,#48134,
#48135,#48136,#48137,#48138,#48139,#48140,#48141,#48142,#48143,#48144,#48145,
#48146,#48147,#48148,#48149,#48150,#48151,#48152,#48153,#48154),
 .UNSPECIFIED.,.F.,.F.,(4,2,2,2,2,2,2,2,2,2,2,2,2,2,2,2,2,4),(2.4866650924994,
2.52556556364955,2.57189071243123,2.61660775868172,2.66344004151552,2.7092720422196,
2.75433484706525,2.80141816191296,2.84671925205663,2.89299554386376,2.93946975715054,
2.98426354830769,3.03112497725156,3.07711531442473,3.12207147536806,3.16932769067158,
3.21478837165691,3.22852173666992),.UNSPECIFIED.) ;
#1226 = B_SPLINE_CURVE_WITH_KNOTS('',3,(#48641,#48642,#48643,#48644,#48645,
#48646),.UNSPECIFIED.,.F.,.F.,(4,2,4),(3.76031917570416,3.76804109815423,
3.80554677388846),.UNSPECIFIED.) ;
#1227 = B_SPLINE_CURVE_WITH_KNOTS('',3,(#48652,#48653,#48654,#48655,#48656,
#48657,#48658,#48659,#48660,#48661,#48662,#48663,#48664,#48665,#48666,#48667,
#48668,#48669,#48670,#48671,#48672,#48673,#48674,#48675,#48676,#48677,#48678,
#48679,#48680,#48681,#48682,#48683,#48684,#48685,#48686,#48687),
 .UNSPECIFIED.,.F.,.F.,(4,2,2,2,2,2,2,2,2,2,2,2,2,2,2,2,2,4),(3.1176227748347,
3.13096592162681,3.17214416512159,3.21178089063607,3.25164155415437,3.29229454274865,
3.331416941854,3.37209007584933,3.41210537289544,3.45097921650868,3.49166209479253,
3.5312435182945,3.57078165411375,3.61138931078773,3.65047051941298,3.69142496434553,
3.73140528845282,3.76031917570416),.UNSPECIFIED.) ;
#1228 = B_SPLINE_CURVE_WITH_KNOTS('',3,(#48690,#48691,#48692,#48693,#48694,
#48695,#48696,#48697,#48698,#48699,#48700,#48701,#48702,#48703,#48704,#48705,
#48706,#48707,#48708,#48709,#48710,#48711,#48712,#48713,#48714,#48715,#48716,
#48717,#48718,#48719,#48720,#48721,#48722,#48723),.UNSPECIFIED.,.F.,.F.,
(4,2,2,2,2,2,2,2,2,2,2,2,2,2,2,2,4),(0.,0.0362447607018933,0.0713825393809272,
0.110374339020624,0.150892059768638,0.190667140095241,0.230173971071058,
0.271217309410474,0.310173121012165,0.350138836987173,0.390769526483312,
0.429629582897894,0.469935119533493,0.509766123742405,0.549077933529619,
0.589919103429393,0.605457920328374),.UNSPECIFIED.) ;
#1229 = B_SPLINE_CURVE_WITH_KNOTS('',3,(#48728,#48729,#48730,#48731,#48732,
#48733,#48734,#48735,#48736,#48737,#48738,#48739,#48740,#48741,#48742,#48743,
#48744,#48745,#48746,#48747,#48748,#48749,#48750,#48751,#48752,#48753,#48754,
#48755,#48756,#48757,#48758,#48759,#48760,#48761,#48762,#48763),
 .UNSPECIFIED.,.F.,.F.,(4,2,2,2,2,2,2,2,2,2,2,2,2,2,2,2,2,4),(2.47551363283054,
2.49265917852922,2.53346259133496,2.57273744940686,2.6127542482078,2.6530100280249,
2.6918288302763,2.73245659923037,2.77235334434581,2.81134989267037,2.85231605851498,
2.89174829275779,2.93165078035237,2.9720823268742,3.01106427522818,3.05181132055974,
3.09190687687269,3.1176227748347),.UNSPECIFIED.) ;
#1230 = B_SPLINE_CURVE_WITH_KNOTS('',3,(#48764,#48765,#48766,#48767,#48768,
#48769,#48770,#48771,#48772,#48773,#48774,#48775,#48776,#48777,#48778,#48779,
#48780,#48781,#48782,#48783,#48784,#48785,#48786,#48787,#48788,#48789,#48790,
#48791,#48792,#48793,#48794,#48795,#48796,#48797,#48798,#48799),
 .UNSPECIFIED.,.F.,.F.,(4,2,2,2,2,2,2,2,2,2,2,2,2,2,2,2,2,4),(0.605457920328374,
0.62882567261221,0.668602087446539,0.709123355352179,0.747832945812351,
0.787971715930476,0.827929939366068,0.867093635478729,0.907781744119965,
0.946706186283578,0.986340613635276,1.0268012450227,1.06542475571967,1.10544143735414,
1.14559125591013,1.18465312778227,1.22523661095565,1.24467539849028),
 .UNSPECIFIED.) ;
#1231 = B_SPLINE_CURVE_WITH_KNOTS('',3,(#48804,#48805,#48806,#48807,#48808,
#48809,#48810,#48811,#48812,#48813,#48814,#48815,#48816,#48817,#48818,#48819,
#48820,#48821,#48822,#48823,#48824,#48825,#48826,#48827,#48828,#48829,#48830,
#48831,#48832,#48833,#48834,#48835,#48836,#48837,#48838,#48839),
 .UNSPECIFIED.,.F.,.F.,(4,2,2,2,2,2,2,2,2,2,2,2,2,2,2,2,2,4),(1.83528891850249,
1.85722847759532,1.8969538274905,1.93605280977056,1.97648770036395,2.01652614280508,
2.05521120838619,2.09574601251688,2.13538722021168,2.17445838474558,2.21514772520206,
2.25431172318189,2.29450885496653,2.33463376922292,2.37335404255371,2.41391189247215,
2.45365730428937,2.47551363283054),.UNSPECIFIED.) ;
#1232 = B_SPLINE_CURVE_WITH_KNOTS('',3,(#48840,#48841,#48842,#48843,#48844,
#48845,#48846,#48847,#48848,#48849,#48850,#48851,#48852,#48853,#48854,#48855,
#48856,#48857,#48858,#48859,#48860,#48861,#48862,#48863,#48864,#48865,#48866,
#48867,#48868,#48869,#48870,#48871,#48872,#48873,#48874,#48875),
 .UNSPECIFIED.,.F.,.F.,(4,2,2,2,2,2,2,2,2,2,2,2,2,2,2,2,2,4),(1.24467539849028,
1.26424176879834,1.30378115879747,1.34422744626993,1.38282758397962,1.42276641203434,
1.46316332143799,1.50216897752343,1.54269549810761,1.58184036229905,1.62133120061554,
1.66180699594723,1.70044290755449,1.74034782923514,1.78103747545853,1.82003173152049,
1.86054803985681,1.88375019029688),.UNSPECIFIED.) ;
#1233 = B_SPLINE_CURVE_WITH_KNOTS('',3,(#48880,#48881,#48882,#48883,#48884,
#48885,#48886,#48887,#48888,#48889,#48890,#48891,#48892,#48893,#48894,#48895,
#48896,#48897,#48898,#48899,#48900,#48901,#48902,#48903,#48904,#48905,#48906,
#48907,#48908,#48909,#48910,#48911,#48912,#48913,#48914,#48915),
 .UNSPECIFIED.,.F.,.F.,(4,2,2,2,2,2,2,2,2,2,2,2,2,2,2,2,2,4),(1.19352210642917,
1.21931788538152,1.25939797995323,1.30012516537162,1.33909103063952,1.37950565671438,
1.41937748903333,1.45879257698243,1.49974090167009,1.53871284696102,1.57859183853036,
1.61919725112725,1.65799679236964,1.69823346376681,1.73821597445172,1.77747140610762,
1.81825458942883,1.83528891850249),.UNSPECIFIED.) ;
#1234 = B_SPLINE_CURVE_WITH_KNOTS('',3,(#48916,#48917,#48918,#48919,#48920,
#48921,#48922,#48923,#48924,#48925,#48926,#48927,#48928,#48929,#48930,#48931,
#48932,#48933,#48934,#48935,#48936,#48937,#48938,#48939,#48940,#48941,#48942,
#48943,#48944,#48945,#48946,#48947,#48948,#48949,#48950,#48951),
 .UNSPECIFIED.,.F.,.F.,(4,2,2,2,2,2,2,2,2,2,2,2,2,2,2,2,2,4),(1.88375019029688,
1.89988198230334,1.94067697355692,1.97994413167152,2.0198125107436,2.0600679972603,
2.0988807154181,2.13947841767806,2.17938687755795,2.218325919683,2.25930801187248,
2.29875579904418,2.33854583410525,2.37899954199203,2.41792903125738,2.45842422439584,
2.49823169141323,2.52462983086155),.UNSPECIFIED.) ;
#1235 = B_SPLINE_CURVE_WITH_KNOTS('',3,(#48956,#48957,#48958,#48959,#48960,
#48961,#48962,#48963,#48964,#48965,#48966,#48967,#48968,#48969,#48970,#48971,
#48972,#48973,#48974,#48975,#48976,#48977,#48978,#48979,#48980,#48981,#48982,
#48983,#48984,#48985,#48986,#48987,#48988,#48989,#48990,#48991),
 .UNSPECIFIED.,.F.,.F.,(4,2,2,2,2,2,2,2,2,2,2,2,2,2,2,2,2,4),(0.551086143700849,
0.580091364104038,0.620060698665072,0.660986348613251,0.700055552534506,
0.74065064044146,0.780165727193365,0.819734488707212,0.860400666874468,
0.899256714752227,0.939258647894076,0.9799148702805,1.01902321382585,1.05966148145784,
1.09949533248928,1.13911718679827,1.18027997197713,1.19352210642917),
 .UNSPECIFIED.) ;
#1236 = B_SPLINE_CURVE_WITH_KNOTS('',3,(#48992,#48993,#48994,#48995,#48996,
#48997,#48998,#48999,#49000,#49001,#49002,#49003,#49004,#49005,#49006,#49007,
#49008,#49009,#49010,#49011,#49012,#49013,#49014,#49015,#49016,#49017,#49018,
#49019,#49020,#49021,#49022,#49023,#49024,#49025,#49026,#49027),
 .UNSPECIFIED.,.F.,.F.,(4,2,2,2,2,2,2,2,2,2,2,2,2,2,2,2,2,4),(2.52462983086155,
2.53695341089861,2.57783997991567,2.61719599397139,2.6566618302656,2.69703185339974,
2.73588298516227,2.77625185641937,2.81599906562349,2.85456780715886,2.8949483004276,
2.93427001044845,2.97345040080917,3.01379553906095,3.05262495156429,3.09316170023457,
3.13289646793589,3.16251647559856),.UNSPECIFIED.) ;
#1237 = B_SPLINE_CURVE_WITH_KNOTS('',3,(#49033,#49034,#49035,#49036,#49037,
#49038,#49039,#49040,#49041,#49042,#49043,#49044,#49045,#49046,#49047,#49048,
#49049,#49050,#49051,#49052,#49053,#49054),.UNSPECIFIED.,.F.,.F.,(4,2,2,
2,2,2,2,2,2,2,4),(-0.5127490185938,-0.4791046818415,-0.422350585875431,
-0.367729891266528,-0.310500088892541,-0.254538834991981,-0.200332174033985,
-0.143564859003832,-0.0882110501729356,-0.0448733995117723,-9.99999997697287E-7),
 .UNSPECIFIED.) ;
#1238 = B_SPLINE_CURVE_WITH_KNOTS('',3,(#49064,#49065,#49066,#49067,#49068,
#49069,#49070,#49071,#49072,#49073,#49074,#49075,#49076,#49077,#49078,#49079,
#49080,#49081),.UNSPECIFIED.,.F.,.F.,(4,2,2,2,2,2,2,2,4),(-4.73647368332327,
-4.69196976536075,-4.64843188712961,-4.59433805239982,-4.53841454670932,
-4.4815415422272,-4.42697305731884,-4.37027094054635,-4.33840784589812),
 .UNSPECIFIED.) ;
#1239 = B_SPLINE_CURVE_WITH_KNOTS('',3,(#49086,#49087,#49088,#49089,#49090,
#49091,#49092,#49093,#49094,#49095,#49096,#49097,#49098,#49099,#49100,#49101,
#49102,#49103,#49104,#49105,#49106,#49107,#49108,#49109,#49110,#49111,#49112,
#49113,#49114,#49115,#49116,#49117,#49118,#49119,#49120,#49121),
 .UNSPECIFIED.,.F.,.F.,(4,2,2,2,2,2,2,2,2,2,2,2,2,2,2,2,2,4),(-1.4130436997725,
-1.37120186134835,-1.31475362738297,-1.26035723096277,-1.20347805742769,
-1.14760499381641,-1.09307418860522,-1.03566282562664,-0.980432459772098,
-0.924723619832426,-0.868039151939393,-0.813480696262236,-0.756668230447416,
-0.700772408702761,-0.646451202546037,-0.589621104290089,-0.534341469973269,
-0.5127490185938),.UNSPECIFIED.) ;
#1240 = B_SPLINE_CURVE_WITH_KNOTS('',3,(#49122,#49123,#49124,#49125,#49126,
#49127,#49128,#49129,#49130,#49131,#49132,#49133,#49134,#49135,#49136,#49137,
#49138,#49139,#49140,#49141,#49142,#49143,#49144,#49145,#49146,#49147,#49148,
#49149,#49150,#49151,#49152,#49153,#49154,#49155,#49156,#49157),
 .UNSPECIFIED.,.F.,.F.,(4,2,2,2,2,2,2,2,2,2,2,2,2,2,2,2,2,4),(-4.33840784589812,
-4.31528370261049,-4.26006124925725,-4.2033565108894,-4.14918639075426,
-4.09335286929486,-4.03666354972709,-3.98217463220581,-3.92556044694046,
-3.87015538869561,-3.81500178242087,-3.75766624363665,-3.70333313608232,
-3.64753965093067,-3.59081629313595,-3.53651544329802,-3.48015656427228,
-3.44034153207722),.UNSPECIFIED.) ;
#1241 = B_SPLINE_CURVE_WITH_KNOTS('',3,(#49162,#49163,#49164,#49165,#49166,
#49167,#49168,#49169,#49170,#49171,#49172,#49173,#49174,#49175,#49176,#49177,
#49178,#49179,#49180,#49181,#49182,#49183,#49184,#49185,#49186,#49187,#49188,
#49189,#49190,#49191,#49192,#49193,#49194,#49195,#49196,#49197),
 .UNSPECIFIED.,.F.,.F.,(4,2,2,2,2,2,2,2,2,2,2,2,2,2,2,2,2,4),(-2.3125340189891,
-2.26280853691107,-2.20670330818657,-2.15246510273515,-2.09565008652731,
-2.04014590130349,-1.98534363457005,-1.92833595983324,-1.87348000641213,
-1.81705543445323,-1.76080108846584,-1.70653159540569,-1.64970741813391,
-1.59404239838814,-1.53942370358624,-1.48223832446272,-1.42721794334907,
-1.4130436997725),.UNSPECIFIED.) ;
#1242 = B_SPLINE_CURVE_WITH_KNOTS('',3,(#49198,#49199,#49200,#49201,#49202,
#49203,#49204,#49205,#49206,#49207,#49208,#49209,#49210,#49211,#49212,#49213,
#49214,#49215,#49216,#49217,#49218,#49219,#49220,#49221,#49222,#49223,#49224,
#49225,#49226,#49227,#49228,#49229,#49230,#49231,#49232,#49233),
 .UNSPECIFIED.,.F.,.F.,(4,2,2,2,2,2,2,2,2,2,2,2,2,2,2,2,2,4),(-3.44034153207722,
-3.42449939324888,-3.3695764327963,-3.31248866822477,-3.25811683401008,
-3.20255259965505,-3.14590743519229,-3.09177932604525,-3.03563435486918,
-2.97961691515219,-2.92488004954696,-2.8679929655988,-2.81348320940942,
-2.75810237416364,-2.70148807555117,-2.64743700528058,-2.59146262196782,
-2.54379457940395),.UNSPECIFIED.) ;
#1243 = B_SPLINE_CURVE_WITH_KNOTS('',3,(#49238,#49239,#49240,#49241,#49242,
#49243,#49244,#49245,#49246,#49247,#49248,#49249,#49250,#49251,#49252,#49253,
#49254,#49255,#49256,#49257,#49258,#49259,#49260,#49261,#49262,#49263,#49264,
#49265,#49266,#49267,#49268,#49269,#49270,#49271,#49272,#49273,#49274,#49275),
 .UNSPECIFIED.,.F.,.F.,(4,2,2,2,2,2,2,2,2,2,2,2,2,2,2,2,2,2,4),(-3.21306377665209,
-3.2109350187238,-3.15630999768433,-3.09955495100989,-3.04394942532879,
-2.98865641028171,-2.93117704806814,-2.87667453878721,-2.82073950424026,
-2.7638518318754,-2.70940943883827,-2.65290505018767,-2.59703151900695,
-2.54196402257734,-2.48472704457828,-2.43017216514208,-2.37446111862928,
-2.31972208641484,-2.3125340189891),.UNSPECIFIED.) ;
#1244 = B_SPLINE_CURVE_WITH_KNOTS('',3,(#49276,#49277,#49278,#49279,#49280,
#49281,#49282,#49283,#49284,#49285,#49286,#49287,#49288,#49289,#49290,#49291,
#49292,#49293,#49294,#49295,#49296,#49297,#49298,#49299,#49300,#49301,#49302,
#49303,#49304,#49305,#49306,#49307,#49308,#49309,#49310,#49311),
 .UNSPECIFIED.,.F.,.F.,(4,2,2,2,2,2,2,2,2,2,2,2,2,2,2,2,2,4),(-2.54379457940395,
-2.53499384249712,-2.48039669454153,-2.42366105417301,-2.36892283947657,
-2.31203709403285,-2.2573015005488,-2.20128396827585,-2.14514036297612,
-2.09101342368331,-2.03436929753395,-1.9788064537663,-1.92443527467436,
-1.86734896827102,-1.81242739278087,-1.75677036765928,-1.7004129599865,
-1.64704707967164),.UNSPECIFIED.) ;
#1245 = B_SPLINE_CURVE_WITH_KNOTS('',3,(#49316,#49317,#49318,#49319,#49320,
#49321,#49322,#49323,#49324,#49325,#49326,#49327,#49328,#49329,#49330,#49331,
#49332,#49333,#49334,#49335,#49336,#49337,#49338,#49339,#49340,#49341,#49342,
#49343,#49344,#49345,#49346,#49347,#49348,#49349,#49350,#49351),
 .UNSPECIFIED.,.F.,.F.,(4,2,2,2,2,2,2,2,2,2,2,2,2,2,2,2,2,4),(-4.11267130303842,
-4.10328051065977,-4.04848046904968,-3.99153304600001,-3.93665386620444,
-3.88120392580031,-3.82439128324491,-3.770151349457,-3.71409683652575,-3.65700590541931,
-3.60230555473109,-3.54546704580972,-3.49029481285965,-3.43493792993847,
-3.37807712349796,-3.32375037552931,-3.2677797079742,-3.21306377665209),
 .UNSPECIFIED.) ;
#1246 = B_SPLINE_CURVE_WITH_KNOTS('',3,(#49352,#49353,#49354,#49355,#49356,
#49357,#49358,#49359,#49360,#49361,#49362,#49363,#49364,#49365,#49366,#49367,
#49368,#49369,#49370,#49371,#49372,#49373,#49374,#49375,#49376,#49377,#49378,
#49379,#49380,#49381,#49382,#49383,#49384,#49385,#49386,#49387,#49388,#49389),
 .UNSPECIFIED.,.F.,.F.,(4,2,2,2,2,2,2,2,2,2,2,2,2,2,2,2,2,2,4),(-1.64704707967164,
-1.64611351156563,-1.58939131209299,-1.53359932931609,-1.47926712186125,
-1.42193315673438,-1.36678104496521,-1.31137640384191,-1.25476379265969,
-1.20027638045271,-1.14358837833567,-1.08775644043887,-1.03358743775143,
-0.976884004990081,-0.92166313991216,-0.866676489253686,-0.809975892999753,
-0.755408860368642,-0.748981824776657),.UNSPECIFIED.) ;
#1247 = B_SPLINE_CURVE_WITH_KNOTS('',3,(#49392,#49393,#49394,#49395,#49396,
#49397,#49398,#49399,#49400,#49401,#49402,#49403,#49404,#49405,#49406,#49407,
#49408,#49409,#49410,#49411,#49412,#49413,#49414,#49415,#49416,#49417,#49418,
#49419,#49420,#49421),.UNSPECIFIED.,.F.,.F.,(4,2,2,2,2,2,2,2,2,2,2,2,2,
2,4),(-0.748981824776657,-0.698535993165537,-0.642614124209802,-0.588521531236234,
-0.531860990174686,-0.476540820790738,-0.421837810676442,-0.365022008689484,
-0.310349358314276,-0.253978727958169,-0.197918590589397,-0.143815584116504,
-0.0871557349535602,-0.04281124218475,-9.99999995254797E-7),
 .UNSPECIFIED.) ;
#1248 = B_SPLINE_CURVE_WITH_KNOTS('',3,(#49424,#49425,#49426,#49427,#49428,
#49429,#49430,#49431,#49432,#49433,#49434,#49435,#49436,#49437,#49438,#49439,
#49440,#49441,#49442,#49443,#49444,#49445,#49446,#49447,#49448,#49449),
 .UNSPECIFIED.,.F.,.F.,(4,2,2,2,2,2,2,2,2,2,2,2,4),(-4.75229088586126,-4.70738064000878,
-4.66190994418552,-4.60554452353605,-4.54940449410308,-4.49445665866338,
-4.43734919801762,-4.38268536498262,-4.32709195636778,-4.27028565227991,
-4.2160470765991,-4.15986005312993,-4.11267130303842),.UNSPECIFIED.) ;
#1249 = B_SPLINE_CURVE_WITH_KNOTS('',3,(#49452,#49453,#49454,#49455,#49456,
#49457,#49458,#49459,#49460,#49461,#49462,#49463,#49464,#49465,#49466,#49467,
#49468,#49469,#49470,#49471,#49472,#49473,#49474,#49475,#49476,#49477,#49478,
#49479,#49480,#49481,#49482,#49483,#49484,#49485,#49486,#49487),
 .UNSPECIFIED.,.F.,.F.,(4,2,2,2,2,2,2,2,2,2,2,2,2,2,2,2,2,4),(3.16251647559856,
3.17137245211693,3.2116796469811,3.25100123675646,3.28999047999364,3.33034285308588,
3.36918080157474,3.40942349288676,3.44918923883973,3.48762599981309,3.52790110502513,
3.56726810641456,3.60611479764238,3.64652089125254,3.68541194336664,3.72540539515703,
3.75694807253539,3.78793834700464),.UNSPECIFIED.) ;
#1250 = B_SPLINE_CURVE_WITH_KNOTS('',3,(#49490,#49491,#49492,#49493,#49494,
#49495,#49496,#49497,#49498,#49499,#49500,#49501,#49502,#49503,#49504,#49505,
#49506,#49507,#49508,#49509,#49510,#49511,#49512,#49513,#49514,#49515,#49516,
#49517,#49518,#49519,#49520,#49521),.UNSPECIFIED.,.F.,.F.,(4,2,2,2,2,2,
2,2,2,2,2,2,2,2,2,4),(0.,0.0310342811770257,0.0631788586655503,0.103792072582309,
0.142927747157277,0.182499758214421,0.223021898301352,0.26169644603923,
0.301676590400516,0.34228887040074,0.381346179193425,0.421927213271208,
0.461229947766521,0.50077767437492,0.541351637872867,0.551086143700849),
 .UNSPECIFIED.) ;
#1251 = B_SPLINE_CURVE_WITH_KNOTS('',3,(#49575,#49576,#49577,#49578,#49579,
#49580,#49581,#49582,#49583,#49584,#49585,#49586,#49587,#49588,#49589,#49590,
#49591,#49592,#49593,#49594,#49595,#49596,#49597,#49598,#49599,#49600,#49601,
#49602),.UNSPECIFIED.,.F.,.F.,(4,2,2,2,2,2,2,2,2,2,2,2,2,4),(0.399647517238767,
0.414836450199711,0.509002403599096,0.597571527890476,0.712371649335664,
0.853837527204609,1.00187230702159,1.07695219700279,1.22621700116326,1.38697607123365,
1.59961645957477,1.92493151906482,2.10597394645267,2.30088796086391),
 .UNSPECIFIED.) ;
#1252 = B_SPLINE_CURVE_WITH_KNOTS('',3,(#49606,#49607,#49608,#49609,#49610,
#49611,#49612,#49613,#49614,#49615,#49616,#49617,#49618,#49619,#49620,#49621),
 .UNSPECIFIED.,.F.,.F.,(4,2,2,2,2,2,2,4),(0.,0.0370319719196131,0.0786050619190432,
0.13215361237448,0.200684934374393,0.287669832057025,0.368937178455222,
0.399647517238767),.UNSPECIFIED.) ;
#1253 = B_SPLINE_CURVE_WITH_KNOTS('',3,(#49622,#49623,#49624,#49625,#49626,
#49627,#49628,#49629,#49630,#49631,#49632,#49633,#49634,#49635),
 .UNSPECIFIED.,.F.,.F.,(4,2,2,2,2,2,4),(-0.43561391109166,-0.34804890840793,
-0.259297090185586,-0.130480653501234,-0.0941897273832555,-0.0477567516765395,
-1.00000015618162E-6),.UNSPECIFIED.) ;
#1254 = B_SPLINE_CURVE_WITH_KNOTS('',3,(#49754,#49755,#49756,#49757,#49758,
#49759,#49760,#49761,#49762,#49763,#49764,#49765,#49766,#49767,#49768,#49769,
#49770,#49771),.UNSPECIFIED.,.F.,.F.,(4,2,2,2,2,2,2,2,4),(-0.187329172980139,
-0.147618547087121,-0.107318887539879,-0.0863692505416251,-0.0717625756301755,
-0.064857392647619,-0.0552393980697806,-0.026417184758918,0.),
 .UNSPECIFIED.) ;
#1255 = B_SPLINE_CURVE_WITH_KNOTS('',3,(#49772,#49773,#49774,#49775,#49776,
#49777,#49778,#49779,#49780,#49781,#49782,#49783,#49784,#49785,#49786,#49787,
#49788,#49789),.UNSPECIFIED.,.F.,.F.,(4,2,2,2,2,2,2,2,4),(-0.248177093231301,
-0.207320659555912,-0.163004039773727,-0.146139995385165,-0.120240458034777,
-0.0958299418542064,-0.0607027452784435,-0.0303308437384981,-1.00000010200274E-6),
 .UNSPECIFIED.) ;
#1256 = B_SPLINE_CURVE_WITH_KNOTS('',3,(#50230,#50231,#50232,#50233,#50234,
#50235,#50236,#50237,#50238,#50239,#50240,#50241,#50242,#50243,#50244,#50245,
#50246,#50247,#50248,#50249,#50250,#50251,#50252,#50253,#50254,#50255,#50256,
#50257),.UNSPECIFIED.,.F.,.F.,(4,2,2,2,2,2,2,2,2,2,2,2,2,4),(0.459093916516044,
0.46455562735916,0.505821881594587,0.520988271639936,0.529970590367133,
0.542578350982259,0.575709939682203,0.614672647551458,0.632542444852366,
0.649281677754947,0.689464111786888,0.720032267469635,0.726902083818049,
0.732437476861398),.UNSPECIFIED.) ;
#1257 = B_SPLINE_CURVE_WITH_KNOTS('',3,(#50260,#50261,#50262,#50263,#50264,
#50265,#50266,#50267,#50268,#50269,#50270,#50271,#50272,#50273,#50274,#50275,
#50276,#50277,#50278,#50279,#50280,#50281,#50282,#50283,#50284,#50285,#50286,
#50287,#50288,#50289,#50290,#50291,#50292,#50293,#50294,#50295),
 .UNSPECIFIED.,.F.,.F.,(4,2,2,2,2,2,2,2,2,2,2,2,2,2,2,2,2,4),(0.000332701134793292,
0.00532995658148356,0.0119825509393597,0.0487188803356833,0.0844089965964979,
0.100361879460944,0.116282468689568,0.149629266254007,0.178290336895723,
0.190733178272163,0.201074425783365,0.210399404436054,0.232074117560219,
0.28208000915706,0.30011450772679,0.315087246273823,0.336912777571983,0.381141457942968),
 .UNSPECIFIED.) ;
#1258 = B_SPLINE_CURVE_WITH_KNOTS('',3,(#50301,#50302,#50303,#50304,#50305,
#50306,#50307,#50308,#50309,#50310,#50311,#50312,#50313,#50314,#50315,#50316,
#50317,#50318,#50319,#50320,#50321,#50322,#50323,#50324,#50325,#50326,#50327,
#50328,#50329,#50330,#50331,#50332,#50333,#50334,#50335,#50336,#50337,#50338,
#50339,#50340,#50341,#50342,#50343,#50344,#50345,#50346,#50347,#50348,#50349,
#50350,#50351,#50352,#50353,#50354,#50355,#50356,#50357,#50358,#50359,#50360,
#50361,#50362,#50363,#50364,#50365,#50366,#50367,#50368,#50369,#50370,#50371,
#50372,#50373,#50374,#50375,#50376,#50377,#50378),.UNSPECIFIED.,.F.,.F.,
(4,2,2,2,2,2,2,2,2,2,2,2,2,2,2,2,2,2,2,2,2,2,2,2,2,2,2,2,2,2,2,2,2,2,2,
2,2,2,4),(1.29365561641325,1.30113546894178,1.31756663056678,1.33312830280463,
1.36194319812924,1.40306001798898,1.41707239726473,1.42583345144023,1.438907235276,
1.4567472055773,1.50742443095404,1.52367565736048,1.53936823703037,1.57015419556187,
1.61065266245251,1.62355132522206,1.63233056992128,1.64662569486736,1.66730671714928,
1.71296324961579,1.72915479064639,1.74486354159992,1.77604692182362,1.81647765873443,
1.82921296125272,1.83797276770033,1.85234265187279,1.87321966665841,1.91832818857784,
1.93450511617934,1.95007856425548,1.97985222672331,2.02092117751393,2.03443886875799,
2.04322587270968,2.05689828304459,2.07604574726155,2.11487866906583,2.12885059658721),
 .UNSPECIFIED.) ;
#1259 = B_SPLINE_CURVE_WITH_KNOTS('',3,(#50379,#50380,#50381,#50382,#50383,
#50384,#50385,#50386,#50387,#50388,#50389,#50390,#50391,#50392,#50393,#50394,
#50395,#50396,#50397,#50398,#50399,#50400,#50401,#50402,#50403,#50404,#50405,
#50406,#50407,#50408,#50409,#50410,#50411,#50412,#50413,#50414,#50415,#50416,
#50417,#50418,#50419,#50420),.UNSPECIFIED.,.F.,.F.,(4,2,2,2,2,2,2,2,2,2,
2,2,2,2,2,2,2,2,2,2,4),(0.000735163267886744,0.0138746955681923,0.0296423865919577,
0.0801063196227826,0.106649689626277,0.116363467174073,0.126486258322458,
0.164825866697053,0.201303399889853,0.217473147550887,0.233580681855967,
0.267585305229778,0.296202685786829,0.313253112284756,0.322102080649573,
0.33246197481545,0.366409709031667,0.408171648460054,0.424893469175312,
0.43988857479256,0.459093916516044),.UNSPECIFIED.) ;
#1260 = B_SPLINE_CURVE_WITH_KNOTS('',3,(#50421,#50422,#50423,#50424,#50425,
#50426,#50427,#50428,#50429,#50430,#50431,#50432,#50433,#50434,#50435,#50436,
#50437,#50438,#50439,#50440,#50441,#50442,#50443,#50444,#50445,#50446,#50447,
#50448,#50449,#50450,#50451,#50452,#50453,#50454,#50455,#50456,#50457,#50458,
#50459,#50460,#50461,#50462,#50463,#50464,#50465,#50466,#50467,#50468,#50469,
#50470,#50471,#50472,#50473,#50474,#50475,#50476,#50477,#50478,#50479,#50480,
#50481,#50482,#50483,#50484,#50485,#50486,#50487,#50488,#50489,#50490,#50491,
#50492,#50493,#50494,#50495,#50496,#50497,#50498,#50499,#50500,#50501,#50502,
#50503,#50504,#50505,#50506,#50507,#50508,#50509,#50510,#50511,#50512,#50513,
#50514,#50515,#50516,#50517,#50518,#50519,#50520,#50521,#50522,#50523,#50524,
#50525,#50526,#50527,#50528,#50529,#50530,#50531,#50532,#50533,#50534),
 .UNSPECIFIED.,.F.,.F.,(4,2,2,2,2,2,2,2,2,2,2,2,2,2,2,2,2,2,2,2,2,2,2,2,
2,2,2,2,2,2,2,2,2,2,2,2,2,2,2,2,2,2,2,2,2,2,2,2,2,2,2,2,2,2,2,2,4),(9.99999991669717E-7,
0.0184447153223968,0.0263230505661795,0.036124778687421,0.0777207405050378,
0.102193231964045,0.121768138081197,0.136562874516093,0.155835590898569,
0.200176795636776,0.223236930617453,0.232676101620211,0.242768076763171,
0.281244235113264,0.318133316641436,0.334188540648712,0.349821365894987,
0.404181271018304,0.421248051626733,0.433948239560394,0.442676632303089,
0.45695402708308,0.498123802940828,0.526459180733287,0.541922825721667,
0.558274678127576,0.608828260701387,0.626375137247475,0.639298848005466,
0.648006132300929,0.661936527802842,0.702985516242036,0.731840841610424,
0.747335614023785,0.763614463819922,0.813238739648188,0.83939123519187,
0.849033315152608,0.858910393837397,0.899917598632736,0.935729657832649,
0.951576711293341,0.96742262672389,1.01680549308803,1.03610593709597,1.04980856829621,
1.05851147029703,1.07163514017831,1.11229204645002,1.14255802948317,1.1581480745398,
1.17429114011009,1.22532712172044,1.25069491457693,1.26029683909567,1.27022952044346,
1.29379821101641),.UNSPECIFIED.) ;
#1261 = B_SPLINE_CURVE_WITH_KNOTS('',3,(#50540,#50541,#50542,#50543,#50544,
#50545,#50546,#50547,#50548,#50549,#50550,#50551,#50552,#50553,#50554,#50555,
#50556,#50557,#50558,#50559,#50560,#50561,#50562,#50563,#50564,#50565,#50566,
#50567,#50568,#50569,#50570,#50571,#50572,#50573,#50574,#50575,#50576,#50577,
#50578,#50579,#50580,#50581,#50582,#50583,#50584,#50585,#50586,#50587,#50588,
#50589,#50590,#50591,#50592,#50593,#50594,#50595,#50596,#50597,#50598,#50599,
#50600,#50601,#50602,#50603,#50604,#50605,#50606,#50607,#50608,#50609,#50610,
#50611,#50612,#50613,#50614,#50615,#50616,#50617,#50618,#50619,#50620,#50621,
#50622,#50623,#50624,#50625,#50626,#50627,#50628,#50629,#50630),
 .UNSPECIFIED.,.F.,.F.,(4,3,3,3,3,3,3,3,3,3,3,3,3,3,3,3,3,3,3,3,3,3,3,3,
3,3,3,3,3,3,4),(15.707963267949,15.8113162289403,15.9146430055769,16.0179789766908,
16.1214346358621,16.2249545823278,16.3224671580076,16.3286700874657,16.3947464669144,
16.3947981013555,16.489367670122,16.4989544967138,16.6029510560627,16.706819180176,
16.8106179355233,16.9143822485449,17.0181469982565,17.1220156832995,17.2259403207901,
17.3243464907781,17.3300437451009,17.3930767925987,17.3931266456449,17.488158788607,
17.4974450344715,17.6010532740212,17.606557916941,17.7106004897465,17.8145739596521,
17.9185190132978,17.9338965643494),.UNSPECIFIED.) ;
#1262 = B_SPLINE_CURVE_WITH_KNOTS('',3,(#50632,#50633,#50634,#50635,#50636,
#50637,#50638,#50639,#50640,#50641,#50642,#50643,#50644,#50645,#50646,#50647,
#50648,#50649,#50650,#50651,#50652,#50653,#50654,#50655,#50656,#50657,#50658,
#50659,#50660,#50661,#50662,#50663,#50664,#50665,#50666,#50667,#50668,#50669,
#50670,#50671),.UNSPECIFIED.,.F.,.F.,(4,3,3,3,3,3,3,3,3,3,3,3,3,4),(14.3981410127767,
14.5041304628989,14.6100344213185,14.7159061169048,14.8217654368488,14.9276423442954,
15.0335668127656,15.1396478264459,15.2458169541302,15.3521882187467,15.3964695570661,
15.5190017212959,15.6402256956334,15.7079554188088),.UNSPECIFIED.) ;
#1263 = B_SPLINE_CURVE_WITH_KNOTS('',3,(#50674,#50675,#50676,#50677,#50678,
#50679,#50680,#50681,#50682,#50683,#50684,#50685,#50686,#50687,#50688,#50689,
#50690,#50691,#50692,#50693,#50694,#50695,#50696,#50697,#50698,#50699,#50700,
#50701,#50702,#50703,#50704,#50705,#50706,#50707,#50708,#50709,#50710,#50711,
#50712,#50713,#50714,#50715,#50716,#50717,#50718,#50719,#50720,#50721,#50722,
#50723,#50724,#50725,#50726,#50727,#50728,#50729,#50730,#50731,#50732,#50733,
#50734,#50735,#50736,#50737,#50738,#50739,#50740,#50741,#50742,#50743,#50744,
#50745,#50746,#50747),.UNSPECIFIED.,.F.,.F.,(4,2,2,2,2,2,2,2,2,2,2,2,2,
2,2,2,2,2,2,2,2,2,2,2,2,2,2,2,2,2,2,2,2,2,2,2,4),(9.08164939039677E-5,0.00964446188066229,
0.0631727038946699,0.0833213424346721,0.0995270112478277,0.11521076241323,
0.168160574823218,0.192914913994012,0.202483681644903,0.212472572657854,
0.25229975169802,0.277505378195093,0.297440690943511,0.312324763000316,
0.331569412660729,0.375644072231997,0.398570725096213,0.408027582384325,
0.418068765141332,0.451392820401004,0.491734973859357,0.508171201472686,
0.52328080899074,0.548904583706971,0.592593255836169,0.607623400269449,
0.616321082217894,0.62824029431287,0.661333455958532,0.699795498757593,
0.715650850691533,0.731252650752003,0.763193487628226,0.808059994616459,
0.818142249781261,0.826085801679224,0.835754501023224),.UNSPECIFIED.) ;
#1264 = B_SPLINE_CURVE_WITH_KNOTS('',3,(#50753,#50754,#50755,#50756,#50757,
#50758),.UNSPECIFIED.,.F.,.F.,(4,2,4),(0.688175935048327,0.722528389859189,
0.732483913740625),.UNSPECIFIED.) ;
#1265 = B_SPLINE_CURVE_WITH_KNOTS('',3,(#50761,#50762,#50763,#50764,#50765,
#50766,#50767,#50768,#50769,#50770,#50771,#50772,#50773,#50774,#50775,#50776,
#50777,#50778),.UNSPECIFIED.,.F.,.F.,(4,2,2,2,2,2,2,2,4),(0.000326322779117739,
0.0053095587093796,0.0119345202360929,0.0491915472726964,0.0845062818898445,
0.100433841269843,0.116331511114054,0.149505453170145,0.152028373115396),
 .UNSPECIFIED.) ;
#1266 = B_SPLINE_CURVE_WITH_KNOTS('',3,(#50784,#50785,#50786,#50787,#50788,
#50789,#50790,#50791,#50792,#50793,#50794,#50795,#50796,#50797,#50798,#50799,
#50800,#50801,#50802,#50803,#50804,#50805,#50806,#50807,#50808,#50809,#50810,
#50811,#50812,#50813,#50814,#50815,#50816,#50817,#50818,#50819,#50820,#50821,
#50822,#50823,#50824,#50825,#50826,#50827,#50828,#50829,#50830,#50831,#50832,
#50833,#50834,#50835,#50836,#50837,#50838,#50839),.UNSPECIFIED.,.F.,.F.,
(4,2,2,2,2,2,2,2,2,2,2,2,2,2,2,2,2,2,2,2,2,2,2,2,2,2,2,4),(1.98102711455768,
1.98958188275697,2.00867262502161,2.03197282727063,2.07443930051198,2.08480989656363,
2.09422631816803,2.11636340346817,2.16057507188391,2.18055526267638,2.19552374775884,
2.21498613387434,2.23909906769021,2.28155745479864,2.29133239102646,2.3011688929944,
2.33194922685791,2.37661912184551,2.39284432220525,2.40839273375275,2.43776671592168,
2.47890861126898,2.49264355354582,2.5014268582012,2.51487424116833,2.53350674094852,
2.5735412222785,2.58730157653673),.UNSPECIFIED.) ;
#1267 = B_SPLINE_CURVE_WITH_KNOTS('',3,(#50840,#50841,#50842,#50843,#50844,
#50845,#50846,#50847,#50848,#50849,#50850,#50851,#50852,#50853,#50854,#50855,
#50856,#50857,#50858,#50859,#50860,#50861,#50862,#50863,#50864,#50865,#50866,
#50867,#50868,#50869,#50870,#50871,#50872,#50873,#50874,#50875,#50876,#50877,
#50878,#50879,#50880,#50881,#50882,#50883,#50884,#50885,#50886,#50887,#50888,
#50889,#50890,#50891,#50892,#50893,#50894,#50895,#50896,#50897,#50898,#50899,
#50900,#50901),.UNSPECIFIED.,.F.,.F.,(4,2,2,2,2,2,2,2,2,2,2,2,2,2,2,2,2,
2,2,2,2,2,2,2,2,2,2,2,2,2,4),(0.000740443363498194,0.0138349862975699,0.0295154725943613,
0.0790451299155813,0.106523846021425,0.116283064754404,0.126365470374231,
0.165172536751136,0.201324346128904,0.217457679525018,0.233551669346709,
0.267457400749719,0.296225634265475,0.313321898958139,0.322168521883493,
0.332525058471953,0.366431274633955,0.408017845899989,0.424714758522178,
0.439696860657482,0.4643168630784,0.505291340570378,0.520968983786635,0.529935246689459,
0.542398396489085,0.575204404091594,0.614943460595965,0.632807529475108,
0.649590886610583,0.66732217651446,0.688175935048327),.UNSPECIFIED.) ;
#1268 = B_SPLINE_CURVE_WITH_KNOTS('',3,(#50903,#50904,#50905,#50906,#50907,
#50908,#50909,#50910,#50911,#50912,#50913,#50914,#50915,#50916,#50917,#50918,
#50919,#50920,#50921,#50922,#50923,#50924),.UNSPECIFIED.,.F.,.F.,(4,2,2,
2,2,2,2,2,2,2,4),(0.152028373115396,0.178271254198615,0.190732100705371,
0.201082878473419,0.210411761708287,0.232100824336856,0.282188910937535,
0.300143539111472,0.315112949643421,0.337038683452346,0.38114427299709),
 .UNSPECIFIED.) ;
#1269 = B_SPLINE_CURVE_WITH_KNOTS('',3,(#50925,#50926,#50927,#50928,#50929,
#50930,#50931,#50932,#50933,#50934,#50935,#50936,#50937,#50938,#50939,#50940,
#50941,#50942,#50943,#50944,#50945,#50946,#50947,#50948,#50949,#50950,#50951,
#50952,#50953,#50954,#50955,#50956,#50957,#50958,#50959,#50960,#50961,#50962,
#50963,#50964,#50965,#50966,#50967,#50968,#50969,#50970,#50971,#50972,#50973,
#50974,#50975,#50976,#50977,#50978,#50979,#50980,#50981,#50982,#50983,#50984,
#50985,#50986,#50987,#50988,#50989,#50990,#50991,#50992,#50993,#50994,#50995,
#50996,#50997,#50998,#50999,#51000,#51001,#51002,#51003,#51004,#51005,#51006,
#51007,#51008,#51009,#51010,#51011,#51012,#51013,#51014,#51015,#51016,#51017,
#51018,#51019,#51020),.UNSPECIFIED.,.F.,.F.,(4,2,2,2,2,2,2,2,2,2,2,2,2,
2,2,2,2,2,2,2,2,2,2,2,2,2,2,2,2,2,2,2,2,2,2,2,2,2,2,2,2,2,2,2,2,2,2,4),
(9.99999998689338E-7,0.0174292635150208,0.0254334249445552,0.034789333326389,
0.0508440411265439,0.0912843741617236,0.111367032937248,0.127643504238079,
0.142995575497015,0.170701023554272,0.20580631807345,0.219337663136388,
0.230262195740999,0.239264644851289,0.257288082646908,0.297769585088541,
0.317929655952516,0.334037200357709,0.349643368751472,0.404845134658746,
0.428697831040931,0.438205956602896,0.448279237366973,0.487071365345615,
0.523692736645848,0.539737861694203,0.555412355415605,0.60929867965605,
0.634103560413446,0.643671473439017,0.653641438561538,0.69361372217156,
0.729510278592592,0.745504798507947,0.76120034152742,0.814297588916916,
0.839633215522294,0.849230500429995,0.859158345347323,0.899622697096617,
0.935800805641872,0.951658023515114,0.967490300857546,1.01703691034612,
1.03627966855327,1.04995760843149,1.05865975920911,1.06478356715028),
 .UNSPECIFIED.) ;
#1270 = B_SPLINE_CURVE_WITH_KNOTS('',3,(#51026,#51027,#51028,#51029,#51030,
#51031,#51032,#51033,#51034,#51035,#51036,#51037,#51038,#51039,#51040,#51041,
#51042,#51043,#51044,#51045,#51046,#51047,#51048,#51049),.UNSPECIFIED.,
 .F.,.F.,(4,2,2,2,2,2,2,2,2,2,2,4),(2.35872509297639,2.36454743071151,2.38374966573916,
2.39854959804016,2.41821532462426,2.44290115786587,2.48383265586654,2.49371083602286,
2.50342578994992,2.52999234611409,2.57237232063052,2.58784193793521),
 .UNSPECIFIED.) ;
#1271 = B_SPLINE_CURVE_WITH_KNOTS('',3,(#51051,#51052,#51053,#51054,#51055,
#51056,#51057,#51058,#51059,#51060,#51061,#51062,#51063,#51064,#51065,#51066,
#51067,#51068,#51069,#51070,#51071,#51072,#51073,#51074,#51075,#51076,#51077,
#51078,#51079,#51080,#51081,#51082,#51083,#51084,#51085,#51086,#51087,#51088,
#51089,#51090,#51091,#51092,#51093,#51094,#51095,#51096,#51097,#51098,#51099,
#51100,#51101,#51102,#51103,#51104,#51105,#51106,#51107,#51108,#51109,#51110,
#51111,#51112,#51113,#51114,#51115,#51116,#51117,#51118,#51119,#51120,#51121,
#51122,#51123,#51124,#51125,#51126,#51127,#51128,#51129,#51130,#51131,#51132,
#51133,#51134,#51135,#51136,#51137,#51138,#51139,#51140,#51141),
 .UNSPECIFIED.,.F.,.F.,(4,3,3,3,3,3,3,3,3,3,3,3,3,3,3,3,3,3,3,3,3,3,3,3,
3,3,3,3,3,3,4),(15.707963267949,15.8112952063224,15.9146002263953,16.0179137372553,
16.1213459971886,16.2248419869704,16.322362584987,16.3285328702908,16.394747429185,
16.3947981013556,16.4893602620961,16.4989462658854,16.6029345449639,16.7067943250266,
16.8105846969145,16.9143405893863,17.0180968837363,17.1219570901659,17.2258732220661,
17.3242843261941,17.3299681660503,17.3930783662191,17.3931266456449,17.4881614419572,
17.4974411081676,17.6010539690716,17.606553977256,17.710593186314,17.8145634851322,
17.9185056328178,17.9338925845213),.UNSPECIFIED.) ;
#1272 = B_SPLINE_CURVE_WITH_KNOTS('',3,(#51143,#51144,#51145,#51146,#51147,
#51148,#51149,#51150,#51151,#51152,#51153,#51154,#51155,#51156,#51157,#51158,
#51159,#51160,#51161,#51162,#51163,#51164,#51165,#51166,#51167,#51168,#51169,
#51170,#51171,#51172,#51173,#51174,#51175,#51176,#51177,#51178,#51179,#51180,
#51181,#51182),.UNSPECIFIED.,.F.,.F.,(4,3,3,3,3,3,3,3,3,3,3,3,3,4),(14.3981410127768,
14.5041552849212,14.610085034542,14.7159837761904,14.8218708833437,14.9277762546341,
15.0337297999276,15.1398405743496,15.246039878247,15.3524416189491,15.3964695570662,
15.5190178529893,15.6402487977518,15.7079553869838),.UNSPECIFIED.) ;
#1273 = B_SPLINE_CURVE_WITH_KNOTS('',3,(#51186,#51187,#51188,#51189,#51190,
#51191,#51192,#51193,#51194,#51195,#51196,#51197,#51198,#51199,#51200,#51201,
#51202,#51203,#51204,#51205,#51206,#51207,#51208,#51209,#51210,#51211,#51212,
#51213,#51214,#51215,#51216,#51217,#51218,#51219,#51220,#51221,#51222,#51223),
 .UNSPECIFIED.,.F.,.F.,(4,2,2,2,2,2,2,2,2,2,2,2,2,2,2,2,2,2,4),(0.000124769152405228,
0.00530283650978471,0.0119163883522527,0.0412949498779639,0.0805290761834309,
0.0975098147518704,0.112590970716538,0.1376147116016,0.175122950526936,
0.188971300360272,0.200067436032103,0.209050888113163,0.226868360620307,
0.258115591573283,0.289449081113609,0.305266632561115,0.321115120108506,
0.358122798341047,0.377579306682493),.UNSPECIFIED.) ;
#1274 = B_SPLINE_CURVE_WITH_KNOTS('',3,(#51224,#51225,#51226,#51227,#51228,
#51229,#51230,#51231,#51232,#51233,#51234,#51235,#51236,#51237,#51238,#51239,
#51240,#51241,#51242,#51243,#51244,#51245,#51246,#51247,#51248,#51249,#51250,
#51251,#51252,#51253,#51254,#51255,#51256,#51257,#51258,#51259,#51260,#51261,
#51262,#51263,#51264,#51265,#51266,#51267,#51268,#51269,#51270,#51271,#51272,
#51273,#51274,#51275,#51276,#51277,#51278,#51279,#51280,#51281,#51282,#51283,
#51284,#51285),.UNSPECIFIED.,.F.,.F.,(4,2,2,2,2,2,2,2,2,2,2,2,2,2,2,2,2,
2,2,2,2,2,2,2,2,2,2,2,2,2,4),(9.999999931312E-7,0.0195843476304998,0.0296126220572481,
0.039313713778823,0.087896979280459,0.109292353934291,0.127460709263585,
0.142411374670944,0.163896663152293,0.207090939979833,0.227594924564628,
0.236857837595574,0.247394214498245,0.288505026781035,0.322917817070159,
0.338779331894746,0.354790271445652,0.392049970295044,0.427641430355377,
0.438989063679899,0.447877993643495,0.465017643283455,0.506415288618611,
0.526589770247727,0.542852862564029,0.558535544036832,0.614023558862245,
0.637818889649371,0.647353831033265,0.657516966897515,0.687313624506759),
 .UNSPECIFIED.) ;
#1275 = B_SPLINE_CURVE_WITH_KNOTS('',3,(#51291,#51292,#51293,#51294,#51295,
#51296,#51297,#51298,#51299,#51300,#51301,#51302,#51303,#51304,#51305,#51306,
#51307,#51308,#51309,#51310,#51311,#51312,#51313,#51314,#51315,#51316,#51317,
#51318),.UNSPECIFIED.,.F.,.F.,(4,2,2,2,2,2,2,2,2,2,2,2,2,4),(0.459106433511841,
0.46421803988814,0.505059886921481,0.52089212016626,0.529860094088288,0.542206609381327,
0.57500566722291,0.615055906254151,0.632916344569532,0.649718573849782,
0.687670392249843,0.719981615275833,0.726884172836083,0.732443895036435),
 .UNSPECIFIED.) ;
#1276 = B_SPLINE_CURVE_WITH_KNOTS('',3,(#51321,#51322,#51323,#51324,#51325,
#51326,#51327,#51328,#51329,#51330,#51331,#51332,#51333,#51334,#51335,#51336,
#51337,#51338,#51339,#51340,#51341,#51342,#51343,#51344,#51345,#51346,#51347,
#51348,#51349,#51350,#51351,#51352,#51353,#51354,#51355,#51356),
 .UNSPECIFIED.,.F.,.F.,(4,2,2,2,2,2,2,2,2,2,2,2,2,2,2,2,2,4),(0.000323627366430275,
0.00530468234356636,0.0119236929644194,0.0492443118740968,0.0845209544914468,
0.100443254054711,0.116328626559381,0.149319629535501,0.178221238025312,
0.190706602926174,0.2010706929436,0.210395000645647,0.232013989441357,0.281746612914986,
0.299850090908258,0.314796919879222,0.33640350897614,0.381145592574581),
 .UNSPECIFIED.) ;
#1277 = B_SPLINE_CURVE_WITH_KNOTS('',3,(#51362,#51363,#51364,#51365,#51366,
#51367,#51368,#51369,#51370,#51371,#51372,#51373,#51374,#51375,#51376,#51377,
#51378,#51379,#51380,#51381,#51382,#51383,#51384,#51385,#51386,#51387,#51388,
#51389,#51390,#51391,#51392,#51393,#51394,#51395,#51396,#51397,#51398,#51399,
#51400,#51401,#51402,#51403,#51404,#51405,#51406,#51407,#51408,#51409,#51410,
#51411,#51412,#51413,#51414,#51415,#51416,#51417,#51418,#51419,#51420,#51421,
#51422,#51423,#51424,#51425,#51426,#51427,#51428,#51429,#51430,#51431,#51432,
#51433,#51434,#51435,#51436,#51437,#51438,#51439),.UNSPECIFIED.,.F.,.F.,
(4,2,2,2,2,2,2,2,2,2,2,2,2,2,2,2,2,2,2,2,2,2,2,2,2,2,2,2,2,2,2,2,2,2,2,
2,2,2,4),(0.458634629932413,0.468300840510139,0.484196861274041,0.50016509288339,
0.548723419503458,0.568340131710824,0.582191837596508,0.59094604609867,
0.604144741830108,0.64702296667436,0.675665519837222,0.691218868871637,
0.70767490065704,0.72781583866651,0.771167490136565,0.786448567224049,0.795305947097795,
0.807310050431355,0.840575503830774,0.87876863269993,0.894763994595969,
0.910638413268068,0.945390278369844,0.985953035480812,0.996560194075815,
1.0057826482125,1.0258531736437,1.06679615831433,1.08978974441653,1.1048418048654,
1.12234040877952,1.14239095099251,1.18372609071405,1.19842596399046,1.20722957825154,
1.21990039351384,1.23683119570789,1.28103441539912,1.29379172823382),
 .UNSPECIFIED.) ;
#1278 = B_SPLINE_CURVE_WITH_KNOTS('',3,(#51440,#51441,#51442,#51443,#51444,
#51445,#51446,#51447,#51448,#51449,#51450,#51451,#51452,#51453,#51454,#51455,
#51456,#51457,#51458,#51459,#51460,#51461,#51462,#51463,#51464,#51465,#51466,
#51467,#51468,#51469,#51470,#51471,#51472,#51473,#51474,#51475,#51476,#51477,
#51478,#51479,#51480,#51481),.UNSPECIFIED.,.F.,.F.,(4,2,2,2,2,2,2,2,2,2,
2,2,2,2,2,2,2,2,2,2,4),(0.000743070825158928,0.0138183874138461,0.0294632506701812,
0.078638337800008,0.106479908835764,0.116255202249531,0.12632377121154,
0.165286117290309,0.201331912606227,0.217452660851885,0.233541178068994,
0.267395556774417,0.296229585496045,0.31334574782802,0.322192112681112,
0.332547173019449,0.366439965368885,0.407958097916761,0.424645227747565,
0.439621348066991,0.459106433511841),.UNSPECIFIED.) ;
#1279 = B_SPLINE_CURVE_WITH_KNOTS('',3,(#51482,#51483,#51484,#51485,#51486,
#51487,#51488,#51489,#51490,#51491,#51492,#51493,#51494,#51495,#51496,#51497,
#51498,#51499,#51500,#51501,#51502,#51503,#51504,#51505,#51506,#51507,#51508,
#51509,#51510,#51511,#51512,#51513,#51514,#51515,#51516,#51517,#51518,#51519,
#51520,#51521,#51522,#51523,#51524,#51525,#51526,#51527,#51528,#51529,#51530,
#51531,#51532,#51533,#51534,#51535,#51536,#51537,#51538,#51539,#51540,#51541,
#51542,#51543,#51544,#51545,#51546,#51547,#51548,#51549,#51550,#51551,#51552,
#51553,#51554,#51555,#51556,#51557,#51558,#51559,#51560,#51561,#51562,#51563,
#51564,#51565,#51566,#51567,#51568,#51569,#51570,#51571,#51572,#51573,#51574,
#51575,#51576,#51577,#51578,#51579,#51580,#51581,#51582,#51583,#51584,#51585,
#51586,#51587,#51588,#51589,#51590,#51591,#51592,#51593,#51594,#51595,#51596,
#51597),.UNSPECIFIED.,.F.,.F.,(4,2,2,2,2,2,2,2,2,2,2,2,2,2,2,2,2,2,2,2,
2,2,2,2,2,2,2,2,2,2,2,2,2,2,2,2,2,2,2,2,2,2,2,2,2,2,2,2,2,2,2,2,2,2,2,2,
2,4),(1.00000002227832E-6,0.0112238415242,0.0192301303887427,0.0272771137891719,
0.0376302766663001,0.0801259453598099,0.103386439221757,0.122405930723958,
0.137206159944638,0.157073182616755,0.201283797023069,0.223466584261481,
0.232832546780453,0.243009558461636,0.286600593259539,0.319563822681232,
0.335294199052886,0.351238688388344,0.387813790697272,0.421429964250173,
0.433991334059334,0.442723428560765,0.457173786303744,0.499600153131827,
0.526857736851706,0.542239034458496,0.558729495818835,0.606205000027797,
0.625114473075408,0.638646897705653,0.647343441333917,0.660607608104126,
0.701332032884221,0.731305251402524,0.746867883638596,0.763022205076203,
0.813861763041297,0.839335603509961,0.848938126424361,0.858852205273181,
0.899417192833346,0.935509224651299,0.951358618903697,0.967186436715782,
1.01669943243797,1.03594198043776,1.04961797458601,1.05831696692786,1.07145231923964,
1.11210924043534,1.1423381118637,1.15792046651988,1.17405768397425,1.22508146764573,
1.25044280360822,1.26004140506794,1.26996816855601,1.29353464663662),
 .UNSPECIFIED.) ;
#1280 = B_SPLINE_CURVE_WITH_KNOTS('',3,(#51603,#51604,#51605,#51606,#51607,
#51608,#51609,#51610,#51611,#51612,#51613,#51614,#51615,#51616,#51617,#51618,
#51619,#51620,#51621,#51622,#51623,#51624,#51625,#51626,#51627,#51628,#51629,
#51630,#51631,#51632,#51633,#51634,#51635,#51636,#51637,#51638,#51639,#51640,
#51641,#51642,#51643,#51644,#51645,#51646,#51647,#51648,#51649,#51650,#51651,
#51652,#51653,#51654,#51655,#51656,#51657,#51658,#51659,#51660,#51661,#51662,
#51663,#51664,#51665,#51666,#51667,#51668,#51669,#51670,#51671,#51672,#51673,
#51674,#51675,#51676,#51677,#51678,#51679,#51680,#51681,#51682,#51683,#51684,
#51685,#51686,#51687,#51688,#51689,#51690,#51691,#51692,#51693),
 .UNSPECIFIED.,.F.,.F.,(4,3,3,3,3,3,3,3,3,3,3,3,3,3,3,3,3,3,3,3,3,3,3,3,
3,3,3,3,3,3,4),(15.7079632679489,15.8112862145918,15.9145819569287,16.0178859166035,
16.1213082644554,16.2247941267765,16.3223176520483,16.328474632555,16.3947477954893,
16.3947981013556,16.489357726852,16.4989433816516,16.6029287721312,16.7067856596915,
16.8105731365216,16.9143261318643,17.0180795274943,17.1219368421535,17.2258500814329,
17.3242629549208,17.3299421537631,17.3930789381131,17.393126645645,17.4881627074684,
17.4974400050297,17.6010549229789,17.6065527859347,17.7105911054467,17.8145605873424,
17.9185020171076,17.9338911286497),.UNSPECIFIED.) ;
#1281 = B_SPLINE_CURVE_WITH_KNOTS('',3,(#51695,#51696,#51697,#51698,#51699,
#51700,#51701,#51702,#51703,#51704,#51705,#51706,#51707,#51708,#51709,#51710,
#51711,#51712,#51713,#51714,#51715,#51716,#51717,#51718,#51719,#51720,#51721,
#51722,#51723,#51724,#51725,#51726,#51727,#51728,#51729,#51730,#51731,#51732,
#51733,#51734),.UNSPECIFIED.,.F.,.F.,(4,3,3,3,3,3,3,3,3,3,3,3,3,4),(14.3981410127768,
14.504165380809,14.6101056089343,14.716015321525,14.8219136896749,14.9278305855172,
15.0337958927558,15.1399186889816,15.2461301728942,15.3525441995258,15.3964695570662,
15.5190228063118,15.640255155241,15.7079553729118),.UNSPECIFIED.) ;
#1282 = B_SPLINE_CURVE_WITH_KNOTS('',3,(#51738,#51739,#51740,#51741,#51742,
#51743,#51744,#51745,#51746,#51747,#51748,#51749,#51750,#51751,#51752,#51753,
#51754,#51755,#51756,#51757,#51758,#51759,#51760,#51761,#51762,#51763,#51764,
#51765,#51766,#51767,#51768,#51769,#51770,#51771,#51772,#51773,#51774,#51775),
 .UNSPECIFIED.,.F.,.F.,(4,2,2,2,2,2,2,2,2,2,2,2,2,2,2,2,2,2,4),(0.000123888491208429,
0.00530097158793175,0.0119135358149671,0.0413087913729525,0.0805378612701992,
0.0975159189419682,0.112586285557099,0.137553323954031,0.175117088689359,
0.188972222625648,0.200071653519827,0.209056561170478,0.22687817831067,
0.25814390936283,0.289431712038232,0.305242605840278,0.321088767321622,
0.358043788409661,0.377582389026477),.UNSPECIFIED.) ;
#1283 = B_SPLINE_CURVE_WITH_KNOTS('',3,(#51776,#51777,#51778,#51779,#51780,
#51781,#51782,#51783,#51784,#51785,#51786,#51787,#51788,#51789,#51790,#51791,
#51792,#51793,#51794,#51795,#51796,#51797,#51798,#51799,#51800,#51801,#51802,
#51803,#51804,#51805,#51806,#51807,#51808,#51809,#51810,#51811,#51812,#51813,
#51814,#51815,#51816,#51817,#51818,#51819,#51820,#51821),.UNSPECIFIED.,
 .F.,.F.,(4,2,2,2,2,2,2,2,2,2,2,2,2,2,2,2,2,2,2,2,2,2,4),(9.62132622118833E-5,
0.0151686805222011,0.0250764405871821,0.0338681801368411,0.0468910424127618,
0.090942954515606,0.119087295147558,0.134543854258273,0.150904946987846,
0.199684592076087,0.218150734757442,0.231497901566788,0.240231336528935,
0.253830368051126,0.294788211242235,0.324295440911908,0.339901492363877,
0.356248065950247,0.405673464097533,0.423906443126347,0.437155718637114,
0.445919717201807,0.458255991027476),.UNSPECIFIED.) ;
#1284 = B_SPLINE_CURVE_WITH_KNOTS('',3,(#51827,#51828,#51829,#51830,#51831,
#51832,#51833,#51834,#51835,#51836,#51837,#51838,#51839,#51840,#51841,#51842,
#51843,#51844,#51845,#51846,#51847,#51848,#51849,#51850,#51851,#51852),
 .UNSPECIFIED.,.F.,.F.,(4,2,2,2,2,2,2,2,2,2,2,2,4),(0.459096610162116,0.464484342986074,
0.505668080579649,0.520933833493707,0.529915992349492,0.54243499630205,
0.575250236487497,0.614798671012523,0.632654644680522,0.649413835000852,
0.667105487768125,0.722540336011944,0.73248042541764),.UNSPECIFIED.) ;
#1285 = B_SPLINE_CURVE_WITH_KNOTS('',3,(#51855,#51856,#51857,#51858,#51859,
#51860,#51861,#51862,#51863,#51864,#51865,#51866,#51867,#51868,#51869,#51870,
#51871,#51872,#51873,#51874,#51875,#51876,#51877,#51878,#51879,#51880,#51881,
#51882,#51883,#51884,#51885,#51886,#51887,#51888,#51889,#51890),
 .UNSPECIFIED.,.F.,.F.,(4,2,2,2,2,2,2,2,2,2,2,2,2,2,2,2,2,4),(0.000330659804311743,
0.00532268279890478,0.0119652393155716,0.0489137712862508,0.0844466789380679,
0.100390177495993,0.116304718668483,0.149639300369354,0.178299187759877,
0.190741385079452,0.201082178857332,0.210410580183121,0.232117158451284,
0.282288937876845,0.300234024157747,0.315213791978961,0.337203182451053,
0.381142147507287),.UNSPECIFIED.) ;
#1286 = B_SPLINE_CURVE_WITH_KNOTS('',3,(#51896,#51897,#51898,#51899,#51900,
#51901,#51902,#51903,#51904,#51905,#51906,#51907,#51908,#51909,#51910,#51911,
#51912,#51913,#51914,#51915,#51916,#51917,#51918,#51919,#51920,#51921,#51922,
#51923,#51924,#51925,#51926,#51927,#51928,#51929,#51930,#51931,#51932,#51933,
#51934,#51935,#51936,#51937,#51938,#51939,#51940,#51941,#51942,#51943,#51944,
#51945,#51946,#51947,#51948,#51949,#51950,#51951,#51952,#51953,#51954,#51955,
#51956,#51957,#51958,#51959,#51960,#51961,#51962,#51963,#51964,#51965,#51966,
#51967,#51968,#51969,#51970,#51971,#51972,#51973),.UNSPECIFIED.,.F.,.F.,
(4,2,2,2,2,2,2,2,2,2,2,2,2,2,2,2,2,2,2,2,2,2,2,2,2,2,2,2,2,2,2,2,2,2,2,
2,2,2,4),(1.29358094859399,1.30102621768796,1.31746349241148,1.33301830687605,
1.36175265660975,1.40289178715733,1.41695745330526,1.42571909490168,1.43874559827101,
1.4564822236342,1.50745376612977,1.52367647047814,1.53938760067812,1.57050924037248,
1.61088197490208,1.62361971586095,1.63240634535552,1.64691310392657,1.66812039125473,
1.71247092468887,1.72876553219963,1.74440242333882,1.77438578117767,1.81523711670643,
1.82858191899148,1.83732061561392,1.8509484004107,1.87005073834989,1.91688275202948,
1.93342514886333,1.94878576328709,1.97562922446084,2.02433805715359,2.035934070784,
2.04486283448474,2.0610646819781,2.08687744711799,2.11459664905666,2.12877604277013),
 .UNSPECIFIED.) ;
#1287 = B_SPLINE_CURVE_WITH_KNOTS('',3,(#51974,#51975,#51976,#51977,#51978,
#51979,#51980,#51981,#51982,#51983,#51984,#51985,#51986,#51987,#51988,#51989,
#51990,#51991,#51992,#51993,#51994,#51995,#51996,#51997,#51998,#51999,#52000,
#52001,#52002,#52003,#52004,#52005,#52006,#52007,#52008,#52009,#52010,#52011,
#52012,#52013,#52014,#52015),.UNSPECIFIED.,.F.,.F.,(4,2,2,2,2,2,2,2,2,2,
2,2,2,2,2,2,2,2,2,2,4),(0.000736727244597652,0.0138630500639099,0.0296047208355221,
0.0797774319646349,0.10660912375222,0.116337527341353,0.12644712976289,
0.164941777871912,0.201310185331325,0.217468062584905,0.233571497463829,
0.267550915715147,0.296211966738743,0.313275697185141,0.322123670998576,
0.332482592175531,0.366416413504128,0.408124252474692,0.424838409521503,
0.439829856362813,0.459096610162116),.UNSPECIFIED.) ;
#1288 = B_SPLINE_CURVE_WITH_KNOTS('',3,(#52016,#52017,#52018,#52019,#52020,
#52021,#52022,#52023,#52024,#52025,#52026,#52027,#52028,#52029,#52030,#52031,
#52032,#52033,#52034,#52035,#52036,#52037,#52038,#52039,#52040,#52041,#52042,
#52043,#52044,#52045,#52046,#52047,#52048,#52049,#52050,#52051,#52052,#52053,
#52054,#52055,#52056,#52057,#52058,#52059,#52060,#52061,#52062,#52063,#52064,
#52065,#52066,#52067,#52068,#52069,#52070,#52071,#52072,#52073,#52074,#52075,
#52076,#52077,#52078,#52079,#52080,#52081,#52082,#52083,#52084,#52085,#52086,
#52087,#52088,#52089,#52090,#52091,#52092,#52093,#52094,#52095,#52096,#52097,
#52098,#52099,#52100,#52101,#52102,#52103,#52104,#52105,#52106,#52107,#52108,
#52109,#52110,#52111,#52112,#52113,#52114,#52115,#52116,#52117,#52118,#52119,
#52120,#52121,#52122,#52123,#52124,#52125,#52126,#52127,#52128,#52129),
 .UNSPECIFIED.,.F.,.F.,(4,2,2,2,2,2,2,2,2,2,2,2,2,2,2,2,2,2,2,2,2,2,2,2,
2,2,2,2,2,2,2,2,2,2,2,2,2,2,2,2,2,2,2,2,2,2,2,2,2,2,2,2,2,2,2,2,4),(9.99999992887031E-7,
0.0186616073847396,0.0265145648287108,0.0364172205219696,0.0768552188462689,
0.101753994768879,0.121515268481445,0.136312633376872,0.155416829288432,
0.199810777329292,0.223169469646049,0.23262884996062,0.242689125040078,
0.281562678656109,0.31632308573852,0.33284556735728,0.348192875678435,0.375112560596473,
0.411072223212628,0.424735680902339,0.435735995351809,0.44475699666495,
0.462801730928076,0.503187277361918,0.523359270112846,0.53945352867169,
0.555087724667914,0.609993057856924,0.63412073326911,0.643643996789702,
0.653668525480734,0.702347086434316,0.731644458141428,0.747167476314061,
0.763395866290607,0.813517561529774,0.839394244676013,0.849020882378051,
0.858913106669476,0.899745295132745,0.935668108620726,0.951516768444482,
0.967356614754378,1.01678695434003,1.036066749431,1.04975998469544,1.05846175303386,
1.07159052398353,1.11224828740261,1.14249992235587,1.15808752367891,1.17422930654474,
1.22525639840622,1.25062473160401,1.26022582485268,1.27015675728782,1.29372477504308),
 .UNSPECIFIED.) ;
#1289 = B_SPLINE_CURVE_WITH_KNOTS('',3,(#52135,#52136,#52137,#52138,#52139,
#52140,#52141,#52142,#52143,#52144,#52145,#52146,#52147,#52148,#52149,#52150,
#52151,#52152,#52153,#52154,#52155,#52156,#52157,#52158,#52159,#52160,#52161,
#52162,#52163,#52164,#52165,#52166,#52167,#52168,#52169,#52170,#52171,#52172,
#52173,#52174,#52175,#52176,#52177,#52178,#52179,#52180,#52181,#52182,#52183,
#52184,#52185,#52186,#52187,#52188,#52189,#52190,#52191,#52192,#52193,#52194,
#52195,#52196,#52197,#52198,#52199,#52200,#52201,#52202,#52203,#52204,#52205,
#52206,#52207,#52208,#52209,#52210,#52211,#52212,#52213,#52214,#52215,#52216,
#52217,#52218,#52219,#52220,#52221,#52222,#52223,#52224,#52225),
 .UNSPECIFIED.,.F.,.F.,(4,3,3,3,3,3,3,3,3,3,3,3,3,3,3,3,3,3,3,3,3,3,3,3,
3,3,3,3,3,3,4),(15.7079632679489,15.8113100481548,15.9146304174514,16.0179597637145,
16.121408506256,16.224921363305,16.3224364904957,16.3286295701974,16.3947467672854,
16.3947981013555,16.4893652458264,16.4989518365239,16.6029457144663,16.7068111290688,
16.8106071575924,16.9143687273476,17.0181307182028,17.1219966306611,17.2259184833068,
17.3243262425669,17.3300191259139,17.3930772951172,17.3931266456449,17.4881595111779,
17.4974436459181,17.6010532040285,17.6065565589844,17.7105979188205,17.8145702361085,
17.918514220579,17.9338952981833),.UNSPECIFIED.) ;
#1290 = B_SPLINE_CURVE_WITH_KNOTS('',3,(#52227,#52228,#52229,#52230,#52231,
#52232,#52233,#52234,#52235,#52236,#52237,#52238,#52239,#52240,#52241,#52242,
#52243,#52244,#52245,#52246,#52247,#52248,#52249,#52250,#52251,#52252,#52253,
#52254,#52255,#52256,#52257,#52258,#52259,#52260,#52261,#52262,#52263,#52264,
#52265,#52266),.UNSPECIFIED.,.F.,.F.,(4,3,3,3,3,3,3,3,3,3,3,3,3,4),(14.3981410127767,
14.504137960918,14.61004971469,14.7159295917658,14.8217973215678,14.9276828478524,
15.0336161250156,15.1397061611793,15.2458844410812,15.3522649548022,15.3964695570661,
15.5190072170087,15.6402338511171,15.7079554096739),.UNSPECIFIED.) ;
#1291 = B_SPLINE_CURVE_WITH_KNOTS('',3,(#52269,#52270,#52271,#52272,#52273,
#52274,#52275,#52276,#52277,#52278,#52279,#52280,#52281,#52282,#52283,#52284,
#52285,#52286,#52287,#52288,#52289,#52290,#52291,#52292,#52293,#52294,#52295,
#52296,#52297,#52298,#52299,#52300,#52301,#52302,#52303,#52304,#52305,#52306,
#52307,#52308,#52309,#52310,#52311,#52312,#52313,#52314,#52315,#52316,#52317,
#52318,#52319,#52320,#52321,#52322,#52323,#52324,#52325,#52326,#52327,#52328,
#52329,#52330,#52331,#52332,#52333,#52334,#52335,#52336,#52337,#52338,#52339,
#52340,#52341,#52342,#52343,#52344),.UNSPECIFIED.,.F.,.F.,(4,2,2,2,2,2,
2,2,2,2,2,2,2,2,2,2,2,2,2,2,2,2,2,2,2,2,2,2,2,2,2,2,2,2,2,2,2,4),(9.03212379660126E-5,
0.00957464539286387,0.063316634352145,0.083467899230563,0.0996371287737807,
0.115333995030373,0.167738796060251,0.192855728715468,0.202445810461218,
0.212412273542816,0.252486125819501,0.277582644409014,0.297467528730337,
0.312346809846427,0.331622833295928,0.375708714755005,0.39859634760076,
0.408047640128789,0.418091316914522,0.430056519706791,0.456400850306449,
0.494030306038328,0.509859880561215,0.525330099484413,0.555914229040669,
0.596369402008556,0.609242891445144,0.617871076698452,0.631503317897237,
0.65068604789205,0.700307170737338,0.716050896621134,0.731757816929863,
0.765959715718328,0.808239304508462,0.818258387720161,0.826154683199369,
0.835771767811734),.UNSPECIFIED.) ;
#1292 = B_SPLINE_CURVE_WITH_KNOTS('',3,(#52351,#52352,#52353,#52354,#52355,
#52356,#52357,#52358,#52359,#52360,#52361,#52362,#52363,#52364,#52365,#52366,
#52367,#52368,#52369,#52370,#52371,#52372,#52373,#52374,#52375,#52376,#52377,
#52378,#52379,#52380,#52381,#52382,#52383,#52384,#52385,#52386,#52387,#52388,
#52389,#52390,#52391,#52392,#52393),.UNSPECIFIED.,.F.,.F.,(4,3,3,3,3,3,
3,3,3,3,3,3,3,3,4),(-17.9381921786934,-17.84255119842,-17.733347647525,
-17.6242554309927,-17.5152330417418,-17.4062390702213,-17.297153285934,
-17.1880265338616,-17.078692513265,-16.9804446462392,-16.9716447107412,
-16.9715852529195,-16.8695603658721,-16.8587108864595,-16.7648968801594),
 .UNSPECIFIED.) ;
#1293 = B_SPLINE_CURVE_WITH_KNOTS('',3,(#52399,#52400,#52401,#52402,#52403,
#52404,#52405,#52406,#52407,#52408,#52409,#52410,#52411,#52412,#52413,#52414,
#52415,#52416,#52417,#52418,#52419,#52420,#52421,#52422,#52423,#52424,#52425,
#52426,#52427,#52428,#52429,#52430,#52431,#52432,#52433,#52434,#52435,#52436,
#52437,#52438,#52439,#52440,#52441,#52442,#52443,#52444,#52445,#52446,#52447,
#52448,#52449,#52450,#52451,#52452,#52453,#52454,#52455,#52456,#52457,#52458,
#52459,#52460,#52461,#52462,#52463,#52464,#52465,#52466,#52467,#52468,#52469,
#52470,#52471,#52472,#52473,#52474,#52475,#52476,#52477,#52478,#52479,#52480,
#52481,#52482,#52483,#52484,#52485,#52486,#52487,#52488,#52489,#52490,#52491,
#52492,#52493,#52494,#52495,#52496,#52497,#52498,#52499,#52500,#52501,#52502,
#52503,#52504,#52505,#52506,#52507,#52508,#52509,#52510,#52511,#52512,#52513,
#52514,#52515,#52516,#52517,#52518,#52519,#52520,#52521,#52522,#52523,#52524,
#52525,#52526,#52527,#52528,#52529,#52530,#52531,#52532,#52533,#52534,#52535,
#52536,#52537,#52538,#52539,#52540,#52541,#52542,#52543,#52544,#52545,#52546,
#52547,#52548,#52549,#52550,#52551,#52552,#52553,#52554,#52555,#52556,#52557,
#52558,#52559,#52560,#52561,#52562,#52563,#52564,#52565,#52566,#52567,#52568,
#52569,#52570,#52571,#52572,#52573,#52574,#52575,#52576,#52577,#52578,#52579,
#52580,#52581,#52582,#52583,#52584,#52585,#52586,#52587,#52588,#52589,#52590,
#52591,#52592,#52593,#52594,#52595,#52596,#52597),.UNSPECIFIED.,.F.,.F.,
(4,3,3,3,3,3,3,3,3,3,3,3,3,3,3,3,3,3,3,3,3,3,3,3,3,3,3,3,3,3,3,3,3,3,3,
3,3,3,3,3,3,3,3,3,3,3,3,3,3,3,3,3,3,3,3,3,3,3,3,3,3,3,3,3,3,3,4),(14.2294985582914,
14.3389460551526,14.4483384046449,14.5577163080432,14.6671996455868,14.7767350734239,
14.8864771704765,14.9748740828937,14.9749281643406,15.0752586873661,15.0846380345985,
15.1957153688525,15.3051222524056,15.414462240541,15.5237761597846,15.6361462969959,
15.7456017222214,15.8594292154257,15.9579697000886,15.9732013864772,15.97325670863,
16.0738005094969,16.0831956290521,16.1942443320355,16.3038817778961,16.4134522833054,
16.5229963245652,16.6351435566538,16.7448256020604,16.8582054274899,16.9568838883179,
16.9715259416915,16.9715852529194,17.0721629157137,17.0813044812162,17.1923806457152,
17.3018057577008,17.4111673178708,17.5205061818026,17.6328580856542,17.7423468637998,
17.8561303305043,17.9543267491162,17.9698505499765,17.9699137972087,18.0695586486444,
18.0792692192989,18.1903908595738,18.299435457365,18.4084113055606,18.5173598834856,
18.6300804979887,18.7391721543765,18.8537072479373,18.9524124448144,18.9682083299824,
18.9682423414981,19.0701276240468,19.0803889423434,19.1922977544505,19.3040678221704,
19.4157344265348,19.5273327084527,19.6389407654977,19.7505444309161,19.8622587312217,
19.9665708857875),.UNSPECIFIED.) ;
#1294 = B_SPLINE_CURVE_WITH_KNOTS('',3,(#52599,#52600,#52601,#52602,#52603,
#52604,#52605,#52606,#52607,#52608,#52609,#52610,#52611,#52612,#52613,#52614,
#52615,#52616,#52617,#52618,#52619,#52620,#52621,#52622,#52623,#52624,#52625,
#52626,#52627,#52628,#52629,#52630,#52631,#52632,#52633,#52634,#52635,#52636,
#52637,#52638,#52639,#52640,#52641,#52642,#52643,#52644,#52645,#52646,#52647,
#52648,#52649,#52650,#52651,#52652,#52653,#52654,#52655,#52656,#52657,#52658,
#52659,#52660,#52661,#52662,#52663,#52664,#52665,#52666,#52667,#52668,#52669,
#52670,#52671,#52672,#52673,#52674,#52675,#52676,#52677,#52678,#52679,#52680,
#52681,#52682,#52683,#52684,#52685,#52686,#52687,#52688,#52689,#52690,#52691,
#52692,#52693,#52694,#52695,#52696,#52697,#52698,#52699,#52700,#52701,#52702),
 .UNSPECIFIED.,.F.,.F.,(4,2,2,2,2,2,2,2,2,2,2,2,2,2,2,2,2,2,2,2,2,2,2,2,
2,2,2,2,2,2,2,2,2,2,2,2,2,2,2,2,2,2,2,2,2,2,2,2,2,2,2,4),(1.10906469945444,
1.11644179379854,1.13767404484332,1.16925937097399,1.18614807304508,1.19521787211305,
1.2079746259431,1.22628467027725,1.26313703689709,1.27862570307869,1.29601903027109,
1.31662312511589,1.35083366981395,1.36044435318284,1.37150334131016,1.40310804188015,
1.4311789832774,1.44633688717477,1.46421088555474,1.4859701109504,1.5186366830229,
1.52796710429679,1.53967142713642,1.55546837692492,1.59652752283311,1.61207491358455,
1.62932310833252,1.64959144102805,1.68487769212845,1.69438184985283,1.70570010383403,
1.72064458309577,1.76585042140126,1.78102778991588,1.7996551503634,1.84829086317497,
1.85912184122804,1.86883008853204,1.88048923002279,1.90864659496912,1.93331757477378,
1.94837534891107,1.96720425580469,2.00360604212628,2.0205483517595,2.02963733862127,
2.04245354220867,2.06087185016348,2.0972058647788,2.11276529158488,2.13033849194594,
2.1591307752799),.UNSPECIFIED.) ;
#1295 = B_SPLINE_CURVE_WITH_KNOTS('',3,(#52708,#52709,#52710,#52711,#52712,
#52713,#52714,#52715,#52716,#52717),.UNSPECIFIED.,.F.,.F.,(4,2,2,2,4),(0.000104814392196666,
0.0139942526189345,0.0233080874743996,0.0329393031166841,0.0589549240516137),
 .UNSPECIFIED.) ;
#1296 = B_SPLINE_CURVE_WITH_KNOTS('',3,(#52719,#52720,#52721,#52722,#52723,
#52724,#52725,#52726,#52727,#52728,#52729,#52730,#52731,#52732,#52733,#52734,
#52735,#52736,#52737,#52738,#52739,#52740,#52741,#52742,#52743,#52744,#52745,
#52746,#52747,#52748,#52749,#52750,#52751,#52752,#52753,#52754,#52755,#52756,
#52757,#52758,#52759,#52760,#52761,#52762,#52763,#52764,#52765,#52766,#52767,
#52768,#52769,#52770,#52771,#52772,#52773,#52774,#52775,#52776,#52777,#52778,
#52779,#52780,#52781,#52782,#52783,#52784,#52785,#52786,#52787,#52788,#52789,
#52790,#52791,#52792,#52793,#52794,#52795,#52796,#52797,#52798,#52799,#52800,
#52801,#52802,#52803,#52804,#52805,#52806,#52807,#52808,#52809,#52810,#52811,
#52812,#52813,#52814,#52815,#52816,#52817,#52818,#52819,#52820,#52821,#52822,
#52823,#52824,#52825,#52826,#52827,#52828,#52829,#52830,#52831,#52832,#52833,
#52834,#52835,#52836,#52837,#52838,#52839,#52840,#52841,#52842,#52843,#52844,
#52845,#52846,#52847,#52848),.UNSPECIFIED.,.F.,.F.,(4,3,3,3,3,3,3,3,3,3,
3,3,3,3,3,3,3,3,3,3,3,3,3,3,3,3,3,3,3,3,3,3,3,3,3,3,3,3,3,3,3,3,3,4),(-3.84638257448865,
-3.73820981375279,-3.63015427375729,-3.52217346020946,-3.41422462150895,
-3.30618883650797,-3.19811283732308,-3.0898366058282,-2.99504494316089,
-2.99498563286816,-2.89440797106735,-2.88526640865405,-2.77419024364464,
-2.66476513576646,-2.55540357970902,-2.44606471989407,-2.33371281206525,
-2.22422403802765,-2.11044056330321,-2.01224414737772,-1.996720335184,-1.99665708857877,
-1.89701223877746,-1.887301676346,-1.77618003483892,-1.66713544615312,-1.55815960676097,
-1.44921103732509,-1.33649041406617,-1.22739876529517,-1.11286365479228,
-1.01415847169605,-0.998362556174536,-0.998328544289387,-0.896443265106951,
-0.886181926854384,-0.774273098472086,-0.662503014698027,-0.550836394538628,
-0.439238097123404,-0.327630025180105,-0.216026345188961,-0.10431203103316,
-1.15547111670624E-13),.UNSPECIFIED.) ;
#1297 = B_SPLINE_CURVE_WITH_KNOTS('',3,(#52852,#52853,#52854,#52855,#52856,
#52857,#52858,#52859,#52860,#52861,#52862,#52863,#52864,#52865,#52866,#52867,
#52868,#52869,#52870,#52871,#52872,#52873,#52874,#52875,#52876,#52877,#52878,
#52879,#52880,#52881,#52882,#52883,#52884,#52885,#52886,#52887,#52888,#52889,
#52890,#52891,#52892,#52893,#52894,#52895,#52896,#52897,#52898,#52899,#52900,
#52901,#52902,#52903,#52904,#52905,#52906,#52907,#52908,#52909,#52910,#52911,
#52912,#52913,#52914,#52915,#52916,#52917,#52918,#52919,#52920,#52921,#52922,
#52923,#52924,#52925,#52926,#52927,#52928,#52929,#52930,#52931,#52932,#52933,
#52934,#52935,#52936,#52937,#52938,#52939,#52940,#52941,#52942,#52943,#52944,
#52945,#52946,#52947,#52948,#52949,#52950,#52951,#52952,#52953,#52954,#52955,
#52956,#52957,#52958,#52959,#52960,#52961,#52962,#52963,#52964,#52965,#52966,
#52967,#52968,#52969,#52970,#52971,#52972,#52973,#52974,#52975,#52976,#52977,
#52978,#52979,#52980,#52981,#52982,#52983,#52984,#52985,#52986,#52987,#52988,
#52989,#52990,#52991,#52992,#52993,#52994,#52995,#52996,#52997,#52998,#52999,
#53000,#53001,#53002,#53003,#53004,#53005,#53006,#53007,#53008,#53009,#53010,
#53011,#53012,#53013,#53014,#53015,#53016,#53017,#53018,#53019,#53020,#53021,
#53022,#53023,#53024,#53025,#53026,#53027,#53028,#53029,#53030,#53031,#53032,
#53033,#53034,#53035,#53036,#53037,#53038,#53039,#53040,#53041,#53042,#53043,
#53044,#53045,#53046,#53047,#53048,#53049,#53050),.UNSPECIFIED.,.F.,.F.,
(4,3,3,3,3,3,3,3,3,3,3,3,3,3,3,3,3,3,3,3,3,3,3,3,3,3,3,3,3,3,3,3,3,3,3,
3,3,3,3,3,3,3,3,3,3,3,3,3,3,3,3,3,3,3,3,3,3,3,3,3,3,3,3,3,3,3,4),(2.02837884434118,
2.1240196911459,2.23322324616186,2.34231546682411,2.45133786021298,2.56033183587889,
2.66941762430942,2.77854438053048,2.88787840524992,2.98612627157822,2.99492617411531,
2.99498563286811,3.095559170198,3.10492126614826,3.21597038002441,3.32560646520527,
3.43517633163416,3.54472045447418,3.65686888514501,3.76655278708082,3.87993348211915,
3.9785834862159,3.99325866988823,3.99331417715749,4.0937196533305,4.10302861870553,
4.2141053815482,4.32351415904549,4.43285503962457,4.54216885140771,4.6545373189175,
4.76399016764901,4.87781644454794,4.97628313139962,4.99158865070613,4.99164272144687,
5.09203035032617,5.10141775971842,5.21248694797065,5.32195859236235,5.43136300708735,
5.54074091187526,5.6530485003405,5.7625660676359,5.87626866668607,5.97482553317191,
5.98991776896683,5.98997126573624,6.09040645084578,6.09976781763968,6.21083431668792,
6.32032871950448,6.42975630058055,6.53915774670571,6.65144326253569,6.76098505495927,
6.87464243249244,6.97319341710015,6.98824593552854,6.98829981002562,7.08940621512439,
7.09951479840276,7.21054371655544,7.32140209163783,7.43216080950087,7.54286222160147,
7.59300756235177),.UNSPECIFIED.) ;
#1298 = B_SPLINE_CURVE_WITH_KNOTS('',3,(#53051,#53052,#53053,#53054,#53055,
#53056,#53057,#53058),.UNSPECIFIED.,.F.,.F.,(4,2,2,4),(-1.10892786928915,
-1.08701579877003,-1.05545668530014,-1.05009726896819),.UNSPECIFIED.) ;
#1299 = B_SPLINE_CURVE_WITH_KNOTS('',3,(#53065,#53066,#53067,#53068,#53069,
#53070,#53071,#53072,#53073,#53074,#53075,#53076,#53077,#53078,#53079,#53080,
#53081,#53082,#53083,#53084,#53085,#53086,#53087,#53088,#53089,#53090,#53091,
#53092,#53093,#53094,#53095,#53096,#53097,#53098,#53099,#53100,#53101,#53102,
#53103,#53104,#53105,#53106,#53107),.UNSPECIFIED.,.F.,.F.,(4,3,3,3,3,3,
3,3,3,3,3,3,3,3,4),(-17.9382970979382,-17.8425540308235,-17.7333535479141,
-17.6242644024251,-17.5152450868105,-17.4062541910623,-17.2971714758685,
-17.1880477943208,-17.0787168207789,-16.9804683437631,-16.9716440068398,
-16.9715852529196,-16.8695599004832,-16.8587139242793,-16.7649015929075),
 .UNSPECIFIED.) ;
#1300 = B_SPLINE_CURVE_WITH_KNOTS('',3,(#53113,#53114,#53115,#53116,#53117,
#53118,#53119,#53120,#53121,#53122,#53123,#53124,#53125,#53126,#53127,#53128,
#53129,#53130,#53131,#53132,#53133,#53134,#53135,#53136,#53137,#53138,#53139,
#53140,#53141,#53142,#53143,#53144,#53145,#53146,#53147,#53148,#53149,#53150,
#53151,#53152,#53153,#53154,#53155,#53156,#53157,#53158,#53159,#53160,#53161,
#53162,#53163,#53164,#53165,#53166,#53167,#53168,#53169,#53170,#53171,#53172,
#53173,#53174,#53175,#53176,#53177,#53178,#53179,#53180,#53181,#53182,#53183,
#53184,#53185,#53186,#53187,#53188,#53189,#53190,#53191,#53192,#53193,#53194,
#53195,#53196,#53197,#53198,#53199,#53200,#53201,#53202,#53203,#53204,#53205,
#53206,#53207,#53208,#53209,#53210,#53211,#53212,#53213,#53214,#53215,#53216,
#53217,#53218,#53219,#53220,#53221,#53222,#53223,#53224,#53225,#53226,#53227,
#53228,#53229,#53230,#53231,#53232,#53233,#53234,#53235,#53236,#53237,#53238,
#53239,#53240,#53241,#53242,#53243,#53244,#53245,#53246,#53247,#53248,#53249,
#53250,#53251,#53252,#53253,#53254,#53255,#53256,#53257,#53258,#53259,#53260,
#53261,#53262,#53263,#53264,#53265,#53266,#53267,#53268,#53269,#53270,#53271,
#53272,#53273,#53274,#53275,#53276,#53277,#53278,#53279,#53280,#53281,#53282,
#53283,#53284,#53285,#53286,#53287,#53288,#53289,#53290,#53291,#53292,#53293,
#53294,#53295,#53296,#53297,#53298,#53299,#53300,#53301,#53302,#53303,#53304,
#53305,#53306,#53307,#53308,#53309,#53310,#53311),.UNSPECIFIED.,.F.,.F.,
(4,3,3,3,3,3,3,3,3,3,3,3,3,3,3,3,3,3,3,3,3,3,3,3,3,3,3,3,3,3,3,3,3,3,3,
3,3,3,3,3,3,3,3,3,3,3,3,3,3,3,3,3,3,3,3,3,3,3,3,3,3,3,3,3,3,3,4),(14.2295041962807,
14.3389527740686,14.4483462151971,14.5577252201524,14.6672096681762,14.7767462138682,
14.8864894271704,14.9748742139681,14.9749281643407,15.0752586275347,15.084638833907,
15.1957160682474,15.3051236621828,15.4144643261432,15.5237788860543,15.6361483416983,
15.7456043152617,15.8594305119459,15.9579714051649,15.973201766293,15.9732567086301,
16.0737983632465,16.0831953062282,16.1942440495646,16.303880929867,16.4134507779162,
16.5229940690511,16.6351418650182,16.744822928944,16.8582040909317,16.9568843065312,
16.9715266399014,16.9715852529195,17.07216214021,17.081301466679,17.1923780079952,
17.3018000786669,17.411158590375,17.5204943992678,17.6328492487531,17.7423349694877,
17.8561243833483,17.9543186908075,17.9698510293629,17.9699137972089,18.0695572552717,
18.0792613911935,18.1903840099816,18.2994213549179,18.4083901820114,18.5173319801007,
18.6300595704501,18.7391451195388,18.8536937305186,18.9523880995745,18.9682080461121,
18.9682423414983,19.0701250867853,19.080401850269,19.1923233312894,19.3041058992852,
19.415784805444,19.5273951605258,19.6390148289136,19.7506298546352,19.8623549565011,
19.9665708857876),.UNSPECIFIED.) ;
#1301 = B_SPLINE_CURVE_WITH_KNOTS('',3,(#53313,#53314,#53315,#53316,#53317,
#53318,#53319,#53320,#53321,#53322,#53323,#53324,#53325,#53326,#53327,#53328,
#53329,#53330,#53331,#53332,#53333,#53334,#53335,#53336,#53337,#53338,#53339,
#53340,#53341,#53342,#53343,#53344,#53345,#53346,#53347,#53348,#53349,#53350,
#53351,#53352,#53353,#53354,#53355,#53356,#53357,#53358,#53359,#53360,#53361,
#53362,#53363,#53364,#53365,#53366,#53367,#53368,#53369,#53370,#53371,#53372,
#53373,#53374,#53375,#53376,#53377,#53378,#53379,#53380,#53381,#53382,#53383,
#53384,#53385,#53386,#53387,#53388,#53389,#53390,#53391,#53392,#53393,#53394,
#53395,#53396,#53397,#53398,#53399,#53400,#53401,#53402,#53403,#53404,#53405,
#53406,#53407,#53408,#53409,#53410,#53411,#53412,#53413,#53414,#53415,#53416),
 .UNSPECIFIED.,.F.,.F.,(4,2,2,2,2,2,2,2,2,2,2,2,2,2,2,2,2,2,2,2,2,2,2,2,
2,2,2,2,2,2,2,2,2,2,2,2,2,2,2,2,2,2,2,2,2,2,2,2,2,2,2,4),(1.10921089576887,
1.1165407497641,1.1377191197715,1.16909543804062,1.18618906391538,1.19528608214462,
1.20790932058952,1.22587909147871,1.26360125462676,1.2790532194091,1.29656844924673,
1.31745268685726,1.35276232031494,1.36183513301177,1.37401990875906,1.39092675320549,
1.43145123251076,1.44661521359877,1.46448147982816,1.48621574539827,1.5189855364488,
1.52831265082856,1.54003542102944,1.5558706418114,1.59684321214082,1.61240079929573,
1.62963855734371,1.64987657864815,1.68530409836741,1.69479824642061,1.70614484450102,
1.72114792974254,1.76623728942954,1.78142302429321,1.80004020942435,1.84859367092729,
1.85948803106446,1.86915885371709,1.88073863170467,1.9083848327913,1.93384705100083,
1.94890686995806,1.9677744135678,2.00274590059768,2.02036028629064,2.02949399608927,
2.04158020440638,2.05821101212464,2.09925252968438,2.11460315827409,2.13296303919467,
2.15968734072935),.UNSPECIFIED.) ;
#1302 = B_SPLINE_CURVE_WITH_KNOTS('',3,(#53422,#53423,#53424,#53425,#53426,
#53427,#53428,#53429,#53430,#53431),.UNSPECIFIED.,.F.,.F.,(4,2,2,2,4),(0.000104517902925009,
0.0138899081821579,0.0231300525877348,0.0326747507448214,0.0589272293900401),
 .UNSPECIFIED.) ;
#1303 = B_SPLINE_CURVE_WITH_KNOTS('',3,(#53433,#53434,#53435,#53436,#53437,
#53438,#53439,#53440,#53441,#53442,#53443,#53444,#53445,#53446,#53447,#53448,
#53449,#53450,#53451,#53452,#53453,#53454,#53455,#53456,#53457,#53458,#53459,
#53460,#53461,#53462,#53463,#53464,#53465,#53466,#53467,#53468,#53469,#53470,
#53471,#53472,#53473,#53474,#53475,#53476,#53477,#53478,#53479,#53480,#53481,
#53482,#53483,#53484,#53485,#53486,#53487,#53488,#53489,#53490,#53491,#53492,
#53493,#53494,#53495,#53496,#53497,#53498,#53499,#53500,#53501,#53502,#53503,
#53504,#53505,#53506,#53507,#53508,#53509,#53510,#53511,#53512,#53513,#53514,
#53515,#53516,#53517,#53518,#53519,#53520,#53521,#53522,#53523,#53524,#53525,
#53526,#53527,#53528,#53529,#53530,#53531,#53532,#53533,#53534,#53535,#53536,
#53537,#53538,#53539,#53540,#53541,#53542,#53543,#53544,#53545,#53546,#53547,
#53548,#53549,#53550,#53551,#53552,#53553,#53554,#53555,#53556,#53557,#53558,
#53559,#53560,#53561,#53562),.UNSPECIFIED.,.F.,.F.,(4,3,3,3,3,3,3,3,3,3,
3,3,3,3,3,3,3,3,3,3,3,3,3,3,3,3,3,3,3,3,3,3,3,3,3,3,3,3,3,3,3,3,3,4),(-3.84638258138888,
-3.73821081936309,-3.63015636590979,-3.52217672366053,-3.41422914122735,
-3.30619474264527,-3.19812020357506,-3.08984554459139,-2.99504424490879,
-2.99498563286818,-2.89440874631802,-2.88526942317335,-2.77419288134903,
-2.6647708147905,-2.55541230721001,-2.44607650245855,-2.33372164898861,
-2.22423593241171,-2.11044651049525,-2.01225220580641,-1.9967198557535,
-1.99665708857879,-1.89701363271621,-1.88730950597383,-1.77618688576327,
-1.66714955140073,-1.55818073455541,-1.44923894637485,-1.33651134585349,
-1.22742580572388,-1.11287717500664,-1.01418282151687,-0.998362840074688,
-0.998328544289396,-0.896445802515984,-0.886169017124272,-0.774247518042122,
-0.662464932220208,-0.550786008513675,-0.439175636205823,-0.327555951244137,
-0.215940909303158,-0.104215792009426,-1.01437695921273E-13),
 .UNSPECIFIED.) ;
#1304 = B_SPLINE_CURVE_WITH_KNOTS('',3,(#53566,#53567,#53568,#53569,#53570,
#53571,#53572,#53573,#53574,#53575,#53576,#53577,#53578,#53579,#53580,#53581,
#53582,#53583,#53584,#53585,#53586,#53587,#53588,#53589,#53590,#53591,#53592,
#53593,#53594,#53595,#53596,#53597,#53598,#53599,#53600,#53601,#53602,#53603,
#53604,#53605,#53606,#53607,#53608,#53609,#53610,#53611,#53612,#53613,#53614,
#53615,#53616,#53617,#53618,#53619,#53620,#53621,#53622,#53623,#53624,#53625,
#53626,#53627,#53628,#53629,#53630,#53631,#53632,#53633,#53634,#53635,#53636,
#53637,#53638,#53639,#53640,#53641,#53642,#53643,#53644,#53645,#53646,#53647,
#53648,#53649,#53650,#53651,#53652,#53653,#53654,#53655,#53656,#53657,#53658,
#53659,#53660,#53661,#53662,#53663,#53664,#53665,#53666,#53667,#53668,#53669,
#53670,#53671,#53672,#53673,#53674,#53675,#53676,#53677,#53678,#53679,#53680,
#53681,#53682,#53683,#53684,#53685,#53686,#53687,#53688,#53689,#53690,#53691,
#53692,#53693,#53694,#53695,#53696,#53697,#53698,#53699,#53700,#53701,#53702,
#53703,#53704,#53705,#53706,#53707,#53708,#53709,#53710,#53711,#53712,#53713,
#53714,#53715,#53716,#53717,#53718,#53719,#53720,#53721,#53722,#53723,#53724,
#53725,#53726,#53727,#53728,#53729,#53730,#53731,#53732,#53733,#53734,#53735,
#53736,#53737,#53738,#53739,#53740,#53741,#53742,#53743,#53744,#53745,#53746,
#53747,#53748,#53749,#53750,#53751,#53752,#53753,#53754,#53755,#53756,#53757,
#53758,#53759,#53760,#53761,#53762,#53763,#53764),.UNSPECIFIED.,.F.,.F.,
(4,3,3,3,3,3,3,3,3,3,3,3,3,3,3,3,3,3,3,3,3,3,3,3,3,3,3,3,3,3,3,3,3,3,3,
3,3,3,3,3,3,3,3,3,3,3,3,3,3,3,3,3,3,3,3,3,3,3,3,3,3,3,3,3,3,3,4),(2.02827393470618,
2.12401685884403,2.2332173459281,2.34230649559061,2.45132581537725,2.5603167152955,
2.66939943464312,2.77852312034262,2.88785409799839,2.98610257413192,2.99492687797345,
2.99498563286815,3.09556048440326,3.10492009829771,3.21596935815519,3.32560452798313,
3.43517357277873,3.54471696644991,3.65686626912681,3.76654966682786,3.87993192199269,
3.97857994078247,3.9932590621024,3.99331417715753,4.09372001119541,4.10302908632675,
4.21410579071677,4.32351514116986,4.43285663280961,4.54217109304234,4.65453900014349,
4.76399258414707,4.877817652797,4.97628416232411,4.99158878638053,4.99164272144692,
5.09203073599517,5.10141887365017,5.21248792266094,5.32196067405111,5.43136619139733,
5.54074519366075,5.65305171167964,5.76257035608005,5.87627081090818,5.97482854624451,
5.98991786319383,5.9899712657363,6.0904065550125,6.09976804010903,6.21083451134862,
6.32032909358392,6.4297568381361,6.53915843204149,6.65144377653754,6.76098567858234,
6.87464274430401,6.97319398049008,6.9882460799675,6.98829981002569,7.08940605201705,
7.09951457708467,7.2105432634816,7.32140139284322,7.43215985716547,7.54286100567203,
7.59300756235177),.UNSPECIFIED.) ;
#1305 = B_SPLINE_CURVE_WITH_KNOTS('',3,(#53765,#53766,#53767,#53768,#53769,
#53770,#53771,#53772),.UNSPECIFIED.,.F.,.F.,(4,2,2,4),(-1.10892889037454,
-1.08702947025092,-1.0554688082652,-1.05009743737373),.UNSPECIFIED.) ;
#1306 = B_SPLINE_CURVE_WITH_KNOTS('',3,(#53779,#53780,#53781,#53782,#53783,
#53784,#53785,#53786,#53787,#53788,#53789,#53790,#53791,#53792,#53793,#53794,
#53795,#53796,#53797,#53798,#53799,#53800,#53801,#53802,#53803,#53804,#53805,
#53806,#53807,#53808,#53809,#53810,#53811,#53812,#53813,#53814,#53815,#53816,
#53817,#53818,#53819,#53820,#53821),.UNSPECIFIED.,.F.,.F.,(4,3,3,3,3,3,
3,3,3,3,3,3,3,3,4),(-17.9379151410847,-17.8425432679218,-17.7333309013929,
-17.6242298257075,-17.5151985361325,-17.4061956253956,-17.29710087273,-17.1879651215466,
-17.0786221284184,-16.9803757539028,-16.9716466477506,-16.9715852529197,
-16.8695608598858,-16.8587017272605,-16.7648831157624),.UNSPECIFIED.) ;
#1307 = B_SPLINE_CURVE_WITH_KNOTS('',3,(#53827,#53828,#53829,#53830,#53831,
#53832,#53833,#53834,#53835,#53836,#53837,#53838,#53839,#53840,#53841,#53842,
#53843,#53844,#53845,#53846,#53847,#53848,#53849,#53850,#53851,#53852,#53853,
#53854,#53855,#53856,#53857,#53858,#53859,#53860,#53861,#53862,#53863,#53864,
#53865,#53866,#53867,#53868,#53869,#53870,#53871,#53872,#53873,#53874,#53875,
#53876,#53877,#53878,#53879,#53880,#53881,#53882,#53883,#53884,#53885,#53886,
#53887,#53888,#53889,#53890,#53891,#53892,#53893,#53894,#53895,#53896,#53897,
#53898,#53899,#53900,#53901,#53902,#53903,#53904,#53905,#53906,#53907,#53908,
#53909,#53910,#53911,#53912,#53913,#53914,#53915,#53916,#53917,#53918,#53919,
#53920,#53921,#53922,#53923,#53924,#53925,#53926,#53927,#53928,#53929,#53930,
#53931,#53932,#53933,#53934,#53935,#53936,#53937,#53938,#53939,#53940,#53941,
#53942,#53943,#53944,#53945,#53946,#53947,#53948,#53949,#53950,#53951,#53952,
#53953,#53954,#53955,#53956,#53957,#53958,#53959,#53960,#53961,#53962,#53963,
#53964,#53965,#53966,#53967,#53968,#53969,#53970,#53971,#53972,#53973,#53974,
#53975,#53976,#53977,#53978,#53979,#53980,#53981,#53982,#53983,#53984,#53985,
#53986,#53987,#53988,#53989,#53990,#53991,#53992,#53993,#53994,#53995,#53996,
#53997,#53998,#53999,#54000,#54001,#54002,#54003,#54004,#54005,#54006,#54007,
#54008,#54009,#54010,#54011,#54012,#54013,#54014,#54015,#54016,#54017,#54018,
#54019,#54020,#54021,#54022,#54023,#54024,#54025),.UNSPECIFIED.,.F.,.F.,
(4,3,3,3,3,3,3,3,3,3,3,3,3,3,3,3,3,3,3,3,3,3,3,3,3,3,3,3,3,3,3,3,3,3,3,
3,3,3,3,3,3,3,3,3,3,3,3,3,3,3,3,3,3,3,3,3,3,3,3,3,3,3,3,3,3,3,4),(14.2294810629657,
14.3389251840774,14.4483141319448,14.5576886102697,14.6671685063617,14.77670047614,
14.8864391301828,14.9748737855452,14.9749281643408,15.075258940077,15.0846355867601,
15.1957132269939,15.3051179526876,15.414455895575,15.523767884172,15.6361400902866,
15.745593885446,15.8594252970381,15.9579642345869,15.9732003327611,15.9732567086302,
16.0738069045067,16.0831975064353,16.1942459747458,16.3038859647742,16.413459264328,
16.523006351189,16.6351510766217,16.7448367857224,16.858211019321,16.9568853997338,
16.9715240189252,16.9715852529196,17.0721654154571,17.0813133909945,17.1923884417713,
17.3018224587493,17.4111929125193,17.520540656044,17.6328839413352,17.742381519234,
17.8561476582214,17.9543503381828,17.9698492848388,17.9699137972089,18.0695607358278,
18.0792872295431,18.1904066185375,18.2994677125777,18.408459452567,18.5174232958139,
18.630128057235,18.7392332550938,18.853737798296,18.9524694433536,18.9682090697805,
18.9682423414983,19.0701346353313,19.0803569178244,19.1922343498211,19.3039734858659,
19.4156096794738,19.5271781448262,19.6387575696301,19.7503332460084,19.8620209741044,
19.9665708857877),.UNSPECIFIED.) ;
#1308 = B_SPLINE_CURVE_WITH_KNOTS('',3,(#54027,#54028,#54029,#54030,#54031,
#54032,#54033,#54034,#54035,#54036,#54037,#54038,#54039,#54040,#54041,#54042,
#54043,#54044,#54045,#54046,#54047,#54048,#54049,#54050,#54051,#54052,#54053,
#54054,#54055,#54056,#54057,#54058,#54059,#54060,#54061,#54062,#54063,#54064,
#54065,#54066,#54067,#54068,#54069,#54070,#54071,#54072,#54073,#54074,#54075,
#54076,#54077,#54078,#54079,#54080,#54081,#54082,#54083,#54084,#54085,#54086,
#54087,#54088,#54089,#54090,#54091,#54092,#54093,#54094,#54095,#54096,#54097,
#54098,#54099,#54100,#54101,#54102,#54103,#54104,#54105,#54106,#54107,#54108,
#54109,#54110,#54111,#54112,#54113,#54114,#54115,#54116,#54117,#54118,#54119,
#54120,#54121,#54122,#54123,#54124,#54125,#54126,#54127,#54128,#54129,#54130),
 .UNSPECIFIED.,.F.,.F.,(4,2,2,2,2,2,2,2,2,2,2,2,2,2,2,2,2,2,2,2,2,2,2,2,
2,2,2,2,2,2,2,2,2,2,2,2,2,2,2,2,2,2,2,2,2,2,2,2,2,2,2,4),(1.10923317368641,
1.11666256443331,1.13796698671944,1.16979398628159,1.18648633306866,1.1955363052136,
1.20845641506686,1.2271779298195,1.26308344394781,1.27862643423749,1.29591470288027,
1.31626339855425,1.35135219608917,1.36087907748399,1.37211876799907,1.40422601455767,
1.43154479013796,1.44684981283533,1.46488734764193,1.48703666194828,1.51867416145164,
1.52807467181166,1.53961320413495,1.55503553052287,1.59723041441357,1.61272025648597,
1.63014776357057,1.65082730757719,1.68477650100827,1.69442112195966,1.70548341908458,
1.73711202265563,1.76510278197234,1.78025690052183,1.79814050897969,1.81991228390051,
1.85264425634999,1.86196800051899,1.87362972720979,1.88934043318008,1.93049967303983,
1.94596068848039,1.9630644315494,1.98305552649924,2.01952385790263,2.02892042589877,
2.04057198294345,2.05620240023131,2.09741648348771,2.11299416773319,2.13056123103445,
2.15945093591691),.UNSPECIFIED.) ;
#1309 = B_SPLINE_CURVE_WITH_KNOTS('',3,(#54136,#54137,#54138,#54139,#54140,
#54141,#54142,#54143,#54144,#54145),.UNSPECIFIED.,.F.,.F.,(4,2,2,2,4),(0.000105573133753892,
0.0138955038549731,0.0231490164641212,0.0327225726684864,0.0589305428466179),
 .UNSPECIFIED.) ;
#1310 = B_SPLINE_CURVE_WITH_KNOTS('',3,(#54147,#54148,#54149,#54150,#54151,
#54152,#54153,#54154,#54155,#54156,#54157,#54158,#54159,#54160,#54161,#54162,
#54163,#54164,#54165,#54166,#54167,#54168,#54169,#54170,#54171,#54172,#54173,
#54174,#54175,#54176,#54177,#54178,#54179,#54180,#54181,#54182,#54183,#54184,
#54185,#54186,#54187,#54188,#54189,#54190,#54191,#54192,#54193,#54194,#54195,
#54196,#54197,#54198,#54199,#54200,#54201,#54202,#54203,#54204,#54205,#54206,
#54207,#54208,#54209,#54210,#54211,#54212,#54213,#54214,#54215,#54216,#54217,
#54218,#54219,#54220,#54221,#54222,#54223,#54224,#54225,#54226,#54227,#54228,
#54229,#54230,#54231,#54232,#54233,#54234,#54235,#54236,#54237,#54238,#54239,
#54240,#54241,#54242,#54243,#54244,#54245,#54246,#54247,#54248,#54249,#54250,
#54251,#54252,#54253,#54254,#54255,#54256,#54257,#54258,#54259,#54260,#54261,
#54262,#54263,#54264,#54265,#54266,#54267,#54268,#54269,#54270,#54271,#54272,
#54273,#54274,#54275,#54276),.UNSPECIFIED.,.F.,.F.,(4,3,3,3,3,3,3,3,3,3,
3,3,3,3,3,3,3,3,3,3,3,3,3,3,3,3,3,3,3,3,3,3,3,3,3,3,3,3,3,3,3,3,3,4),(-3.84638255852685,
-3.73820615619476,-3.63014673992374,-3.5221618213571,-3.41420864885417,
-3.30616818381397,-3.19808730684748,-3.08980590461576,-2.99504686603603,
-2.99498563286819,-2.8944054715389,-2.88525749870731,-2.77418244744124,
-2.66474843435285,-2.55537798445871,-2.44603024479486,-2.33368695574084,
-2.22418938164505,-2.11042323511192,-2.01222055801228,-1.99672160042913,
-1.99665708857879,-1.89701015027871,-1.88728366291615,-1.7761642730878,
-1.66710318509831,-1.55811145091343,-1.4491476132164,-1.33644284598465,
-1.22733765298158,-1.11283309863549,-1.01410146365423,-0.998361816309247,
-0.998328544289396,-0.89643625326683,-0.886213955367558,-0.774336511044062,
-0.662597362857677,-0.550961157321703,-0.439392680283066,-0.327813244270253,
-0.21623755694208,-0.104549818462726,-8.74178244858098E-13),
 .UNSPECIFIED.) ;
#1311 = B_SPLINE_CURVE_WITH_KNOTS('',3,(#54280,#54281,#54282,#54283,#54284,
#54285,#54286,#54287,#54288,#54289,#54290,#54291,#54292,#54293,#54294,#54295,
#54296,#54297,#54298,#54299,#54300,#54301,#54302,#54303,#54304,#54305,#54306,
#54307,#54308,#54309,#54310,#54311,#54312,#54313,#54314,#54315,#54316,#54317,
#54318,#54319,#54320,#54321,#54322,#54323,#54324,#54325,#54326,#54327,#54328,
#54329,#54330,#54331,#54332,#54333,#54334,#54335,#54336,#54337,#54338,#54339,
#54340,#54341,#54342,#54343,#54344,#54345,#54346,#54347,#54348,#54349,#54350,
#54351,#54352,#54353,#54354,#54355,#54356,#54357,#54358,#54359,#54360,#54361,
#54362,#54363,#54364,#54365,#54366,#54367,#54368,#54369,#54370,#54371,#54372,
#54373,#54374,#54375,#54376,#54377,#54378,#54379,#54380,#54381,#54382,#54383,
#54384,#54385,#54386,#54387,#54388,#54389,#54390,#54391,#54392,#54393,#54394,
#54395,#54396,#54397,#54398,#54399,#54400,#54401,#54402,#54403,#54404,#54405,
#54406,#54407,#54408,#54409,#54410,#54411,#54412,#54413,#54414,#54415,#54416,
#54417,#54418,#54419,#54420,#54421,#54422,#54423,#54424,#54425,#54426,#54427,
#54428,#54429,#54430,#54431,#54432,#54433,#54434,#54435,#54436,#54437,#54438,
#54439,#54440,#54441,#54442,#54443,#54444,#54445,#54446,#54447,#54448,#54449,
#54450,#54451,#54452,#54453,#54454,#54455,#54456,#54457,#54458,#54459,#54460,
#54461,#54462,#54463,#54464,#54465,#54466,#54467,#54468,#54469,#54470,#54471,
#54472,#54473,#54474,#54475,#54476,#54477,#54478),.UNSPECIFIED.,.F.,.F.,
(4,3,3,3,3,3,3,3,3,3,3,3,3,3,3,3,3,3,3,3,3,3,3,3,3,3,3,3,3,3,3,3,3,3,3,
3,3,3,3,3,3,3,3,3,3,3,3,3,3,3,3,3,3,3,3,3,3,3,3,3,3,3,3,3,3,3,4),(2.02865585856489,
2.12402762122252,2.23323999155846,2.34234107107911,2.45137236451629,2.56037527914099,
2.66947003572026,2.77860579083783,2.88794878790004,2.9861951620001,2.99492423721753,
2.99498563286815,3.09555643554825,3.10492541786507,3.21597401277663,3.32561358356885,
3.43518668625693,3.54473379827187,3.65687889299329,3.76656517412907,3.8799396756433,
3.97859548600955,3.99325757945939,3.99331417715754,4.09371825155224,4.10302725066695,
4.21410418451445,4.32351125154536,4.43285029772412,4.54216215354018,4.65453229551687,
4.76398290563599,4.87781281354146,4.97628013227034,4.9915883385075,4.99164272144692,
5.09202893482422,5.10141432669419,5.21248394407445,5.32195215739788,5.43135314730772,
5.54072763591608,5.65303854337114,5.76255273957561,5.87626200265596,5.97481642665783,
5.98991760907827,5.98997126573631,6.09040615425878,6.09976697233783,6.21083357704881,
6.32032727182328,6.42975419592545,6.53915503546805,6.65144122910747,6.76098253848876,
6.87464117425723,6.97319126496119,6.98824561473473,6.9882998100257,7.08940671165733,
7.09951538805716,7.21054493226041,7.32140398308574,7.43216340464187,7.54286555752923,
7.59300756235177),.UNSPECIFIED.) ;
#1312 = B_SPLINE_CURVE_WITH_KNOTS('',3,(#54479,#54480,#54481,#54482,#54483,
#54484,#54485,#54486),.UNSPECIFIED.,.F.,.F.,(4,2,2,4),(-1.10884496276699,
-1.08689879128658,-1.05535201010488,-1.05003008412879),.UNSPECIFIED.) ;
#1313 = B_SPLINE_CURVE_WITH_KNOTS('',3,(#54493,#54494,#54495,#54496,#54497,
#54498,#54499,#54500,#54501,#54502,#54503,#54504,#54505,#54506,#54507,#54508,
#54509,#54510,#54511,#54512,#54513,#54514,#54515,#54516,#54517,#54518,#54519,
#54520,#54521,#54522,#54523,#54524,#54525,#54526,#54527,#54528,#54529,#54530,
#54531,#54532,#54533,#54534,#54535),.UNSPECIFIED.,.F.,.F.,(4,3,3,3,3,3,
3,3,3,3,3,3,3,3,4),(-17.9380018385438,-17.8425458057697,-17.7333362973642,
-17.6242380988214,-17.5152097045172,-17.4062097063169,-17.2971178825619,
-17.1879850740603,-17.0786450208909,-16.9803981893995,-16.9716460291613,
-16.9715852529196,-16.8695608211846,-16.8587047742622,-16.7648876345291),
 .UNSPECIFIED.) ;
#1314 = B_SPLINE_CURVE_WITH_KNOTS('',3,(#54541,#54542,#54543,#54544,#54545,
#54546,#54547,#54548,#54549,#54550,#54551,#54552,#54553,#54554,#54555,#54556,
#54557,#54558,#54559,#54560,#54561,#54562,#54563,#54564,#54565,#54566,#54567,
#54568,#54569,#54570,#54571,#54572,#54573,#54574,#54575,#54576,#54577,#54578,
#54579,#54580,#54581,#54582,#54583,#54584,#54585,#54586,#54587,#54588,#54589,
#54590,#54591,#54592,#54593,#54594,#54595,#54596,#54597,#54598,#54599,#54600,
#54601,#54602,#54603,#54604,#54605,#54606,#54607,#54608,#54609,#54610,#54611,
#54612,#54613,#54614,#54615,#54616,#54617,#54618,#54619,#54620,#54621,#54622,
#54623,#54624,#54625,#54626,#54627,#54628,#54629,#54630,#54631,#54632,#54633,
#54634,#54635,#54636,#54637,#54638,#54639,#54640,#54641,#54642,#54643,#54644,
#54645,#54646,#54647,#54648,#54649,#54650,#54651,#54652,#54653,#54654,#54655,
#54656,#54657,#54658,#54659,#54660,#54661,#54662,#54663,#54664,#54665,#54666,
#54667,#54668,#54669,#54670,#54671,#54672,#54673,#54674,#54675,#54676,#54677,
#54678,#54679,#54680,#54681,#54682,#54683,#54684,#54685,#54686,#54687,#54688,
#54689,#54690,#54691,#54692,#54693,#54694,#54695,#54696,#54697,#54698,#54699,
#54700,#54701,#54702,#54703,#54704,#54705,#54706,#54707,#54708,#54709,#54710,
#54711,#54712,#54713,#54714,#54715,#54716,#54717,#54718,#54719,#54720,#54721,
#54722,#54723,#54724,#54725,#54726,#54727,#54728,#54729,#54730,#54731,#54732,
#54733,#54734,#54735,#54736,#54737,#54738,#54739),.UNSPECIFIED.,.F.,.F.,
(4,3,3,3,3,3,3,3,3,3,3,3,3,3,3,3,3,3,3,3,3,3,3,3,3,3,3,3,3,3,3,3,3,3,3,
3,3,3,3,3,3,3,3,3,3,3,3,3,3,3,3,3,3,3,3,3,3,3,3,3,3,3,3,3,3,3,4),(14.2294869669467,
14.3389322308676,14.4483223291313,14.5576979646225,14.6671790216403,14.7767121569683,
14.8864519699031,14.9748738708372,14.9749281643408,15.0752588397667,15.0846363989758,
15.1957139376826,15.3051193758575,15.4144579925258,15.5237706155259,15.636142138802,
15.7455964652154,15.8594265869228,15.9579660798332,15.9732006708539,15.9732567086302,
16.0738047882785,16.0831967562974,16.1942453183752,16.3038843458098,16.4134566034534,
16.5230025687912,16.6351482398233,16.744832633098,16.8582089430088,16.9568845136797,
16.9715246332023,16.9715852529196,17.0721645754056,17.081310467377,17.192385883606,
17.3018169902679,17.4111845419844,17.5205293926883,17.6328754938185,17.742370217053,
17.856142007131,17.9543426244737,17.9698496806575,17.969913797209,18.0695603136759,
18.0792819826719,18.1904020275252,18.299458347709,18.4084455018845,18.5174049537962,
18.6301143007217,18.7392156390599,18.8537289902791,18.9524526707438,18.968208839462,
18.9682423414984,19.0701323904312,19.0803666377335,19.192253585914,19.3040020972769,
19.4156475035808,19.5272249970061,19.6388130843005,19.7503972247079,19.8620929819371,
19.9665708857877),.UNSPECIFIED.) ;
#1315 = B_SPLINE_CURVE_WITH_KNOTS('',3,(#54741,#54742,#54743,#54744,#54745,
#54746,#54747,#54748,#54749,#54750,#54751,#54752,#54753,#54754,#54755,#54756,
#54757,#54758,#54759,#54760,#54761,#54762,#54763,#54764,#54765,#54766,#54767,
#54768,#54769,#54770,#54771,#54772,#54773,#54774,#54775,#54776,#54777,#54778,
#54779,#54780,#54781,#54782,#54783,#54784,#54785,#54786,#54787,#54788,#54789,
#54790,#54791,#54792,#54793,#54794,#54795,#54796,#54797,#54798,#54799,#54800,
#54801,#54802,#54803,#54804,#54805,#54806,#54807,#54808,#54809,#54810,#54811,
#54812,#54813,#54814,#54815,#54816,#54817,#54818,#54819,#54820,#54821,#54822,
#54823,#54824,#54825,#54826,#54827,#54828,#54829,#54830,#54831,#54832,#54833,
#54834,#54835,#54836,#54837,#54838,#54839,#54840,#54841,#54842,#54843,#54844),
 .UNSPECIFIED.,.F.,.F.,(4,2,2,2,2,2,2,2,2,2,2,2,2,2,2,2,2,2,2,2,2,2,2,2,
2,2,2,2,2,2,2,2,2,2,2,2,2,2,2,2,2,2,2,2,2,2,2,2,2,2,2,4),(1.10920453594835,
1.1166320815093,1.13793450121648,1.16974966156749,1.18645799264353,1.19551033122356,
1.20841878766804,1.22710875477439,1.26309690717015,1.27863717849374,1.29593413862243,
1.31630153851001,1.35134179362724,1.36087497196007,1.3721034776389,1.40414323734612,
1.43154792730153,1.4467050506917,1.46463919801635,1.48653286711609,1.51886748686928,
1.52822543273842,1.53987769753952,1.5555523588918,1.59701777933286,1.61255121200086,
1.62986742642601,1.65028403353202,1.68511285067916,1.69466952558485,1.70590048122777,
1.73794741238401,1.76525899060161,1.78040499829536,1.79833960200703,1.82023252238522,
1.85263795723406,1.86198361343096,1.87358284299029,1.88915308158601,1.93075092780285,
1.94618976202995,1.96335684506068,1.98349276395793,2.01944550510397,2.0288905106591,
2.04041875376629,2.05577463402855,2.09782802978038,2.11336056920194,2.13105185822123,
2.15957942398687),.UNSPECIFIED.) ;
#1316 = B_SPLINE_CURVE_WITH_KNOTS('',3,(#54850,#54851,#54852,#54853,#54854,
#54855,#54856,#54857,#54858,#54859),.UNSPECIFIED.,.F.,.F.,(4,2,2,2,4),(0.00010533907809324,
0.013377535183783,0.022284006867853,0.0315331293986908,0.0589297775460328),
 .UNSPECIFIED.) ;
#1317 = B_SPLINE_CURVE_WITH_KNOTS('',3,(#54861,#54862,#54863,#54864,#54865,
#54866,#54867,#54868,#54869,#54870,#54871,#54872,#54873,#54874,#54875,#54876,
#54877,#54878,#54879,#54880,#54881,#54882,#54883,#54884,#54885,#54886,#54887,
#54888,#54889,#54890,#54891,#54892,#54893,#54894,#54895,#54896,#54897,#54898,
#54899,#54900,#54901,#54902,#54903,#54904,#54905,#54906,#54907,#54908,#54909,
#54910,#54911,#54912,#54913,#54914,#54915,#54916,#54917,#54918,#54919,#54920,
#54921,#54922,#54923,#54924,#54925,#54926,#54927,#54928,#54929,#54930,#54931,
#54932,#54933,#54934,#54935,#54936,#54937,#54938,#54939,#54940,#54941,#54942,
#54943,#54944,#54945,#54946,#54947,#54948,#54949,#54950,#54951,#54952,#54953,
#54954,#54955,#54956,#54957,#54958,#54959,#54960,#54961,#54962,#54963,#54964,
#54965,#54966,#54967,#54968,#54969,#54970,#54971,#54972,#54973,#54974,#54975,
#54976,#54977,#54978,#54979,#54980,#54981,#54982,#54983,#54984,#54985,#54986,
#54987,#54988,#54989,#54990),.UNSPECIFIED.,.F.,.F.,(4,3,3,3,3,3,3,3,3,3,
3,3,3,3,3,3,3,3,3,3,3,3,3,3,3,3,3,3,3,3,3,3,3,3,3,3,3,3,3,3,3,3,3,4),(-3.84638256364261,
-3.73820745978248,-3.63014941624604,-3.52216594268968,-3.41421428740373,
-3.30617544820113,-3.19809625937625,-3.08981663623424,-2.99504625172493,
-2.99498563286813,-2.89440631145632,-2.88526042240579,-2.77418500567741,
-2.66475390299952,-2.55538635525859,-2.44604150852038,-2.33369540353497,
-2.22420068422119,-2.11042888639997,-2.0122282719807,-1.99672120457837,
-1.99665708857875,-1.89701057277755,-1.88728891067,-1.77616886487242,-1.66711255158284,
-1.55812540403875,-1.44916595848633,-1.33645660493709,-1.22735527221197,
-1.11284190825067,-1.01411823893781,-0.998362046647454,-0.99832854428937,
-0.896438498507768,-0.886204234316478,-0.77431727268097,-0.662568748059076,
-0.550923328723212,-0.43934582252413,-0.327757722968657,-0.216173570578685,
-0.104477801978497,-5.02812373608076E-13),.UNSPECIFIED.) ;
#1318 = B_SPLINE_CURVE_WITH_KNOTS('',3,(#54994,#54995,#54996,#54997,#54998,
#54999,#55000,#55001,#55002,#55003,#55004,#55005,#55006,#55007,#55008,#55009,
#55010,#55011,#55012,#55013,#55014,#55015,#55016,#55017,#55018,#55019,#55020,
#55021,#55022,#55023,#55024,#55025,#55026,#55027,#55028,#55029,#55030,#55031,
#55032,#55033,#55034,#55035,#55036,#55037,#55038,#55039,#55040,#55041,#55042,
#55043,#55044,#55045,#55046,#55047,#55048,#55049,#55050,#55051,#55052,#55053,
#55054,#55055,#55056,#55057,#55058,#55059,#55060,#55061,#55062,#55063,#55064,
#55065,#55066,#55067,#55068,#55069,#55070,#55071,#55072,#55073,#55074,#55075,
#55076,#55077,#55078,#55079,#55080,#55081,#55082,#55083,#55084,#55085,#55086,
#55087,#55088,#55089,#55090,#55091,#55092,#55093,#55094,#55095,#55096,#55097,
#55098,#55099,#55100,#55101,#55102,#55103,#55104,#55105,#55106,#55107,#55108,
#55109,#55110,#55111,#55112,#55113,#55114,#55115,#55116,#55117,#55118,#55119,
#55120,#55121,#55122,#55123,#55124,#55125,#55126,#55127,#55128,#55129,#55130,
#55131,#55132,#55133,#55134,#55135,#55136,#55137,#55138,#55139,#55140,#55141,
#55142,#55143,#55144,#55145,#55146,#55147,#55148,#55149,#55150,#55151,#55152,
#55153,#55154,#55155,#55156,#55157,#55158,#55159,#55160,#55161,#55162,#55163,
#55164,#55165,#55166,#55167,#55168,#55169,#55170,#55171,#55172,#55173,#55174,
#55175,#55176,#55177,#55178,#55179,#55180,#55181,#55182,#55183,#55184,#55185,
#55186,#55187,#55188,#55189,#55190,#55191,#55192),.UNSPECIFIED.,.F.,.F.,
(4,3,3,3,3,3,3,3,3,3,3,3,3,3,3,3,3,3,3,3,3,3,3,3,3,3,3,3,3,3,3,3,3,3,3,
3,3,3,3,3,3,3,3,3,3,3,3,3,3,3,3,3,3,3,3,3,3,3,3,3,3,3,3,3,3,3,4),(2.02856916811818,
2.12402508352432,2.23323459585707,2.3423327983503,2.45136119662696,2.56036119882055,
2.66945302658712,2.77858583911685,2.88792589630695,2.98617272709135,2.99492485577242,
2.99498563286816,3.09555717591128,3.10492395017402,3.21597272854696,3.32561103972279,
3.43518296101929,3.54472896932239,3.65687527128118,3.76656064185824,3.87993740950789,
3.97859131455151,3.99325792967966,3.99331417715755,4.09371875826342,4.10302769217917,
4.21410457083764,4.32351219675406,4.43285184432446,4.54216434323133,4.65453393778523,
4.76398528807051,4.87781400475873,4.97628109455529,4.99158842889737,4.99164272144694,
5.09202944416287,5.1014154817733,5.21248495476868,5.32195432557387,5.43135647200078,
5.54073211535619,5.65304190295122,5.76255724150614,5.87626425362123,5.97481946627002,
5.98991764446527,5.98997126573632,6.09040625393766,6.09976728300663,6.21083384888401,
6.32032780763715,6.4297549783069,6.53915604721805,6.65144198791996,6.76098348433243,
6.87464164717906,6.9731920566554,6.98824570503598,6.9882998100257,7.08940654529792,
7.09951520459782,7.21054455240904,7.32140338904543,7.4321625863856,7.54286450158988,
7.59300756235177),.UNSPECIFIED.) ;
#1319 = B_SPLINE_CURVE_WITH_KNOTS('',3,(#55193,#55194,#55195,#55196,#55197,
#55198,#55199,#55200),.UNSPECIFIED.,.F.,.F.,(4,2,2,4),(-1.10884009192702,
-1.08690736009366,-1.05535892792443,-1.05002476366986),.UNSPECIFIED.) ;
#1320 = B_SPLINE_CURVE_WITH_KNOTS('',3,(#55206,#55207,#55208,#55209,#55210,
#55211,#55212,#55213,#55214,#55215,#55216,#55217,#55218,#55219,#55220,#55221,
#55222,#55223,#55224,#55225,#55226,#55227,#55228,#55229,#55230,#55231,#55232,
#55233),.UNSPECIFIED.,.F.,.F.,(4,2,2,2,2,2,2,2,2,2,2,2,2,4),(0.459098935875569,
0.464417734433904,0.505520800153837,0.520882111108831,0.52986479302885,
0.5423026928859,0.575113037158553,0.614875876244612,0.632729769250043,0.649501533827279,
0.687496632532719,0.719965224203154,0.726875831338429,0.732438471583609),
 .UNSPECIFIED.) ;
#1321 = B_SPLINE_CURVE_WITH_KNOTS('',3,(#55236,#55237,#55238,#55239,#55240,
#55241,#55242,#55243,#55244,#55245,#55246,#55247,#55248,#55249,#55250,#55251,
#55252,#55253,#55254,#55255,#55256,#55257,#55258,#55259,#55260,#55261,#55262,
#55263,#55264,#55265,#55266,#55267,#55268,#55269,#55270,#55271),
 .UNSPECIFIED.,.F.,.F.,(4,2,2,2,2,2,2,2,2,2,2,2,2,2,2,2,2,4),(0.0003284355859769,
0.00531767720044407,0.0119536835984835,0.0490121209748348,0.0844681757214455,
0.100405765516477,0.11631259325507,0.149557305146467,0.178278962167049,
0.190732222627568,0.201079007639284,0.210406505179939,0.232092261470985,
0.282159926353324,0.300140818751553,0.315111986607238,0.33700779754842,
0.381142777041596),.UNSPECIFIED.) ;
#1322 = B_SPLINE_CURVE_WITH_KNOTS('',3,(#55277,#55278,#55279,#55280,#55281,
#55282,#55283,#55284,#55285,#55286,#55287,#55288,#55289,#55290,#55291,#55292,
#55293,#55294,#55295,#55296,#55297,#55298,#55299,#55300,#55301,#55302,#55303,
#55304,#55305,#55306,#55307,#55308,#55309,#55310,#55311,#55312,#55313,#55314,
#55315,#55316,#55317,#55318,#55319,#55320,#55321,#55322,#55323,#55324,#55325,
#55326,#55327,#55328,#55329,#55330,#55331,#55332,#55333,#55334,#55335,#55336,
#55337,#55338,#55339,#55340,#55341,#55342,#55343,#55344,#55345,#55346,#55347,
#55348,#55349,#55350),.UNSPECIFIED.,.F.,.F.,(4,2,2,2,2,2,2,2,2,2,2,2,2,
2,2,2,2,2,2,2,2,2,2,2,2,2,2,2,2,2,2,2,2,2,2,2,4),(1.29359998411323,1.30095406668721,
1.31741432341847,1.33295482268895,1.36148535680912,1.40267840562338,1.4168827682256,
1.42564857009657,1.43856307377589,1.45605514494036,1.50897620000202,1.52485836063247,
1.54087322196961,1.57757886415223,1.61688912127807,1.62695610494123,1.63658903940002,
1.66191828021951,1.71494369390444,1.73069937007811,1.74683327998757,1.78395462238556,
1.82219256849362,1.832340258941,1.84185095546442,1.86546888373326,1.92105272943006,
1.93665099692755,1.95279196240484,1.97294420449489,2.01346271879964,2.03165906133175,
2.04072270747648,2.05190736557107,2.06584925450052,2.11923314491368,2.12891857368306),
 .UNSPECIFIED.) ;
#1323 = B_SPLINE_CURVE_WITH_KNOTS('',3,(#55351,#55352,#55353,#55354,#55355,
#55356,#55357,#55358,#55359,#55360,#55361,#55362,#55363,#55364,#55365,#55366,
#55367,#55368,#55369,#55370,#55371,#55372,#55373,#55374,#55375,#55376,#55377,
#55378,#55379,#55380,#55381,#55382,#55383,#55384,#55385,#55386,#55387,#55388,
#55389,#55390,#55391,#55392),.UNSPECIFIED.,.F.,.F.,(4,2,2,2,2,2,2,2,2,2,
2,2,2,2,2,2,2,2,2,2,4),(0.000738082385943926,0.0138519484644011,0.0295692425710776,
0.0794798266889706,0.106573518509978,0.116314733841013,0.126412928211499,
0.165039800973681,0.201315998205497,0.217463598449292,0.233563252041158,
0.267515628887756,0.296218550217051,0.313295008909005,0.322142293471645,
0.332500284255174,0.366422341235642,0.408081104489123,0.424788295102322,
0.439776151822035,0.459098935875569),.UNSPECIFIED.) ;
#1324 = B_SPLINE_CURVE_WITH_KNOTS('',3,(#55393,#55394,#55395,#55396,#55397,
#55398,#55399,#55400,#55401,#55402,#55403,#55404,#55405,#55406,#55407,#55408,
#55409,#55410,#55411,#55412,#55413,#55414,#55415,#55416,#55417,#55418,#55419,
#55420,#55421,#55422,#55423,#55424,#55425,#55426,#55427,#55428,#55429,#55430,
#55431,#55432,#55433,#55434,#55435,#55436,#55437,#55438,#55439,#55440,#55441,
#55442,#55443,#55444,#55445,#55446,#55447,#55448,#55449,#55450,#55451,#55452,
#55453,#55454,#55455,#55456,#55457,#55458,#55459,#55460,#55461,#55462,#55463,
#55464,#55465,#55466,#55467,#55468,#55469,#55470,#55471,#55472,#55473,#55474,
#55475,#55476,#55477,#55478,#55479,#55480,#55481,#55482,#55483,#55484,#55485,
#55486,#55487,#55488,#55489,#55490,#55491,#55492,#55493,#55494,#55495,#55496,
#55497,#55498,#55499,#55500,#55501,#55502,#55503,#55504,#55505,#55506),
 .UNSPECIFIED.,.F.,.F.,(4,2,2,2,2,2,2,2,2,2,2,2,2,2,2,2,2,2,2,2,2,2,2,2,
2,2,2,2,2,2,2,2,2,2,2,2,2,2,2,2,2,2,2,2,2,2,2,2,2,2,2,2,2,2,2,2,4),(9.9999999911049E-7,
0.0181412579621644,0.0260517011858928,0.03569506804886,0.0856389271588889,
0.114970951918313,0.130443396223946,0.146521745286428,0.197472647378066,
0.222831685352658,0.23242000657169,0.242317758348657,0.28307583406927,0.318816335082925,
0.334727678149403,0.350487394344637,0.404321518915359,0.421345075068166,
0.434025097613039,0.442753508335243,0.457052499386952,0.501754765373651,
0.527684940848551,0.542966732260761,0.559688778480777,0.595876018588788,
0.629041013088632,0.64065417101676,0.649497725865986,0.665641909499553,
0.708103849070844,0.728232473019738,0.744532529259699,0.760012287632047,
0.788626677992194,0.82285658068839,0.841440446077428,0.850502880244777,
0.861330836969597,0.911157653131982,0.938261616252987,0.953631128251108,
0.970141586102395,1.01737241808675,1.03635678173686,1.04992207666676,1.05862155682344,
1.07186549350823,1.11259380862868,1.142628458096,1.15820158179272,1.17436083719213,
1.22518214710482,1.25065900116484,1.2602658284382,1.2701883131198,1.29377606271217),
 .UNSPECIFIED.) ;
#1325 = B_SPLINE_CURVE_WITH_KNOTS('',3,(#55512,#55513,#55514,#55515,#55516,
#55517,#55518,#55519,#55520,#55521,#55522,#55523,#55524,#55525,#55526,#55527,
#55528,#55529,#55530,#55531,#55532,#55533,#55534,#55535,#55536,#55537,#55538,
#55539,#55540,#55541,#55542,#55543,#55544,#55545,#55546,#55547,#55548,#55549,
#55550,#55551,#55552,#55553,#55554,#55555,#55556,#55557,#55558,#55559,#55560,
#55561,#55562,#55563,#55564,#55565,#55566,#55567,#55568,#55569,#55570,#55571,
#55572,#55573,#55574,#55575,#55576,#55577,#55578,#55579,#55580,#55581,#55582,
#55583,#55584,#55585,#55586,#55587,#55588,#55589,#55590,#55591,#55592,#55593,
#55594,#55595,#55596,#55597,#55598,#55599,#55600,#55601,#55602),
 .UNSPECIFIED.,.F.,.F.,(4,3,3,3,3,3,3,3,3,3,3,3,3,3,3,3,3,3,3,3,3,3,3,3,
3,3,3,3,3,3,4),(15.7079632679487,15.8113041863724,15.9146184877327,16.0179415683624,
16.1213837812541,16.2248899519759,16.3224073436296,16.3285912852237,16.3947470380404,
16.394798101354,16.4893631462319,16.4989495063346,16.6029410394302,16.7068040901932,
16.8105977431501,16.9143569262867,17.0181165201345,17.1219800282497,17.2258994684857,
17.3243086209598,17.3299977052375,17.3930777392184,17.3931266456435,17.488160245186,
17.4974425219354,17.6010533657214,17.6065554326192,17.7105958268345,17.8145672327603,
17.9185103805803,17.9338941646706),.UNSPECIFIED.) ;
#1326 = B_SPLINE_CURVE_WITH_KNOTS('',3,(#55604,#55605,#55606,#55607,#55608,
#55609,#55610,#55611,#55612,#55613,#55614,#55615,#55616,#55617,#55618,#55619,
#55620,#55621,#55622,#55623,#55624,#55625,#55626,#55627,#55628,#55629,#55630,
#55631,#55632,#55633,#55634,#55635,#55636,#55637,#55638,#55639,#55640,#55641,
#55642,#55643),.UNSPECIFIED.,.F.,.F.,(4,3,3,3,3,3,3,3,3,3,3,3,3,4),(14.3981410127754,
14.5041449103233,14.6100638854506,14.7159513361487,14.8218268476716,14.9277203457283,
15.033661766908,15.1397601395315,15.245946872782,15.3523359246553,15.3964695570646,
15.5190118197687,15.6402404822583,15.7079554008178),.UNSPECIFIED.) ;
#1327 = B_SPLINE_CURVE_WITH_KNOTS('',3,(#55646,#55647,#55648,#55649,#55650,
#55651,#55652,#55653,#55654,#55655,#55656,#55657,#55658,#55659,#55660,#55661,
#55662,#55663,#55664,#55665,#55666,#55667,#55668,#55669,#55670,#55671,#55672,
#55673,#55674,#55675,#55676,#55677,#55678,#55679,#55680,#55681,#55682,#55683,
#55684,#55685,#55686,#55687,#55688,#55689,#55690,#55691,#55692,#55693,#55694,
#55695,#55696,#55697,#55698,#55699,#55700,#55701,#55702,#55703,#55704,#55705,
#55706,#55707,#55708,#55709,#55710,#55711,#55712,#55713,#55714,#55715,#55716,
#55717,#55718,#55719),.UNSPECIFIED.,.F.,.F.,(4,2,2,2,2,2,2,2,2,2,2,2,2,
2,2,2,2,2,2,2,2,2,2,2,2,2,2,2,2,2,2,2,2,2,2,2,4),(8.98756407565875E-5,0.00958673476959858,
0.0632031336255092,0.0833445098038401,0.0995431819327776,0.115206036663946,
0.168389320176256,0.192964400571718,0.202521587597258,0.212531919880494,
0.252085336041996,0.277375924344348,0.29734241960763,0.31221965819781,0.33141213917936,
0.375535701000085,0.398575768451147,0.408036346243251,0.418062919419705,
0.451131415410438,0.491791764285841,0.508201330943047,0.523322593889842,
0.549083529179824,0.593368985045316,0.607943154443325,0.616608600447831,
0.628783684406638,0.661898827321747,0.699758037739072,0.715623109939765,
0.731218812619801,0.763029012118359,0.808061561073486,0.818144105240131,
0.826091049587224,0.835764201608868),.UNSPECIFIED.) ;
#1328 = B_SPLINE_CURVE_WITH_KNOTS('',3,(#55725,#55726,#55727,#55728,#55729,
#55730,#55731,#55732,#55733,#55734,#55735,#55736,#55737,#55738,#55739,#55740,
#55741,#55742,#55743,#55744,#55745,#55746,#55747,#55748,#55749,#55750,#55751,
#55752),.UNSPECIFIED.,.F.,.F.,(4,2,2,2,2,2,2,2,2,2,2,2,2,4),(0.45910898550012,
0.464123317728498,0.504834291857946,0.520817723021585,0.529788408837737,
0.542027898291406,0.574819933375454,0.615161849610536,0.633018213721076,
0.649838699815419,0.687975160352418,0.719992757768681,0.726888844299736,
0.732445412692217),.UNSPECIFIED.) ;
#1329 = B_SPLINE_CURVE_WITH_KNOTS('',3,(#55755,#55756,#55757,#55758,#55759,
#55760,#55761,#55762,#55763,#55764,#55765,#55766,#55767,#55768,#55769,#55770,
#55771,#55772,#55773,#55774,#55775,#55776,#55777,#55778,#55779,#55780,#55781,
#55782,#55783,#55784,#55785,#55786,#55787,#55788,#55789,#55790),
 .UNSPECIFIED.,.F.,.F.,(4,2,2,2,2,2,2,2,2,2,2,2,2,2,2,2,2,4),(0.000321553292874637,
0.00529579930759916,0.0119020171496447,0.0494611338648065,0.0845644657484785,
0.100475323375435,0.116356578470903,0.149389590129435,0.178249519548127,
0.190726728454751,0.201086130709088,0.210416304464164,0.232095757180373,
0.282140266304572,0.300085602459823,0.315048158012112,0.336954443421903,
0.381146228182771),.UNSPECIFIED.) ;
#1330 = B_SPLINE_CURVE_WITH_KNOTS('',3,(#55796,#55797,#55798,#55799,#55800,
#55801,#55802,#55803,#55804,#55805,#55806,#55807,#55808,#55809,#55810,#55811,
#55812,#55813,#55814,#55815,#55816,#55817,#55818,#55819,#55820,#55821,#55822,
#55823,#55824,#55825,#55826,#55827,#55828,#55829,#55830,#55831,#55832,#55833,
#55834,#55835,#55836,#55837,#55838,#55839,#55840,#55841,#55842,#55843,#55844,
#55845,#55846,#55847,#55848,#55849,#55850,#55851,#55852,#55853,#55854,#55855,
#55856,#55857,#55858,#55859,#55860,#55861,#55862,#55863,#55864,#55865,#55866,
#55867,#55868,#55869,#55870,#55871,#55872,#55873),.UNSPECIFIED.,.F.,.F.,
(4,2,2,2,2,2,2,2,2,2,2,2,2,2,2,2,2,2,2,2,2,2,2,2,2,2,2,2,2,2,2,2,2,2,2,
2,2,2,4),(0.458614805141202,0.468276334293724,0.484172078983711,0.500138368708875,
0.548722523717207,0.568332719679477,0.582181641216813,0.590935448093863,
0.604134706231622,0.647012452574512,0.675653447701051,0.691206326288677,
0.707661678880968,0.727803084519804,0.771146082241682,0.786438447891096,
0.795296281120897,0.807292273622826,0.840558191000508,0.878772863383274,
0.894768757920461,0.910644605195344,0.94542027431542,0.985939907421154,
0.99655236593802,1.00576978002281,1.02579542812151,1.06650639499888,1.08968052587657,
1.10474702453885,1.12218254242584,1.14210899514003,1.18334736526887,1.19827456080035,
1.20708809368799,1.21960615721636,1.25306240072434,1.2797654071498,1.29379501408075),
 .UNSPECIFIED.) ;
#1331 = B_SPLINE_CURVE_WITH_KNOTS('',3,(#55874,#55875,#55876,#55877,#55878,
#55879,#55880,#55881,#55882,#55883,#55884,#55885,#55886,#55887,#55888,#55889,
#55890,#55891,#55892,#55893,#55894,#55895,#55896,#55897,#55898,#55899,#55900,
#55901,#55902,#55903,#55904,#55905,#55906,#55907,#55908,#55909,#55910,#55911,
#55912,#55913,#55914,#55915),.UNSPECIFIED.,.F.,.F.,(4,2,2,2,2,2,2,2,2,2,
2,2,2,2,2,2,2,2,2,2,4),(0.00074538786090497,0.0138027418242267,0.0294144634151981,
0.078270908564491,0.106441999089265,0.11623114716668,0.126288013383736,
0.165379768164886,0.201338030985534,0.217448030072118,0.233531439200502,
0.26733290588678,0.296230510522788,0.313365850679765,0.322212279066863,
0.332565896103022,0.36644770944264,0.407902212188932,0.424580316139229,
0.439550483908069,0.45910898550012),.UNSPECIFIED.) ;
#1332 = B_SPLINE_CURVE_WITH_KNOTS('',3,(#55916,#55917,#55918,#55919,#55920,
#55921,#55922,#55923,#55924,#55925,#55926,#55927,#55928,#55929,#55930,#55931,
#55932,#55933,#55934,#55935,#55936,#55937,#55938,#55939,#55940,#55941,#55942,
#55943,#55944,#55945,#55946,#55947,#55948,#55949,#55950,#55951,#55952,#55953,
#55954,#55955,#55956,#55957,#55958,#55959,#55960,#55961,#55962,#55963,#55964,
#55965,#55966,#55967,#55968,#55969,#55970,#55971,#55972,#55973,#55974,#55975,
#55976,#55977,#55978,#55979,#55980,#55981,#55982,#55983,#55984,#55985,#55986,
#55987,#55988,#55989,#55990,#55991,#55992,#55993,#55994,#55995,#55996,#55997,
#55998,#55999,#56000,#56001,#56002,#56003,#56004,#56005,#56006,#56007,#56008,
#56009,#56010,#56011,#56012,#56013,#56014,#56015,#56016,#56017,#56018,#56019,
#56020,#56021,#56022,#56023,#56024,#56025,#56026,#56027,#56028,#56029,#56030,
#56031),.UNSPECIFIED.,.F.,.F.,(4,2,2,2,2,2,2,2,2,2,2,2,2,2,2,2,2,2,2,2,
2,2,2,2,2,2,2,2,2,2,2,2,2,2,2,2,2,2,2,2,2,2,2,2,2,2,2,2,2,2,2,2,2,2,2,2,
2,4),(1.00000001892163E-6,0.0125988430125637,0.0214541379866562,0.030189816183294,
0.0430833350666729,0.0868476702733789,0.115249975074114,0.130656050971666,
0.146839979433289,0.196767185511196,0.21481261268838,0.227955380941075,
0.236633839533386,0.250201735758349,0.29112270602314,0.32059920547237,0.336134579367343,
0.352340352688741,0.404741003149359,0.42865449581047,0.43816468646413,0.448226683737091,
0.48711735581692,0.521799384735325,0.538317185364559,0.553685912926676,
0.58074739823862,0.616635941990185,0.630291683837093,0.641287517650734,
0.65029001640104,0.668227485523075,0.708737595010008,0.728900958505633,
0.745001307548107,0.760605312967583,0.815946752036598,0.839765022519998,
0.849264640463107,0.859307773470979,0.898409307993087,0.935515748610904,
0.951393430137624,0.967197254334127,1.01705271376006,1.03617851658254,1.04980500103518,
1.05850438042598,1.07168754742342,1.11238036824938,1.14252866008741,1.158107881077,
1.17425428651828,1.22521120025375,1.25061763376755,1.26022001215864,1.27014486204402,
1.29372393529934),.UNSPECIFIED.) ;
#1333 = B_SPLINE_CURVE_WITH_KNOTS('',3,(#56037,#56038,#56039,#56040,#56041,
#56042,#56043,#56044,#56045,#56046,#56047,#56048,#56049,#56050,#56051,#56052,
#56053,#56054,#56055,#56056,#56057,#56058,#56059,#56060,#56061,#56062,#56063,
#56064,#56065,#56066,#56067,#56068,#56069,#56070,#56071,#56072,#56073,#56074,
#56075,#56076,#56077,#56078,#56079,#56080,#56081,#56082,#56083,#56084,#56085,
#56086,#56087,#56088,#56089,#56090,#56091,#56092,#56093,#56094,#56095,#56096,
#56097,#56098,#56099,#56100,#56101,#56102,#56103,#56104,#56105,#56106,#56107,
#56108,#56109,#56110,#56111,#56112,#56113,#56114,#56115,#56116,#56117,#56118,
#56119,#56120,#56121,#56122,#56123,#56124,#56125,#56126,#56127),
 .UNSPECIFIED.,.F.,.F.,(4,3,3,3,3,3,3,3,3,3,3,3,3,3,3,3,3,3,3,3,3,3,3,3,
3,3,3,3,3,3,4),(15.7079632679487,15.811277521818,15.9145643079774,16.0178590600282,
16.1212718704572,16.2247479979436,16.3222741136381,16.3284185432556,16.3947481283565,
16.394798101356,16.4893555683339,16.4989409022619,16.6029238165732,16.7067782344606,
16.8105632454197,16.9143137789071,17.0180647169156,17.1219195878195,17.2258303871081,
17.3242448251247,17.3299200437246,17.3930794452619,17.3931266456454,17.4881639775743,
17.4974391842717,17.6010561100227,17.6065518441373,17.7105895362785,17.8145584563115,
17.9184994130691,17.9338898237342),.UNSPECIFIED.) ;
#1334 = B_SPLINE_CURVE_WITH_KNOTS('',3,(#56129,#56130,#56131,#56132,#56133,
#56134,#56135,#56136,#56137,#56138,#56139,#56140,#56141,#56142,#56143,#56144,
#56145,#56146,#56147,#56148,#56149,#56150,#56151,#56152,#56153,#56154,#56155,
#56156,#56157,#56158,#56159,#56160,#56161,#56162,#56163,#56164,#56165,#56166,
#56167,#56168),.UNSPECIFIED.,.F.,.F.,(4,3,3,3,3,3,3,3,3,3,3,3,3,4),(14.3981410127773,
14.5041748950571,14.610124992509,14.7160450299549,14.8219539908772,14.9278817223058,
15.0338580831529,15.1399921691173,15.2462150867062,15.3526406391366,15.3964695570665,
15.5190266859576,15.6402596565994,15.7079553591874),.UNSPECIFIED.) ;
#1335 = B_SPLINE_CURVE_WITH_KNOTS('',3,(#56172,#56173,#56174,#56175,#56176,
#56177,#56178,#56179,#56180,#56181,#56182,#56183,#56184,#56185,#56186,#56187,
#56188,#56189,#56190,#56191,#56192,#56193,#56194,#56195,#56196,#56197,#56198,
#56199,#56200,#56201,#56202,#56203,#56204,#56205,#56206,#56207,#56208,#56209),
 .UNSPECIFIED.,.F.,.F.,(4,2,2,2,2,2,2,2,2,2,2,2,2,2,2,2,2,2,4),(0.000123090557559488,
0.00529923882504241,0.0119107487871958,0.0413163072992257,0.0805438068736347,
0.097519789031416,0.112580594592888,0.137496734407516,0.175111623725341,
0.188973027739506,0.200075494695848,0.20906163629957,0.226886150571072,
0.258165447247631,0.289415603200177,0.305220905766297,0.321065189093378,
0.357976300969813,0.377585064672507),.UNSPECIFIED.) ;
#1336 = B_SPLINE_CURVE_WITH_KNOTS('',3,(#56210,#56211,#56212,#56213,#56214,
#56215,#56216,#56217,#56218,#56219,#56220,#56221,#56222,#56223,#56224,#56225,
#56226,#56227,#56228,#56229,#56230,#56231,#56232,#56233,#56234,#56235,#56236,
#56237,#56238,#56239,#56240,#56241,#56242,#56243,#56244,#56245,#56246,#56247,
#56248,#56249,#56250,#56251,#56252,#56253,#56254,#56255),.UNSPECIFIED.,
 .F.,.F.,(4,2,2,2,2,2,2,2,2,2,2,2,2,2,2,2,2,2,2,2,2,2,4),(9.56198978167309E-5,
0.0155193550344561,0.0256373012228276,0.0344142215086527,0.0480745154991777,
0.0898821437212078,0.11876831069995,0.134277603293621,0.15055282867365,
0.200251947837585,0.218411629353159,0.231621827313627,0.240355829566199,
0.25409557288221,0.295119188869773,0.32439106078887,0.339982215933523,0.356354956915731,
0.405519961437129,0.423843305304581,0.437133033790102,0.445895732161899,
0.458271301746286),.UNSPECIFIED.) ;
#1337 = B_SPLINE_CURVE_WITH_KNOTS('',3,(#56262,#56263,#56264,#56265,#56266,
#56267,#56268,#56269,#56270,#56271,#56272,#56273,#56274,#56275,#56276,#56277,
#56278,#56279,#56280,#56281,#56282,#56283,#56284,#56285,#56286,#56287,#56288,
#56289,#56290,#56291,#56292,#56293,#56294,#56295,#56296,#56297,#56298,#56299,
#56300,#56301,#56302,#56303,#56304),.UNSPECIFIED.,.F.,.F.,(4,3,3,3,3,3,
3,3,3,3,3,3,3,3,4),(-17.9383918421104,-17.842556478735,-17.7333586134708,
-17.6242720817764,-17.515255375924,-17.4062670857227,-17.2971869615572,
-17.1880658673982,-17.0787374538633,-16.9804883875736,-16.9716433848556,
-16.9715852529204,-16.8695593508381,-16.8587164708144,-16.7649056225393),
 .UNSPECIFIED.) ;
#1338 = B_SPLINE_CURVE_WITH_KNOTS('',3,(#56310,#56311,#56312,#56313,#56314,
#56315,#56316,#56317,#56318,#56319,#56320,#56321,#56322,#56323,#56324,#56325,
#56326,#56327,#56328,#56329,#56330,#56331,#56332,#56333,#56334,#56335,#56336,
#56337,#56338,#56339,#56340,#56341,#56342,#56343,#56344,#56345,#56346,#56347,
#56348,#56349,#56350,#56351,#56352,#56353,#56354,#56355,#56356,#56357,#56358,
#56359,#56360,#56361,#56362,#56363,#56364,#56365,#56366,#56367,#56368,#56369,
#56370,#56371,#56372,#56373,#56374,#56375,#56376,#56377,#56378,#56379,#56380,
#56381,#56382,#56383,#56384,#56385,#56386,#56387,#56388,#56389,#56390,#56391,
#56392,#56393,#56394,#56395,#56396,#56397,#56398,#56399,#56400,#56401,#56402,
#56403,#56404,#56405,#56406,#56407,#56408,#56409,#56410,#56411,#56412,#56413,
#56414,#56415,#56416,#56417,#56418,#56419,#56420,#56421,#56422,#56423,#56424,
#56425,#56426,#56427,#56428,#56429,#56430,#56431,#56432,#56433,#56434,#56435,
#56436,#56437,#56438,#56439,#56440,#56441,#56442,#56443,#56444,#56445,#56446,
#56447,#56448,#56449,#56450,#56451,#56452,#56453,#56454,#56455,#56456,#56457,
#56458,#56459,#56460,#56461,#56462,#56463,#56464,#56465,#56466,#56467,#56468,
#56469,#56470,#56471,#56472,#56473,#56474,#56475,#56476,#56477,#56478,#56479,
#56480,#56481,#56482,#56483,#56484,#56485,#56486,#56487,#56488,#56489,#56490,
#56491,#56492,#56493,#56494,#56495,#56496,#56497,#56498,#56499,#56500,#56501,
#56502,#56503,#56504,#56505,#56506,#56507,#56508),.UNSPECIFIED.,.F.,.F.,
(4,3,3,3,3,3,3,3,3,3,3,3,3,3,3,3,3,3,3,3,3,3,3,3,3,3,3,3,3,3,3,3,3,3,3,
3,3,3,3,3,3,3,3,3,3,3,3,3,3,3,3,3,3,3,3,3,3,3,3,3,3,3,3,3,3,3,4),(14.2295088655003,
14.3389583388931,14.4483526855265,14.5577326052243,14.6672179769316,14.7767554532794,
14.8864995972602,14.9748743412368,14.9749281643414,15.0752585779058,15.0846394854706,
15.1957166383656,15.3051248124756,15.4144660288951,15.5237811130958,15.6361500119795,
15.7456064359459,15.8594315722883,15.9579727480213,15.9732021021314,15.9732567086308,
16.0737965463703,16.0831951929036,16.1942439504057,16.30388050249,16.4134499406568,
16.522992739184,16.635140867618,16.7448212310155,16.8582032419678,16.9568851477706,
16.9715272588334,16.9715852529202,17.0721615462789,17.081298932139,17.1923757902729,
17.3017952886031,17.4111512159923,17.5204844288647,17.6328417709509,17.7423248774763,
17.856119337343,17.9543118630367,17.9698514639413,17.9699137972097,18.0695556702309,
18.0792537650142,18.1903773370748,18.299407578028,18.4083695126169,18.5173046389224,
18.6300390645666,18.7391185616584,18.8536804515787,18.9523645764336,18.968207786416,
18.9682423414991,19.070122838832,19.0804139585051,19.1923473335779,19.3041416432842,
19.4158321105052,19.5274538174148,19.6390844118875,19.7507101321439,19.8624454103262,
19.9665708857883),.UNSPECIFIED.) ;
#1339 = B_SPLINE_CURVE_WITH_KNOTS('',3,(#56510,#56511,#56512,#56513,#56514,
#56515,#56516,#56517,#56518,#56519,#56520,#56521,#56522,#56523,#56524,#56525,
#56526,#56527,#56528,#56529,#56530,#56531,#56532,#56533,#56534,#56535,#56536,
#56537,#56538,#56539,#56540,#56541,#56542,#56543,#56544,#56545,#56546,#56547,
#56548,#56549,#56550,#56551,#56552,#56553,#56554,#56555,#56556,#56557,#56558,
#56559,#56560,#56561,#56562,#56563,#56564,#56565,#56566,#56567,#56568,#56569,
#56570,#56571,#56572,#56573,#56574,#56575,#56576,#56577,#56578,#56579,#56580,
#56581,#56582,#56583,#56584,#56585,#56586,#56587,#56588,#56589,#56590,#56591,
#56592,#56593,#56594,#56595,#56596,#56597,#56598,#56599,#56600,#56601,#56602,
#56603,#56604,#56605,#56606,#56607,#56608,#56609,#56610,#56611,#56612,#56613),
 .UNSPECIFIED.,.F.,.F.,(4,2,2,2,2,2,2,2,2,2,2,2,2,2,2,2,2,2,2,2,2,2,2,2,
2,2,2,2,2,2,2,2,2,2,2,2,2,2,2,2,2,2,2,2,2,2,2,2,2,2,2,4),(1.10920986980175,
1.11653740164681,1.13771123831766,1.16907366933029,1.18617897538512,1.19527680512883,
1.20788932723244,1.22583306009734,1.26361823026631,1.27906578579854,1.29658710580061,
1.31748720980365,1.35274550512533,1.36182087986681,1.3739898364051,1.39085974376577,
1.43148096289359,1.44663902389709,1.46451981315105,1.48629077793157,1.51895929967274,
1.52829235454364,1.53999383830962,1.55578141362031,1.59688701040672,1.61243501408099,
1.62969110733505,1.64997265934366,1.68525287030369,1.69476096474687,1.70607270300085,
1.7210004004899,1.76627501983604,1.78145697493476,1.80010059834877,1.84881182401862,
1.85960372224137,1.86933452340368,1.8810400885696,1.90948454784739,1.93419108950702,
1.94922498732281,1.96834389747161,1.99335689267842,2.01853610278449,2.02826757682473,
2.03921222740924,2.07090038355154,2.09901082443907,2.11438713698595,2.13260513630923,
2.15965741239705),.UNSPECIFIED.) ;
#1340 = B_SPLINE_CURVE_WITH_KNOTS('',3,(#56619,#56620,#56621,#56622,#56623,
#56624,#56625,#56626,#56627,#56628),.UNSPECIFIED.,.F.,.F.,(4,2,2,2,4),(0.000104245096920715,
0.0139017618315296,0.0231479761800173,0.0326957883926925,0.0589262539191868),
 .UNSPECIFIED.) ;
#1341 = B_SPLINE_CURVE_WITH_KNOTS('',3,(#56630,#56631,#56632,#56633,#56634,
#56635,#56636,#56637,#56638,#56639,#56640,#56641,#56642,#56643,#56644,#56645,
#56646,#56647,#56648,#56649,#56650,#56651,#56652,#56653,#56654,#56655,#56656,
#56657,#56658,#56659,#56660,#56661,#56662,#56663,#56664,#56665,#56666,#56667,
#56668,#56669,#56670,#56671,#56672,#56673,#56674,#56675,#56676,#56677,#56678,
#56679,#56680,#56681,#56682,#56683,#56684,#56685,#56686,#56687,#56688,#56689,
#56690,#56691,#56692,#56693,#56694,#56695,#56696,#56697,#56698,#56699,#56700,
#56701,#56702,#56703,#56704,#56705,#56706,#56707,#56708,#56709,#56710,#56711,
#56712,#56713,#56714,#56715,#56716,#56717,#56718,#56719,#56720,#56721,#56722,
#56723,#56724,#56725,#56726,#56727,#56728,#56729,#56730,#56731,#56732,#56733,
#56734,#56735,#56736,#56737,#56738,#56739,#56740,#56741,#56742,#56743,#56744,
#56745,#56746,#56747,#56748,#56749,#56750,#56751,#56752,#56753,#56754,#56755,
#56756,#56757,#56758,#56759),.UNSPECIFIED.,.F.,.F.,(4,3,3,3,3,3,3,3,3,3,
3,3,3,3,3,3,3,3,3,3,3,3,3,3,3,3,3,3,3,3,3,3,3,3,3,3,3,3,3,3,3,3,3,4),(-3.84638258862878,
-3.73821155326556,-3.63015790575673,-3.52217914496424,-3.41423251978327,
-3.30619919528476,-3.19812579616014,-3.08985237906168,-2.9950436281227,
-2.9949856328683,-2.89440933850989,-2.88527194896355,-2.77419509141547,
-2.66477558831422,-2.55541965612589,-2.4460864384266,-2.33372910096467,
-2.22424598956245,-2.11045153907066,-2.01225901005051,-1.99671942268382,
-1.99665708857887,-1.89701521204593,-1.8873171055871,-1.77619353542489,
-1.66716328029021,-1.55820133192825,-1.44926619227649,-1.33653178027973,
-1.22745227104431,-1.11289040766687,-1.01420626267801,-0.998363098870108,
-0.998328544289432,-0.896448042701214,-0.886156950979831,-0.774223599193483,
-0.662429312480799,-0.550738867904862,-0.439117183235771,-0.327486610177047,
-0.215860910885113,-0.104125652658588,-2.11597950287882E-13),
 .UNSPECIFIED.) ;
#1342 = B_SPLINE_CURVE_WITH_KNOTS('',3,(#56763,#56764,#56765,#56766,#56767,
#56768,#56769,#56770,#56771,#56772,#56773,#56774,#56775,#56776,#56777,#56778,
#56779,#56780,#56781,#56782,#56783,#56784,#56785,#56786,#56787,#56788,#56789,
#56790,#56791,#56792,#56793,#56794,#56795,#56796,#56797,#56798,#56799,#56800,
#56801,#56802,#56803,#56804,#56805,#56806,#56807,#56808,#56809,#56810,#56811,
#56812,#56813,#56814,#56815,#56816,#56817,#56818,#56819,#56820,#56821,#56822,
#56823,#56824,#56825,#56826,#56827,#56828,#56829,#56830,#56831,#56832,#56833,
#56834,#56835,#56836,#56837,#56838,#56839,#56840,#56841,#56842,#56843,#56844,
#56845,#56846,#56847,#56848,#56849,#56850,#56851,#56852,#56853,#56854,#56855,
#56856,#56857,#56858,#56859,#56860,#56861,#56862,#56863,#56864,#56865,#56866,
#56867,#56868,#56869,#56870,#56871,#56872,#56873,#56874,#56875,#56876,#56877,
#56878,#56879,#56880,#56881,#56882,#56883,#56884,#56885,#56886,#56887,#56888,
#56889,#56890,#56891,#56892,#56893,#56894,#56895,#56896,#56897,#56898,#56899,
#56900,#56901,#56902,#56903,#56904,#56905,#56906,#56907,#56908,#56909,#56910,
#56911,#56912,#56913,#56914,#56915,#56916,#56917,#56918,#56919,#56920,#56921,
#56922,#56923,#56924,#56925,#56926,#56927,#56928,#56929,#56930,#56931,#56932,
#56933,#56934,#56935,#56936,#56937,#56938,#56939,#56940,#56941,#56942,#56943,
#56944,#56945,#56946,#56947,#56948,#56949,#56950,#56951,#56952,#56953,#56954,
#56955,#56956,#56957,#56958,#56959,#56960,#56961),.UNSPECIFIED.,.F.,.F.,
(4,3,3,3,3,3,3,3,3,3,3,3,3,3,3,3,3,3,3,3,3,3,3,3,3,3,3,3,3,3,3,3,3,3,3,
3,3,3,3,3,3,3,3,3,3,3,3,3,3,3,3,3,3,3,3,3,3,3,3,3,3,3,3,3,3,3,4),(2.02817886070011,
2.12401440243833,2.23321226279834,2.34229878960224,2.45131549057795,2.56030377591627,
2.66938389525482,2.77850498459844,2.88783339337641,2.98608246080593,2.99492750212187,
2.99498563286828,3.09556180779865,3.10491922853353,3.21596859711155,3.32560312559594,
3.43517161345578,3.54471453327594,3.65686444424638,3.76654756863079,3.87993087289425,
3.97857719176355,3.99325940849771,3.9933141771577,4.09372024726719,4.10302947216521,
4.21410612832545,4.32351594885692,4.43285794107218,4.54217293183031,4.65454037923451,
4.7639945634008,4.87781864242396,4.97628500966465,4.9915889173842,4.99164272144712,
5.09203102228959,5.10141980278939,5.21248873565778,5.32196240779199,5.43136884125333,
5.5407487543607,5.65305438220467,5.76257391804421,5.87627259189038,5.97483109049847,
5.98991796320581,5.98997126573655,6.09040665155374,6.09976820578768,6.21083465631747,
6.32032936931871,6.42975723173439,6.53915893081329,6.65144415061646,6.7609861270978,
6.87464296856189,6.9731943976366,6.98824622069259,6.98829981002598,7.08940591454106,
7.09951438005358,7.21054286125676,7.32140077463895,7.43215901695895,7.54285993587725,
7.59300756235165),.UNSPECIFIED.) ;
#1343 = B_SPLINE_CURVE_WITH_KNOTS('',3,(#56962,#56963,#56964,#56965,#56966,
#56967,#56968,#56969),.UNSPECIFIED.,.F.,.F.,(4,2,2,4),(-1.10885368045049,
-1.08696980493825,-1.05541474700099,-1.05003427160778),.UNSPECIFIED.) ;
#1344 = B_SPLINE_CURVE_WITH_KNOTS('',3,(#56976,#56977,#56978,#56979,#56980,
#56981,#56982,#56983,#56984,#56985,#56986,#56987,#56988,#56989,#56990,#56991,
#56992,#56993,#56994,#56995,#56996,#56997,#56998,#56999,#57000,#57001,#57002,
#57003,#57004,#57005,#57006,#57007,#57008,#57009,#57010,#57011,#57012,#57013,
#57014,#57015,#57016,#57017,#57018),.UNSPECIFIED.,.F.,.F.,(4,3,3,3,3,3,
3,3,3,3,3,3,3,3,4),(-17.938079539449,-17.8425480409392,-17.7333410205706,
-17.6242453229645,-17.5152194418143,-17.4062219683227,-17.2971326783531,
-17.188002412777,-17.0786648957393,-16.9804176491229,-16.9716454844279,
-16.9715852529204,-16.8695606965042,-16.8587073643271,-16.7648915192752),
 .UNSPECIFIED.) ;
#1345 = B_SPLINE_CURVE_WITH_KNOTS('',3,(#57024,#57025,#57026,#57027,#57028,
#57029,#57030,#57031,#57032,#57033,#57034,#57035,#57036,#57037,#57038,#57039,
#57040,#57041,#57042,#57043,#57044,#57045,#57046,#57047,#57048,#57049,#57050,
#57051,#57052,#57053,#57054,#57055,#57056,#57057,#57058,#57059,#57060,#57061,
#57062,#57063,#57064,#57065,#57066,#57067,#57068,#57069,#57070,#57071,#57072,
#57073,#57074,#57075,#57076,#57077,#57078,#57079,#57080,#57081,#57082,#57083,
#57084,#57085,#57086,#57087,#57088,#57089,#57090,#57091,#57092,#57093,#57094,
#57095,#57096,#57097,#57098,#57099,#57100,#57101,#57102,#57103,#57104,#57105,
#57106,#57107,#57108,#57109,#57110,#57111,#57112,#57113,#57114,#57115,#57116,
#57117,#57118,#57119,#57120,#57121,#57122,#57123,#57124,#57125,#57126,#57127,
#57128,#57129,#57130,#57131,#57132,#57133,#57134,#57135,#57136,#57137,#57138,
#57139,#57140,#57141,#57142,#57143,#57144,#57145,#57146,#57147,#57148,#57149,
#57150,#57151,#57152,#57153,#57154,#57155,#57156,#57157,#57158,#57159,#57160,
#57161,#57162,#57163,#57164,#57165,#57166,#57167,#57168,#57169,#57170,#57171,
#57172,#57173,#57174,#57175,#57176,#57177,#57178,#57179,#57180,#57181,#57182,
#57183,#57184,#57185,#57186,#57187,#57188,#57189,#57190,#57191,#57192,#57193,
#57194,#57195,#57196,#57197,#57198,#57199,#57200,#57201,#57202,#57203,#57204,
#57205,#57206,#57207,#57208,#57209,#57210,#57211,#57212,#57213,#57214,#57215,
#57216,#57217,#57218,#57219,#57220,#57221,#57222),.UNSPECIFIED.,.F.,.F.,
(4,3,3,3,3,3,3,3,3,3,3,3,3,3,3,3,3,3,3,3,3,3,3,3,3,3,3,3,3,3,3,3,3,3,3,
3,3,3,3,3,3,3,3,3,3,3,3,3,3,3,3,3,3,3,3,3,3,3,3,3,3,3,3,3,3,3,4),(14.2294919259517,
14.3389381490702,14.4483292137904,14.5577058223085,14.6671878568696,14.776721974381,
14.8864627651101,14.9748739536409,14.9749281643414,15.0752587674523,15.0846370954552,
15.1957145471022,15.3051205991587,15.4144597976302,15.5237729697857,15.636143904497,
15.7455986944277,15.8594277015293,15.9579676391285,15.9732009683324,15.9732567086308,
16.0738029748843,16.0831962089879,16.1942448394794,16.3038831313914,16.4134545829914,
16.5229996713677,16.6351460667559,16.7448294089135,16.8582073309168,16.9568840398618,
16.9715251758643,16.9715852529202,17.0721638612044,17.0813079395613,17.1923836717674,
17.3018122533801,17.411177283829,17.520519617807,17.6328681626577,17.7423603933053,
17.8561370952575,17.9543359365701,17.9698500367431,17.9699137972097,18.0695597591183,
18.0792769675553,18.1903976392982,18.2994493704183,18.4084321055174,18.5173873144738,
18.6301010712301,18.7391986507741,18.8537204961366,18.9524367761661,18.9682086314664,
18.9682423414991,19.0701304113359,19.0803756098126,19.1922713484363,19.3040285239676,
19.415682447892,19.5272682918946,19.6388643971447,19.7504563748751,19.8621595718363,
19.9665708857883),.UNSPECIFIED.) ;
#1346 = B_SPLINE_CURVE_WITH_KNOTS('',3,(#57224,#57225,#57226,#57227,#57228,
#57229,#57230,#57231,#57232,#57233,#57234,#57235,#57236,#57237,#57238,#57239,
#57240,#57241,#57242,#57243,#57244,#57245,#57246,#57247,#57248,#57249,#57250,
#57251,#57252,#57253,#57254,#57255,#57256,#57257,#57258,#57259,#57260,#57261,
#57262,#57263,#57264,#57265,#57266,#57267,#57268,#57269,#57270,#57271,#57272,
#57273,#57274,#57275,#57276,#57277,#57278,#57279,#57280,#57281,#57282,#57283,
#57284,#57285,#57286,#57287,#57288,#57289,#57290,#57291,#57292,#57293,#57294,
#57295,#57296,#57297,#57298,#57299,#57300,#57301,#57302,#57303,#57304,#57305,
#57306,#57307,#57308,#57309,#57310,#57311,#57312,#57313,#57314,#57315,#57316,
#57317,#57318,#57319,#57320,#57321,#57322,#57323,#57324,#57325),
 .UNSPECIFIED.,.F.,.F.,(4,2,2,2,2,2,2,2,2,2,2,2,2,2,2,2,2,2,2,2,2,2,2,2,
2,2,2,2,2,2,2,2,2,2,2,2,2,2,2,2,2,2,2,2,2,2,2,2,2,2,4),(1.10894604130966,
1.11627336363691,1.13744845361287,1.16882272821857,1.18590494333013,1.19499960459813,
1.20762946026794,1.22561879302956,1.26326981320216,1.27872261588766,1.29623077539129,
1.31710179780014,1.3524222080599,1.36149198082141,1.37368390575001,1.39061053417187,
1.43106308715466,1.44622844891658,1.46408529560854,1.4858009244646,1.51858805580375,
1.52791156434614,1.53964154921547,1.55549588654148,1.59639725374685,1.6119563226357,
1.62918243733498,1.64939828671883,1.68486297139135,1.69435047401396,1.70571168392109,
1.72074904504411,1.7652272488211,1.78046325505563,1.79874084752736,1.85028822390102,
1.86025453118219,1.87073306078469,1.90215593343046,1.93149459367087,1.94659576105821,
1.96424361239819,1.98550925177549,2.01975587604291,2.02890229557161,2.04093901561324,
2.05745505594631,2.09872531277398,2.11406288297816,2.13250330112224,2.15906108059027),
 .UNSPECIFIED.) ;
#1347 = B_SPLINE_CURVE_WITH_KNOTS('',3,(#57331,#57332,#57333,#57334,#57335,
#57336,#57337,#57338,#57339,#57340),.UNSPECIFIED.,.F.,.F.,(4,2,2,2,4),(0.000105126802572485,
0.014031716210766,0.0233742014449894,0.0330434563056765,0.0589148629143721),
 .UNSPECIFIED.) ;
#1348 = B_SPLINE_CURVE_WITH_KNOTS('',3,(#57342,#57343,#57344,#57345,#57346,
#57347,#57348,#57349,#57350,#57351,#57352,#57353,#57354,#57355,#57356,#57357,
#57358,#57359,#57360,#57361,#57362,#57363,#57364,#57365,#57366,#57367,#57368,
#57369,#57370,#57371,#57372,#57373,#57374,#57375,#57376,#57377,#57378,#57379,
#57380,#57381,#57382,#57383,#57384,#57385,#57386,#57387,#57388,#57389,#57390,
#57391,#57392,#57393,#57394,#57395,#57396,#57397,#57398,#57399,#57400,#57401,
#57402,#57403,#57404,#57405,#57406,#57407,#57408,#57409,#57410,#57411,#57412,
#57413,#57414,#57415,#57416,#57417,#57418,#57419,#57420,#57421,#57422,#57423,
#57424,#57425,#57426,#57427,#57428,#57429,#57430,#57431,#57432,#57433,#57434,
#57435,#57436,#57437,#57438,#57439,#57440,#57441,#57442,#57443,#57444,#57445,
#57446,#57447,#57448,#57449,#57450,#57451,#57452,#57453,#57454,#57455,#57456,
#57457,#57458,#57459,#57460,#57461,#57462,#57463,#57464,#57465,#57466,#57467,
#57468,#57469,#57470,#57471),.UNSPECIFIED.,.F.,.F.,(4,3,3,3,3,3,3,3,3,3,
3,3,3,3,3,3,3,3,3,3,3,3,3,3,3,3,3,3,3,3,3,3,3,3,3,3,3,3,3,3,3,3,3,4),(-3.84638256813386,
-3.73820850425281,-3.63015156663993,-3.52216926327145,-3.41421884243916,
-3.30618133487243,-3.19810353321684,-3.08982537936042,-2.99504571094475,
-2.9949856328683,-2.89440702304788,-2.88526294147605,-2.77418720986391,
-2.66475862349703,-2.55539358829796,-2.44605124957496,-2.33370270932594,
-2.22421047397042,-2.11043378127464,-2.01223493666377,-1.99672084972804,
-1.99665708857887,-1.89701112545988,-1.88729390833867,-1.77617323783252,
-1.66712149763544,-1.5581387537861,-1.44918353641828,-1.33646978838607,
-1.22737220136461,-1.11285037282702,-1.01413407829555,-0.998362253922141,
-0.998328544289434,-0.896440470790495,-0.886195293396442,-0.774299571846485,
-0.662542413147004,-0.550888505773211,-0.439302677999796,-0.327706588337476,
-0.216114625846442,-0.104411443356276,-5.31522163870105E-13),
 .UNSPECIFIED.) ;
#1349 = B_SPLINE_CURVE_WITH_KNOTS('',3,(#57475,#57476,#57477,#57478,#57479,
#57480,#57481,#57482,#57483,#57484,#57485,#57486,#57487,#57488,#57489,#57490,
#57491,#57492,#57493,#57494,#57495,#57496,#57497,#57498,#57499,#57500,#57501,
#57502,#57503,#57504,#57505,#57506,#57507,#57508,#57509,#57510,#57511,#57512,
#57513,#57514,#57515,#57516,#57517,#57518,#57519,#57520,#57521,#57522,#57523,
#57524,#57525,#57526,#57527,#57528,#57529,#57530,#57531,#57532,#57533,#57534,
#57535,#57536,#57537,#57538,#57539,#57540,#57541,#57542,#57543,#57544,#57545,
#57546,#57547,#57548,#57549,#57550,#57551,#57552,#57553,#57554,#57555,#57556,
#57557,#57558,#57559,#57560,#57561,#57562,#57563,#57564,#57565,#57566,#57567,
#57568,#57569,#57570,#57571,#57572,#57573,#57574,#57575,#57576,#57577,#57578,
#57579,#57580,#57581,#57582,#57583,#57584,#57585,#57586,#57587,#57588,#57589,
#57590,#57591,#57592,#57593,#57594,#57595,#57596,#57597,#57598,#57599,#57600,
#57601,#57602,#57603,#57604,#57605,#57606,#57607,#57608,#57609,#57610,#57611,
#57612,#57613,#57614,#57615,#57616,#57617,#57618,#57619,#57620,#57621,#57622,
#57623,#57624,#57625,#57626,#57627,#57628,#57629,#57630,#57631,#57632,#57633,
#57634,#57635,#57636,#57637,#57638,#57639,#57640,#57641,#57642,#57643,#57644,
#57645,#57646,#57647,#57648,#57649,#57650,#57651,#57652,#57653,#57654,#57655,
#57656,#57657,#57658,#57659,#57660,#57661,#57662,#57663,#57664,#57665,#57666,
#57667,#57668,#57669,#57670,#57671,#57672,#57673),.UNSPECIFIED.,.F.,.F.,
(4,3,3,3,3,3,3,3,3,3,3,3,3,3,3,3,3,3,3,3,3,3,3,3,3,3,3,3,3,3,3,3,3,3,3,
3,3,3,3,3,3,3,3,3,3,3,3,3,3,3,3,3,3,3,3,3,3,3,3,3,3,3,3,3,3,3,4),(2.02849119681895,
2.12402284058456,2.23322985623704,2.34232554910588,2.45135142549916,2.56034889421509,
2.66943817939672,2.77856844017022,2.8879059524223,2.98615319978999,2.99492540240048,
2.99498563286828,3.09555793178458,3.1049227617298,3.21597168865829,3.32560899891808,
3.43517998953789,3.54472513678483,3.65687239687805,3.76655707843461,3.87993562779616,
3.97858788803385,3.99325823756284,3.99331417715771,4.09371916216987,4.10302808104315,
4.21410491109365,4.32351302343983,4.43285319274963,4.54216624802883,4.65453536638341,
4.76398735355505,4.87781503750109,4.97628194727701,4.99158851592506,4.99164272144713,
5.09202984908505,5.10141645669967,5.21248580782928,5.32195615323443,5.43135927257129,
5.5407358864701,5.65304473128672,5.76256102779188,5.87626614676422,5.97482204959029,
5.98991768793335,5.98997126573656,6.0904063371316,6.0997675247197,6.21083406038298,
6.32032822177535,6.42975558054475,6.53915682320765,6.65144256991223,6.76098420489217,
6.87464200745908,6.97319267264661,6.98824579430711,6.98829981002598,7.0894064044638,
7.099515038111,7.21054420905378,7.32140285463792,7.43216185294655,7.54286355851905,
7.59300756235355),.UNSPECIFIED.) ;
#1350 = B_SPLINE_CURVE_WITH_KNOTS('',3,(#57674,#57675,#57676,#57677,#57678,
#57679,#57680,#57681),.UNSPECIFIED.,.F.,.F.,(4,2,2,4),(-1.10883530707003,
-1.08691376692716,-1.0553640497396,-1.05001965519088),.UNSPECIFIED.) ;
#1351 = B_SPLINE_CURVE_WITH_KNOTS('',3,(#57687,#57688,#57689,#57690,#57691,
#57692,#57693,#57694,#57695,#57696,#57697,#57698,#57699,#57700,#57701,#57702,
#57703,#57704,#57705,#57706,#57707,#57708,#57709,#57710,#57711,#57712),
 .UNSPECIFIED.,.F.,.F.,(4,2,2,2,2,2,2,2,2,2,2,2,4),(0.459092828659847,0.46458280938324,
0.505879393319841,0.521008735046651,0.529991319325623,0.542633449959227,
0.575929685166336,0.614621897851766,0.632497588871837,0.649228900547743,
0.666866115107942,0.722578742135439,0.732479068875876),.UNSPECIFIED.) ;
#1352 = B_SPLINE_CURVE_WITH_KNOTS('',3,(#57715,#57716,#57717,#57718,#57719,
#57720,#57721,#57722,#57723,#57724,#57725,#57726,#57727,#57728,#57729,#57730,
#57731,#57732,#57733,#57734,#57735,#57736,#57737,#57738,#57739,#57740,#57741,
#57742,#57743,#57744,#57745,#57746,#57747,#57748,#57749,#57750),
 .UNSPECIFIED.,.F.,.F.,(4,2,2,2,2,2,2,2,2,2,2,2,2,2,2,2,2,4),(0.000333295488794572,
0.00533169420316919,0.0119863859187359,0.048691939483201,0.0844017923136275,
0.100356581500467,0.116281319030886,0.149692705305946,0.1783076015109,0.190742024534847,
0.201078659920755,0.210405171548014,0.232103074145979,0.282226565630108,
0.300212219360226,0.315193011616712,0.337127704802259,0.381140802024926),
 .UNSPECIFIED.) ;
#1353 = B_SPLINE_CURVE_WITH_KNOTS('',3,(#57756,#57757,#57758,#57759,#57760,
#57761,#57762,#57763,#57764,#57765,#57766,#57767,#57768,#57769,#57770,#57771,
#57772,#57773,#57774,#57775,#57776,#57777,#57778,#57779,#57780,#57781,#57782,
#57783,#57784,#57785,#57786,#57787,#57788,#57789,#57790,#57791,#57792,#57793,
#57794,#57795,#57796,#57797,#57798,#57799,#57800,#57801,#57802,#57803,#57804,
#57805,#57806,#57807,#57808,#57809,#57810,#57811,#57812,#57813,#57814,#57815,
#57816,#57817,#57818,#57819,#57820,#57821,#57822,#57823,#57824,#57825,#57826,
#57827,#57828,#57829,#57830,#57831,#57832,#57833),.UNSPECIFIED.,.F.,.F.,
(4,2,2,2,2,2,2,2,2,2,2,2,2,2,2,2,2,2,2,2,2,2,2,2,2,2,2,2,2,2,2,2,2,2,2,
2,2,2,4),(1.29359361912601,1.30106987292448,1.31750403155353,1.33306635135568,
1.36187428370035,1.40299397077918,1.41701197002479,1.42577387270662,1.43884531163003,
1.45667948572154,1.50738242336099,1.52363298492541,1.53932799920826,1.57014056486922,
1.61063065145667,1.623517366373,1.63229811331715,1.64661281546571,1.66734113986291,
1.71288214330797,1.7290835487098,1.74478576388706,1.77584413634624,1.81632835476311,
1.82912521118274,1.83788291242882,1.85217474358337,1.87285804431839,1.9184471776329,
1.93458554047298,1.95018735587936,1.9803875670598,2.02133212904445,2.03461501728283,
2.04340752395374,2.05733245183337,2.07707132400357,2.11467829361035,2.12882907516074),
 .UNSPECIFIED.) ;
#1354 = B_SPLINE_CURVE_WITH_KNOTS('',3,(#57834,#57835,#57836,#57837,#57838,
#57839,#57840,#57841,#57842,#57843,#57844,#57845,#57846,#57847,#57848,#57849,
#57850,#57851,#57852,#57853,#57854,#57855,#57856,#57857,#57858,#57859,#57860,
#57861,#57862,#57863,#57864,#57865,#57866,#57867,#57868,#57869,#57870,#57871,
#57872,#57873,#57874,#57875),.UNSPECIFIED.,.F.,.F.,(4,2,2,2,2,2,2,2,2,2,
2,2,2,2,2,2,2,2,2,2,4),(0.000734533073629474,0.0138790511024117,0.0296566148513827,
0.0802346251044167,0.106665857315606,0.116373796810632,0.126501899960165,
0.164778388123386,0.201300657865272,0.217475187060577,0.233584299088167,
0.267597394367349,0.296198479539202,0.313243933653704,0.322093358567795,
0.332453617478739,0.366407046245808,0.408190077661704,0.424914882262875,
0.439911329919575,0.459092828659847),.UNSPECIFIED.) ;
#1355 = B_SPLINE_CURVE_WITH_KNOTS('',3,(#57876,#57877,#57878,#57879,#57880,
#57881,#57882,#57883,#57884,#57885,#57886,#57887,#57888,#57889,#57890,#57891,
#57892,#57893,#57894,#57895,#57896,#57897,#57898,#57899,#57900,#57901,#57902,
#57903,#57904,#57905,#57906,#57907,#57908,#57909,#57910,#57911,#57912,#57913,
#57914,#57915,#57916,#57917,#57918,#57919,#57920,#57921,#57922,#57923,#57924,
#57925,#57926,#57927,#57928,#57929,#57930,#57931,#57932,#57933,#57934,#57935,
#57936,#57937,#57938,#57939,#57940,#57941,#57942,#57943,#57944,#57945,#57946,
#57947,#57948,#57949,#57950,#57951,#57952,#57953,#57954,#57955,#57956,#57957,
#57958,#57959,#57960,#57961,#57962,#57963,#57964,#57965,#57966,#57967,#57968,
#57969,#57970,#57971,#57972,#57973,#57974,#57975,#57976,#57977,#57978,#57979,
#57980,#57981,#57982,#57983,#57984,#57985,#57986,#57987,#57988,#57989,#57990,
#57991,#57992,#57993),.UNSPECIFIED.,.F.,.F.,(4,2,2,2,2,2,2,2,2,2,2,2,2,
2,2,2,2,2,2,2,2,2,2,2,2,2,2,2,2,2,2,2,2,2,2,2,2,2,2,2,2,2,2,2,2,2,2,2,2,
2,2,2,2,2,2,2,2,2,4),(9.9999999739413E-7,0.0160738874198969,0.0243015288141959,
0.0331995744590351,0.0509725032934508,0.0913818065799422,0.111457641442597,
0.127727564529213,0.143078744774428,0.170817330016844,0.20581943179008,
0.219335709806031,0.230254102060281,0.239265195718039,0.257369449100544,
0.297791259046865,0.317949924898833,0.334051303539227,0.349654113706522,
0.404856472005175,0.428706238735585,0.438214816383149,0.448294410421727,
0.48701762271562,0.521794091712671,0.53832480323903,0.553696441310369,0.580724198831505,
0.616695673361533,0.630366418165186,0.641370973970987,0.650377376883583,
0.668310842685775,0.708820817694532,0.72899296528574,0.745097716403503,
0.760716399539172,0.815957566093128,0.839872655156268,0.849381354834161,
0.85942268120762,0.89860037183343,0.935662834432564,0.951546389770785,0.967363065175678,
1.01717070951904,1.03632569817519,1.04996676214464,1.05867044847102,1.0718550912914,
1.11255678435931,1.14271858391255,1.15830493726752,1.17446102876239,1.22539811312515,
1.25082901670304,1.26043620180714,1.270367123206,1.29395065554619),
 .UNSPECIFIED.) ;
#1356 = B_SPLINE_CURVE_WITH_KNOTS('',3,(#57999,#58000,#58001,#58002,#58003,
#58004,#58005,#58006,#58007,#58008,#58009,#58010,#58011,#58012,#58013,#58014,
#58015,#58016,#58017,#58018,#58019,#58020,#58021,#58022,#58023,#58024,#58025,
#58026,#58027,#58028,#58029,#58030,#58031,#58032,#58033,#58034,#58035,#58036,
#58037,#58038,#58039,#58040,#58041,#58042,#58043,#58044,#58045,#58046,#58047,
#58048,#58049,#58050,#58051,#58052,#58053,#58054,#58055,#58056,#58057,#58058,
#58059,#58060,#58061,#58062,#58063,#58064,#58065,#58066,#58067,#58068,#58069,
#58070,#58071,#58072,#58073,#58074,#58075,#58076,#58077,#58078,#58079,#58080,
#58081,#58082,#58083,#58084,#58085,#58086,#58087,#58088,#58089),
 .UNSPECIFIED.,.F.,.F.,(4,3,3,3,3,3,3,3,3,3,3,3,3,3,3,3,3,3,3,3,3,3,3,3,
3,3,3,3,3,3,4),(15.7079632679487,15.8113185661092,15.9146477682657,16.0179862497935,
16.1214445336244,16.2249671723021,16.3224787353659,16.3286854519248,16.3947463489873,
16.394798101356,16.4893686487847,16.4989555611429,16.6029531946589,16.7068224059803,
16.8106222565616,16.9143876724686,17.0181535323515,17.122023334568,17.2259490949981,
17.3243546278831,17.3300536422211,17.3930765924381,17.3931266456453,17.4881585315426,
17.4974456208808,17.6010533743386,17.6065584824799,17.7106015728288,17.8145755365523,
17.9185210511146,17.9338970672771),.UNSPECIFIED.) ;
#1357 = B_SPLINE_CURVE_WITH_KNOTS('',3,(#58091,#58092,#58093,#58094,#58095,
#58096,#58097,#58098,#58099,#58100,#58101,#58102,#58103,#58104,#58105,#58106,
#58107,#58108,#58109,#58110,#58111,#58112,#58113,#58114,#58115,#58116,#58117,
#58118,#58119,#58120,#58121,#58122,#58123,#58124,#58125,#58126,#58127,#58128,
#58129,#58130),.UNSPECIFIED.,.F.,.F.,(4,3,3,3,3,3,3,3,3,3,3,3,3,4),(14.3981410127773,
14.5041275779632,14.6100285359095,14.7158970806972,14.8217531608633,14.9276267469892,
15.0335478199294,15.1396253540428,15.2457909511983,15.3521586464516,15.3964695570666,
15.5189994551258,15.6402222711559,15.7079554221965),.UNSPECIFIED.) ;
#1358 = B_SPLINE_CURVE_WITH_KNOTS('',3,(#58133,#58134,#58135,#58136,#58137,
#58138,#58139,#58140,#58141,#58142,#58143,#58144,#58145,#58146,#58147,#58148,
#58149,#58150,#58151,#58152,#58153,#58154,#58155,#58156,#58157,#58158,#58159,
#58160,#58161,#58162,#58163,#58164,#58165,#58166,#58167,#58168,#58169,#58170,
#58171,#58172,#58173,#58174,#58175,#58176,#58177,#58178,#58179,#58180,#58181,
#58182,#58183,#58184,#58185,#58186,#58187,#58188,#58189,#58190,#58191,#58192,
#58193,#58194,#58195,#58196,#58197,#58198,#58199,#58200,#58201,#58202,#58203,
#58204,#58205,#58206,#58207,#58208,#58209,#58210),.UNSPECIFIED.,.F.,.F.,
(4,2,2,2,2,2,2,2,2,2,2,2,2,2,2,2,2,2,2,2,2,2,2,2,2,2,2,2,2,2,2,2,2,2,2,
2,2,2,4),(9.11640338329011E-5,0.0051025466412606,0.0113875670523336,0.0548470562170383,
0.0857482806918087,0.101417815155263,0.117653019630782,0.166957731175739,
0.192706981078215,0.202333248824673,0.212252232765116,0.252876439023877,
0.277779339804877,0.297584062449989,0.312468457507578,0.331838238059752,
0.375873450570578,0.398590164456944,0.408032189351106,0.418096415804966,
0.430099242590052,0.456627998374622,0.494015251410843,0.5098507658762,0.525317201277499,
0.55584552958573,0.596302274316993,0.609196791407187,0.617827198975333,
0.631448481288996,0.650604889682355,0.700320208050008,0.716058185493827,
0.731770099253375,0.766102498367211,0.808240308785967,0.818255737119278,
0.826146810363654,0.835757597382848),.UNSPECIFIED.) ;
#1359 = B_SPLINE_CURVE_WITH_KNOTS('',3,(#58216,#58217,#58218,#58219,#58220,
#58221,#58222,#58223,#58224,#58225,#58226,#58227,#58228,#58229,#58230,#58231,
#58232,#58233,#58234,#58235,#58236,#58237,#58238,#58239,#58240,#58241),
 .UNSPECIFIED.,.F.,.F.,(4,2,2,2,2,2,2,2,2,2,2,2,4),(0.459101110943174,0.464354084783774,
0.505377027644394,0.520997705906278,0.529963645940253,0.542471817233919,
0.575280333026665,0.614901030815203,0.632766276068313,0.649542615135927,
0.667261331011091,0.72253469686435,0.732483173568347),.UNSPECIFIED.) ;
#1360 = B_SPLINE_CURVE_WITH_KNOTS('',3,(#58244,#58245,#58246,#58247,#58248,
#58249,#58250,#58251,#58252,#58253,#58254,#58255,#58256,#58257,#58258,#58259,
#58260,#58261,#58262,#58263,#58264,#58265,#58266,#58267,#58268,#58269,#58270,
#58271,#58272,#58273,#58274,#58275,#58276,#58277,#58278,#58279),
 .UNSPECIFIED.,.F.,.F.,(4,2,2,2,2,2,2,2,2,2,2,2,2,2,2,2,2,4),(0.000327211641307999,
0.00531276958370105,0.011942178793651,0.0491171206788442,0.0844907768687678,
0.100422340388374,0.116322911773884,0.149510046624113,0.178269548979332,
0.190729453077571,0.201079787432153,0.210407580488322,0.232088112343222,
0.282131222632167,0.300112650559163,0.315080422309398,0.336959281230109,
0.381143861704028),.UNSPECIFIED.) ;
#1361 = B_SPLINE_CURVE_WITH_KNOTS('',3,(#58285,#58286,#58287,#58288,#58289,
#58290,#58291,#58292,#58293,#58294,#58295,#58296,#58297,#58298,#58299,#58300,
#58301,#58302,#58303,#58304,#58305,#58306,#58307,#58308,#58309,#58310,#58311,
#58312,#58313,#58314,#58315,#58316,#58317,#58318,#58319,#58320,#58321,#58322,
#58323,#58324,#58325,#58326,#58327,#58328,#58329,#58330,#58331,#58332,#58333,
#58334,#58335,#58336,#58337,#58338,#58339,#58340,#58341,#58342,#58343,#58344,
#58345,#58346,#58347,#58348,#58349,#58350,#58351,#58352,#58353,#58354,#58355,
#58356,#58357,#58358,#58359,#58360,#58361,#58362),.UNSPECIFIED.,.F.,.F.,
(4,2,2,2,2,2,2,2,2,2,2,2,2,2,2,2,2,2,2,2,2,2,2,2,2,2,2,2,2,2,2,2,2,2,2,
2,2,2,4),(1.29362987758487,1.30089907076155,1.31737875058471,1.3329043258506,
1.36124830246446,1.40248211826036,1.41681275265866,1.42558201814846,1.43839619816745,
1.45567241916341,1.5097097437419,1.52544352982289,1.54163064892364,1.56182405576991,
1.60248744352981,1.62033145379943,1.62928220105769,1.64040671981978,1.65427714699489,
1.69156480647918,1.71735948797143,1.73253846774084,1.74936390666995,1.76804611359679,
1.81102421322096,1.82682871782048,1.83567257446723,1.84753935964157,1.88074677457094,
1.91928590673729,1.93521642888214,1.9509776165905,1.98422212626801,2.02765785097719,
2.03789161381674,2.04743919730058,2.0707566216888,2.1163762040201,2.12870581412763),
 .UNSPECIFIED.) ;
#1362 = B_SPLINE_CURVE_WITH_KNOTS('',3,(#58363,#58364,#58365,#58366,#58367,
#58368,#58369,#58370,#58371,#58372,#58373,#58374,#58375,#58376,#58377,#58378,
#58379,#58380,#58381,#58382,#58383,#58384,#58385,#58386,#58387,#58388,#58389,
#58390,#58391,#58392,#58393,#58394,#58395,#58396,#58397,#58398,#58399,#58400,
#58401,#58402,#58403,#58404),.UNSPECIFIED.,.F.,.F.,(4,2,2,2,2,2,2,2,2,2,
2,2,2,2,2,2,2,2,2,2,4),(0.000739397909415687,0.0138412325044495,0.0295352759641673,
0.0792037035965399,0.106541526696309,0.116294270869245,0.126382320725574,
0.165125340584505,0.201321192902339,0.217459634847154,0.233555712978872,
0.267479454618907,0.296223261584647,0.313312125494654,0.322158943272101,
0.332516024622701,0.366427842431594,0.408040859835102,0.424741542140745,
0.439725818137328,0.459101110943174),.UNSPECIFIED.) ;
#1363 = B_SPLINE_CURVE_WITH_KNOTS('',3,(#58405,#58406,#58407,#58408,#58409,
#58410,#58411,#58412,#58413,#58414,#58415,#58416,#58417,#58418,#58419,#58420,
#58421,#58422,#58423,#58424,#58425,#58426,#58427,#58428,#58429,#58430,#58431,
#58432,#58433,#58434,#58435,#58436,#58437,#58438,#58439,#58440,#58441,#58442,
#58443,#58444,#58445,#58446,#58447,#58448,#58449,#58450,#58451,#58452,#58453,
#58454,#58455,#58456,#58457,#58458,#58459,#58460,#58461,#58462,#58463,#58464,
#58465,#58466,#58467,#58468,#58469,#58470,#58471,#58472,#58473,#58474,#58475,
#58476,#58477,#58478,#58479,#58480,#58481,#58482,#58483,#58484,#58485,#58486,
#58487,#58488,#58489,#58490,#58491,#58492,#58493,#58494,#58495,#58496,#58497,
#58498,#58499,#58500,#58501,#58502,#58503,#58504,#58505,#58506,#58507,#58508,
#58509,#58510,#58511,#58512,#58513,#58514,#58515,#58516,#58517,#58518,#58519,
#58520),.UNSPECIFIED.,.F.,.F.,(4,2,2,2,2,2,2,2,2,2,2,2,2,2,2,2,2,2,2,2,
2,2,2,2,2,2,2,2,2,2,2,2,2,2,2,2,2,2,2,2,2,2,2,2,2,2,2,2,2,2,2,2,2,2,2,2,
2,4),(1.0000000227918E-6,0.016150234256278,0.0243635252181724,0.0333737690104111,
0.0514110440662363,0.0918108935996449,0.111922267913714,0.128057346526151,
0.143494986960628,0.172393810303427,0.206237998757624,0.219576650432681,
0.23039822943815,0.239439859401816,0.257874384261227,0.297938597922265,
0.318067340872359,0.334141819533777,0.3497721960782,0.40436017980479,0.428614839934304,
0.438149900351881,0.448189395863537,0.487401859487926,0.523758810157126,
0.53978852569054,0.555476142512416,0.609030315051042,0.634063864344299,
0.643645826385148,0.653599569332248,0.693758198031548,0.730119447399353,
0.745976834881271,0.761797529179021,0.791625082917581,0.823689745585661,
0.841721547803439,0.850732235107347,0.861699880985403,0.911297282661011,
0.938339273537299,0.953703949654931,0.970223302942397,1.01736770922379,
1.03638319681025,1.04996207192976,1.05866165389312,1.07189242424699,1.11261372824132,
1.14267376817757,1.15824847834276,1.17440513574077,1.22525734750247,1.25071900847628,
1.26032500820491,1.27024816493027,1.2938343569962),.UNSPECIFIED.) ;
#1364 = B_SPLINE_CURVE_WITH_KNOTS('',3,(#58526,#58527,#58528,#58529,#58530,
#58531,#58532,#58533,#58534,#58535,#58536,#58537,#58538,#58539,#58540,#58541,
#58542,#58543,#58544,#58545,#58546,#58547,#58548,#58549,#58550,#58551,#58552,
#58553,#58554,#58555,#58556,#58557,#58558,#58559,#58560,#58561,#58562,#58563,
#58564,#58565,#58566,#58567,#58568,#58569,#58570,#58571,#58572,#58573,#58574,
#58575,#58576,#58577,#58578,#58579,#58580,#58581,#58582,#58583,#58584,#58585,
#58586,#58587,#58588,#58589,#58590,#58591,#58592,#58593,#58594,#58595,#58596,
#58597,#58598,#58599,#58600,#58601,#58602,#58603,#58604,#58605,#58606,#58607,
#58608,#58609,#58610,#58611,#58612,#58613,#58614,#58615,#58616),
 .UNSPECIFIED.,.F.,.F.,(4,3,3,3,3,3,3,3,3,3,3,3,3,3,3,3,3,3,3,3,3,3,3,3,
3,3,3,3,3,3,4),(15.7079632679487,15.811298560919,15.9146070461799,16.0179241280816,
16.1213600993717,16.2248598840742,16.3223793192546,16.3285546604084,16.3947472862124,
16.3947981013537,16.4893612956316,16.4989474321208,16.6029368813412,16.7067978361585,
16.8105893856834,16.9143464584217,17.0181039354167,17.1219653241399,17.2258826400782,
17.3242930388564,17.3299787615837,17.3930781390119,17.3931266456432,17.4881609860694,
17.4974415964232,17.6010536984685,17.6065544877355,17.7105941015318,17.814564776613,
17.9185072616035,17.9338931616724),.UNSPECIFIED.) ;
#1365 = B_SPLINE_CURVE_WITH_KNOTS('',3,(#58618,#58619,#58620,#58621,#58622,
#58623,#58624,#58625,#58626,#58627,#58628,#58629,#58630,#58631,#58632,#58633,
#58634,#58635,#58636,#58637,#58638,#58639,#58640,#58641,#58642,#58643,#58644,
#58645,#58646,#58647,#58648,#58649,#58650,#58651,#58652,#58653,#58654,#58655,
#58656,#58657),.UNSPECIFIED.,.F.,.F.,(4,3,3,3,3,3,3,3,3,3,3,3,3,4),(14.3981410127747,
14.5041514455698,14.6100772086715,14.7159717739477,14.8218545927831,14.9277555738488,
15.0337046369196,15.1398108276545,15.2460054861428,15.3524025388386,15.3964695570642,
15.519015734404,15.6402459361385,15.7079553921828),.UNSPECIFIED.) ;
#1366 = B_SPLINE_CURVE_WITH_KNOTS('',3,(#58660,#58661,#58662,#58663,#58664,
#58665,#58666,#58667,#58668,#58669,#58670,#58671,#58672,#58673,#58674,#58675,
#58676,#58677,#58678,#58679,#58680,#58681,#58682,#58683,#58684,#58685,#58686,
#58687,#58688,#58689,#58690,#58691,#58692,#58693,#58694,#58695,#58696,#58697,
#58698,#58699,#58700,#58701,#58702,#58703,#58704,#58705,#58706,#58707,#58708,
#58709,#58710,#58711,#58712,#58713,#58714,#58715,#58716,#58717,#58718,#58719,
#58720,#58721,#58722,#58723,#58724,#58725,#58726,#58727,#58728,#58729,#58730,
#58731,#58732,#58733),.UNSPECIFIED.,.F.,.F.,(4,2,2,2,2,2,2,2,2,2,2,2,2,
2,2,2,2,2,2,2,2,2,2,2,2,2,2,2,2,2,2,2,2,2,2,2,4),(8.9593587986984E-5,0.00952093609751188,
0.0633488659849307,0.0834941189489905,0.099655415189997,0.115334705893301,
0.167927086572246,0.192896620540458,0.202477430415909,0.212461292430139,
0.252316259026952,0.277477254805576,0.297385234412671,0.312258519839811,
0.331492489948905,0.375621279613763,0.398601940600346,0.408056006597219,
0.418087133787787,0.451228293324594,0.491755232729443,0.508170422783087,
0.523289133651666,0.549016933433626,0.593139017551487,0.607852077954839,
0.616524557735506,0.628609638320433,0.661720602807763,0.699769801191,0.715631535074734,
0.731230302036858,0.763097776354719,0.808060373537215,0.818141454642955,
0.826088585101868,0.835762250436862),.UNSPECIFIED.) ;
#1367 = B_SPLINE_CURVE_WITH_KNOTS('',3,(#58740,#58741,#58742,#58743,#58744,
#58745,#58746,#58747,#58748,#58749,#58750,#58751,#58752,#58753,#58754,#58755,
#58756,#58757,#58758,#58759,#58760,#58761,#58762,#58763,#58764,#58765,#58766,
#58767,#58768,#58769,#58770,#58771,#58772,#58773,#58774,#58775,#58776,#58777,
#58778,#58779,#58780,#58781,#58782),.UNSPECIFIED.,.F.,.F.,(4,3,3,3,3,3,
3,3,3,3,3,3,3,3,4),(-17.9381511473345,-17.8425500608732,-17.7333452660566,
-17.6242518023618,-17.5152281629583,-17.4062329385398,-17.2971459013018,
-17.188017894178,-17.0786826257273,-16.9804349880921,-16.9716449904015,
-16.9715852529217,-16.8695605066972,-16.8587096350255,-16.7648949639448),
 .UNSPECIFIED.) ;
#1368 = B_SPLINE_CURVE_WITH_KNOTS('',3,(#58788,#58789,#58790,#58791,#58792,
#58793,#58794,#58795,#58796,#58797,#58798,#58799,#58800,#58801,#58802,#58803,
#58804,#58805,#58806,#58807,#58808,#58809,#58810,#58811,#58812,#58813,#58814,
#58815,#58816,#58817,#58818,#58819,#58820,#58821,#58822,#58823,#58824,#58825,
#58826,#58827,#58828,#58829,#58830,#58831,#58832,#58833,#58834,#58835,#58836,
#58837,#58838,#58839,#58840,#58841,#58842,#58843,#58844,#58845,#58846,#58847,
#58848,#58849,#58850,#58851,#58852,#58853,#58854,#58855,#58856,#58857,#58858,
#58859,#58860,#58861,#58862,#58863,#58864,#58865,#58866,#58867,#58868,#58869,
#58870,#58871,#58872,#58873,#58874,#58875,#58876,#58877,#58878,#58879,#58880,
#58881,#58882,#58883,#58884,#58885,#58886,#58887,#58888,#58889,#58890,#58891,
#58892,#58893,#58894,#58895,#58896,#58897,#58898,#58899,#58900,#58901,#58902,
#58903,#58904,#58905,#58906,#58907,#58908,#58909,#58910,#58911,#58912,#58913,
#58914,#58915,#58916,#58917,#58918,#58919,#58920,#58921,#58922,#58923,#58924,
#58925,#58926,#58927,#58928,#58929,#58930,#58931,#58932,#58933,#58934,#58935,
#58936,#58937,#58938,#58939,#58940,#58941,#58942,#58943,#58944,#58945,#58946,
#58947,#58948,#58949,#58950,#58951,#58952,#58953,#58954,#58955,#58956,#58957,
#58958,#58959,#58960,#58961,#58962,#58963,#58964,#58965,#58966,#58967,#58968,
#58969,#58970,#58971,#58972,#58973,#58974,#58975,#58976,#58977,#58978,#58979,
#58980,#58981,#58982,#58983,#58984,#58985,#58986),.UNSPECIFIED.,.F.,.F.,
(4,3,3,3,3,3,3,3,3,3,3,3,3,3,3,3,3,3,3,3,3,3,3,3,3,3,3,3,3,3,3,3,3,3,3,
3,3,3,3,3,3,3,3,3,3,3,3,3,3,3,3,3,3,3,3,3,3,3,3,3,3,3,3,3,3,3,4),(14.22949621209,
14.3389432582009,14.4483351528519,14.5577125976453,14.667195473431,14.7767304367527,
14.8864720704545,14.9748740343502,14.9749281643426,15.0752587140259,15.0846377010481,
15.1957150769961,15.3051216647848,15.4144613718424,15.5237750249548,15.6361454458741,
15.7456006442242,15.8594286764281,15.9579689742753,15.9732012351861,15.9732567086321,
16.0738013897155,16.0831958125145,16.1942444925654,16.303882218346,16.4134530400326,
16.5229974342433,16.6351443889129,16.7448268782272,16.8582060655744,16.956883871392,
16.9715256642228,16.9715852529216,17.0721632484324,17.0813057177578,17.1923817276894,
17.3018080824215,17.4111708864129,17.5205109949489,17.6328616955145,17.7423517142398,
17.8561327557255,17.954330039963,17.9698503625424,17.9699137972111,18.0695590982029,
18.0792721224164,18.190393399802,18.2994406760192,18.4084191124463,18.5173701848731,
18.63008822403,18.7391821149852,18.8537122282429,18.9524215317913,18.9682084403491,
18.9682423415007,19.0701286333108,19.0803840166759,19.1922879973418,19.304053299737,
19.4157152161891,19.5273088990212,19.6389125354701,19.7505118772813,19.8622220689861,
19.96657088579),.UNSPECIFIED.) ;
#1369 = B_SPLINE_CURVE_WITH_KNOTS('',3,(#58988,#58989,#58990,#58991,#58992,
#58993,#58994,#58995,#58996,#58997,#58998,#58999,#59000,#59001,#59002,#59003,
#59004,#59005,#59006,#59007,#59008,#59009,#59010,#59011,#59012,#59013,#59014,
#59015,#59016,#59017,#59018,#59019,#59020,#59021,#59022,#59023,#59024,#59025,
#59026,#59027,#59028,#59029,#59030,#59031,#59032,#59033,#59034,#59035,#59036,
#59037,#59038,#59039,#59040,#59041,#59042,#59043,#59044,#59045,#59046,#59047,
#59048,#59049,#59050,#59051,#59052,#59053,#59054,#59055,#59056,#59057,#59058,
#59059,#59060,#59061,#59062,#59063,#59064,#59065,#59066,#59067,#59068,#59069,
#59070,#59071,#59072,#59073,#59074,#59075,#59076,#59077,#59078,#59079,#59080,
#59081,#59082,#59083,#59084,#59085,#59086,#59087,#59088,#59089,#59090,#59091),
 .UNSPECIFIED.,.F.,.F.,(4,2,2,2,2,2,2,2,2,2,2,2,2,2,2,2,2,2,2,2,2,2,2,2,
2,2,2,2,2,2,2,2,2,2,2,2,2,2,2,2,2,2,2,2,2,2,2,2,2,2,2,4),(1.10915693870482,
1.11653647298846,1.13777455317558,1.16937210321511,1.18625815048209,1.19532910777744,
1.20809347272472,1.22642008117511,1.2632474552953,1.2787409213987,1.29613448763331,
1.3167350062781,1.35097542441865,1.36058555646715,1.37165177568789,1.40326323007923,
1.43132946312879,1.4464905459374,1.46436978353603,1.48613741210746,1.51879622492545,
1.52812939115584,1.53983435924038,1.55563078244551,1.59670910640585,1.61225905008095,
1.62951253261758,1.64978938441473,1.68506412274503,1.69457193167923,1.70588981021872,
1.72083164811916,1.76605846754896,1.78123805415975,1.79986981076746,1.84852087613937,
1.85935080091146,1.86906430813207,1.88073228386662,1.90893636218579,1.93356771082283,
1.94862623505778,1.96747335279999,2.00244608157891,2.01999222969602,2.02924579125722,
2.04132595857289,2.05794208021421,2.0989728229684,2.11432310360108,2.13270315491108,
2.15940621679325),.UNSPECIFIED.) ;
#1370 = B_SPLINE_CURVE_WITH_KNOTS('',3,(#59097,#59098,#59099,#59100,#59101,
#59102,#59103,#59104,#59105,#59106),.UNSPECIFIED.,.F.,.F.,(4,2,2,2,4),(0.000104928857968991,
0.0136473364548126,0.0227277261700891,0.0321175737869646,0.0589236362380934),
 .UNSPECIFIED.) ;
#1371 = B_SPLINE_CURVE_WITH_KNOTS('',3,(#59108,#59109,#59110,#59111,#59112,
#59113,#59114,#59115,#59116,#59117,#59118,#59119,#59120,#59121,#59122,#59123,
#59124,#59125,#59126,#59127,#59128,#59129,#59130,#59131,#59132,#59133,#59134,
#59135,#59136,#59137,#59138,#59139,#59140,#59141,#59142,#59143,#59144,#59145,
#59146,#59147,#59148,#59149,#59150,#59151,#59152,#59153,#59154,#59155,#59156,
#59157,#59158,#59159,#59160,#59161,#59162,#59163,#59164,#59165,#59166,#59167,
#59168,#59169,#59170,#59171,#59172,#59173,#59174,#59175,#59176,#59177,#59178,
#59179,#59180,#59181,#59182,#59183,#59184,#59185,#59186,#59187,#59188,#59189,
#59190,#59191,#59192,#59193,#59194,#59195,#59196,#59197,#59198,#59199,#59200,
#59201,#59202,#59203,#59204,#59205,#59206,#59207,#59208,#59209,#59210,#59211,
#59212,#59213,#59214,#59215,#59216,#59217,#59218,#59219,#59220,#59221,#59222,
#59223,#59224,#59225,#59226,#59227,#59228,#59229,#59230,#59231,#59232,#59233,
#59234,#59235,#59236,#59237),.UNSPECIFIED.,.F.,.F.,(4,3,3,3,3,3,3,3,3,3,
3,3,3,3,3,3,3,3,3,3,3,3,3,3,3,3,3,3,3,3,3,3,3,3,3,3,3,3,3,3,3,3,3,4),(-3.84638257219504,
-3.73820936453911,-3.63015334337089,-3.52217201520158,-3.41422262837725,
-3.30618624416936,-3.19810961675877,-3.0898327132607,-2.99504522064809,
-2.99498563286853,-2.8944076385451,-2.88526517210916,-2.77418916166789,
-2.664762811029,-2.55540001113266,-2.44605990669266,-2.33370920216425,-2.22421918751735,
-2.11043813804818,-2.01224085665499,-1.99672052263736,-1.99665708857902,
-1.89701178895675,-1.88729877268755,-1.7761774941378,-1.66713022650311,
-1.55815179836512,-1.44920073392293,-1.33648268651457,-1.22738880270019,
-1.11285867349485,-1.01414938328435,-0.998362445800008,-0.99832854428951,
-0.896442255853368,-0.886186853182638,-0.774282856892657,-0.662517539088778,
-0.550855607479958,-0.439261909779892,-0.32765825904241,-0.216058903257302,
-0.10434869827575,0.),.UNSPECIFIED.) ;
#1372 = B_SPLINE_CURVE_WITH_KNOTS('',3,(#59241,#59242,#59243,#59244,#59245,
#59246,#59247,#59248,#59249,#59250,#59251,#59252,#59253,#59254,#59255,#59256,
#59257,#59258,#59259,#59260,#59261,#59262,#59263,#59264,#59265,#59266,#59267,
#59268,#59269,#59270,#59271,#59272,#59273,#59274,#59275,#59276,#59277,#59278,
#59279,#59280,#59281,#59282,#59283,#59284,#59285,#59286,#59287,#59288,#59289,
#59290,#59291,#59292,#59293,#59294,#59295,#59296,#59297,#59298,#59299,#59300,
#59301,#59302,#59303,#59304,#59305,#59306,#59307,#59308,#59309,#59310,#59311,
#59312,#59313,#59314,#59315,#59316,#59317,#59318,#59319,#59320,#59321,#59322,
#59323,#59324,#59325,#59326,#59327,#59328,#59329,#59330,#59331,#59332,#59333,
#59334,#59335,#59336,#59337,#59338,#59339,#59340,#59341,#59342,#59343,#59344,
#59345,#59346,#59347,#59348,#59349,#59350,#59351,#59352,#59353,#59354,#59355,
#59356,#59357,#59358,#59359,#59360,#59361,#59362,#59363,#59364,#59365,#59366,
#59367,#59368,#59369,#59370,#59371,#59372,#59373,#59374,#59375,#59376,#59377,
#59378,#59379,#59380,#59381,#59382,#59383,#59384,#59385,#59386,#59387,#59388,
#59389,#59390,#59391,#59392,#59393,#59394,#59395,#59396,#59397,#59398,#59399,
#59400,#59401,#59402,#59403,#59404,#59405,#59406,#59407,#59408,#59409,#59410,
#59411,#59412,#59413,#59414,#59415,#59416,#59417,#59418,#59419,#59420,#59421,
#59422,#59423,#59424,#59425,#59426,#59427,#59428,#59429,#59430,#59431,#59432,
#59433,#59434,#59435,#59436,#59437,#59438,#59439),.UNSPECIFIED.,.F.,.F.,
(4,3,3,3,3,3,3,3,3,3,3,3,3,3,3,3,3,3,3,3,3,3,3,3,3,3,3,3,3,3,3,3,3,3,3,
3,3,3,3,3,3,3,3,3,3,3,3,3,3,3,3,3,3,3,3,3,3,3,3,3,3,3,3,3,3,3,4),(2.02841987206312,
2.12402082864211,2.23322562754713,2.34231909534285,2.45134273885873,2.56033796740028,
2.66942500876404,2.77855302002171,2.88788829258475,2.98613592948803,2.99492589447402,
2.99498563286853,3.0955586975681,3.1049217827746,3.21597083207253,3.32560733508656,
3.43517758256086,3.5447220500906,3.65687008185746,3.766554239541,3.87993420834952,
3.97858502075132,3.99325851352659,3.99331417715804,4.09371948668603,4.10302842613273,
4.21410521304708,4.32351375319195,4.43285438022156,4.54216792256757,4.65453662228756,
4.76398916469203,4.87781594306978,4.97628270692179,4.99158860021678,4.99164272144754,
5.09203017823468,5.10141729746262,5.21248654349692,5.32195772755063,5.4313616833961,
5.5407391310821,5.65304716474584,5.76256428251417,5.87626777412561,5.97482429279774,
5.98991773692861,5.98997126573705,6.09040640986076,6.09976771772371,6.21083422926157,
6.32032855031362,6.42975605635821,6.53915743408588,6.65144302807105,6.76098476827248,
6.87464228914952,6.97319316334142,6.98824588229396,6.98829981002656,7.08940628246248,
7.09951488574536,7.21054389577484,7.32140236885079,7.4321611881387,7.54286270613221,
7.59300756235356),.UNSPECIFIED.) ;
#1373 = B_SPLINE_CURVE_WITH_KNOTS('',3,(#59440,#59441,#59442,#59443,#59444,
#59445,#59446,#59447),.UNSPECIFIED.,.F.,.F.,(4,2,2,4),(-1.10892742733099,
-1.0870101516285,-1.05545170465039,-1.05009718249423),.UNSPECIFIED.) ;
#1374 = B_SPLINE_CURVE_WITH_KNOTS('',3,(#59454,#59455,#59456,#59457,#59458,
#59459,#59460,#59461,#59462,#59463,#59464,#59465,#59466,#59467,#59468,#59469,
#59470,#59471,#59472,#59473,#59474,#59475,#59476,#59477,#59478,#59479,#59480,
#59481,#59482,#59483,#59484,#59485,#59486,#59487,#59488,#59489,#59490,#59491,
#59492,#59493,#59494,#59495,#59496),.UNSPECIFIED.,.F.,.F.,(4,3,3,3,3,3,
3,3,3,3,3,3,3,3,4),(-17.9378810482228,-17.8425422594294,-17.7333287470564,
-17.6242265167285,-17.5151940640977,-17.4061899822639,-17.297094050263,
-17.1879571133028,-17.0786129340523,-16.9803667380989,-16.9716468941508,
-16.971585252919,-16.8695608459483,-16.8587004832189,-16.7648812846952),
 .UNSPECIFIED.) ;
#1375 = B_SPLINE_CURVE_WITH_KNOTS('',3,(#59502,#59503,#59504,#59505,#59506,
#59507,#59508,#59509,#59510,#59511,#59512,#59513,#59514,#59515,#59516,#59517,
#59518,#59519,#59520,#59521,#59522,#59523,#59524,#59525,#59526,#59527,#59528,
#59529,#59530,#59531,#59532,#59533,#59534,#59535,#59536,#59537,#59538,#59539,
#59540,#59541,#59542,#59543,#59544,#59545,#59546,#59547,#59548,#59549,#59550,
#59551,#59552,#59553,#59554,#59555,#59556,#59557,#59558,#59559,#59560,#59561,
#59562,#59563,#59564,#59565,#59566,#59567,#59568,#59569,#59570,#59571,#59572,
#59573,#59574,#59575,#59576,#59577,#59578,#59579,#59580,#59581,#59582,#59583,
#59584,#59585,#59586,#59587,#59588,#59589,#59590,#59591,#59592,#59593,#59594,
#59595,#59596,#59597,#59598,#59599,#59600,#59601,#59602,#59603,#59604,#59605,
#59606,#59607,#59608,#59609,#59610,#59611,#59612,#59613,#59614,#59615,#59616,
#59617,#59618,#59619,#59620,#59621,#59622,#59623,#59624,#59625,#59626,#59627,
#59628,#59629,#59630,#59631,#59632,#59633,#59634,#59635,#59636,#59637,#59638,
#59639,#59640,#59641,#59642,#59643,#59644,#59645,#59646,#59647,#59648,#59649,
#59650,#59651,#59652,#59653,#59654,#59655,#59656,#59657,#59658,#59659,#59660,
#59661,#59662,#59663,#59664,#59665,#59666,#59667,#59668,#59669,#59670,#59671,
#59672,#59673,#59674,#59675,#59676,#59677,#59678,#59679,#59680,#59681,#59682,
#59683,#59684,#59685,#59686,#59687,#59688,#59689,#59690,#59691,#59692,#59693,
#59694,#59695,#59696,#59697,#59698,#59699,#59700),.UNSPECIFIED.,.F.,.F.,
(4,3,3,3,3,3,3,3,3,3,3,3,3,3,3,3,3,3,3,3,3,3,3,3,3,3,3,3,3,3,3,3,3,3,3,
3,3,3,3,3,3,3,3,3,3,3,3,3,3,3,3,3,3,3,3,3,3,3,3,3,3,3,3,3,3,3,4),(14.2294786280813,
14.338922276967,14.4483107497908,14.557684750591,14.6671641680892,14.7766956576339,
14.8864338346194,14.9748737539835,14.9749281643402,15.0752589866694,15.0846352575163,
15.1957129389055,15.3051173769189,15.4144550482415,15.523766781667,15.6361392634077,
15.7455928462855,15.8594247774576,15.9579634795709,15.9732001976188,15.9732567086296,
16.0738077652168,16.0831978427548,16.1942462690253,16.3038866797998,16.413460431536,
16.5230080020905,16.6351523147976,16.7448385841499,16.8582119185344,16.9568858525924,
16.9715237741764,16.9715852529189,17.0721657571332,17.081314571444,17.1923894746645,
17.3018246639043,17.4111962855185,17.5205451920549,17.6328873433433,17.7423860660186,
17.8561499316134,17.9543534474692,17.9698491292093,17.9699137972083,18.0695608481754,
18.079289201519,18.1904083440163,18.2994712242243,18.4084646767039,18.5174301563394,
18.630133202629,18.7392398295538,18.8537410855257,18.9524757897826,18.9682091601267,
18.9682423414976,19.0701355316434,19.0803531665545,19.1922269279062,19.3039624488416,
19.4155950912131,19.5271600776355,19.6387361661106,19.7503085835541,19.8619932217595,
19.9665708857868),.UNSPECIFIED.) ;
#1376 = B_SPLINE_CURVE_WITH_KNOTS('',3,(#59702,#59703,#59704,#59705,#59706,
#59707,#59708,#59709,#59710,#59711,#59712,#59713,#59714,#59715,#59716,#59717,
#59718,#59719,#59720,#59721,#59722,#59723,#59724,#59725,#59726,#59727,#59728,
#59729,#59730,#59731,#59732,#59733,#59734,#59735,#59736,#59737,#59738,#59739,
#59740,#59741,#59742,#59743,#59744,#59745,#59746,#59747,#59748,#59749,#59750,
#59751,#59752,#59753,#59754,#59755,#59756,#59757,#59758,#59759,#59760,#59761,
#59762,#59763,#59764,#59765,#59766,#59767,#59768,#59769,#59770,#59771,#59772,
#59773,#59774,#59775,#59776,#59777,#59778,#59779,#59780,#59781,#59782,#59783,
#59784,#59785,#59786,#59787,#59788,#59789,#59790,#59791,#59792,#59793,#59794,
#59795,#59796,#59797,#59798,#59799,#59800,#59801,#59802,#59803,#59804,#59805),
 .UNSPECIFIED.,.F.,.F.,(4,2,2,2,2,2,2,2,2,2,2,2,2,2,2,2,2,2,2,2,2,2,2,2,
2,2,2,2,2,2,2,2,2,2,2,2,2,2,2,2,2,2,2,2,2,2,2,2,2,2,2,4),(1.10923445814272,
1.11666497858643,1.13797140915878,1.16980477676763,1.18649199766935,1.19554160045309,
1.20846695437517,1.22720172171421,1.26307764714478,1.27862260987191,1.29590862498156,
1.31625148391788,1.35136039511481,1.36088547756677,1.37213003076759,1.40426460938443,
1.4315528060664,1.44670778896382,1.46465320683135,1.48657603571803,1.51881468477099,
1.52817783896307,1.53981594437058,1.55546005225205,1.59701085189892,1.61253832989724,
1.6298665872769,1.65031352546849,1.68502329566247,1.69459082162201,1.70580180457738,
1.73773773559284,1.76517201833841,1.7803173091195,1.79823685726372,1.82009585491647,
1.85259182246046,1.86193134040701,1.87355251831195,1.88917171818081,1.93059177790007,
1.94603630598094,1.96317990033113,1.98326148971095,2.0194272706928,2.02885251398158,
2.04043217677661,2.05590113240821,2.09758105669224,2.11313303528988,2.13078190515427,
2.15945489884343),.UNSPECIFIED.) ;
#1377 = B_SPLINE_CURVE_WITH_KNOTS('',3,(#59811,#59812,#59813,#59814,#59815,
#59816,#59817,#59818,#59819,#59820),.UNSPECIFIED.,.F.,.F.,(4,2,2,2,4),(0.000105664403462806,
0.013888256199573,0.0231378033575992,0.0327082927549276,0.0589309959070275),
 .UNSPECIFIED.) ;
#1378 = B_SPLINE_CURVE_WITH_KNOTS('',3,(#59822,#59823,#59824,#59825,#59826,
#59827,#59828,#59829,#59830,#59831,#59832,#59833,#59834,#59835,#59836,#59837,
#59838,#59839,#59840,#59841,#59842,#59843,#59844,#59845,#59846,#59847,#59848,
#59849,#59850,#59851,#59852,#59853,#59854,#59855,#59856,#59857,#59858,#59859,
#59860,#59861,#59862,#59863,#59864,#59865,#59866,#59867,#59868,#59869,#59870,
#59871,#59872,#59873,#59874,#59875,#59876,#59877,#59878,#59879,#59880,#59881,
#59882,#59883,#59884,#59885,#59886,#59887,#59888,#59889,#59890,#59891,#59892,
#59893,#59894,#59895,#59896,#59897,#59898,#59899,#59900,#59901,#59902,#59903,
#59904,#59905,#59906,#59907,#59908,#59909,#59910,#59911,#59912,#59913,#59914,
#59915,#59916,#59917,#59918,#59919,#59920,#59921,#59922,#59923,#59924,#59925,
#59926,#59927,#59928,#59929,#59930,#59931,#59932,#59933,#59934,#59935,#59936,
#59937,#59938,#59939,#59940,#59941,#59942,#59943,#59944,#59945,#59946,#59947,
#59948,#59949,#59950,#59951),.UNSPECIFIED.,.F.,.F.,(4,3,3,3,3,3,3,3,3,3,
3,3,3,3,3,3,3,3,3,3,3,3,3,3,3,3,3,3,3,3,3,3,3,3,3,3,3,3,3,3,3,3,3,4),(-3.84638255648223,
-3.7382056031972,-3.63014560658662,-3.52216007910798,-3.41420626916828,
-3.30616512394713,-3.19808354221321,-3.08980139966837,-2.99504711079657,
-2.99498563286806,-2.89440512981233,-2.88525631822079,-2.77418141451553,
-2.66474622912418,-2.55537461134289,-2.44602570862247,-2.33368355361152,
-2.22418483468985,-2.11042096163427,-2.0122174484571,-1.99672175606977,
-1.9966570885787,-1.89701003804244,-1.88728169061728,-1.77616254732629,
-1.66709967286179,-1.55810622588554,-1.44914075150563,-1.33643769970156,
-1.22733107735769,-1.11282981082352,-1.01409511633373,-0.998361725954698,
-0.998328544289352,-0.89643535725085,-0.886217707062147,-0.774343933803599,
-0.662608401142561,-0.550975747253691,-0.439410749549519,-0.327834650256548,
-0.216262222247108,-0.104577574025189,0.),.UNSPECIFIED.) ;
#1379 = B_SPLINE_CURVE_WITH_KNOTS('',3,(#59955,#59956,#59957,#59958,#59959,
#59960,#59961,#59962,#59963,#59964,#59965,#59966,#59967,#59968,#59969,#59970,
#59971,#59972,#59973,#59974,#59975,#59976,#59977,#59978,#59979,#59980,#59981,
#59982,#59983,#59984,#59985,#59986,#59987,#59988,#59989,#59990,#59991,#59992,
#59993,#59994,#59995,#59996,#59997,#59998,#59999,#60000,#60001,#60002,#60003,
#60004,#60005,#60006,#60007,#60008,#60009,#60010,#60011,#60012,#60013,#60014,
#60015,#60016,#60017,#60018,#60019,#60020,#60021,#60022,#60023,#60024,#60025,
#60026,#60027,#60028,#60029,#60030,#60031,#60032,#60033,#60034,#60035,#60036,
#60037,#60038,#60039,#60040,#60041,#60042,#60043,#60044,#60045,#60046,#60047,
#60048,#60049,#60050,#60051,#60052,#60053,#60054,#60055,#60056,#60057,#60058,
#60059,#60060,#60061,#60062,#60063,#60064,#60065,#60066,#60067,#60068,#60069,
#60070,#60071,#60072,#60073,#60074,#60075,#60076,#60077,#60078,#60079,#60080,
#60081,#60082,#60083,#60084,#60085,#60086,#60087,#60088,#60089,#60090,#60091,
#60092,#60093,#60094,#60095,#60096,#60097,#60098,#60099,#60100,#60101,#60102,
#60103,#60104,#60105,#60106,#60107,#60108,#60109,#60110,#60111,#60112,#60113,
#60114,#60115,#60116,#60117,#60118,#60119,#60120,#60121,#60122,#60123,#60124,
#60125,#60126,#60127,#60128,#60129,#60130,#60131,#60132,#60133,#60134,#60135,
#60136,#60137,#60138,#60139,#60140,#60141,#60142,#60143,#60144,#60145,#60146,
#60147,#60148,#60149,#60150,#60151,#60152,#60153),.UNSPECIFIED.,.F.,.F.,
(4,3,3,3,3,3,3,3,3,3,3,3,3,3,3,3,3,3,3,3,3,3,3,3,3,3,3,3,3,3,3,3,3,3,3,
3,3,3,3,3,3,3,3,3,3,3,3,3,3,3,3,3,3,3,3,3,3,3,3,3,3,3,3,3,3,3,4),(2.02868994874317,
2.12402862965265,2.23324214578185,2.34234437989576,2.4513768363412,2.56038092201705,
2.66947685788854,2.77861379874124,2.88795798188678,2.98620417724028,2.99492399082981,
2.99498563286805,3.09555617348582,3.10492603756324,3.21597455501251,3.32561466385153,
3.43518827380549,3.54473586247821,3.65688044114801,3.76656712248518,3.87994064982129,
3.97859723168738,3.99325743938423,3.9933141771574,4.09371803583068,4.10302707563617,
4.21410403136249,4.32351087460842,4.43284967933567,4.54216127636544,4.65453163763577,
4.76398194856462,4.87781233500568,4.97627975308706,4.99158830482236,4.99164272144675,
5.09202871645766,5.1014138513281,5.2124835281291,5.32195126426091,5.431351777065,
5.54072578898615,5.65303715817364,5.76255088203706,5.87626107388658,5.9748151813961,
5.98991759903774,5.9899712657361,6.09040611229201,6.09976683700301,6.21083345863081,
6.32032703737286,6.42975385265224,6.5391545904993,6.65144089538084,6.76098212066125,
6.87464096534335,6.97319091957135,6.98824558193009,6.98829981002545,7.089406779752,
7.09951545927819,7.21054508021919,7.32140421541049,7.43216372563492,7.54286597301087,
7.593007562351),.UNSPECIFIED.) ;
#1380 = B_SPLINE_CURVE_WITH_KNOTS('',3,(#60154,#60155,#60156,#60157,#60158,
#60159,#60160,#60161),.UNSPECIFIED.,.F.,.F.,(4,2,2,4),(-1.10884682316275,
-1.08689503526884,-1.05534897114704,-1.05003214208722),.UNSPECIFIED.) ;
#1381 = B_SPLINE_CURVE_WITH_KNOTS('',3,(#60163,#60164,#60165,#60166,#60167,
#60168,#60169,#60170,#60171,#60172,#60173,#60174,#60175,#60176,#60177,#60178,
#60179,#60180,#60181,#60182,#60183,#60184,#60185,#60186,#60187,#60188,#60189,
#60190,#60191,#60192,#60193,#60194,#60195,#60196,#60197,#60198,#60199,#60200,
#60201,#60202,#60203,#60204,#60205,#60206,#60207,#60208,#60209,#60210,#60211,
#60212,#60213,#60214,#60215,#60216,#60217,#60218,#60219,#60220,#60221,#60222,
#60223,#60224,#60225,#60226,#60227,#60228,#60229,#60230,#60231,#60232,#60233,
#60234,#60235,#60236,#60237,#60238,#60239,#60240,#60241,#60242,#60243,#60244,
#60245,#60246,#60247,#60248,#60249,#60250,#60251,#60252,#60253,#60254,#60255,
#60256,#60257,#60258,#60259,#60260,#60261,#60262,#60263,#60264,#60265,#60266),
 .UNSPECIFIED.,.F.,.F.,(4,2,2,2,2,2,2,2,2,2,2,2,2,2,2,2,2,2,2,2,2,2,2,2,
2,2,2,2,2,2,2,2,2,2,2,2,2,2,2,2,2,2,2,2,2,2,2,2,2,2,2,4),(-1.05003214208722,
-1.04431790606983,-1.03481094545539,-1.00003759698371,-0.979677257209173,
-0.962430901614528,-0.947036722863476,-0.904868645028897,-0.889517257790306,
-0.878029357298292,-0.86871841066293,-0.831920651739553,-0.812142554503174,
-0.795148484116817,-0.779653060990973,-0.739156076372092,-0.723227683493391,
-0.711482092797267,-0.702260210393523,-0.668597701106728,-0.647240311786537,
-0.629569615001816,-0.614483019326602,-0.586107260480668,-0.554586077874824,
-0.543725444409351,-0.534110794360145,-0.522617749546019,-0.495427129208312,
-0.470333279145638,-0.455188297948145,-0.436976322937294,-0.385563849403027,
-0.375618860991466,-0.36523374758677,-0.33385290221376,-0.304245283135888,
-0.289146936842405,-0.271518785459582,-0.250261593351171,-0.21639347451471,
-0.207186878728247,-0.195386560398939,-0.1793331484783,-0.139082756965759,
-0.123556325726735,-0.106601404037852,-0.0869187355250082,-0.0498664571300566,
-0.0405757086686247,-0.0289749179513464,-0.000105736955589282),
 .UNSPECIFIED.) ;
#1382 = B_SPLINE_CURVE_WITH_KNOTS('',3,(#60267,#60268,#60269,#60270,#60271,
#60272,#60273,#60274,#60275,#60276,#60277,#60278,#60279,#60280,#60281,#60282,
#60283,#60284,#60285,#60286,#60287,#60288,#60289,#60290,#60291,#60292,#60293,
#60294,#60295,#60296,#60297,#60298,#60299,#60300,#60301,#60302,#60303,#60304,
#60305,#60306,#60307,#60308,#60309,#60310,#60311,#60312,#60313,#60314,#60315,
#60316,#60317,#60318,#60319,#60320,#60321,#60322,#60323,#60324,#60325,#60326,
#60327,#60328,#60329,#60330,#60331,#60332,#60333,#60334,#60335,#60336,#60337,
#60338,#60339,#60340,#60341,#60342,#60343,#60344,#60345,#60346,#60347,#60348,
#60349,#60350,#60351,#60352,#60353,#60354,#60355,#60356,#60357,#60358,#60359,
#60360,#60361,#60362,#60363,#60364,#60365,#60366,#60367,#60368,#60369,#60370),
 .UNSPECIFIED.,.F.,.F.,(4,2,2,2,2,2,2,2,2,2,2,2,2,2,2,2,2,2,2,2,2,2,2,2,
2,2,2,2,2,2,2,2,2,2,2,2,2,2,2,2,2,2,2,2,2,2,2,2,2,2,2,4),(0.0589309959070275,
0.0673105367891647,0.0878341697386557,0.105168713875815,0.120538545156185,
0.163277448753101,0.17845889663062,0.189880980338227,0.199296845798575,
0.235398156440507,0.255440965567746,0.272592461106828,0.288162209074821,
0.328658023811127,0.344638658922391,0.35642349567249,0.365753075913841,
0.398554535466949,0.420249228806342,0.438102775994272,0.453287441577484,
0.482604518844649,0.514080146699166,0.524638787758827,0.534591712082898,
0.586106633858573,0.604383068624081,0.61963489171561,0.664163839882258,
0.679244465726587,0.690625320536653,0.700085867517545,0.735796022663253,
0.755940679691749,0.773141156071703,0.788719090741103,0.829419033780146,
0.845359343849969,0.857128308161983,0.866447839550388,0.899377133437613,
0.921049672023105,0.938896990836141,0.954081508026912,0.984436791901902,
1.0075127403737,1.02196478051473,1.03088118671146,1.04712733482288,1.08003058740821,
1.10162173533867,1.10923445814272),.UNSPECIFIED.) ;
#1383 = B_SPLINE_CURVE_WITH_KNOTS('',3,(#60372,#60373,#60374,#60375,#60376,
#60377,#60378,#60379,#60380,#60381,#60382,#60383,#60384,#60385,#60386,#60387,
#60388,#60389,#60390,#60391,#60392,#60393,#60394,#60395,#60396,#60397,#60398,
#60399,#60400,#60401,#60402,#60403,#60404,#60405,#60406,#60407,#60408,#60409,
#60410,#60411,#60412,#60413,#60414,#60415,#60416,#60417,#60418,#60419,#60420,
#60421,#60422,#60423,#60424,#60425,#60426,#60427,#60428,#60429,#60430,#60431,
#60432,#60433,#60434,#60435,#60436,#60437,#60438,#60439,#60440,#60441,#60442,
#60443,#60444,#60445,#60446,#60447,#60448,#60449,#60450,#60451,#60452,#60453,
#60454,#60455,#60456,#60457,#60458,#60459,#60460,#60461,#60462,#60463,#60464,
#60465,#60466,#60467,#60468,#60469,#60470,#60471,#60472,#60473,#60474,#60475,
#60476,#60477),.UNSPECIFIED.,.F.,.F.,(4,2,2,2,2,2,2,2,2,2,2,2,2,2,2,2,2,
2,2,2,2,2,2,2,2,2,2,2,2,2,2,2,2,2,2,2,2,2,2,2,2,2,2,2,2,2,2,2,2,2,2,2,4),
(-1.05009718249423,-1.04440384069162,-1.03490404059468,-1.00003925538964,
-0.979699394704859,-0.9624609922212,-0.947063577815217,-0.90492974045796,
-0.889561950214529,-0.87806598790377,-0.868757119523483,-0.8319166108485,
-0.8121451658037,-0.79515310473938,-0.779655329980471,-0.739161316490995,
-0.723226287841405,-0.711477106871101,-0.702255796851051,-0.668562333963969,
-0.647209575251974,-0.629539800290398,-0.614451716572985,-0.58607026667325,
-0.554543131940902,-0.543680915499547,-0.534066041098232,-0.522573554312757,
-0.495392626353674,-0.470323986373885,-0.455172730104426,-0.436992966401846,
-0.414397046252215,-0.384057785509152,-0.374628212069828,-0.363426593882055,
-0.331397695516476,-0.304073226126729,-0.28900212031638,-0.271284376210517,
-0.249810927369898,-0.216556601359796,-0.207310013978551,-0.195641197707316,
-0.179886111662056,-0.138787884050401,-0.123317797916446,-0.106240021436115,
-0.086275842155076,-0.0502059381847442,-0.0408239803117995,-0.0294675766559434,
-0.000104999262269449),.UNSPECIFIED.) ;
#1384 = B_SPLINE_CURVE_WITH_KNOTS('',3,(#60478,#60479,#60480,#60481,#60482,
#60483,#60484,#60485,#60486,#60487,#60488,#60489,#60490,#60491,#60492,#60493,
#60494,#60495,#60496,#60497,#60498,#60499,#60500,#60501,#60502,#60503,#60504,
#60505,#60506,#60507,#60508,#60509,#60510,#60511,#60512,#60513,#60514,#60515,
#60516,#60517,#60518,#60519,#60520,#60521,#60522,#60523,#60524,#60525,#60526,
#60527,#60528,#60529,#60530,#60531,#60532,#60533,#60534,#60535,#60536,#60537,
#60538,#60539,#60540,#60541,#60542,#60543,#60544,#60545,#60546,#60547,#60548,
#60549,#60550,#60551,#60552,#60553,#60554,#60555,#60556,#60557,#60558,#60559,
#60560,#60561,#60562,#60563,#60564,#60565,#60566,#60567,#60568,#60569,#60570,
#60571,#60572,#60573,#60574,#60575,#60576,#60577,#60578,#60579,#60580,#60581,
#60582,#60583),.UNSPECIFIED.,.F.,.F.,(4,2,2,2,2,2,2,2,2,2,2,2,2,2,2,2,2,
2,2,2,2,2,2,2,2,2,2,2,2,2,2,2,2,2,2,2,2,2,2,2,2,2,2,2,2,2,2,2,2,2,2,2,4),
(0.0589236362380934,0.0635158185275896,0.0858196264570916,0.103894607137741,
0.119066674557036,0.163592372683235,0.178616439360702,0.189965040437009,
0.199403587897761,0.230190402340796,0.252671422661968,0.27084276731401,
0.286105385067266,0.327666480543899,0.344180445075028,0.356196540140646,
0.365448975000031,0.391370214599746,0.416825269071937,0.436124283029981,
0.451244414490889,0.475409609913047,0.504250489047926,0.516029893130278,
0.525802523841248,0.536603275814354,0.585229402586121,0.603855483269689,
0.619039288280215,0.664396476118038,0.679334919830258,0.690649514845529,
0.70013435020136,0.735569547448692,0.755790762571726,0.773021648641629,
0.788576830600346,0.829547704455815,0.845389112552175,0.857113299376208,
0.866442959077371,0.899173315808385,0.920911931681626,0.938783952092706,
0.953954915089721,0.982337188402188,1.00677377473397,1.02164504182984,1.03054546711717,
1.04675751171221,1.07985896645351,1.10149884302173,1.10915693870482),
 .UNSPECIFIED.) ;
#1385 = B_SPLINE_CURVE_WITH_KNOTS('',3,(#60585,#60586,#60587,#60588,#60589,
#60590,#60591,#60592,#60593,#60594,#60595,#60596,#60597,#60598,#60599,#60600,
#60601,#60602,#60603,#60604,#60605,#60606,#60607,#60608,#60609,#60610,#60611,
#60612,#60613,#60614,#60615,#60616,#60617,#60618,#60619,#60620,#60621,#60622,
#60623,#60624,#60625,#60626,#60627,#60628,#60629,#60630,#60631,#60632,#60633,
#60634,#60635,#60636,#60637,#60638,#60639,#60640,#60641,#60642,#60643,#60644,
#60645,#60646,#60647,#60648,#60649,#60650,#60651,#60652,#60653,#60654,#60655,
#60656,#60657,#60658,#60659,#60660,#60661,#60662,#60663,#60664,#60665,#60666,
#60667,#60668,#60669,#60670,#60671,#60672,#60673,#60674,#60675,#60676,#60677,
#60678,#60679,#60680,#60681,#60682,#60683,#60684,#60685,#60686,#60687,#60688,
#60689,#60690,#60691,#60692,#60693,#60694),.UNSPECIFIED.,.F.,.F.,(4,2,2,
2,2,2,2,2,2,2,2,2,2,2,2,2,2,2,2,2,2,2,2,2,2,2,2,2,2,2,2,2,2,2,2,2,2,2,2,
2,2,2,2,2,2,2,2,2,2,2,2,2,2,2,4),(1.00000006361678E-6,0.0403383732114231,
0.0710490831136922,0.0867357356300736,0.102991445296282,0.153634238618413,
0.171497745854947,0.184581571030169,0.193340939594793,0.207334580300476,
0.248434086191359,0.277268820022062,0.292829275133986,0.309253163863494,
0.358041871857424,0.384682999262059,0.394382470861302,0.404335350906858,
0.444894402162554,0.469642610349295,0.489384110315505,0.50435428197641,
0.524055829842245,0.568418671704122,0.591013749967294,0.600462010919991,
0.610750427743009,0.653783778641295,0.676896139556732,0.695899514262901,
0.710880679088112,0.731418553902633,0.776255216756211,0.797065187062705,
0.806367710856781,0.816895594993979,0.858066414896168,0.881774919635306,
0.901050994782059,0.916022397211022,0.936215694056919,0.980397646718051,
1.00227270642186,1.01166355421563,1.02203884108323,1.06439103413832,1.09744727041259,
1.11340959527833,1.12932874960038,1.16537276803491,1.20613695542018,1.21607213983233,
1.2257852226005,1.2527447650388,1.29362987758487),.UNSPECIFIED.) ;
#1386 = B_SPLINE_CURVE_WITH_KNOTS('',3,(#60695,#60696,#60697,#60698,#60699,
#60700,#60701,#60702,#60703,#60704,#60705,#60706,#60707,#60708,#60709,#60710,
#60711,#60712,#60713,#60714,#60715,#60716,#60717,#60718,#60719,#60720,#60721,
#60722,#60723,#60724,#60725,#60726,#60727,#60728,#60729,#60730,#60731,#60732,
#60733,#60734,#60735,#60736,#60737,#60738,#60739,#60740,#60741,#60742,#60743,
#60744,#60745,#60746,#60747,#60748,#60749,#60750,#60751,#60752,#60753,#60754,
#60755,#60756,#60757,#60758,#60759,#60760,#60761,#60762,#60763,#60764,#60765,
#60766,#60767,#60768,#60769,#60770,#60771,#60772,#60773,#60774,#60775,#60776,
#60777,#60778,#60779,#60780,#60781,#60782,#60783,#60784,#60785,#60786,#60787,
#60788,#60789,#60790,#60791,#60792,#60793,#60794,#60795,#60796,#60797,#60798,
#60799,#60800,#60801,#60802,#60803,#60804),.UNSPECIFIED.,.F.,.F.,(4,2,2,
2,2,2,2,2,2,2,2,2,2,2,2,2,2,2,2,2,2,2,2,2,2,2,2,2,2,2,2,2,2,2,2,2,2,2,2,
2,2,2,2,2,2,2,2,2,2,2,2,2,2,2,4),(1.2938343569962,1.29398644728992,1.34783545812506,
1.36349764754707,1.37953598958877,1.41609269887716,1.45505304576164,1.46511091332811,
1.47460836802503,1.49835596884893,1.55374208105197,1.5693454850041,1.58546726978071,
1.60563639211527,1.64628913244785,1.66412627491977,1.67311923424172,1.68413580579912,
1.69783089178063,1.73402395581065,1.76078590541362,1.77612431867759,1.7926753326203,
1.82773843505827,1.86601644822502,1.87612478810658,1.88558195322214,1.90877340853656,
1.95321180938884,1.97248661377819,1.98737303650753,2.00727513183119,2.03247215463915,
2.07178122202493,2.08181336623754,2.09135166230483,2.11568099593797,2.16947189389525,
2.18523202350263,2.2011463073406,2.23690321446718,2.27767661820716,2.28757639189183,
2.29716180922901,2.32248742106138,2.37545195516269,2.39108242253067,2.40695936596739,
2.44285289843246,2.48359334606267,2.49348873341424,2.50318828476119,2.52944381027782,
2.57223691900561,2.5876387803254),.UNSPECIFIED.) ;
#1387 = B_SPLINE_CURVE_WITH_KNOTS('',3,(#60806,#60807,#60808,#60809,#60810,
#60811,#60812,#60813,#60814,#60815,#60816,#60817,#60818,#60819,#60820,#60821,
#60822,#60823,#60824,#60825,#60826,#60827,#60828,#60829,#60830,#60831,#60832,
#60833,#60834,#60835,#60836,#60837,#60838,#60839,#60840,#60841,#60842,#60843,
#60844,#60845,#60846,#60847,#60848,#60849,#60850,#60851,#60852,#60853,#60854,
#60855,#60856,#60857,#60858,#60859,#60860,#60861,#60862,#60863,#60864,#60865,
#60866,#60867,#60868,#60869,#60870,#60871,#60872,#60873,#60874,#60875,#60876,
#60877,#60878,#60879,#60880,#60881,#60882,#60883,#60884,#60885,#60886,#60887,
#60888,#60889,#60890,#60891,#60892,#60893,#60894,#60895,#60896,#60897,#60898,
#60899,#60900,#60901,#60902,#60903,#60904,#60905,#60906,#60907,#60908,#60909,
#60910,#60911,#60912,#60913,#60914,#60915),.UNSPECIFIED.,.F.,.F.,(4,2,2,
2,2,2,2,2,2,2,2,2,2,2,2,2,2,2,2,2,2,2,2,2,2,2,2,2,2,2,2,2,2,2,2,2,2,2,2,
2,2,2,2,2,2,2,2,2,2,2,2,2,2,2,4),(9.99999998185342E-7,0.0393714830762708,
0.0614236531788015,0.0799292118101189,0.0949519681806495,0.116270989140045,
0.159883898289276,0.180479303284034,0.189763590677115,0.20033136580239,
0.241164152569101,0.275664123794416,0.291528803690653,0.307548732072641,
0.345030200504205,0.378312653339943,0.390714015177875,0.399512834452093,
0.414445222726917,0.45574206941328,0.483324276412407,0.498802954998541,
0.515405335642074,0.562420894589255,0.581517250452164,0.59514795180082,
0.603903959020001,0.617325670303496,0.658170984699609,0.687970130931299,
0.703599983395622,0.719931630249499,0.76967450999556,0.795778492662367,
0.805454247909864,0.815447969538123,0.855566785240905,0.880484772404275,
0.900301104785482,0.915272635873529,0.934904310459233,0.980299415569464,
1.00221168927269,1.0116075141433,1.02198370292319,1.06434990025255,1.09740580169878,
1.11337285036377,1.12929989543337,1.16547076629152,1.20604506774957,1.2159999821617,
1.22570125360452,1.25238244100321,1.29359361912601),.UNSPECIFIED.) ;
#1388 = B_SPLINE_CURVE_WITH_KNOTS('',3,(#60916,#60917,#60918,#60919,#60920,
#60921,#60922,#60923,#60924,#60925,#60926,#60927,#60928,#60929,#60930,#60931,
#60932,#60933,#60934,#60935,#60936,#60937,#60938,#60939,#60940,#60941,#60942,
#60943,#60944,#60945,#60946,#60947,#60948,#60949,#60950,#60951,#60952,#60953,
#60954,#60955,#60956,#60957,#60958,#60959,#60960,#60961,#60962,#60963,#60964,
#60965,#60966,#60967,#60968,#60969,#60970,#60971,#60972,#60973,#60974,#60975,
#60976,#60977,#60978,#60979,#60980,#60981,#60982,#60983,#60984,#60985,#60986,
#60987,#60988,#60989,#60990,#60991,#60992,#60993,#60994,#60995,#60996,#60997,
#60998,#60999,#61000,#61001,#61002,#61003,#61004,#61005,#61006,#61007,#61008,
#61009,#61010,#61011,#61012,#61013,#61014,#61015,#61016,#61017,#61018,#61019,
#61020,#61021,#61022,#61023,#61024,#61025,#61026,#61027,#61028,#61029,#61030,
#61031),.UNSPECIFIED.,.F.,.F.,(4,2,2,2,2,2,2,2,2,2,2,2,2,2,2,2,2,2,2,2,
2,2,2,2,2,2,2,2,2,2,2,2,2,2,2,2,2,2,2,2,2,2,2,2,2,2,2,2,2,2,2,2,2,2,2,2,
2,4),(1.29395065554619,1.29412647113177,1.34795804332071,1.36362730258072,
1.37967165797811,1.41624234391851,1.45520805147782,1.46526976129763,1.47477123977964,
1.49853687016536,1.55392487778237,1.56953545477562,1.5856648617973,1.60584013193459,
1.64652189029532,1.66434295951244,1.6732490038614,1.68420760483371,1.69779163750427,
1.73320528500144,1.76069411255744,1.77609419629443,1.79254509788095,1.81268172166021,
1.8567235700942,1.87156474690353,1.88031423644406,1.8925944261694,1.92580139257715,
1.96350669917209,1.97946235972831,1.99521499737111,2.02843530105521,2.07150917094093,
2.08176608365818,2.09115063374276,2.11331061581725,2.15749481019505,2.17739473887451,
2.1922709953139,2.2115115535979,2.23520582028204,2.27649462642989,2.28698612839726,
2.29618617478099,2.31630502514474,2.35761391596731,2.38024673649518,2.39519879687926,
2.41264245577691,2.43263755004155,2.4737413512898,2.48868791950007,2.49746205768953,
2.50981633664026,2.54328067721221,2.57241596901025,2.58798484160242),
 .UNSPECIFIED.) ;
#1389 = B_SPLINE_CURVE_WITH_KNOTS('',3,(#61033,#61034,#61035,#61036,#61037,
#61038,#61039,#61040,#61041,#61042,#61043,#61044,#61045,#61046,#61047,#61048,
#61049,#61050,#61051,#61052,#61053,#61054,#61055,#61056,#61057,#61058,#61059,
#61060,#61061,#61062,#61063,#61064,#61065,#61066,#61067,#61068,#61069,#61070,
#61071,#61072,#61073,#61074,#61075,#61076,#61077,#61078,#61079,#61080,#61081,
#61082,#61083,#61084,#61085,#61086,#61087,#61088,#61089,#61090,#61091,#61092,
#61093,#61094,#61095,#61096,#61097,#61098,#61099,#61100,#61101,#61102,#61103,
#61104,#61105,#61106,#61107,#61108,#61109,#61110,#61111,#61112,#61113,#61114,
#61115,#61116,#61117,#61118,#61119,#61120,#61121,#61122,#61123,#61124,#61125,
#61126,#61127,#61128,#61129,#61130,#61131,#61132,#61133,#61134,#61135,#61136),
 .UNSPECIFIED.,.F.,.F.,(4,2,2,2,2,2,2,2,2,2,2,2,2,2,2,2,2,2,2,2,2,2,2,2,
2,2,2,2,2,2,2,2,2,2,2,2,2,2,2,2,2,2,2,2,2,2,2,2,2,2,2,4),(-1.05001965519088,
-1.04432229220903,-1.03482244015609,-0.999986602611031,-0.979645339017254,
-0.962408079697338,-0.947014267261727,-0.904879744379389,-0.889518808648716,
-0.878026928319333,-0.868719204200551,-0.831896248184208,-0.812126667939335,
-0.795137154664959,-0.77964276881305,-0.739155410492211,-0.72322492607398,
-0.711478769469322,-0.70225896360659,-0.668579624151552,-0.647229501402792,
-0.629562664283716,-0.614477677909573,-0.586102822255114,-0.554582908261496,
-0.543723031213306,-0.53410993118934,-0.522619347725069,-0.49544069022844,
-0.470370427488178,-0.455223536809314,-0.437038830035277,-0.385789447446468,
-0.375756530464295,-0.365474424583251,-0.334289141005716,-0.304256187657895,
-0.289159638986684,-0.27153775255282,-0.250294373321025,-0.216377731948496,
-0.207174965230979,-0.195367424126632,-0.179297432410926,-0.13910749793898,
-0.123578808245063,-0.106631042130916,-0.0869649081841599,-0.0498455866748933,
-0.0405616460688914,-0.0289500608303166,-0.000105196980790777),
 .UNSPECIFIED.) ;
#1390 = B_SPLINE_CURVE_WITH_KNOTS('',3,(#61137,#61138,#61139,#61140,#61141,
#61142,#61143,#61144,#61145,#61146,#61147,#61148,#61149,#61150,#61151,#61152,
#61153,#61154,#61155,#61156,#61157,#61158,#61159,#61160,#61161,#61162,#61163,
#61164,#61165,#61166,#61167,#61168,#61169,#61170,#61171,#61172,#61173,#61174,
#61175,#61176,#61177,#61178,#61179,#61180,#61181,#61182,#61183,#61184,#61185,
#61186,#61187,#61188,#61189,#61190,#61191,#61192,#61193,#61194,#61195,#61196,
#61197,#61198,#61199,#61200,#61201,#61202,#61203,#61204,#61205,#61206,#61207,
#61208,#61209,#61210,#61211,#61212,#61213,#61214,#61215,#61216,#61217,#61218,
#61219,#61220,#61221,#61222,#61223,#61224,#61225,#61226,#61227,#61228,#61229,
#61230,#61231,#61232,#61233,#61234,#61235,#61236,#61237,#61238,#61239,#61240,
#61241,#61242),.UNSPECIFIED.,.F.,.F.,(4,2,2,2,2,2,2,2,2,2,2,2,2,2,2,2,2,
2,2,2,2,2,2,2,2,2,2,2,2,2,2,2,2,2,2,2,2,2,2,2,2,2,2,2,2,2,2,2,2,2,2,2,4),
(0.0589148629143721,0.0590186788227545,0.0836761261735466,0.10266362385716,
0.11770045310667,0.142731334957056,0.170798172465959,0.182445136240436,
0.192146244794664,0.202991157601695,0.251571998328379,0.270187004540828,
0.285363261691562,0.330569697155811,0.345527115094681,0.356849783314103,
0.366352722562126,0.401610304980716,0.421865590172558,0.439108591303875,
0.454658352339863,0.495729706689891,0.511539689650347,0.52324851840138,
0.532578071094702,0.565222290830694,0.586966370475972,0.604834760960242,
0.61999608870806,0.648144808479112,0.679759751805539,0.690793721242204,
0.700419500266837,0.734452537107621,0.75509311217183,0.772503489209045,
0.787989107541598,0.830126108597528,0.845565484279735,0.857109903499478,
0.866505825827409,0.898184038219147,0.920310094295822,0.938340224985504,
0.953646219623509,0.98103141025493,1.00622467106084,1.02131892231489,1.03021556836862,
1.04615682168103,1.0795269050592,1.10123582673028,1.10894604130966),
 .UNSPECIFIED.) ;
#1391 = B_SPLINE_CURVE_WITH_KNOTS('',3,(#61244,#61245,#61246,#61247,#61248,
#61249,#61250,#61251,#61252,#61253,#61254,#61255,#61256,#61257,#61258,#61259,
#61260,#61261,#61262,#61263,#61264,#61265,#61266,#61267,#61268,#61269,#61270,
#61271,#61272,#61273,#61274,#61275,#61276,#61277,#61278,#61279,#61280,#61281,
#61282,#61283,#61284,#61285,#61286,#61287,#61288,#61289,#61290,#61291,#61292,
#61293,#61294,#61295,#61296,#61297,#61298,#61299,#61300,#61301,#61302,#61303,
#61304,#61305,#61306,#61307,#61308,#61309,#61310,#61311,#61312,#61313,#61314,
#61315,#61316,#61317,#61318,#61319,#61320,#61321,#61322,#61323,#61324,#61325,
#61326,#61327,#61328,#61329,#61330,#61331,#61332,#61333,#61334,#61335,#61336,
#61337,#61338,#61339,#61340,#61341,#61342,#61343,#61344,#61345,#61346,#61347),
 .UNSPECIFIED.,.F.,.F.,(4,2,2,2,2,2,2,2,2,2,2,2,2,2,2,2,2,2,2,2,2,2,2,2,
2,2,2,2,2,2,2,2,2,2,2,2,2,2,2,2,2,2,2,2,2,2,2,2,2,2,2,4),(-1.05003427160778,
-1.04435856196008,-1.03486818366525,-0.999945685105154,-0.979630166743616,
-0.962404972765004,-0.947011042222545,-0.90492026072272,-0.889545514766985,
-0.878047724810931,-0.868744437208028,-0.831882697078646,-0.812124960359172,
-0.795141543650289,-0.779648118856279,-0.739172494515501,-0.723238453872111,
-0.711491071959062,-0.702274075222173,-0.668567244734658,-0.647227292105553,
-0.62956556934539,-0.614482386638978,-0.586107510929279,-0.554588074280767,
-0.543729090856765,-0.534118059507347,-0.522630917087615,-0.495470415892834,
-0.47030772509645,-0.455171105694208,-0.436950734071715,-0.385470085972787,
-0.375561409040591,-0.365137513394907,-0.333740001661664,-0.304258370282471,
-0.289166007387783,-0.271547832939874,-0.250311065427103,-0.216367816106483,
-0.207167837468608,-0.195359300860494,-0.179286661749316,-0.139120348630675,
-0.123592900897117,-0.106648729599607,-0.0869901536427567,-0.0498352677481177,
-0.0405556676512946,-0.0289429427664708,-0.000104312699258312),
 .UNSPECIFIED.) ;
#1392 = B_SPLINE_CURVE_WITH_KNOTS('',3,(#61348,#61349,#61350,#61351,#61352,
#61353,#61354,#61355,#61356,#61357,#61358,#61359,#61360,#61361,#61362,#61363,
#61364,#61365,#61366,#61367,#61368,#61369,#61370,#61371,#61372,#61373,#61374,
#61375,#61376,#61377,#61378,#61379,#61380,#61381,#61382,#61383,#61384,#61385,
#61386,#61387,#61388,#61389,#61390,#61391,#61392,#61393,#61394,#61395,#61396,
#61397,#61398,#61399,#61400,#61401,#61402,#61403,#61404,#61405,#61406,#61407,
#61408,#61409,#61410,#61411,#61412,#61413,#61414,#61415,#61416,#61417,#61418,
#61419,#61420,#61421,#61422,#61423,#61424,#61425,#61426,#61427,#61428,#61429,
#61430,#61431,#61432,#61433,#61434,#61435,#61436,#61437,#61438,#61439,#61440,
#61441,#61442,#61443,#61444,#61445,#61446,#61447,#61448,#61449,#61450,#61451,
#61452,#61453),.UNSPECIFIED.,.F.,.F.,(4,2,2,2,2,2,2,2,2,2,2,2,2,2,2,2,2,
2,2,2,2,2,2,2,2,2,2,2,2,2,2,2,2,2,2,2,2,2,2,2,2,2,2,2,2,2,2,2,2,2,2,2,4),
(0.0589262539191868,0.0674589489708446,0.0878852571293232,0.105172489890227,
0.12056093050769,0.163102704451498,0.178378182981949,0.189840085832997,
0.199222968064391,0.230895882994569,0.253023047339911,0.271050725853291,
0.286344983340089,0.313636635725664,0.34571657438274,0.356950670003054,
0.366493554486396,0.40137455207624,0.421753053350218,0.439050689179136,
0.454579718139182,0.496016837231611,0.511704630651829,0.523360210578599,
0.532708319661394,0.565093236046014,0.586944265165279,0.604857738723409,
0.620006820866124,0.647380229141851,0.679455188035899,0.69068762666048,
0.700210850991282,0.735277934835015,0.755613916385321,0.772894683574981,
0.788428618510123,0.829762639212868,0.845484365887109,0.85715598102644,
0.866503864136571,0.898970769041028,0.920811093617175,0.938725579502742,
0.953886202071171,0.981483984745242,1.00652350405074,1.02157450004231,1.03047164643318,
1.04645508624164,1.07979589234157,1.10149951924504,1.10920986980175),
 .UNSPECIFIED.) ;
#1393 = B_SPLINE_CURVE_WITH_KNOTS('',3,(#61456,#61457,#61458,#61459,#61460,
#61461,#61462,#61463,#61464,#61465,#61466,#61467,#61468,#61469,#61470,#61471,
#61472,#61473,#61474,#61475,#61476,#61477,#61478,#61479,#61480,#61481,#61482,
#61483,#61484,#61485,#61486,#61487,#61488,#61489,#61490,#61491,#61492,#61493,
#61494,#61495,#61496,#61497,#61498,#61499,#61500,#61501,#61502,#61503,#61504,
#61505,#61506,#61507,#61508,#61509,#61510,#61511,#61512,#61513,#61514,#61515,
#61516,#61517,#61518,#61519,#61520,#61521,#61522,#61523,#61524,#61525,#61526,
#61527,#61528,#61529),.UNSPECIFIED.,.F.,.F.,(4,2,2,2,2,2,2,2,2,2,2,2,2,
2,2,2,2,2,2,2,2,2,2,2,2,2,2,2,2,2,2,2,2,2,2,2,4),(0.458271301746286,0.459696961893322,
0.50071918436547,0.529866039232826,0.545453324099051,0.561854599946403,
0.605115484680842,0.636907063955616,0.646775116783392,0.656555485465506,
0.68508855298933,0.733440945751511,0.749423771495339,0.765306871599009,
0.800337081203133,0.842743224519512,0.852520067962606,0.862384999107365,
0.894120906034862,0.937386088170665,0.953775264351649,0.969360379418854,
0.998517034301751,1.03957160201334,1.05338169136163,1.06213617398809,1.07537553769902,
1.09358430461608,1.1431151311845,1.15945817017287,1.17506808487596,1.2046248561194,
1.24707412640119,1.25983807041739,1.26860932330893,1.2784677893318,1.29350131041376),
 .UNSPECIFIED.) ;
#1394 = B_SPLINE_CURVE_WITH_KNOTS('',3,(#61530,#61531,#61532,#61533,#61534,
#61535,#61536,#61537,#61538,#61539,#61540,#61541,#61542,#61543,#61544,#61545,
#61546,#61547,#61548,#61549,#61550,#61551,#61552,#61553,#61554,#61555,#61556,
#61557,#61558,#61559,#61560,#61561,#61562,#61563,#61564,#61565,#61566,#61567,
#61568,#61569),.UNSPECIFIED.,.F.,.F.,(4,2,2,2,2,2,2,2,2,2,2,2,2,2,2,2,2,
2,2,4),(0.00015657270929297,0.0264102910096243,0.0485396520684821,0.0670798630069268,
0.0820848444237249,0.103290341817068,0.14701667650591,0.167626528888988,
0.176910384667272,0.187467114579088,0.228394169883757,0.262867798966582,
0.278730545736736,0.294744744645573,0.342796479572657,0.371534998513901,
0.381323072066321,0.391174076235,0.432782250961712,0.458614805141202),
 .UNSPECIFIED.) ;
#1395 = B_SPLINE_CURVE_WITH_KNOTS('',3,(#61570,#61571,#61572,#61573,#61574,
#61575,#61576,#61577,#61578,#61579,#61580,#61581,#61582,#61583,#61584,#61585,
#61586,#61587,#61588,#61589,#61590,#61591,#61592,#61593,#61594,#61595,#61596,
#61597,#61598,#61599,#61600,#61601,#61602,#61603,#61604,#61605,#61606,#61607,
#61608,#61609,#61610,#61611,#61612,#61613,#61614,#61615,#61616,#61617,#61618,
#61619,#61620,#61621,#61622,#61623,#61624,#61625,#61626,#61627,#61628,#61629,
#61630,#61631,#61632,#61633,#61634,#61635,#61636,#61637,#61638,#61639,#61640,
#61641,#61642,#61643,#61644,#61645,#61646,#61647,#61648,#61649,#61650,#61651,
#61652,#61653,#61654,#61655,#61656,#61657,#61658,#61659,#61660,#61661,#61662,
#61663,#61664,#61665,#61666,#61667,#61668,#61669,#61670,#61671,#61672,#61673,
#61674,#61675,#61676,#61677,#61678,#61679,#61680,#61681,#61682,#61683),
 .UNSPECIFIED.,.F.,.F.,(4,2,2,2,2,2,2,2,2,2,2,2,2,2,2,2,2,2,2,2,2,2,2,2,
2,2,2,2,2,2,2,2,2,2,2,2,2,2,2,2,2,2,2,2,2,2,2,2,2,2,2,2,2,2,2,2,4),(1.29372393529934,
1.29389165145828,1.3477247698968,1.36338665343711,1.37942178206577,1.41593890161886,
1.45496340266735,1.46501581980054,1.47451571088236,1.49830469099948,1.55362642680886,
1.56923105143439,1.58534631717237,1.60551642460622,1.64611486918859,1.66400744466805,
1.67300503360996,1.68400464949734,1.69766791991536,1.73364309516177,1.76059251207417,
1.7759435724897,1.79246065053425,1.82718944538032,1.86605176840251,1.87611448862571,
1.88560409335675,1.90924819107751,1.96483131168275,1.9804314858423,1.99656502026702,
2.01673445888671,2.05750711527526,2.07521596593425,2.08411509894518,2.09513299955481,
2.10882816573146,2.14503183083195,2.17171024741712,2.1870413249484,2.20361151984989,
2.23883311592371,2.27693116894822,2.28705230069124,2.2964556708009,2.31912953096445,
2.36344520140104,2.38298311665709,2.39778152172152,2.41710519578955,2.44103323028988,
2.48166690739291,2.49222908946604,2.50146856752791,2.52151851403579,2.574412876524,
2.58747754236347),.UNSPECIFIED.) ;
#1396 = B_SPLINE_CURVE_WITH_KNOTS('',3,(#61685,#61686,#61687,#61688,#61689,
#61690,#61691,#61692,#61693,#61694,#61695,#61696,#61697,#61698,#61699,#61700,
#61701,#61702,#61703,#61704,#61705,#61706,#61707,#61708,#61709,#61710,#61711,
#61712,#61713,#61714,#61715,#61716,#61717,#61718,#61719,#61720,#61721,#61722,
#61723,#61724,#61725,#61726,#61727,#61728,#61729,#61730,#61731,#61732,#61733,
#61734,#61735,#61736,#61737,#61738,#61739,#61740,#61741,#61742,#61743,#61744,
#61745,#61746,#61747,#61748,#61749,#61750,#61751,#61752,#61753,#61754,#61755,
#61756,#61757,#61758,#61759,#61760,#61761,#61762,#61763,#61764,#61765,#61766,
#61767,#61768,#61769,#61770,#61771,#61772,#61773,#61774,#61775,#61776,#61777,
#61778,#61779,#61780,#61781,#61782,#61783,#61784,#61785,#61786,#61787,#61788,
#61789,#61790,#61791,#61792,#61793,#61794),.UNSPECIFIED.,.F.,.F.,(4,2,2,
2,2,2,2,2,2,2,2,2,2,2,2,2,2,2,2,2,2,2,2,2,2,2,2,2,2,2,2,2,2,2,2,2,2,2,2,
2,2,2,2,2,2,2,2,2,2,2,2,2,2,2,4),(9.99999998198343E-7,0.0378677308412848,
0.0606088389240463,0.0794397917309287,0.0944374645074597,0.115242832303476,
0.159678588171962,0.180421250368242,0.189717841754718,0.20025712450469,
0.241313725536981,0.275691031872575,0.291548808371455,0.307567579574782,
0.344798028502518,0.378087372069843,0.390600235981472,0.399387436423962,
0.414136507208067,0.455477455001117,0.483241979914481,0.498731328275587,
0.515301196188564,0.562607862053707,0.581599441470349,0.59518414720667,
0.60393825112704,0.617397357754011,0.658262856211241,0.687993752682849,
0.703616937221341,0.719950329799739,0.769651031232493,0.795776575367118,
0.805452368229739,0.815441140145354,0.855603025458804,0.880503336598619,
0.900310866404954,0.915279375543088,0.934909706911577,0.980303960619791,
1.00221521240317,1.01160984773296,1.02198258948594,1.06436558015494,1.09740872360189,
1.11337248517989,1.12929494759968,1.16539062845426,1.20608183630062,1.21602500675469,
1.22573336956587,1.25257572330547,1.29359998411323),.UNSPECIFIED.) ;
#1397 = B_SPLINE_CURVE_WITH_KNOTS('',3,(#61795,#61796,#61797,#61798,#61799,
#61800,#61801,#61802,#61803,#61804,#61805,#61806,#61807,#61808,#61809,#61810,
#61811,#61812,#61813,#61814,#61815,#61816,#61817,#61818,#61819,#61820,#61821,
#61822,#61823,#61824,#61825,#61826,#61827,#61828,#61829,#61830,#61831,#61832,
#61833,#61834,#61835,#61836,#61837,#61838,#61839,#61840,#61841,#61842,#61843,
#61844,#61845,#61846,#61847,#61848,#61849,#61850,#61851,#61852,#61853,#61854,
#61855,#61856,#61857,#61858,#61859,#61860,#61861,#61862,#61863,#61864,#61865,
#61866,#61867,#61868,#61869,#61870,#61871,#61872,#61873,#61874,#61875,#61876,
#61877,#61878,#61879,#61880,#61881,#61882,#61883,#61884,#61885,#61886,#61887,
#61888,#61889,#61890,#61891,#61892,#61893,#61894,#61895,#61896,#61897,#61898,
#61899,#61900,#61901,#61902,#61903,#61904,#61905,#61906,#61907,#61908,#61909,
#61910),.UNSPECIFIED.,.F.,.F.,(4,2,2,2,2,2,2,2,2,2,2,2,2,2,2,2,2,2,2,2,
2,2,2,2,2,2,2,2,2,2,2,2,2,2,2,2,2,2,2,2,2,2,2,2,2,2,2,2,2,2,2,2,2,2,2,2,
2,4),(1.29377606271217,1.29392351502004,1.34777604763363,1.36343799978644,
1.37947695175275,1.41604465257822,1.45498511301125,1.46504437813709,1.47454088905445,
1.49827556414381,1.5536800943017,1.56928282945217,1.58540627245887,1.6055747008952,
1.64624343008846,1.66406282706303,1.6729658822995,1.68391911069071,1.69749525559918,
1.73287541645481,1.76036773521383,1.7757621088021,1.79220268332038,1.81232231140674,
1.85626750477301,1.87117857076983,1.87992907867113,1.89215835918365,1.92535646145756,
1.96313340070119,1.97908169110938,1.99483064261501,2.02806592004094,2.07109458732773,
2.08135259644495,2.09072853025411,2.1128140568377,2.15696991938091,2.17691336389267,
2.19178871196546,2.21099013704729,2.23460408242267,2.27607538771201,2.28653736585331,
2.29574252189067,2.31597627275637,2.35788951162614,2.38012594925297,2.39504701479166,
2.41264503530438,2.43295434217051,2.47429677095681,2.48857756112717,2.49731826701906,
2.51009738568464,2.52728843814934,2.57252021960535,2.587449001183),
 .UNSPECIFIED.) ;
#1398 = B_SPLINE_CURVE_WITH_KNOTS('',3,(#61912,#61913,#61914,#61915,#61916,
#61917,#61918,#61919,#61920,#61921,#61922,#61923,#61924,#61925,#61926,#61927,
#61928,#61929,#61930,#61931,#61932,#61933,#61934,#61935,#61936,#61937,#61938,
#61939,#61940,#61941,#61942,#61943,#61944,#61945,#61946,#61947,#61948,#61949,
#61950,#61951,#61952,#61953,#61954,#61955,#61956,#61957,#61958,#61959,#61960,
#61961,#61962,#61963,#61964,#61965,#61966,#61967,#61968,#61969,#61970,#61971,
#61972,#61973,#61974,#61975,#61976,#61977,#61978,#61979,#61980,#61981,#61982,
#61983,#61984,#61985,#61986,#61987,#61988,#61989,#61990,#61991,#61992,#61993,
#61994,#61995,#61996,#61997,#61998,#61999,#62000,#62001,#62002,#62003,#62004,
#62005,#62006,#62007,#62008,#62009,#62010,#62011,#62012,#62013,#62014,#62015),
 .UNSPECIFIED.,.F.,.F.,(4,2,2,2,2,2,2,2,2,2,2,2,2,2,2,2,2,2,2,2,2,2,2,2,
2,2,2,2,2,2,2,2,2,2,2,2,2,2,2,2,2,2,2,2,2,2,2,2,2,2,2,4),(-1.05002476366986,
-1.0443211325236,-1.03481859349597,-1.00000617019621,-0.979657693011989,
-0.962416978791812,-0.947023007851114,-0.904875942109422,-0.889518566018222,
-0.87802815988194,-0.868719190779288,-0.831905832730221,-0.812132972524423,
-0.795141696024252,-0.77964689262054,-0.739155899933678,-0.723226180474464,
-0.71148021956807,-0.702259600028155,-0.668586779268195,-0.647233829327134,
-0.629565487276017,-0.614479867209571,-0.586104652776703,-0.554584234200954,
-0.54372403980417,-0.534110324425165,-0.522618767533955,-0.495435388023178,
-0.470356062419595,-0.455209933462259,-0.43701462918738,-0.385701707579139,
-0.375703277640384,-0.365381682155171,-0.334024036953984,-0.30425235752251,
-0.289155087271841,-0.271530862722873,-0.250282382749226,-0.216383491377353,
-0.207179303012565,-0.195374357598536,-0.179310344845435,-0.139098457746932,
-0.123570529204034,-0.106620051208684,-0.0869477113173263,-0.0498534596826706,
-0.040566965275065,-0.0289594292659833,-0.000105410653251608),
 .UNSPECIFIED.) ;
#1399 = B_SPLINE_CURVE_WITH_KNOTS('',3,(#62016,#62017,#62018,#62019,#62020,
#62021,#62022,#62023,#62024,#62025,#62026,#62027,#62028,#62029,#62030,#62031,
#62032,#62033,#62034,#62035,#62036,#62037,#62038,#62039,#62040,#62041,#62042,
#62043,#62044,#62045,#62046,#62047,#62048,#62049,#62050,#62051,#62052,#62053,
#62054,#62055,#62056,#62057,#62058,#62059,#62060,#62061,#62062,#62063,#62064,
#62065,#62066,#62067,#62068,#62069,#62070,#62071,#62072,#62073,#62074,#62075,
#62076,#62077,#62078,#62079,#62080,#62081,#62082,#62083,#62084,#62085,#62086,
#62087,#62088,#62089,#62090,#62091,#62092,#62093,#62094,#62095,#62096,#62097,
#62098,#62099,#62100,#62101,#62102,#62103,#62104,#62105,#62106,#62107,#62108,
#62109,#62110,#62111,#62112,#62113,#62114,#62115,#62116,#62117,#62118,#62119,
#62120,#62121),.UNSPECIFIED.,.F.,.F.,(4,2,2,2,2,2,2,2,2,2,2,2,2,2,2,2,2,
2,2,2,2,2,2,2,2,2,2,2,2,2,2,2,2,2,2,2,2,2,2,2,2,2,2,2,2,2,2,2,2,2,2,2,4),
(0.0589297775460328,0.0652894712739869,0.0867420242877471,0.104468805486226,
0.119547855356985,0.146949856125031,0.178893239915403,0.190095662433324,
0.199605936431439,0.234732066332288,0.255055236302571,0.272327573690126,
0.287848119587509,0.329144758396892,0.344849153091511,0.356511468726538,
0.365881017427153,0.398040119826413,0.419969302454997,0.437918608740246,
0.453078159402929,0.480393408602737,0.512533638082787,0.523779103299443,
0.533305107312649,0.568336299464638,0.588669247427223,0.60594654111988,
0.621480015828052,0.664040370741232,0.679135999295418,0.690524147030703,
0.699981851612583,0.735733289664909,0.755870022630079,0.773067461583054,
0.788646363490021,0.829341590851685,0.845286548425108,0.857057941006012,
0.866376791841605,0.899329554935797,0.920997560296477,0.938843512856045,
0.954028607693655,0.984413321031502,1.00747521618607,1.02192342342242,1.03084004932114,
1.04708845541304,1.07999538023816,1.10158853164967,1.10920453594835),
 .UNSPECIFIED.) ;
#1400 = B_SPLINE_CURVE_WITH_KNOTS('',3,(#62123,#62124,#62125,#62126,#62127,
#62128,#62129,#62130,#62131,#62132,#62133,#62134,#62135,#62136,#62137,#62138,
#62139,#62140,#62141,#62142,#62143,#62144,#62145,#62146,#62147,#62148,#62149,
#62150,#62151,#62152,#62153,#62154,#62155,#62156,#62157,#62158,#62159,#62160,
#62161,#62162,#62163,#62164,#62165,#62166,#62167,#62168,#62169,#62170,#62171,
#62172,#62173,#62174,#62175,#62176,#62177,#62178,#62179,#62180,#62181,#62182,
#62183,#62184,#62185,#62186,#62187,#62188,#62189,#62190,#62191,#62192,#62193,
#62194,#62195,#62196,#62197,#62198,#62199,#62200,#62201,#62202,#62203,#62204,
#62205,#62206,#62207,#62208,#62209,#62210,#62211,#62212,#62213,#62214,#62215,
#62216,#62217,#62218,#62219,#62220,#62221,#62222,#62223,#62224,#62225,#62226),
 .UNSPECIFIED.,.F.,.F.,(4,2,2,2,2,2,2,2,2,2,2,2,2,2,2,2,2,2,2,2,2,2,2,2,
2,2,2,2,2,2,2,2,2,2,2,2,2,2,2,2,2,2,2,2,2,2,2,2,2,2,2,4),(-1.05003008412879,
-1.04431896404847,-1.03481328881548,-1.00002851916316,-0.979671626744206,
-0.962426905678517,-0.947032780484766,-0.90487086648857,-0.889517720277496,
-0.878029080838536,-0.868718700745103,-0.831916430753326,-0.812139837211625,
-0.795146566431792,-0.779651315447274,-0.739156080255804,-0.723227292799457,
-0.71148158843511,-0.702260063727722,-0.668594613438749,-0.647238488275157,
-0.629568461293717,-0.614482141385646,-0.586106536452459,-0.554585569414328,
-0.543725053222038,-0.534110665469483,-0.522618039398998,-0.495429458990086,
-0.47033973122144,-0.455194435549932,-0.436987176613918,-0.385602805275799,
-0.375642806311598,-0.36527583333481,-0.333901495841986,-0.304247482853878,
-0.289149427153854,-0.271522452069984,-0.250267892143036,-0.216390464090898,
-0.207184587899735,-0.195382843131259,-0.179326169847952,-0.139087503231474,
-0.123560589981618,-0.106606992543605,-0.086927419905541,-0.0498625771347933,
-0.0405730962597217,-0.028970261341665,-0.000105645403308168),
 .UNSPECIFIED.) ;
#1401 = B_SPLINE_CURVE_WITH_KNOTS('',3,(#62227,#62228,#62229,#62230,#62231,
#62232,#62233,#62234,#62235,#62236,#62237,#62238,#62239,#62240,#62241,#62242,
#62243,#62244,#62245,#62246,#62247,#62248,#62249,#62250,#62251,#62252,#62253,
#62254,#62255,#62256,#62257,#62258,#62259,#62260,#62261,#62262,#62263,#62264,
#62265,#62266,#62267,#62268,#62269,#62270,#62271,#62272,#62273,#62274,#62275,
#62276,#62277,#62278,#62279,#62280,#62281,#62282,#62283,#62284,#62285,#62286,
#62287,#62288,#62289,#62290,#62291,#62292,#62293,#62294,#62295,#62296,#62297,
#62298,#62299,#62300,#62301,#62302,#62303,#62304,#62305,#62306,#62307,#62308,
#62309,#62310,#62311,#62312,#62313,#62314,#62315,#62316,#62317,#62318,#62319,
#62320,#62321,#62322,#62323,#62324,#62325,#62326,#62327,#62328,#62329,#62330),
 .UNSPECIFIED.,.F.,.F.,(4,2,2,2,2,2,2,2,2,2,2,2,2,2,2,2,2,2,2,2,2,2,2,2,
2,2,2,2,2,2,2,2,2,2,2,2,2,2,2,2,2,2,2,2,2,2,2,2,2,2,2,4),(0.0589305428466179,
0.0672845159977873,0.0878174041535288,0.105155502442307,0.120524223180403,
0.163295642882688,0.178468096249972,0.189885861115552,0.199302354612582,
0.235392943926774,0.255437742804592,0.272590091372826,0.288159982715115,
0.328657569317303,0.344637669732123,0.356422205311361,0.365751083807702,
0.398559148128537,0.420251806610186,0.43810445199171,0.453288864247402,
0.482630270258008,0.514102600365068,0.524650646116702,0.534611151253447,
0.586112101532517,0.604385950945008,0.619637337659203,0.664154967711524,
0.679239299425177,0.69062178060246,0.700081096373092,0.735801621662722,
0.755943121607322,0.77314197730984,0.78871951163143,0.829416287168497,0.845357242850418,
0.857126395520116,0.866445333001415,0.899379873989889,0.921050193673692,
0.938896356258789,0.954080380361352,0.984443454819893,1.00751392957382,
1.02196410313733,1.03088019431753,1.04712650694432,1.08002915852087,1.10161988420202,
1.10923317368641),.UNSPECIFIED.) ;
#1402 = B_SPLINE_CURVE_WITH_KNOTS('',3,(#62332,#62333,#62334,#62335,#62336,
#62337,#62338,#62339,#62340,#62341,#62342,#62343,#62344,#62345,#62346,#62347,
#62348,#62349,#62350,#62351,#62352,#62353,#62354,#62355,#62356,#62357,#62358,
#62359,#62360,#62361,#62362,#62363,#62364,#62365,#62366,#62367,#62368,#62369,
#62370,#62371,#62372,#62373,#62374,#62375,#62376,#62377,#62378,#62379,#62380,
#62381,#62382,#62383,#62384,#62385,#62386,#62387,#62388,#62389,#62390,#62391,
#62392,#62393,#62394,#62395,#62396,#62397,#62398,#62399,#62400,#62401,#62402,
#62403,#62404,#62405,#62406,#62407,#62408,#62409,#62410,#62411,#62412,#62413,
#62414,#62415,#62416,#62417,#62418,#62419,#62420,#62421,#62422,#62423,#62424,
#62425,#62426,#62427,#62428,#62429,#62430,#62431,#62432,#62433,#62434,#62435,
#62436,#62437),.UNSPECIFIED.,.F.,.F.,(4,2,2,2,2,2,2,2,2,2,2,2,2,2,2,2,2,
2,2,2,2,2,2,2,2,2,2,2,2,2,2,2,2,2,2,2,2,2,2,2,2,2,2,2,2,2,2,2,2,2,2,2,4),
(-1.05009743737373,-1.0444142954407,-1.03491901187677,-1.00001404596187,
-0.979686405976698,-0.962453803642405,-0.947056484787095,-0.904943448966669,
-0.889569365922612,-0.878070757400633,-0.868764044760531,-0.831905808769755,
-0.812140071074282,-0.79515101259579,-0.779653833199217,-0.739165661846125,
-0.723229129130369,-0.711479489481218,-0.702259576976015,-0.668553609235896,
-0.647205795595896,-0.629538572785096,-0.614451472915272,-0.58607028319706,
-0.55454366833602,-0.543681971177213,-0.534068151231903,-0.522577375586239,
-0.495405157151037,-0.470348621534463,-0.455196052630545,-0.437033285757907,
-0.414478636632468,-0.384038960855417,-0.374615326660911,-0.363403168420454,
-0.331313186786754,-0.304066188094179,-0.288998088171465,-0.27127773942017,
-0.249796997202879,-0.21655996628468,-0.207312682283666,-0.195649433482483,
-0.179906744369181,-0.13877991492888,-0.123312887067026,-0.106230980957928,
-0.0862570340744459,-0.0502170126684645,-0.0408326493672609,-0.0294865495056169,
-0.00010458719840716),.UNSPECIFIED.) ;
#1403 = B_SPLINE_CURVE_WITH_KNOTS('',3,(#62438,#62439,#62440,#62441,#62442,
#62443,#62444,#62445,#62446,#62447,#62448,#62449,#62450,#62451,#62452,#62453,
#62454,#62455,#62456,#62457,#62458,#62459,#62460,#62461,#62462,#62463,#62464,
#62465,#62466,#62467,#62468,#62469,#62470,#62471,#62472,#62473,#62474,#62475,
#62476,#62477,#62478,#62479,#62480,#62481,#62482,#62483,#62484,#62485,#62486,
#62487,#62488,#62489,#62490,#62491,#62492,#62493,#62494,#62495,#62496,#62497,
#62498,#62499,#62500,#62501,#62502,#62503,#62504,#62505,#62506,#62507,#62508,
#62509,#62510,#62511,#62512,#62513,#62514,#62515,#62516,#62517,#62518,#62519,
#62520,#62521,#62522,#62523,#62524,#62525,#62526,#62527,#62528,#62529,#62530,
#62531,#62532,#62533,#62534,#62535,#62536,#62537,#62538,#62539,#62540,#62541,
#62542,#62543),.UNSPECIFIED.,.F.,.F.,(4,2,2,2,2,2,2,2,2,2,2,2,2,2,2,2,2,
2,2,2,2,2,2,2,2,2,2,2,2,2,2,2,2,2,2,2,2,2,2,2,2,2,2,2,2,2,2,2,2,2,2,2,4),
(0.0589272293900401,0.067488527546277,0.0879063949391725,0.105190876153072,
0.120580062603249,0.163086583564848,0.178370124455571,0.189836172480497,
0.199220285299566,0.230888475691084,0.253019666091311,0.271049193657553,
0.286342783191366,0.313603294782333,0.34571001824462,0.356949024196235,
0.366491537998796,0.40138208509266,0.421757515981374,0.43905423508961,0.454585623739544,
0.496006631946285,0.511701765732417,0.523360784388823,0.532709138807078,
0.565099812285689,0.586948556420365,0.604861666564845,0.620013213321861,
0.647439325735318,0.679473081914327,0.690698573057144,0.700226682596672,
0.735250884255282,0.75560024473867,0.772887397615669,0.788421292124127,
0.829778469040536,0.845493086314554,0.857161780545748,0.866512173995915,
0.898950068658538,0.920801877962503,0.938721682216242,0.953882995774727,
0.981451106708084,1.00651465352988,1.02157299203097,1.03047098559634,1.04645179889171,
1.0797962414394,1.10150145357039,1.10921089576887),.UNSPECIFIED.) ;
#1404 = B_SPLINE_CURVE_WITH_KNOTS('',3,(#62545,#62546,#62547,#62548,#62549,
#62550,#62551,#62552,#62553,#62554,#62555,#62556,#62557,#62558,#62559,#62560,
#62561,#62562,#62563,#62564,#62565,#62566,#62567,#62568,#62569,#62570,#62571,
#62572,#62573,#62574,#62575,#62576,#62577,#62578,#62579,#62580,#62581,#62582,
#62583,#62584,#62585,#62586,#62587,#62588,#62589,#62590,#62591,#62592,#62593,
#62594,#62595,#62596,#62597,#62598,#62599,#62600,#62601,#62602,#62603,#62604,
#62605,#62606,#62607,#62608,#62609,#62610,#62611,#62612,#62613,#62614,#62615,
#62616,#62617,#62618,#62619,#62620,#62621,#62622,#62623,#62624,#62625,#62626,
#62627,#62628,#62629,#62630,#62631,#62632,#62633,#62634,#62635,#62636,#62637,
#62638,#62639,#62640,#62641,#62642,#62643,#62644,#62645,#62646,#62647,#62648,
#62649,#62650),.UNSPECIFIED.,.F.,.F.,(4,2,2,2,2,2,2,2,2,2,2,2,2,2,2,2,2,
2,2,2,2,2,2,2,2,2,2,2,2,2,2,2,2,2,2,2,2,2,2,2,2,2,2,2,2,2,2,2,2,2,2,2,4),
(-1.05009726896819,-1.04440689227039,-1.03490838516155,-1.00003204688939,
-0.979695682343558,-0.962458936406225,-0.947061549754477,-0.904933676652856,
-0.889564086487481,-0.878067365688205,-0.868759104476544,-0.831913581237844,
-0.812143746083211,-0.795152530839052,-0.779654921673552,-0.739162567398497,
-0.723227109103028,-0.711477795798406,-0.702256877846236,-0.668559896246528,
-0.647208528123987,-0.629539470444578,-0.614451662430445,-0.586070287160119,
-0.55454329746179,-0.543681222134124,-0.534066641030603,-0.52257463065588,
-0.495396126215626,-0.470331462097326,-0.455179785820508,-0.43700513146238,
-0.414421650912579,-0.384052129926698,-0.374624326885522,-0.36341951780383,
-0.331372181117148,-0.304071121534662,-0.289000893687606,-0.271282309783265,
-0.249806563201047,-0.216557673856157,-0.207310849350346,-0.195643719865775,
-0.179892400381864,-0.138785413988915,-0.123316229615429,-0.106237128833854,
-0.0862698516545277,-0.0502094735454203,-0.0408267314315204,-0.0294735284731143,
-0.000104884473885925),.UNSPECIFIED.) ;
#1405 = B_SPLINE_CURVE_WITH_KNOTS('',3,(#62651,#62652,#62653,#62654,#62655,
#62656,#62657,#62658,#62659,#62660,#62661,#62662,#62663,#62664,#62665,#62666,
#62667,#62668,#62669,#62670,#62671,#62672,#62673,#62674,#62675,#62676,#62677,
#62678,#62679,#62680,#62681,#62682,#62683,#62684,#62685,#62686,#62687,#62688,
#62689,#62690,#62691,#62692,#62693,#62694,#62695,#62696,#62697,#62698,#62699,
#62700,#62701,#62702,#62703,#62704,#62705,#62706,#62707,#62708,#62709,#62710,
#62711,#62712,#62713,#62714,#62715,#62716,#62717,#62718,#62719,#62720,#62721,
#62722,#62723,#62724,#62725,#62726,#62727,#62728,#62729,#62730,#62731,#62732,
#62733,#62734,#62735,#62736,#62737,#62738,#62739,#62740,#62741,#62742,#62743,
#62744,#62745,#62746,#62747,#62748,#62749,#62750,#62751,#62752,#62753,#62754),
 .UNSPECIFIED.,.F.,.F.,(4,2,2,2,2,2,2,2,2,2,2,2,2,2,2,2,2,2,2,2,2,2,2,2,
2,2,2,2,2,2,2,2,2,2,2,2,2,2,2,2,2,2,2,2,2,2,2,2,2,2,2,4),(0.0589549240516137,
0.0851958477970781,0.103550850472164,0.118668784507955,0.163514220667212,
0.178609712524909,0.189990117089629,0.199411350087213,0.235404136686533,
0.2554656216767,0.272623939957196,0.288191317490099,0.328713719397892,0.344681365607318,
0.356459305376491,0.365782713816312,0.390581005212486,0.416498591395869,
0.435959052999002,0.451062007752223,0.475597303193304,0.504307905591082,
0.516065863436386,0.525827296003839,0.536639628375923,0.585236274830679,
0.603855211162292,0.61903599680304,0.664368619002719,0.679310380176029,
0.690625651735391,0.700107017687091,0.735552088727983,0.755764892071041,
0.772990398066607,0.788542736619561,0.829499046965055,0.845339896149365,
0.857062914604454,0.866390041503749,0.899124586325224,0.92085552352727,
0.938722574775654,0.953890511976325,0.982278565287995,1.00670264296543,
1.0215687162022,1.03046723474578,1.04667705716277,1.07977179153917,1.10140738512334,
1.10906469945444),.UNSPECIFIED.) ;
#1406 = B_SPLINE_CURVE_WITH_KNOTS('',3,(#62756,#62757,#62758,#62759,#62760,
#62761,#62762,#62763,#62764,#62765,#62766,#62767,#62768,#62769,#62770,#62771,
#62772,#62773,#62774,#62775,#62776,#62777,#62778,#62779,#62780,#62781,#62782,
#62783,#62784,#62785,#62786,#62787,#62788,#62789,#62790,#62791,#62792,#62793,
#62794,#62795,#62796,#62797,#62798,#62799,#62800,#62801,#62802,#62803,#62804,
#62805,#62806,#62807,#62808,#62809,#62810,#62811,#62812,#62813,#62814,#62815,
#62816,#62817,#62818,#62819,#62820,#62821,#62822,#62823,#62824,#62825,#62826,
#62827,#62828,#62829,#62830,#62831,#62832,#62833,#62834,#62835,#62836,#62837,
#62838,#62839,#62840,#62841,#62842,#62843,#62844,#62845,#62846,#62847,#62848,
#62849,#62850,#62851,#62852,#62853,#62854,#62855,#62856,#62857,#62858,#62859,
#62860,#62861,#62862,#62863,#62864,#62865,#62866,#62867),.UNSPECIFIED.,
 .F.,.F.,(4,2,2,2,2,2,2,2,2,2,2,2,2,2,2,2,2,2,2,2,2,2,2,2,2,2,2,2,2,2,2,
2,2,2,2,2,2,2,2,2,2,2,2,2,2,2,2,2,2,2,2,2,2,2,2,4),(9.99999995666184E-7,
0.0356604468915954,0.070133267113053,0.0860029358249983,0.102035258196422,
0.138479242783618,0.172338809078127,0.184971208474476,0.193753965955692,
0.208347154612707,0.249637057802738,0.277597724849303,0.293098631733098,
0.309636799854698,0.357306543037373,0.37618928683413,0.389726264706006,
0.398478041709008,0.411971492751561,0.452852617873533,0.48252321909239,
0.498145991493354,0.514493440612958,0.558427122283655,0.579863109805348,
0.594462050137506,0.603245437648757,0.615877543116213,0.656167568986894,
0.678164181503244,0.696643297064956,0.711660116607348,0.732993373069633,
0.776520196897853,0.797095232053959,0.806378324128922,0.816947486375974,
0.857796463240435,0.881613343056727,0.900939343464071,0.915911945969393,
0.936054711457947,0.980258017814283,1.00220505651952,1.01160250446526,1.02197120600625,
1.06438132506819,1.09740639518348,1.11336964497618,1.12929361424787,1.16544165924478,
1.20604664522996,1.21599727173067,1.22569914880269,1.2524117708616,1.29358094859399),
 .UNSPECIFIED.) ;
#1407 = B_SPLINE_CURVE_WITH_KNOTS('',3,(#62868,#62869,#62870,#62871,#62872,
#62873,#62874,#62875,#62876,#62877,#62878,#62879,#62880,#62881,#62882,#62883,
#62884,#62885,#62886,#62887,#62888,#62889,#62890,#62891,#62892,#62893,#62894,
#62895,#62896,#62897,#62898,#62899,#62900,#62901,#62902,#62903,#62904,#62905,
#62906,#62907,#62908,#62909,#62910,#62911,#62912,#62913,#62914,#62915,#62916,
#62917,#62918,#62919,#62920,#62921,#62922,#62923,#62924,#62925,#62926,#62927,
#62928,#62929,#62930,#62931,#62932,#62933,#62934,#62935,#62936,#62937,#62938,
#62939,#62940,#62941,#62942,#62943,#62944,#62945,#62946,#62947,#62948,#62949,
#62950,#62951,#62952,#62953,#62954,#62955,#62956,#62957,#62958,#62959,#62960,
#62961,#62962,#62963,#62964,#62965,#62966,#62967,#62968,#62969,#62970,#62971,
#62972,#62973,#62974,#62975,#62976,#62977,#62978,#62979),.UNSPECIFIED.,
 .F.,.F.,(4,2,2,2,2,2,2,2,2,2,2,2,2,2,2,2,2,2,2,2,2,2,2,2,2,2,2,2,2,2,2,
2,2,2,2,2,2,2,2,2,2,2,2,2,2,2,2,2,2,2,2,2,2,2,2,4),(1.29372477504308,1.29392078486775,
1.34771417135715,1.36337948433266,1.37941702445609,1.41594491724888,1.45495248269729,
1.4650070265992,1.47450844368933,1.49830749219453,1.55361694431632,1.56922485042015,
1.58534467078816,1.60551503339217,1.64613979410088,1.66400243912571,1.67299833222239,
1.68400882395125,1.69769229140463,1.73380226128087,1.76064384945758,1.77598994206369,
1.79253106836518,1.82748552452238,1.86593840949346,1.87603382421201,1.88550173505765,
1.90884295174587,1.953307274162,1.97249844204928,1.9873870874903,2.00738698304974,
2.06018929708678,2.07611514395467,2.08494812909607,2.09669278149997,2.12988195170081,
2.16863710080455,2.18455246760019,2.20030743542534,2.2337567200133,2.27655125126105,
2.28684273706431,2.29614776549758,2.31751585780158,2.36591766411947,2.38439846426727,
2.39922231412712,2.41979440095639,2.45845623747862,2.48257741921665,2.49281856811981,
2.50225778233022,2.52451208356163,2.5734104755075,2.58752750405949),
 .UNSPECIFIED.) ;
#1408 = B_SPLINE_CURVE_WITH_KNOTS('',3,(#62982,#62983,#62984,#62985,#62986,
#62987,#62988,#62989,#62990,#62991,#62992,#62993,#62994,#62995,#62996,#62997,
#62998,#62999,#63000,#63001,#63002,#63003,#63004,#63005,#63006,#63007,#63008,
#63009,#63010,#63011,#63012,#63013,#63014,#63015,#63016,#63017,#63018,#63019,
#63020,#63021,#63022,#63023,#63024,#63025,#63026,#63027,#63028,#63029,#63030,
#63031,#63032,#63033,#63034,#63035,#63036,#63037,#63038,#63039,#63040,#63041,
#63042,#63043,#63044,#63045,#63046,#63047,#63048,#63049,#63050,#63051,#63052,
#63053),.UNSPECIFIED.,.F.,.F.,(4,2,2,2,2,2,2,2,2,2,2,2,2,2,2,2,2,2,2,2,
2,2,2,2,2,2,2,2,2,2,2,2,2,2,2,4),(0.458255991027476,0.459769175149047,0.500809246661114,
0.52987537666172,0.54545746136114,0.561868843971101,0.605000429750257,0.636881854988211,
0.646751201848579,0.65653133861299,0.685049665674218,0.733419643225896,
0.749401028417448,0.765287692550303,0.800400729865581,0.842672430761068,
0.852462666429538,0.862314719448503,0.893347021290769,0.937660583205908,
0.953970312708293,0.969607854792279,0.999561963597051,1.04037794907665,
1.05372007222468,1.06247360622918,1.07617407775912,1.0954328549492,1.1449737191145,
1.16086909755882,1.1768498703973,1.21266798211965,1.25342411010337,1.26334590831044,
1.27307733955482,1.29346035014047),.UNSPECIFIED.) ;
#1409 = B_SPLINE_CURVE_WITH_KNOTS('',3,(#63054,#63055,#63056,#63057,#63058,
#63059,#63060,#63061,#63062,#63063,#63064,#63065,#63066,#63067,#63068,#63069,
#63070,#63071,#63072,#63073,#63074,#63075,#63076,#63077,#63078,#63079,#63080,
#63081,#63082,#63083,#63084,#63085,#63086,#63087,#63088,#63089,#63090,#63091),
 .UNSPECIFIED.,.F.,.F.,(4,2,2,2,2,2,2,2,2,2,2,2,2,2,2,2,2,2,4),(0.000157521932395551,
0.0468596001704785,0.0661006226859243,0.0810704747273422,0.101297244207578,
0.146666255253819,0.167568294536989,0.176877493818213,0.187388572022809,
0.228675693240133,0.262938074258254,0.278793151198754,0.294817688832346,
0.342740512631854,0.37155204865316,0.38134278249533,0.39119193768519,0.432818454349516,
0.458634629932413),.UNSPECIFIED.) ;
#1410 = B_SPLINE_CURVE_WITH_KNOTS('',3,(#63092,#63093,#63094,#63095,#63096,
#63097,#63098,#63099,#63100,#63101,#63102,#63103,#63104,#63105,#63106,#63107,
#63108,#63109,#63110,#63111,#63112,#63113,#63114,#63115,#63116,#63117,#63118,
#63119,#63120,#63121,#63122,#63123,#63124,#63125,#63126,#63127,#63128,#63129,
#63130,#63131,#63132,#63133,#63134,#63135,#63136,#63137,#63138,#63139,#63140,
#63141,#63142,#63143,#63144,#63145,#63146,#63147,#63148,#63149,#63150,#63151,
#63152,#63153,#63154,#63155,#63156,#63157,#63158,#63159,#63160,#63161,#63162,
#63163,#63164,#63165,#63166,#63167,#63168,#63169,#63170,#63171,#63172,#63173,
#63174,#63175,#63176,#63177,#63178,#63179,#63180,#63181,#63182,#63183,#63184,
#63185,#63186,#63187,#63188,#63189,#63190,#63191,#63192,#63193,#63194,#63195,
#63196,#63197,#63198,#63199,#63200,#63201,#63202,#63203,#63204,#63205),
 .UNSPECIFIED.,.F.,.F.,(4,2,2,2,2,2,2,2,2,2,2,2,2,2,2,2,2,2,2,2,2,2,2,2,
2,2,2,2,2,2,2,2,2,2,2,2,2,2,2,2,2,2,2,2,2,2,2,2,2,2,2,2,2,2,2,2,4),(1.29353464663662,
1.29372323750481,1.3475200935386,1.36318078637633,1.3792129271178,1.4157123566257,
1.45474845020589,1.46479785145263,1.47429790587587,1.49810584329248,1.55338296284456,
1.56898695054761,1.58509875748223,1.60526577596705,1.64584584633556,1.66374549430997,
1.67274276260631,1.68373842464409,1.69739536328701,1.73333585412455,1.76030822097165,
1.77565954125108,1.79217111565895,1.82686267755522,1.86576778396304,1.87582498390098,
1.88531655585195,1.90900852615565,1.96450623220877,1.98010753845972,1.99623433804176,
2.01640149277719,2.05712850439889,2.0748684940139,2.083769679733,2.09477725393964,
2.10845413999575,2.14454097979264,2.17131164699336,2.18664689472732,2.20319667803955,
2.23823665944315,2.27663031234181,2.28672721931645,2.29614763773492,2.31905107458434,
2.36339129187136,2.3827724850076,2.39756729629176,2.41703584670838,2.44128701126702,
2.48333346315426,2.49309918628749,2.50291126105775,2.53199399121754,2.57116295231783,
2.58701551590747),.UNSPECIFIED.) ;
#1411 = B_SPLINE_CURVE_WITH_KNOTS('',3,(#63207,#63208,#63209,#63210,#63211,
#63212,#63213,#63214,#63215,#63216,#63217,#63218,#63219,#63220,#63221,#63222,
#63223,#63224,#63225,#63226,#63227,#63228,#63229,#63230,#63231,#63232,#63233,
#63234,#63235,#63236,#63237,#63238,#63239,#63240,#63241,#63242,#63243,#63244,
#63245,#63246,#63247,#63248,#63249,#63250,#63251,#63252,#63253,#63254,#63255,
#63256,#63257,#63258,#63259,#63260,#63261,#63262,#63263,#63264,#63265,#63266,
#63267,#63268,#63269,#63270,#63271,#63272,#63273,#63274,#63275,#63276,#63277,
#63278,#63279,#63280,#63281,#63282,#63283,#63284,#63285,#63286,#63287,#63288,
#63289,#63290,#63291,#63292,#63293,#63294,#63295,#63296,#63297,#63298,#63299,
#63300,#63301,#63302,#63303,#63304,#63305,#63306,#63307,#63308,#63309,#63310,
#63311,#63312,#63313,#63314,#63315,#63316,#63317,#63318),.UNSPECIFIED.,
 .F.,.F.,(4,2,2,2,2,2,2,2,2,2,2,2,2,2,2,2,2,2,2,2,2,2,2,2,2,2,2,2,2,2,2,
2,2,2,2,2,2,2,2,2,2,2,2,2,2,2,2,2,2,2,2,2,2,2,2,4),(0.687313624506759,0.701487328335802,
0.734261479337814,0.750051238807075,0.766148089620778,0.81322549738789,
0.842574340968868,0.852382433439021,0.862219315435964,0.904004889536085,
0.92830389317549,0.947846979049493,0.962817779763856,0.982722800982418,
1.02701784679081,1.04930750026651,1.0587322877403,1.06905631150427,1.11181989420872,
1.14526522935246,1.16108870200738,1.17715297117741,1.22461845419938,1.25371347403238,
1.2635155650422,1.27336541533369,1.29364526539605,1.3389703542264,1.35871221493386,
1.37367940451246,1.39336987329903,1.41800449057946,1.45892736397017,1.46884990288418,
1.47858448850023,1.50593422863064,1.55335686814451,1.56991071464222,1.58540750930348,
1.61326782805456,1.65461961511933,1.6693127286257,1.67809689378171,1.69064592279205,
1.72409721773405,1.76105117914191,1.77706975302792,1.79292690452481,1.82724216113084,
1.86846855252021,1.87899235408722,1.88829788557021,1.90913766874792,1.95414060546348,
1.97459517707942,1.98102711455768),.UNSPECIFIED.) ;
#1412 = B_SPLINE_CURVE_WITH_KNOTS('',3,(#63319,#63320,#63321,#63322,#63323,
#63324,#63325,#63326,#63327,#63328,#63329,#63330,#63331,#63332,#63333,#63334,
#63335,#63336,#63337,#63338,#63339,#63340,#63341,#63342,#63343,#63344,#63345,
#63346,#63347,#63348,#63349,#63350,#63351,#63352,#63353,#63354,#63355,#63356,
#63357,#63358,#63359,#63360,#63361,#63362,#63363,#63364,#63365,#63366,#63367,
#63368,#63369,#63370,#63371,#63372,#63373,#63374,#63375,#63376,#63377,#63378,
#63379,#63380,#63381,#63382,#63383,#63384,#63385,#63386,#63387,#63388,#63389,
#63390,#63391,#63392,#63393,#63394,#63395,#63396,#63397,#63398,#63399,#63400,
#63401,#63402,#63403,#63404,#63405,#63406,#63407,#63408,#63409,#63410,#63411,
#63412,#63413,#63414,#63415,#63416,#63417,#63418,#63419,#63420,#63421,#63422,
#63423,#63424,#63425,#63426,#63427,#63428,#63429,#63430),.UNSPECIFIED.,
 .F.,.F.,(4,2,2,2,2,2,2,2,2,2,2,2,2,2,2,2,2,2,2,2,2,2,2,2,2,2,2,2,2,2,2,
2,2,2,2,2,2,2,2,2,2,2,2,2,2,2,2,2,2,2,2,2,2,2,2,4),(1.06478356715028,1.07180327287809,
1.11247574840424,1.14270741058747,1.15829491714819,1.17443915661351,1.22546484370874,
1.25084218307447,1.26044459806911,1.27037500521748,1.29413790167027,1.34795120278219,
1.36361751705694,1.37965595762295,1.41617789572498,1.45520969852429,1.46526393074012,
1.47476671412784,1.49857395341122,1.55388273738589,1.5694919492235,1.58561111503344,
1.6057845335696,1.64639377285377,1.66428268995742,1.67328161761124,1.68428615114499,
1.69795741869486,1.73397654054865,1.76090093670943,1.7762537542395,1.79278143882586,
1.82758785260108,1.86632141360382,1.87639668433993,1.88588088324249,1.90943173426611,
1.96518601904047,1.98078348737423,1.99692903713025,2.01710053753758,2.05797545704317,
2.07539889105169,2.08441862376016,2.09541973305932,2.10908212808277,2.14504995500031,
2.17194393727841,2.18729207683965,2.20382663615556,2.23867415361913,2.27743584746603,
2.28750870492712,2.29695511804877,2.32016061345587,2.35872509297639),
 .UNSPECIFIED.) ;
#1413 = B_SPLINE_CURVE_WITH_KNOTS('',3,(#63432,#63433,#63434,#63435,#63436,
#63437,#63438,#63439,#63440,#63441,#63442,#63443,#63444,#63445,#63446,#63447,
#63448,#63449,#63450,#63451,#63452,#63453,#63454,#63455,#63456,#63457,#63458,
#63459,#63460,#63461,#63462,#63463,#63464,#63465,#63466,#63467,#63468,#63469,
#63470,#63471,#63472,#63473,#63474,#63475,#63476,#63477,#63478,#63479,#63480,
#63481,#63482,#63483,#63484,#63485,#63486,#63487,#63488,#63489,#63490,#63491,
#63492,#63493,#63494,#63495,#63496,#63497,#63498,#63499,#63500,#63501,#63502,
#63503,#63504,#63505,#63506,#63507,#63508,#63509,#63510,#63511,#63512,#63513,
#63514,#63515,#63516,#63517,#63518,#63519,#63520,#63521,#63522,#63523,#63524,
#63525,#63526,#63527,#63528,#63529,#63530,#63531,#63532,#63533,#63534,#63535,
#63536,#63537,#63538,#63539),.UNSPECIFIED.,.F.,.F.,(4,2,2,2,2,2,2,2,2,2,
2,2,2,2,2,2,2,2,2,2,2,2,2,2,2,2,2,2,2,2,2,2,2,2,2,2,2,2,2,2,2,2,2,2,2,2,
2,2,2,2,2,2,2,4),(1.00000007181855E-6,0.04310229809024,0.0717672045422332,
0.08732439453051,0.103789024716376,0.152286090776099,0.17089027468351,0.184306167100127,
0.193061495476943,0.206693618374769,0.247627785375472,0.277039577271946,
0.29264137290383,0.309009459026135,0.35841804016586,0.384729351107226,0.39441285665854,
0.404387843685088,0.44471198748948,0.481024551681036,0.496954337073038,
0.512918819493949,0.561699672081028,0.590022275536263,0.599798646286373,
0.609681813849166,0.655828673281404,0.67800925118522,0.696576734116657,
0.711587951794427,0.73278117752412,0.776535005070598,0.797151998635442,
0.806439356836159,0.817003621720242,0.857897183765614,0.881700127370489,
0.90102041460234,0.915994706807118,0.936149449285819,0.980349387386379,
1.00228158178055,1.01167842912849,1.02205077680465,1.06443874400431,1.0974786836724,
1.11344391614396,1.12936979350977,1.16554051541397,1.20611103437312,1.21606544033483,
1.22576567221527,1.25243626665452,1.29365561641325),.UNSPECIFIED.) ;
#1414 = B_SPLINE_CURVE_WITH_KNOTS('',3,(#63540,#63541,#63542,#63543,#63544,
#63545,#63546,#63547,#63548,#63549,#63550,#63551,#63552,#63553,#63554,#63555,
#63556,#63557,#63558,#63559,#63560,#63561,#63562,#63563,#63564,#63565,#63566,
#63567,#63568,#63569,#63570,#63571,#63572,#63573,#63574,#63575,#63576,#63577,
#63578,#63579,#63580,#63581,#63582,#63583,#63584,#63585,#63586,#63587,#63588,
#63589,#63590,#63591,#63592,#63593,#63594,#63595,#63596,#63597,#63598,#63599,
#63600,#63601,#63602,#63603,#63604,#63605,#63606,#63607,#63608,#63609,#63610,
#63611,#63612,#63613,#63614,#63615,#63616,#63617,#63618,#63619,#63620,#63621,
#63622,#63623,#63624,#63625,#63626,#63627,#63628,#63629,#63630,#63631,#63632,
#63633,#63634,#63635,#63636,#63637,#63638,#63639,#63640,#63641,#63642,#63643,
#63644,#63645,#63646,#63647,#63648,#63649,#63650,#63651,#63652,#63653,#63654,
#63655),.UNSPECIFIED.,.F.,.F.,(4,2,2,2,2,2,2,2,2,2,2,2,2,2,2,2,2,2,2,2,
2,2,2,2,2,2,2,2,2,2,2,2,2,2,2,2,2,2,2,2,2,2,2,2,2,2,2,2,2,2,2,2,2,2,2,2,
2,4),(1.29379821101641,1.29399768775507,1.34779007049791,1.36345729999771,
1.37949685755168,1.41603312542794,1.45503519551955,1.46509141930463,1.47459359649869,
1.49839194456128,1.55371126551867,1.56932094490488,1.58544360588411,1.60561564754221,
1.6462548501808,1.6641066737258,1.67310240150238,1.68411759843942,1.69780934608688,
1.73397078218191,1.76077543185893,1.77612055038952,1.79267091237169,1.82770495891532,
1.8660237806458,1.87613061406909,1.88559207883374,1.90883701585102,1.95329571087948,
1.97254754275993,1.98743643684044,2.00737058109388,2.03264141988664,2.0717603407041,
2.08180971648824,2.09133976928329,2.11552667077626,2.17017172158935,2.18579355255731,
2.20186872193732,2.22200592038068,2.26209434447167,2.28054700882681,2.28959063495702,
2.30041802100384,2.31376315994981,2.34766677696385,2.37642573705158,2.3918495327552,
2.4079984449846,2.42810851253555,2.46928473134019,2.48665829153025,2.49566329786108,
2.50677095702138,2.52059062840577,2.5749061863343,2.58760867156725),
 .UNSPECIFIED.) ;
#1415 = B_SPLINE_CURVE_WITH_KNOTS('',3,(#63789,#63790,#63791,#63792,#63793,
#63794,#63795,#63796,#63797,#63798,#63799,#63800,#63801,#63802,#63803,#63804,
#63805,#63806,#63807,#63808,#63809,#63810,#63811,#63812,#63813,#63814,#63815,
#63816,#63817,#63818,#63819,#63820,#63821,#63822,#63823,#63824,#63825,#63826,
#63827,#63828,#63829,#63830,#63831,#63832,#63833,#63834,#63835,#63836,#63837,
#63838,#63839,#63840,#63841,#63842,#63843,#63844,#63845,#63846,#63847,#63848,
#63849,#63850,#63851,#63852,#63853,#63854,#63855,#63856,#63857,#63858,#63859,
#63860,#63861,#63862,#63863,#63864,#63865,#63866,#63867,#63868,#63869,#63870,
#63871,#63872,#63873,#63874,#63875,#63876),.UNSPECIFIED.,.F.,.F.,(4,3,3,
3,3,3,3,3,3,3,3,3,3,3,3,3,3,3,3,3,3,3,3,3,3,3,3,3,3,4),(1.00729736670009E-13,
0.0221235299431287,0.0446174963640137,0.0671263177453645,0.0720884332894729,
0.076729319300931,0.0810427188638101,0.102988755137381,0.124600311552118,
0.142904081042321,0.150434907716478,0.153947638893036,0.15757063756295,
0.178344943855092,0.19730630612935,0.219592370862223,0.224536090126318,
0.229375759206846,0.250039152971169,0.270700034753772,0.285804623298588,
0.292050600364105,0.29668581086518,0.300587021381912,0.320363777276505,
0.334366308076049,0.338839275887222,0.357867994143732,0.375594823992338,
0.378621596831646),.UNSPECIFIED.) ;
#1416 = B_SPLINE_CURVE_WITH_KNOTS('',3,(#63877,#63878,#63879,#63880),
 .UNSPECIFIED.,.F.,.F.,(4,4),(-0.0138074141789072,0.),.UNSPECIFIED.) ;
#1417 = B_SPLINE_CURVE_WITH_KNOTS('',3,(#63881,#63882,#63883,#63884,#63885,
#63886,#63887,#63888,#63889,#63890,#63891,#63892,#63893,#63894,#63895,#63896,
#63897,#63898,#63899,#63900,#63901,#63902,#63903,#63904,#63905,#63906,#63907,
#63908,#63909,#63910,#63911,#63912,#63913,#63914,#63915,#63916,#63917,#63918,
#63919,#63920,#63921,#63922,#63923,#63924,#63925,#63926,#63927,#63928,#63929,
#63930,#63931,#63932,#63933,#63934,#63935,#63936,#63937,#63938,#63939,#63940,
#63941,#63942,#63943,#63944,#63945,#63946,#63947,#63948,#63949,#63950,#63951,
#63952,#63953,#63954,#63955,#63956,#63957,#63958,#63959,#63960,#63961,#63962),
 .UNSPECIFIED.,.F.,.F.,(4,3,3,3,3,3,3,3,3,3,3,3,3,3,3,3,3,3,3,3,3,3,3,3,
3,3,3,4),(0.,0.0192100399714304,0.0384200799428608,0.055785952962528,0.0645126646314185,
0.0684606658468628,0.0884975138119028,0.108898824373168,0.126010884304925,
0.133916812365884,0.137322332661616,0.158397233054311,0.177347064100198,
0.197886036319214,0.205726140874419,0.209179108299885,0.230195957097379,
0.251694413295706,0.267939703341714,0.278006548808323,0.281855553762351,
0.304704589038728,0.321841365496011,0.327921806975797,0.332526964769193,
0.355052364906858,0.373251694867859,0.376839357608217),.UNSPECIFIED.) ;
#1418 = B_SPLINE_CURVE_WITH_KNOTS('',3,(#63964,#63965,#63966,#63967,#63968,
#63969,#63970,#63971,#63972,#63973,#63974,#63975,#63976,#63977,#63978,#63979,
#63980,#63981,#63982,#63983,#63984,#63985,#63986,#63987,#63988,#63989,#63990,
#63991,#63992,#63993,#63994,#63995,#63996,#63997,#63998,#63999,#64000,#64001,
#64002,#64003,#64004,#64005,#64006,#64007,#64008,#64009,#64010,#64011,#64012,
#64013,#64014,#64015,#64016,#64017,#64018,#64019,#64020,#64021,#64022,#64023,
#64024,#64025,#64026,#64027,#64028,#64029,#64030,#64031,#64032,#64033,#64034,
#64035,#64036,#64037,#64038,#64039,#64040,#64041,#64042,#64043,#64044,#64045,
#64046,#64047,#64048,#64049,#64050,#64051),.UNSPECIFIED.,.F.,.F.,(4,3,3,
3,3,3,3,3,3,3,3,3,3,3,3,3,3,3,3,3,3,3,3,3,3,3,3,3,3,4),(5.34946170487962E-14,
0.0220613291570655,0.0446321217778821,0.0636200746038394,0.0720889029016907,
0.0767303357960608,0.0810429822369568,0.102989201024467,0.124600515521827,
0.142904269786994,0.150435349014095,0.153949373757925,0.15757105346863,
0.178345139325078,0.197306306129323,0.218627577357312,0.22453625458675,
0.229375801300445,0.250064043909956,0.270695862024059,0.285804876280239,
0.292050902532932,0.296684879018388,0.30058685343006,0.32036361603869,0.334365964016229,
0.342126630243114,0.361105414329871,0.375594823991594,0.378621596831076),
 .UNSPECIFIED.) ;
#1419 = B_SPLINE_CURVE_WITH_KNOTS('',3,(#64052,#64053,#64054,#64055),
 .UNSPECIFIED.,.F.,.F.,(4,4),(-0.0134973973772337,0.),.UNSPECIFIED.) ;
#1420 = B_SPLINE_CURVE_WITH_KNOTS('',3,(#64056,#64057,#64058,#64059,#64060,
#64061,#64062,#64063,#64064,#64065,#64066,#64067,#64068,#64069,#64070,#64071,
#64072,#64073,#64074,#64075,#64076,#64077,#64078,#64079,#64080,#64081,#64082,
#64083,#64084,#64085,#64086,#64087,#64088,#64089,#64090,#64091,#64092,#64093,
#64094,#64095,#64096,#64097,#64098,#64099,#64100,#64101,#64102,#64103,#64104,
#64105,#64106,#64107,#64108,#64109,#64110,#64111,#64112,#64113,#64114,#64115,
#64116,#64117,#64118,#64119,#64120,#64121,#64122,#64123,#64124,#64125,#64126,
#64127,#64128,#64129,#64130,#64131,#64132,#64133,#64134,#64135,#64136,#64137),
 .UNSPECIFIED.,.F.,.F.,(4,3,3,3,3,3,3,3,3,3,3,3,3,3,3,3,3,3,3,3,3,3,3,3,
3,3,3,4),(3.17409362789655E-14,0.0186663984199296,0.0380218662608163,0.0557872186169466,
0.0645149005559747,0.0684613229714192,0.0884994930860193,0.108901579487709,
0.126012950640826,0.133920158377381,0.13732459125606,0.158399696136409,
0.177347064100177,0.197885577244719,0.205726115616592,0.209179162683429,
0.230011587728157,0.251527757213882,0.267940059171801,0.278007542448308,
0.281856177051311,0.304705056505491,0.321841716096126,0.327925912502187,
0.332533113463834,0.355058546105816,0.37325169486803,0.376841786571624),
 .UNSPECIFIED.) ;
#1421 = B_SPLINE_CURVE_WITH_KNOTS('',3,(#64248,#64249,#64250,#64251,#64252,
#64253,#64254,#64255,#64256,#64257,#64258,#64259,#64260,#64261,#64262,#64263,
#64264,#64265,#64266,#64267,#64268,#64269,#64270,#64271,#64272,#64273,#64274,
#64275,#64276,#64277,#64278,#64279,#64280,#64281,#64282,#64283,#64284,#64285,
#64286,#64287,#64288,#64289,#64290,#64291,#64292,#64293,#64294,#64295,#64296,
#64297,#64298,#64299,#64300,#64301,#64302,#64303,#64304,#64305,#64306,#64307,
#64308,#64309,#64310,#64311,#64312,#64313,#64314,#64315,#64316,#64317,#64318,
#64319,#64320,#64321,#64322,#64323,#64324,#64325,#64326,#64327,#64328,#64329,
#64330,#64331,#64332,#64333,#64334,#64335),.UNSPECIFIED.,.F.,.F.,(4,3,3,
3,3,3,3,3,3,3,3,3,3,3,3,3,3,3,3,3,3,3,3,3,3,3,3,3,3,4),(3.89216075304479E-14,
0.0220602863195691,0.0446307899041969,0.0636188651664292,0.0720885386670094,
0.0767295469819096,0.0810427777397907,0.102989666982509,0.124601161044241,
0.142904125735975,0.15043500853201,0.153948033803229,0.157570731855551,
0.17834498986759,0.197306306129356,0.219592370862149,0.224536128779729,
0.229375769171433,0.249977950539616,0.270610274779213,0.285804685006822,
0.292050674378722,0.296685588060879,0.300586982663982,0.320363742140175,
0.334366234094961,0.338839181965638,0.357867873624408,0.375594823991698,
0.378621596831146),.UNSPECIFIED.) ;
#1422 = B_SPLINE_CURVE_WITH_KNOTS('',3,(#64336,#64337,#64338,#64339),
 .UNSPECIFIED.,.F.,.F.,(4,4),(-0.013736327206518,0.),.UNSPECIFIED.) ;
#1423 = B_SPLINE_CURVE_WITH_KNOTS('',3,(#64340,#64341,#64342,#64343,#64344,
#64345,#64346,#64347,#64348,#64349,#64350,#64351,#64352,#64353,#64354,#64355,
#64356,#64357,#64358,#64359,#64360,#64361,#64362,#64363,#64364,#64365,#64366,
#64367,#64368,#64369,#64370,#64371,#64372,#64373,#64374,#64375,#64376,#64377,
#64378,#64379,#64380,#64381,#64382,#64383,#64384,#64385,#64386,#64387,#64388,
#64389,#64390,#64391,#64392,#64393,#64394,#64395,#64396,#64397,#64398,#64399,
#64400,#64401,#64402,#64403,#64404,#64405,#64406,#64407,#64408,#64409,#64410,
#64411,#64412,#64413,#64414,#64415,#64416,#64417,#64418,#64419,#64420,#64421),
 .UNSPECIFIED.,.F.,.F.,(4,3,3,3,3,3,3,3,3,3,3,3,3,3,3,3,3,3,3,3,3,3,3,3,
3,3,3,4),(0.,0.0192102002368296,0.0384204004736592,0.0580717225209105,0.0645131601572585,
0.0684608111803333,0.0885193531365119,0.108980282713294,0.126011344795134,
0.133917558241526,0.137322834176858,0.158397782796061,0.177347064100205,
0.19793323080713,0.205726138478045,0.209179123689474,0.230012007766502,
0.25152839500007,0.267939779531672,0.278006763196592,0.281855688543813,
0.304103277722834,0.321841441310683,0.327922698413653,0.332528297341932,
0.355053704892794,0.373251694868088,0.376839994115088),.UNSPECIFIED.) ;
#1424 = B_SPLINE_CURVE_WITH_KNOTS('',3,(#64423,#64424,#64425,#64426,#64427,
#64428,#64429,#64430,#64431,#64432,#64433,#64434,#64435,#64436,#64437,#64438,
#64439,#64440,#64441,#64442,#64443,#64444,#64445,#64446,#64447,#64448,#64449,
#64450,#64451,#64452,#64453,#64454,#64455,#64456,#64457,#64458,#64459,#64460,
#64461,#64462,#64463,#64464,#64465,#64466,#64467,#64468,#64469,#64470,#64471,
#64472,#64473,#64474,#64475,#64476,#64477,#64478,#64479,#64480,#64481,#64482,
#64483,#64484,#64485,#64486,#64487,#64488,#64489,#64490,#64491,#64492,#64493,
#64494,#64495,#64496,#64497,#64498,#64499,#64500,#64501,#64502,#64503,#64504,
#64505,#64506,#64507,#64508,#64509,#64510),.UNSPECIFIED.,.F.,.F.,(4,3,3,
3,3,3,3,3,3,3,3,3,3,3,3,3,3,3,3,3,3,3,3,3,3,3,3,3,3,4),(1.00729736669584E-13,
0.0222595867875412,0.0445191735749817,0.0670286285400456,0.0720881472512565,
0.0767287027071146,0.0810425597515141,0.10298847612419,0.124769835483849,
0.142903953145218,0.150434629214208,0.153946551955451,0.157570379123684,
0.178344813275407,0.197306306129324,0.219592370862128,0.224535980326332,
0.229375730713216,0.250039050954983,0.270699830372278,0.285804444287051,
0.292050384204472,0.296686448092421,0.300587128415665,0.320363869220581,
0.334366498947699,0.338839516680554,0.357868298713684,0.375594823991754,
0.378621596831215),.UNSPECIFIED.) ;
#1425 = B_SPLINE_CURVE_WITH_KNOTS('',3,(#64511,#64512,#64513,#64514),
 .UNSPECIFIED.,.F.,.F.,(4,4),(-0.0140044709886694,0.),.UNSPECIFIED.) ;
#1426 = B_SPLINE_CURVE_WITH_KNOTS('',3,(#64515,#64516,#64517,#64518,#64519,
#64520,#64521,#64522,#64523,#64524,#64525,#64526,#64527,#64528,#64529,#64530,
#64531,#64532,#64533,#64534,#64535,#64536,#64537,#64538,#64539,#64540,#64541,
#64542,#64543,#64544,#64545,#64546,#64547,#64548,#64549,#64550,#64551,#64552,
#64553,#64554,#64555,#64556,#64557,#64558,#64559,#64560,#64561,#64562,#64563,
#64564,#64565,#64566,#64567,#64568,#64569,#64570,#64571,#64572,#64573,#64574,
#64575,#64576,#64577,#64578,#64579,#64580,#64581,#64582,#64583,#64584,#64585,
#64586,#64587,#64588,#64589,#64590,#64591,#64592,#64593,#64594,#64595,#64596),
 .UNSPECIFIED.,.F.,.F.,(4,3,3,3,3,3,3,3,3,3,3,3,3,3,3,3,3,3,3,3,3,3,3,3,
3,3,3,4),(0.,0.0185723777350143,0.0384192135306582,0.0580697119410092,0.0645113251116958,
0.0684602738285915,0.0884963219684918,0.10889715448173,0.126009631886339,
0.133914783248957,0.137320974046069,0.158395735620463,0.177347064100166,
0.197886298886923,0.20572613840078,0.209179057335835,0.230196205898824,
0.251694832634604,0.267939505072923,0.278005985924277,0.281855198662189,
0.30470432271361,0.321841165752176,0.327919447372899,0.332523443571899,
0.355048823266237,0.373251694867873,0.376837924097267),.UNSPECIFIED.) ;
#1427 = B_SPLINE_CURVE_WITH_KNOTS('',3,(#64698,#64699,#64700,#64701,#64702,
#64703,#64704,#64705,#64706,#64707,#64708,#64709,#64710,#64711,#64712,#64713,
#64714,#64715,#64716,#64717,#64718,#64719,#64720,#64721,#64722,#64723,#64724,
#64725,#64726,#64727,#64728,#64729,#64730,#64731,#64732,#64733,#64734,#64735,
#64736,#64737,#64738,#64739,#64740,#64741,#64742,#64743,#64744,#64745,#64746,
#64747,#64748,#64749,#64750,#64751,#64752,#64753,#64754,#64755,#64756,#64757,
#64758,#64759,#64760,#64761,#64762,#64763,#64764,#64765,#64766,#64767,#64768,
#64769,#64770,#64771,#64772,#64773,#64774,#64775,#64776,#64777,#64778,#64779),
 .UNSPECIFIED.,.F.,.F.,(4,3,3,3,3,3,3,3,3,3,3,3,3,3,3,3,3,3,3,3,3,3,3,3,
3,3,3,4),(8.24698146814812E-14,0.0185733671595044,0.0384200792770817,0.0580711800398123,
0.0645126636019183,0.068460665561335,0.088497512914447,0.10895830285563,
0.126010883358896,0.133916810832616,0.137322331620615,0.158397231988687,
0.177347064100123,0.197886036524632,0.20572614087733,0.209179108308654,
0.230195957342159,0.251694413674633,0.267939703154651,0.278006548277264,
0.28185555342019,0.304704588782137,0.321841365303597,0.327921804787657,
0.332526961499993,0.355052361625049,0.373251694867978,0.376636436824541),
 .UNSPECIFIED.) ;
#1428 = B_SPLINE_CURVE_WITH_KNOTS('',3,(#64781,#64782,#64783,#64784,#64785,
#64786,#64787,#64788,#64789,#64790,#64791,#64792,#64793,#64794,#64795,#64796,
#64797,#64798,#64799,#64800,#64801,#64802,#64803,#64804,#64805,#64806,#64807,
#64808,#64809,#64810,#64811,#64812,#64813,#64814,#64815,#64816,#64817,#64818,
#64819,#64820,#64821,#64822,#64823,#64824,#64825,#64826,#64827,#64828,#64829,
#64830,#64831,#64832,#64833,#64834,#64835,#64836,#64837,#64838,#64839,#64840,
#64841,#64842,#64843,#64844,#64845,#64846,#64847,#64848,#64849,#64850,#64851,
#64852,#64853,#64854,#64855,#64856,#64857,#64858,#64859,#64860,#64861,#64862,
#64863,#64864,#64865,#64866,#64867,#64868),.UNSPECIFIED.,.F.,.F.,(4,3,3,
3,3,3,3,3,3,3,3,3,3,3,3,3,3,3,3,3,3,3,3,3,3,3,3,3,3,4),(5.76922506808559E-14,
0.0219456891822088,0.0445202601827566,0.0636185159260876,0.0720884335083992,
0.076729319773797,0.0810427189711626,0.102988755333381,0.124770006124255,
0.142904081125542,0.150434907918552,0.1539476396971,0.157570637756284,0.17834494394397,
0.197306306129405,0.219592370862145,0.224536090207257,0.229375759240474,
0.250063857568636,0.270700034922499,0.285804623459792,0.292050600549566,
0.296685810329238,0.300587021291056,0.320363777194857,0.334366307920816,
0.338839275713723,0.357867993938263,0.375594823991326,0.378621596830935),
 .UNSPECIFIED.) ;
#1429 = B_SPLINE_CURVE_WITH_KNOTS('',3,(#64869,#64870,#64871,#64872),
 .UNSPECIFIED.,.F.,.F.,(4,4),(-0.0138072657414553,0.),.UNSPECIFIED.) ;
#1430 = B_SPLINE_CURVE_WITH_KNOTS('',3,(#64873,#64874,#64875,#64876,#64877,
#64878,#64879,#64880,#64881,#64882,#64883,#64884,#64885,#64886,#64887,#64888,
#64889,#64890,#64891,#64892,#64893,#64894,#64895,#64896,#64897,#64898,#64899,
#64900,#64901,#64902,#64903,#64904,#64905,#64906,#64907,#64908,#64909,#64910,
#64911,#64912,#64913,#64914,#64915,#64916,#64917,#64918,#64919,#64920,#64921,
#64922,#64923,#64924,#64925,#64926,#64927,#64928,#64929,#64930,#64931,#64932,
#64933,#64934,#64935,#64936,#64937,#64938,#64939,#64940,#64941,#64942,#64943,
#64944,#64945,#64946,#64947,#64948,#64949,#64950,#64951,#64952,#64953,#64954),
 .UNSPECIFIED.,.F.,.F.,(4,3,3,3,3,3,3,3,3,3,3,3,3,3,3,3,3,3,3,3,3,3,3,3,
3,3,3,4),(3.4584468016288E-14,0.0186663974215186,0.0380218644258986,0.0557872178449611,
0.0645148991924529,0.0684613225756388,0.0885208853153824,0.108982177034512,
0.12601294939485,0.133920156360152,0.137324589860616,0.158399694620118,
0.17734706410018,0.197885577533013,0.205726115643369,0.209179162646155,
0.230436403891952,0.251693645137749,0.267940058956061,0.278007541853836,
0.281856176673541,0.304103707162294,0.321841715883582,0.327925910083578,
0.332533109824159,0.355058542437522,0.37325169486792,0.376642568111857),
 .UNSPECIFIED.) ;
#1431 = B_SPLINE_CURVE_WITH_KNOTS('',3,(#64956,#64957,#64958,#64959,#64960,
#64961,#64962,#64963,#64964,#64965,#64966,#64967,#64968,#64969,#64970,#64971,
#64972,#64973,#64974,#64975,#64976,#64977,#64978,#64979,#64980,#64981,#64982,
#64983,#64984,#64985,#64986,#64987,#64988,#64989,#64990,#64991,#64992,#64993,
#64994,#64995,#64996,#64997,#64998,#64999,#65000,#65001,#65002,#65003,#65004,
#65005,#65006,#65007,#65008,#65009,#65010,#65011,#65012,#65013,#65014,#65015,
#65016,#65017,#65018,#65019,#65020,#65021,#65022,#65023,#65024,#65025,#65026,
#65027,#65028,#65029,#65030,#65031,#65032,#65033,#65034,#65035,#65036,#65037,
#65038,#65039,#65040,#65041,#65042,#65043),.UNSPECIFIED.,.F.,.F.,(4,3,3,
3,3,3,3,3,3,3,3,3,3,3,3,3,3,3,3,3,3,3,3,3,3,3,3,3,3,4),(5.01899537219355E-14,
0.022261021302217,0.0445220426043838,0.063620075545003,0.0720889031852736,
0.0767303364111753,0.081042982385457,0.102989991413452,0.124601296415552,
0.142904269884553,0.150435349267875,0.153949374744116,0.157571053709541,
0.178345139423612,0.197306306129337,0.219592370862122,0.224536254679833,
0.229375801326243,0.249978049553714,0.270610495293834,0.285804876420835,
0.292050902697761,0.296684878486927,0.300586853329895,0.320363615935058,
0.334365963793087,0.338838836352753,0.357867421790014,0.375594823991614,
0.378621596831099),.UNSPECIFIED.) ;
#1432 = B_SPLINE_CURVE_WITH_KNOTS('',3,(#65044,#65045,#65046,#65047),
 .UNSPECIFIED.,.F.,.F.,(4,4),(-0.0134972157492807,0.),.UNSPECIFIED.) ;
#1433 = B_SPLINE_CURVE_WITH_KNOTS('',3,(#65105,#65106,#65107,#65108,#65109,
#65110,#65111,#65112,#65113,#65114,#65115,#65116,#65117,#65118,#65119,#65120,
#65121,#65122,#65123,#65124,#65125,#65126,#65127,#65128,#65129,#65130,#65131,
#65132,#65133,#65134,#65135,#65136,#65137,#65138,#65139,#65140,#65141,#65142,
#65143,#65144,#65145,#65146,#65147,#65148,#65149,#65150,#65151,#65152,#65153,
#65154,#65155,#65156,#65157,#65158,#65159,#65160,#65161,#65162,#65163,#65164,
#65165,#65166,#65167,#65168,#65169,#65170,#65171,#65172,#65173,#65174,#65175,
#65176,#65177,#65178,#65179,#65180,#65181,#65182,#65183,#65184,#65185,#65186),
 .UNSPECIFIED.,.F.,.F.,(4,3,3,3,3,3,3,3,3,3,3,3,3,3,3,3,3,3,3,3,3,3,3,3,
3,3,3,4),(0.,0.0190097553505953,0.0380195107011905,0.0557862339567285,0.06451316109333,
0.0684608114710175,0.0884979543611649,0.108958851497587,0.12601134567694,
0.133917559668794,0.137322835116023,0.15839778382808,0.177347064100199,
0.19788593667367,0.205726138471509,0.209179123708651,0.230195858569767,
0.251694250143536,0.273404722411164,0.278006763619963,0.281855688822625,
0.304103277964979,0.321841441467572,0.327922700231332,0.332528300050647,
0.355053707620067,0.373251694868217,0.376638067983665),.UNSPECIFIED.) ;
#1434 = B_SPLINE_CURVE_WITH_KNOTS('',3,(#65188,#65189,#65190,#65191,#65192,
#65193,#65194,#65195,#65196,#65197,#65198,#65199,#65200,#65201,#65202,#65203,
#65204,#65205,#65206,#65207,#65208,#65209,#65210,#65211,#65212,#65213,#65214,
#65215,#65216,#65217,#65218,#65219,#65220,#65221,#65222,#65223,#65224,#65225,
#65226,#65227,#65228,#65229,#65230,#65231,#65232,#65233,#65234,#65235,#65236,
#65237,#65238,#65239,#65240,#65241,#65242,#65243,#65244,#65245,#65246,#65247,
#65248,#65249,#65250,#65251,#65252,#65253,#65254,#65255,#65256,#65257,#65258,
#65259,#65260,#65261,#65262,#65263,#65264,#65265,#65266,#65267,#65268,#65269,
#65270,#65271,#65272,#65273,#65274,#65275),.UNSPECIFIED.,.F.,.F.,(4,3,3,
3,3,3,3,3,3,3,3,3,3,3,3,3,3,3,3,3,3,3,3,3,3,3,3,3,3,4),(9.162090914368E-15,
0.0220602857583224,0.0446307891766625,0.0636188645106495,0.0720885384695292,
0.0767295465548163,0.0810427776264755,0.102988856337251,0.124600360073992,
0.142904125650606,0.150435008341509,0.153948033057643,0.157570731677898,
0.17834498979002,0.197306306129364,0.219592370862108,0.224536128708099,
0.229375769148714,0.250063899389668,0.27070010984115,0.285804684882141,
0.292050674233032,0.296685588486541,0.300586982738274,0.320363742208751,
0.334366234242714,0.338839182158917,0.357867873880841,0.375594823991314,
0.378621596830874),.UNSPECIFIED.) ;
#1435 = B_SPLINE_CURVE_WITH_KNOTS('',3,(#65276,#65277,#65278,#65279),
 .UNSPECIFIED.,.F.,.F.,(4,4),(-0.0137364598392755,0.),.UNSPECIFIED.) ;
#1436 = B_SPLINE_CURVE_WITH_KNOTS('',3,(#65280,#65281,#65282,#65283,#65284,
#65285,#65286,#65287,#65288,#65289,#65290,#65291,#65292,#65293,#65294,#65295,
#65296,#65297,#65298,#65299,#65300,#65301,#65302,#65303,#65304,#65305,#65306,
#65307,#65308,#65309,#65310,#65311,#65312,#65313,#65314,#65315,#65316,#65317,
#65318,#65319,#65320,#65321,#65322,#65323,#65324,#65325,#65326,#65327,#65328,
#65329,#65330,#65331,#65332,#65333,#65334,#65335,#65336,#65337,#65338,#65339,
#65340,#65341,#65342,#65343,#65344,#65345,#65346,#65347,#65348,#65349,#65350,
#65351,#65352,#65353,#65354,#65355,#65356,#65357,#65358,#65359,#65360,#65361),
 .UNSPECIFIED.,.F.,.F.,(4,3,3,3,3,3,3,3,3,3,3,3,3,3,3,3,3,3,3,3,3,3,3,3,
3,3,3,4),(0.,0.0185723782769974,0.0384192140048957,0.0557851952668067,0.0645113258447557,
0.0684602740353268,0.0884963226141113,0.108897155391316,0.126009632568533,
0.133914784354806,0.137320974779134,0.158395736535551,0.177347064100184,
0.19788629874665,0.205726138406649,0.209179057380608,0.230196205783086,
0.251694832427267,0.267939505171459,0.278005986203941,0.281855198863098,
0.304704322864273,0.321841165865154,0.327919448698485,0.332523445539268,
0.355048825232304,0.373251694867799,0.376632014560555),.UNSPECIFIED.) ;
#1437 = B_SPLINE_CURVE_WITH_KNOTS('',3,(#65363,#65364,#65365,#65366,#65367,
#65368,#65369,#65370,#65371,#65372,#65373,#65374,#65375,#65376,#65377,#65378,
#65379,#65380,#65381,#65382,#65383,#65384,#65385,#65386,#65387,#65388,#65389,
#65390,#65391,#65392,#65393,#65394,#65395,#65396,#65397,#65398,#65399,#65400,
#65401,#65402,#65403,#65404,#65405,#65406,#65407,#65408,#65409,#65410,#65411,
#65412,#65413,#65414,#65415,#65416,#65417,#65418,#65419,#65420,#65421,#65422,
#65423,#65424,#65425,#65426,#65427,#65428,#65429,#65430,#65431,#65432,#65433,
#65434,#65435,#65436,#65437,#65438,#65439,#65440,#65441,#65442,#65443,#65444,
#65445,#65446,#65447,#65448,#65449,#65450),.UNSPECIFIED.,.F.,.F.,(4,3,3,
3,3,3,3,3,3,3,3,3,3,3,3,3,3,3,3,3,3,3,3,3,3,3,3,3,3,4),(9.16209091435299E-15,
0.0219448159624867,0.0445191729753408,0.0636175646195905,0.0720881470932013,
0.0767287023669779,0.0810425596539183,0.102969490401943,0.124769835375746,
0.142903953064144,0.150434629052655,0.15394655131555,0.157570378974426,
0.178344813208512,0.197306306129339,0.219592370862245,0.22453598026394,
0.229375730702232,0.250063743644679,0.270695308858957,0.285804444199926,
0.29205038409226,0.296686448479134,0.300587128478452,0.320363869272083,
0.334366499045275,0.338839516795851,0.357868298847846,0.375594823992585,
0.378621596831857),.UNSPECIFIED.) ;
#1438 = B_SPLINE_CURVE_WITH_KNOTS('',3,(#65451,#65452,#65453,#65454),
 .UNSPECIFIED.,.F.,.F.,(4,4),(-0.0140045813698995,0.),.UNSPECIFIED.) ;
#1439 = B_SPLINE_CURVE_WITH_KNOTS('',3,(#65519,#65520,#65521,#65522,#65523,
#65524,#65525,#65526,#65527,#65528),.UNSPECIFIED.,.F.,.F.,(4,2,2,2,4),(-1.45697727039821,
-1.34636560256276,-1.11265580623236,-0.878946009902128,-0.0207808841702046),
 .UNSPECIFIED.) ;
#1440 = B_SPLINE_CURVE_WITH_KNOTS('',3,(#65610,#65611,#65612,#65613,#65614,
#65615,#65616,#65617,#65618,#65619),.UNSPECIFIED.,.F.,.F.,(4,2,2,2,4),(-0.99020975865206,
-0.4845401415634,-0.346827783328,-0.2091154250925,-0.143938039021296),
 .UNSPECIFIED.) ;
#1441 = B_SPLINE_CURVE_WITH_KNOTS('',3,(#67179,#67180,#67181,#67182,#67183,
#67184,#67185,#67186,#67187,#67188,#67189,#67190,#67191,#67192,#67193,#67194,
#67195,#67196,#67197,#67198,#67199,#67200,#67201,#67202,#67203,#67204,#67205,
#67206,#67207,#67208,#67209,#67210,#67211,#67212,#67213,#67214,#67215,#67216,
#67217,#67218,#67219,#67220,#67221,#67222,#67223,#67224,#67225,#67226,#67227,
#67228,#67229,#67230,#67231,#67232,#67233,#67234,#67235,#67236,#67237,#67238,
#67239,#67240,#67241,#67242,#67243,#67244,#67245,#67246,#67247,#67248,#67249,
#67250,#67251,#67252,#67253,#67254,#67255,#67256,#67257,#67258,#67259,#67260),
 .UNSPECIFIED.,.F.,.F.,(4,3,3,3,3,3,3,3,3,3,3,3,3,3,3,3,3,3,3,3,3,3,3,3,
3,3,3,4),(0.,0.0192098677598375,0.038419735519675,0.0557856515922359,0.0645121321462078,
0.0684605097531964,0.0884970404929436,0.108898162240786,0.12601038770563,
0.133916007890461,0.137321792996603,0.15839663960389,0.177347064100162,
0.19788614178249,0.205726141447246,0.209179089705576,0.230196058990523,
0.251694583642526,0.267939623149047,0.278006322053237,0.28185541093348,
0.304704481917046,0.321841285154721,0.32792085991946,0.33252555045799,0.355050942519894,
0.373251694867745,0.376838869958313),.UNSPECIFIED.) ;
#1442 = B_SPLINE_CURVE_WITH_KNOTS('',3,(#67262,#67263,#67264,#67265),
 .UNSPECIFIED.,.F.,.F.,(4,4),(-0.0138846719219583,0.),.UNSPECIFIED.) ;
#1443 = B_SPLINE_CURVE_WITH_KNOTS('',3,(#67266,#67267,#67268,#67269,#67270,
#67271,#67272,#67273,#67274,#67275,#67276,#67277,#67278,#67279,#67280,#67281,
#67282,#67283,#67284,#67285,#67286,#67287,#67288,#67289,#67290,#67291,#67292,
#67293,#67294,#67295,#67296,#67297,#67298,#67299,#67300,#67301,#67302,#67303,
#67304,#67305,#67306,#67307,#67308,#67309,#67310,#67311,#67312,#67313,#67314,
#67315,#67316,#67317,#67318,#67319,#67320,#67321,#67322,#67323,#67324,#67325,
#67326,#67327,#67328,#67329,#67330,#67331,#67332,#67333,#67334,#67335,#67336,
#67337,#67338,#67339,#67340,#67341,#67342,#67343,#67344,#67345,#67346,#67347,
#67348,#67349,#67350,#67351,#67352,#67353),.UNSPECIFIED.,.F.,.F.,(4,3,3,
3,3,3,3,3,3,3,3,3,3,3,3,3,3,3,3,3,3,3,3,3,3,3,3,3,3,4),(0.,0.0219453428433969,
0.0445198298319151,0.0636181393690862,0.0720883201313736,0.0767290751133605,
0.0810426557911561,0.102988645412413,0.124769940064907,0.142904031581002,
0.150434798366333,0.153947211434901,0.15757053574031,0.178344893157862,
0.197306306129284,0.219592370862123,0.22453604752966,0.229375748144095,
0.250039112563139,0.270699953850697,0.285804554234559,0.292050517273299,
0.296686057701859,0.300587063445754,0.320363814274873,0.334366385364846,
0.338839373506665,0.357868118438046,0.375594823991995,0.378621596831454),
 .UNSPECIFIED.) ;
#1444 = B_SPLINE_CURVE_WITH_KNOTS('',3,(#67447,#67448,#67449,#67450,#67451,
#67452,#67453,#67454,#67455,#67456,#67457,#67458,#67459,#67460,#67461,#67462,
#67463,#67464,#67465,#67466,#67467,#67468,#67469,#67470,#67471,#67472,#67473,
#67474,#67475,#67476,#67477,#67478,#67479,#67480,#67481,#67482,#67483,#67484,
#67485,#67486,#67487,#67488,#67489,#67490,#67491,#67492,#67493,#67494,#67495,
#67496,#67497,#67498,#67499,#67500,#67501,#67502,#67503,#67504,#67505,#67506,
#67507,#67508,#67509,#67510,#67511,#67512,#67513,#67514,#67515,#67516,#67517,
#67518,#67519,#67520,#67521,#67522,#67523,#67524,#67525,#67526,#67527,#67528,
#67529,#67530,#67531,#67532,#67533,#67534),.UNSPECIFIED.,.F.,.F.,(4,3,3,
3,3,3,3,3,3,3,3,3,3,3,3,3,3,3,3,3,3,3,3,3,3,3,3,3,3,4),(0.,0.0219453433760758,
0.0445198304945081,0.0636181399488659,0.0720883203064331,0.0767290754908875,
0.0810426558425648,0.102988645536193,0.124600257382722,0.142904031624236,
0.150434798509977,0.153947211955859,0.157570535874629,0.178344893214354,
0.19730630612937,0.219592370862188,0.224536047596205,0.229375748203205,
0.250039112667709,0.270699954016998,0.285804554457835,0.292050517506586,
0.296686057253529,0.300587063371026,0.320363814208887,0.33436638523497,
0.338839373502662,0.357868118393394,0.375594823991909,0.378621596831355),
 .UNSPECIFIED.) ;
#1445 = B_SPLINE_CURVE_WITH_KNOTS('',3,(#67535,#67536,#67537,#67538,#67539,
#67540,#67541,#67542,#67543,#67544,#67545,#67546,#67547,#67548,#67549,#67550,
#67551,#67552,#67553,#67554,#67555,#67556,#67557,#67558,#67559,#67560,#67561,
#67562,#67563,#67564,#67565,#67566,#67567,#67568,#67569,#67570,#67571,#67572,
#67573,#67574,#67575,#67576,#67577,#67578,#67579,#67580,#67581,#67582,#67583,
#67584,#67585,#67586,#67587,#67588,#67589,#67590,#67591,#67592,#67593,#67594,
#67595,#67596,#67597,#67598,#67599,#67600,#67601,#67602,#67603,#67604,#67605,
#67606,#67607,#67608,#67609,#67610,#67611,#67612,#67613,#67614,#67615,#67616),
 .UNSPECIFIED.,.F.,.F.,(4,3,3,3,3,3,3,3,3,3,3,3,3,3,3,3,3,3,3,3,3,3,3,3,
3,3,3,4),(0.,0.0185729748977862,0.0384197360480747,0.0557856520545772,0.0645121329631303,
0.0684605101522518,0.0884970413840062,0.108898163423802,0.126010388592875,
0.133916009318279,0.137321793976508,0.158396640753416,0.177347064100094,
0.197886141621918,0.205726141448321,0.209179089633135,0.230196058731556,
0.251694583277031,0.267939623337495,0.278006322595857,0.281855411237803,
0.304704482145257,0.321841285325848,0.327920862075213,0.332525553640298,
0.355050945703461,0.37325169486762,0.376634694330848),.UNSPECIFIED.) ;
#1446 = B_SPLINE_CURVE_WITH_KNOTS('',3,(#67617,#67618,#67619,#67620),
 .UNSPECIFIED.,.F.,.F.,(4,4),(-0.0138845519224747,0.),.UNSPECIFIED.) ;
#1447 = B_SPLINE_CURVE_WITH_KNOTS('',3,(#67713,#67714,#67715,#67716,#67717,
#67718,#67719,#67720,#67721,#67722,#67723,#67724,#67725,#67726,#67727,#67728,
#67729,#67730,#67731,#67732,#67733,#67734,#67735,#67736,#67737,#67738,#67739,
#67740,#67741,#67742,#67743,#67744,#67745,#67746,#67747,#67748,#67749,#67750,
#67751,#67752,#67753,#67754,#67755,#67756,#67757,#67758,#67759,#67760,#67761,
#67762,#67763,#67764,#67765,#67766,#67767,#67768,#67769,#67770,#67771,#67772,
#67773,#67774,#67775,#67776,#67777,#67778,#67779,#67780,#67781,#67782,#67783,
#67784,#67785,#67786,#67787,#67788,#67789,#67790,#67791,#67792,#67793,#67794),
 .UNSPECIFIED.,.F.,.F.,(4,3,3,3,3,3,3,3,3,3,3,3,3,3,3,3,3,3,3,3,3,3,3,3,
3,3,3,4),(0.,0.0192105369393153,0.0384210738786305,0.0557868226563222,0.0645142011204561,
0.0684611170545584,0.0884988752384408,0.108900721836266,0.12601230740224,
0.133919117045334,0.137323885863973,0.158398930385445,0.177347064100164,
0.197885723726412,0.205726127529494,0.209179149862764,0.230195640933277,
0.251693894552056,0.267939944540674,0.2780072243568,0.281855977887993,0.304704907132977,
0.321841604066715,0.327924605076911,0.332531152092866,0.355056574852911,
0.373251694867928,0.376841042462691),.UNSPECIFIED.) ;
#1448 = B_SPLINE_CURVE_WITH_KNOTS('',3,(#67796,#67797,#67798,#67799),
 .UNSPECIFIED.,.F.,.F.,(4,4),(-0.0135915899488536,0.),.UNSPECIFIED.) ;
#1449 = B_SPLINE_CURVE_WITH_KNOTS('',3,(#67800,#67801,#67802,#67803,#67804,
#67805,#67806,#67807,#67808,#67809,#67810,#67811,#67812,#67813,#67814,#67815,
#67816,#67817,#67818,#67819,#67820,#67821,#67822,#67823,#67824,#67825,#67826,
#67827,#67828,#67829,#67830,#67831,#67832,#67833,#67834,#67835,#67836,#67837,
#67838,#67839,#67840,#67841,#67842,#67843,#67844,#67845,#67846,#67847,#67848,
#67849,#67850,#67851,#67852,#67853,#67854,#67855,#67856,#67857,#67858,#67859,
#67860,#67861,#67862,#67863,#67864,#67865,#67866,#67867,#67868,#67869,#67870,
#67871,#67872,#67873,#67874,#67875,#67876,#67877,#67878,#67879,#67880,#67881,
#67882,#67883,#67884,#67885,#67886,#67887),.UNSPECIFIED.,.F.,.F.,(4,3,3,
3,3,3,3,3,3,3,3,3,3,3,3,3,3,3,3,3,3,3,3,3,3,3,3,3,3,4),(0.,0.0219466832367342,
0.0445214891325778,0.0636195912571624,0.0720887573235693,0.0767300202064994,
0.0810429003250497,0.102989064460608,0.124770183534997,0.142904214183562,
0.150435214461133,0.153948842921585,0.157570925748775,0.17834508145342,
0.197306306129255,0.21959237086207,0.224536205782459,0.229375788908732,
0.250039268285765,0.270671218902195,0.285804804321276,0.292050816876209,
0.29668514998534,0.300586904076222,0.320363667238304,0.334366074527694,
0.338838978333996,0.357867609002265,0.375594823991774,0.378621596831228),
 .UNSPECIFIED.) ;
#1450 = B_SPLINE_CURVE_WITH_KNOTS('',3,(#67981,#67982,#67983,#67984,#67985,
#67986,#67987,#67988,#67989,#67990,#67991,#67992,#67993,#67994,#67995,#67996,
#67997,#67998,#67999,#68000,#68001,#68002,#68003,#68004,#68005,#68006,#68007,
#68008,#68009,#68010,#68011,#68012,#68013,#68014,#68015,#68016,#68017,#68018,
#68019,#68020,#68021,#68022,#68023,#68024,#68025,#68026,#68027,#68028,#68029,
#68030,#68031,#68032,#68033,#68034,#68035,#68036,#68037,#68038,#68039,#68040,
#68041,#68042,#68043,#68044,#68045,#68046,#68047,#68048,#68049,#68050,#68051,
#68052,#68053,#68054,#68055,#68056,#68057,#68058,#68059,#68060,#68061,#68062,
#68063,#68064,#68065,#68066,#68067,#68068),.UNSPECIFIED.,.F.,.F.,(4,3,3,
3,3,3,3,3,3,3,3,3,3,3,3,3,3,3,3,3,3,3,3,3,3,3,3,3,3,4),(0.,0.02194668392425,
0.0445170790582017,0.0636195919983632,0.0720887575464768,0.076730020689144,
0.0810429004598939,0.102970387789171,0.124601244883116,0.142904214276635,
0.150435214673167,0.153948843786557,0.157570925953124,0.17834508154455,
0.197306306129309,0.219592370862138,0.224536205859184,0.229375788928963,
0.250039268366105,0.270700265757003,0.285804804442111,0.292050817016587,
0.296685149518139,0.300586903991452,0.320363667154172,0.334366074352361,
0.33883897815507,0.357867608757828,0.37559482399194,0.378621596831415),
 .UNSPECIFIED.) ;
#1451 = B_SPLINE_CURVE_WITH_KNOTS('',3,(#68069,#68070,#68071,#68072,#68073,
#68074,#68075,#68076,#68077,#68078,#68079,#68080,#68081,#68082,#68083,#68084,
#68085,#68086,#68087,#68088,#68089,#68090,#68091,#68092,#68093,#68094,#68095,
#68096,#68097,#68098,#68099,#68100,#68101,#68102,#68103,#68104,#68105,#68106,
#68107,#68108,#68109,#68110,#68111,#68112,#68113,#68114,#68115,#68116,#68117,
#68118,#68119,#68120,#68121,#68122,#68123,#68124,#68125,#68126,#68127,#68128,
#68129,#68130,#68131,#68132,#68133,#68134,#68135,#68136,#68137,#68138,#68139,
#68140,#68141,#68142,#68143,#68144,#68145,#68146,#68147,#68148,#68149,#68150),
 .UNSPECIFIED.,.F.,.F.,(4,3,3,3,3,3,3,3,3,3,3,3,3,3,3,3,3,3,3,3,3,3,3,3,
3,3,3,4),(5.54425544496214E-15,0.0185745046356664,0.0384210745687243,0.05578682326015,
0.0645142021869443,0.0684611173773682,0.0886809202670926,0.108900723156817,
0.126012308392645,0.133919118648472,0.137323886999474,0.158398931615403,
0.17734706410013,0.197885723504055,0.20572612751327,0.209179149774556,0.230195640588201,
0.251693894061592,0.267939944783251,0.278007225045027,0.28185597836749,
0.304704907492569,0.321841604336379,0.327924608234368,0.332531156960973,
0.355056579722441,0.373251694867806,0.376640442450949),.UNSPECIFIED.) ;
#1452 = B_SPLINE_CURVE_WITH_KNOTS('',3,(#68151,#68152,#68153,#68154),
 .UNSPECIFIED.,.F.,.F.,(4,4),(-0.0135914441700036,0.),.UNSPECIFIED.) ;
#1453 = B_SPLINE_CURVE_WITH_KNOTS('',3,(#68247,#68248,#68249,#68250,#68251,
#68252,#68253,#68254,#68255,#68256,#68257,#68258,#68259,#68260,#68261,#68262,
#68263,#68264,#68265,#68266,#68267,#68268,#68269,#68270,#68271,#68272,#68273,
#68274,#68275,#68276,#68277,#68278,#68279,#68280,#68281,#68282,#68283,#68284,
#68285,#68286,#68287,#68288,#68289,#68290,#68291,#68292,#68293,#68294,#68295,
#68296,#68297,#68298,#68299,#68300,#68301,#68302,#68303,#68304,#68305,#68306,
#68307,#68308,#68309,#68310,#68311,#68312,#68313,#68314,#68315,#68316,#68317,
#68318,#68319,#68320,#68321,#68322,#68323,#68324,#68325,#68326,#68327,#68328),
 .UNSPECIFIED.,.F.,.F.,(4,3,3,3,3,3,3,3,3,3,3,3,3,3,3,3,3,3,3,3,3,3,3,3,
3,3,3,4),(0.,0.0186653277497641,0.0380199011942217,0.0557863969301571,0.0645134490238413,
0.0684608959992006,0.0886803456960418,0.108899795392883,0.126011612569693,
0.13391799191486,0.137323126160168,0.158398102128668,0.177347064100122,
0.197885878293307,0.205726136246136,0.209179131767074,0.230195799832242,
0.251694153565121,0.267939824662252,0.27800688974131,0.281855768049264,
0.304704749753896,0.32184148603237,0.327923223223719,0.332529082546112,
0.355054494362095,0.373251694867791,0.376840316779234),.UNSPECIFIED.) ;
#1454 = B_SPLINE_CURVE_WITH_KNOTS('',3,(#68330,#68331,#68332,#68333),
 .UNSPECIFIED.,.F.,.F.,(4,4),(-0.0136957314155904,0.),.UNSPECIFIED.) ;
#1455 = B_SPLINE_CURVE_WITH_KNOTS('',3,(#68334,#68335,#68336,#68337,#68338,
#68339,#68340,#68341,#68342,#68343,#68344,#68345,#68346,#68347,#68348,#68349,
#68350,#68351,#68352,#68353,#68354,#68355,#68356,#68357,#68358,#68359,#68360,
#68361,#68362,#68363,#68364,#68365,#68366,#68367,#68368,#68369,#68370,#68371,
#68372,#68373,#68374,#68375,#68376,#68377,#68378,#68379,#68380,#68381,#68382,
#68383,#68384,#68385,#68386,#68387,#68388,#68389,#68390,#68391,#68392,#68393,
#68394,#68395,#68396,#68397,#68398,#68399,#68400,#68401,#68402,#68403,#68404,
#68405,#68406,#68407,#68408,#68409,#68410,#68411,#68412,#68413,#68414,#68415,
#68416,#68417,#68418,#68419,#68420,#68421),.UNSPECIFIED.,.F.,.F.,(4,3,3,
3,3,3,3,3,3,3,3,3,3,3,3,3,3,3,3,3,3,3,3,3,3,3,3,3,3,4),(0.,0.0219461975997884,
0.0445208898907668,0.0636190669205846,0.0720885994199383,0.0767296783629433,
0.0810428117268152,0.102988914619533,0.12477009913424,0.142904150883007,
0.150435066187135,0.153948260028433,0.157570785971653,0.178345015861808,
0.197306306129309,0.219592370862132,0.22453615061269,0.229375774806808,
0.250063923624211,0.270700153327392,0.285804719459338,0.292050715582947,
0.296685462822605,0.300586960556721,0.320363721577313,0.334366190543196,
0.338839126472829,0.357867801974519,0.375594823991889,0.37862159683132),
 .UNSPECIFIED.) ;
#1456 = B_SPLINE_CURVE_WITH_KNOTS('',3,(#68515,#68516,#68517,#68518,#68519,
#68520,#68521,#68522,#68523,#68524,#68525,#68526,#68527,#68528,#68529,#68530,
#68531,#68532,#68533,#68534,#68535,#68536,#68537,#68538,#68539,#68540,#68541,
#68542,#68543,#68544,#68545,#68546,#68547,#68548,#68549,#68550,#68551,#68552,
#68553,#68554,#68555,#68556,#68557,#68558,#68559,#68560,#68561,#68562,#68563,
#68564,#68565,#68566,#68567,#68568,#68569,#68570,#68571,#68572,#68573,#68574,
#68575,#68576,#68577,#68578,#68579,#68580,#68581,#68582,#68583,#68584,#68585,
#68586,#68587,#68588,#68589,#68590,#68591,#68592,#68593,#68594,#68595,#68596,
#68597,#68598,#68599,#68600,#68601,#68602),.UNSPECIFIED.,.F.,.F.,(4,3,3,
3,3,3,3,3,3,3,3,3,3,3,3,3,3,3,3,3,3,3,3,3,3,3,3,3,3,4),(0.,0.022060460365473,
0.0446310129567534,0.0636190676004925,0.0720885996247624,0.0767296788060056,
0.0810428118689025,0.102969752522996,0.124770099274268,0.142904150988042,
0.150435066396597,0.153948260818437,0.15757078615856,0.178345015953213,
0.197306306129363,0.219592370862223,0.224536150685866,0.229375774747225,
0.250039212190931,0.270700153395456,0.285804719367065,0.292050715531525,
0.296685462786989,0.300586960539555,0.32036372156161,0.334366190473772,
0.338839126428367,0.357867801873638,0.375594823992243,0.378621596831708),
 .UNSPECIFIED.) ;
#1457 = B_SPLINE_CURVE_WITH_KNOTS('',3,(#68603,#68604,#68605,#68606,#68607,
#68608,#68609,#68610,#68611,#68612,#68613,#68614,#68615,#68616,#68617,#68618,
#68619,#68620,#68621,#68622,#68623,#68624,#68625,#68626,#68627,#68628,#68629,
#68630,#68631,#68632,#68633,#68634,#68635,#68636,#68637,#68638,#68639,#68640,
#68641,#68642,#68643,#68644,#68645,#68646,#68647,#68648,#68649,#68650,#68651,
#68652,#68653,#68654,#68655,#68656,#68657,#68658,#68659,#68660,#68661,#68662,
#68663,#68664,#68665,#68666,#68667,#68668,#68669,#68670,#68671,#68672,#68673,
#68674,#68675,#68676,#68677,#68678,#68679,#68680,#68681,#68682,#68683,#68684),
 .UNSPECIFIED.,.F.,.F.,(4,3,3,3,3,3,3,3,3,3,3,3,3,3,3,3,3,3,3,3,3,3,3,3,
3,3,3,4),(5.86898037579802E-15,0.0185739485137251,0.0384205879620368,0.0557863974793096,
0.0645134499942184,0.0684608962591978,0.0884982104060516,0.108959169029463,
0.126011613449541,0.133917993341252,0.13732312730515,0.15839810341835,0.177347064100219,
0.19788587809615,0.205726136237969,0.209179131790411,0.230436642512244,
0.251694153234078,0.267939824818217,0.278006890178637,0.281855768372809,
0.304704749996589,0.321841486214424,0.327923225385788,0.332529085719319,
0.355054497541321,0.373251694867928,0.376638087048362),.UNSPECIFIED.) ;
#1458 = B_SPLINE_CURVE_WITH_KNOTS('',3,(#68685,#68686,#68687,#68688),
 .UNSPECIFIED.,.F.,.F.,(4,4),(-0.013695595170466,0.),.UNSPECIFIED.) ;
#1459 = B_SPLINE_CURVE_WITH_KNOTS('',3,(#68726,#68727,#68728,#68729,#68730,
#68731,#68732,#68733,#68734,#68735,#68736,#68737,#68738,#68739,#68740,#68741,
#68742,#68743,#68744,#68745,#68746,#68747,#68748,#68749,#68750,#68751,#68752,
#68753,#68754,#68755,#68756,#68757,#68758,#68759,#68760,#68761,#68762,#68763,
#68764,#68765,#68766,#68767,#68768,#68769,#68770,#68771,#68772,#68773,#68774,
#68775,#68776,#68777,#68778,#68779,#68780,#68781,#68782,#68783,#68784,#68785,
#68786,#68787,#68788,#68789,#68790,#68791,#68792,#68793,#68794,#68795,#68796,
#68797,#68798,#68799,#68800,#68801,#68802,#68803,#68804,#68805,#68806,#68807),
 .UNSPECIFIED.,.F.,.F.,(4,3,3,3,3,3,3,3,3,3,3,3,3,3,3,3,3,3,3,3,3,3,3,3,
3,3,3,4),(0.,0.0185725451103903,0.0384193599840902,0.0557853229985777,0.064511551541945,
0.0684603399778252,0.0884965237471075,0.108897437788649,0.126009844366484,
0.1339151275527,0.137321204015421,0.158395989927514,0.17734706409999,0.197886255136487,
0.205726139728722,0.209179066900041,0.230196165563191,0.251694763856776,
0.267939537791735,0.278006079354413,0.281855257762263,0.304704367038516,
0.321841198995705,0.327919841261155,0.332524030692079,0.355049413867223,
0.373251694867274,0.376632749066777),.UNSPECIFIED.) ;
#1460 = B_SPLINE_CURVE_WITH_KNOTS('',3,(#68809,#68810,#68811,#68812,#68813,
#68814,#68815,#68816,#68817,#68818,#68819,#68820,#68821,#68822,#68823,#68824,
#68825,#68826,#68827,#68828,#68829,#68830,#68831,#68832,#68833,#68834,#68835,
#68836,#68837,#68838,#68839,#68840,#68841,#68842,#68843,#68844,#68845,#68846,
#68847,#68848,#68849,#68850,#68851,#68852,#68853,#68854,#68855,#68856,#68857,
#68858,#68859,#68860,#68861,#68862,#68863,#68864,#68865,#68866,#68867,#68868,
#68869,#68870,#68871,#68872,#68873,#68874,#68875,#68876,#68877,#68878,#68879,
#68880,#68881,#68882,#68883,#68884,#68885,#68886,#68887,#68888,#68889,#68890,
#68891,#68892,#68893,#68894,#68895,#68896),.UNSPECIFIED.,.F.,.F.,(4,3,3,
3,3,3,3,3,3,3,3,3,3,3,3,3,3,3,3,3,3,3,3,3,3,3,3,3,3,4),(0.,0.0219449635441618,
0.0445193572281392,0.0636177258407953,0.0720881956305002,0.0767288068387337,
0.0810425866069912,0.102988523717188,0.12476986522952,0.142903975454487,
0.150434676809413,0.153946737384955,0.157570423094632,0.178344835953805,
0.197306306129388,0.219592370862226,0.224535999387828,0.229375735630069,
0.250039068149565,0.27069986487445,0.285804475479312,0.292050422080681,
0.296686337887541,0.300587110247004,0.320363854122266,0.334366467833364,
0.338839477495732,0.357868249573945,0.375594823992091,0.378621596831544),
 .UNSPECIFIED.) ;
#1461 = B_SPLINE_CURVE_WITH_KNOTS('',3,(#68897,#68898,#68899,#68900),
 .UNSPECIFIED.,.F.,.F.,(4,4),(-0.0139707365649134,0.),.UNSPECIFIED.) ;
#1462 = B_SPLINE_CURVE_WITH_KNOTS('',3,(#68993,#68994,#68995,#68996,#68997,
#68998,#68999,#69000,#69001,#69002,#69003,#69004,#69005,#69006,#69007,#69008,
#69009,#69010,#69011,#69012,#69013,#69014,#69015,#69016,#69017,#69018,#69019,
#69020,#69021,#69022,#69023,#69024,#69025,#69026,#69027,#69028,#69029,#69030,
#69031,#69032,#69033,#69034,#69035,#69036,#69037,#69038,#69039,#69040,#69041,
#69042,#69043,#69044,#69045,#69046,#69047,#69048,#69049,#69050,#69051,#69052,
#69053,#69054,#69055,#69056,#69057,#69058,#69059,#69060,#69061,#69062,#69063,
#69064,#69065,#69066,#69067,#69068,#69069,#69070,#69071,#69072,#69073,#69074),
 .UNSPECIFIED.,.F.,.F.,(4,3,3,3,3,3,3,3,3,3,3,3,3,3,3,3,3,3,3,3,3,3,3,3,
3,3,3,4),(0.,0.0185725445526958,0.0384193594961247,0.055785322571625,0.0645115507874783,
0.0684603398259577,0.088496523143581,0.108897436913417,0.126009843710094,
0.133915126485099,0.137321203268634,0.158395989100451,0.177347064100127,
0.197886255284734,0.205726139725896,0.209179066906955,0.230196165737754,
0.251694764126909,0.267939537662014,0.278006078980002,0.28185525752262,
0.304704366858893,0.321841198861098,0.327919839794464,0.332524028582538,
0.355049411823982,0.373251694867712,0.376838226244513),.UNSPECIFIED.) ;
#1463 = B_SPLINE_CURVE_WITH_KNOTS('',3,(#69168,#69169,#69170,#69171,#69172,
#69173,#69174,#69175,#69176,#69177,#69178,#69179,#69180,#69181,#69182,#69183,
#69184,#69185,#69186,#69187,#69188,#69189,#69190,#69191,#69192,#69193,#69194,
#69195,#69196,#69197,#69198,#69199,#69200,#69201,#69202,#69203,#69204,#69205,
#69206,#69207,#69208,#69209,#69210,#69211,#69212,#69213,#69214,#69215,#69216,
#69217,#69218,#69219,#69220,#69221,#69222,#69223,#69224,#69225,#69226,#69227,
#69228,#69229,#69230,#69231,#69232,#69233,#69234,#69235,#69236,#69237,#69238,
#69239,#69240,#69241,#69242,#69243,#69244,#69245,#69246,#69247,#69248,#69249,
#69250,#69251,#69252,#69253,#69254,#69255),.UNSPECIFIED.,.F.,.F.,(4,3,3,
3,3,3,3,3,3,3,3,3,3,3,3,3,3,3,3,3,3,3,3,3,3,3,3,3,3,4),(0.,0.0219449640383438,
0.0445193578452532,0.0636177263807443,0.0720881957929118,0.0767288071884963,
0.081042586603963,0.102988523783161,0.124769865235439,0.142903975458875,
0.150434676914754,0.153946737722924,0.157570423195002,0.178344835982706,
0.197306306129181,0.219592370861987,0.224535999451756,0.229375735630213,
0.250039068191406,0.270699864974871,0.285804475544972,0.29205042217151,
0.296686337413507,0.300587110169541,0.320413064822319,0.334366467704069,
0.338839477396653,0.357868249441859,0.375594823991625,0.378621596831076),
 .UNSPECIFIED.) ;
#1464 = B_SPLINE_CURVE_WITH_KNOTS('',3,(#69256,#69257,#69258,#69259),
 .UNSPECIFIED.,.F.,.F.,(4,4),(-0.013970623523499,0.),.UNSPECIFIED.) ;
#1465 = B_SPLINE_CURVE_WITH_KNOTS('',3,(#73267,#73268,#73269,#73270,#73271,
#73272,#73273,#73274,#73275,#73276,#73277,#73278,#73279,#73280,#73281,#73282,
#73283,#73284,#73285,#73286,#73287,#73288,#73289,#73290,#73291,#73292,#73293,
#73294,#73295,#73296),.UNSPECIFIED.,.F.,.F.,(4,2,2,2,2,2,2,2,2,2,2,2,2,
2,4),(5.38322315691615,5.39304224466059,5.44283774773947,5.49094177554178,
5.54078719639314,5.58893137971754,5.63882779437621,5.68701378651527,5.73696225957411,
5.78519165817847,5.83519324032231,5.88346758749165,5.93352331326918,5.96001227251581,
5.9859643020004),.UNSPECIFIED.) ;
#1466 = B_SPLINE_CURVE_WITH_KNOTS('',3,(#73298,#73299,#73300,#73301,#73302,
#73303,#73304,#73305,#73306,#73307,#73308,#73309,#73310,#73311,#73312,#73313,
#73314,#73315,#73316,#73317),.UNSPECIFIED.,.F.,.F.,(4,2,2,2,2,2,2,2,2,4),
(7.31782604883876E-6,0.0263666176495937,0.037553661598818,0.0425964016162713,
0.0454386289948368,0.047407628077252,0.0492660600371864,0.0517020860709678,
0.0562207204627482,0.0621887848993301),.UNSPECIFIED.) ;
#1467 = B_SPLINE_CURVE_WITH_KNOTS('',3,(#73337,#73338,#73339,#73340,#73341,
#73342,#73343,#73344,#73345,#73346,#73347,#73348,#73349,#73350,#73351,#73352,
#73353,#73354,#73355,#73356,#73357,#73358,#73359,#73360,#73361,#73362,#73363,
#73364,#73365,#73366,#73367,#73368,#73369,#73370,#73371,#73372),
 .UNSPECIFIED.,.F.,.F.,(4,2,2,2,2,2,2,2,2,2,2,2,2,2,2,2,2,4),(4.60003021189608,
4.61274167729195,4.66217697523756,4.71002576797143,4.75950232363626,4.80737612312307,
4.85689499325532,4.90479586715314,4.95435812268451,5.00228809284381,5.05189481547456,
5.09985585554143,5.14950813428105,5.19750216765418,5.24720109538024,5.29522999351585,
5.3449766636052,5.38322315691615),.UNSPECIFIED.) ;
#1468 = B_SPLINE_CURVE_WITH_KNOTS('',3,(#73373,#73374,#73375,#73376,#73377,
#73378,#73379,#73380,#73381,#73382,#73383,#73384,#73385,#73386,#73387,#73388,
#73389,#73390,#73391,#73392,#73393,#73394,#73395,#73396,#73397,#73398,#73399,
#73400,#73401,#73402,#73403,#73404,#73405,#73406,#73407,#73408),
 .UNSPECIFIED.,.F.,.F.,(4,2,2,2,2,2,2,2,2,2,2,2,2,2,2,2,2,4),(9.99999999529826E-7,
0.0459602279933998,0.0920695348905101,0.139957279080918,0.189615634502391,
0.237441516424779,0.287034114948666,0.334798867035155,0.384326339251411,
0.432030727703635,0.481493727813977,0.529138554079275,0.578537760391974,
0.626123862656481,0.675459978011906,0.722988232703908,0.772261984819088,
0.778702098235824),.UNSPECIFIED.) ;
#1469 = B_SPLINE_CURVE_WITH_KNOTS('',3,(#73413,#73414,#73415,#73416,#73417,
#73418,#73419,#73420,#73421,#73422,#73423,#73424,#73425,#73426,#73427,#73428,
#73429,#73430,#73431,#73432,#73433,#73434,#73435,#73436,#73437,#73438,#73439,
#73440,#73441,#73442,#73443,#73444,#73445,#73446,#73447,#73448),
 .UNSPECIFIED.,.F.,.F.,(4,2,2,2,2,2,2,2,2,2,2,2,2,2,2,2,2,4),(3.81988880202525,
3.83647397316643,3.88561458706625,3.9333421952396,3.98251645873818,4.03025128324564,
4.07946004725098,4.12720439576857,4.17644854178362,4.22420470701037,4.27348514691473,
4.32125540179386,4.37057307694049,4.41835967007874,4.46771554978086,4.5155207011067,
4.56491578059664,4.60003021189608),.UNSPECIFIED.) ;
#1470 = B_SPLINE_CURVE_WITH_KNOTS('',3,(#73449,#73450,#73451,#73452,#73453,
#73454,#73455,#73456,#73457,#73458,#73459,#73460,#73461,#73462,#73463,#73464,
#73465,#73466,#73467,#73468,#73469,#73470,#73471,#73472,#73473,#73474,#73475,
#73476,#73477,#73478,#73479,#73480,#73481,#73482,#73483,#73484),
 .UNSPECIFIED.,.F.,.F.,(4,2,2,2,2,2,2,2,2,2,2,2,2,2,2,2,2,4),(0.778702098235824,
0.819733360806915,0.868945565724245,0.916360975939174,0.965512348499289,
1.01287278482948,1.06196412844517,1.10927063523921,1.1583027785071,1.20555644572237,
1.25453024216171,1.30173220673077,1.35064853435815,1.39779998148816,1.44665974221353,
1.49376190660287,1.54256602543321,1.55035468946618),.UNSPECIFIED.) ;
#1471 = B_SPLINE_CURVE_WITH_KNOTS('',3,(#73489,#73490,#73491,#73492,#73493,
#73494,#73495,#73496,#73497,#73498,#73499,#73500,#73501,#73502,#73503,#73504,
#73505,#73506,#73507,#73508,#73509,#73510,#73511,#73512,#73513,#73514,#73515,
#73516,#73517,#73518,#73519,#73520,#73521,#73522,#73523,#73524),
 .UNSPECIFIED.,.F.,.F.,(4,2,2,2,2,2,2,2,2,2,2,2,2,2,2,2,2,4),(3.04133107078369,
3.0626282680782,3.11152720317147,3.15928030527985,3.20820694674183,3.25594886385393,
3.30490390645472,3.35263688694587,3.40162102871175,3.44934734517854,3.49836129357941,
3.54608323836105,3.59512771579646,3.64284759626698,3.69192334477632,3.73964347845932,
3.78875126360541,3.81988880202525),.UNSPECIFIED.) ;
#1472 = B_SPLINE_CURVE_WITH_KNOTS('',3,(#73525,#73526,#73527,#73528,#73529,
#73530,#73531,#73532,#73533,#73534,#73535,#73536,#73537,#73538,#73539,#73540,
#73541,#73542,#73543,#73544,#73545,#73546,#73547,#73548,#73549,#73550,#73551,
#73552,#73553,#73554,#73555,#73556,#73557,#73558,#73559,#73560),
 .UNSPECIFIED.,.F.,.F.,(4,2,2,2,2,2,2,2,2,2,2,2,2,2,2,2,2,4),(1.55035468946618,
1.58962019238811,1.63836961642577,1.6853771228589,1.73407282008343,1.78103505537499,
1.82967801319886,1.87659641990022,1.92518764349159,1.97206371785068,2.02060422821941,
2.06743952050657,2.1159303523536,2.16272646696657,2.21116866630124,2.2579272616282,
2.30632188316308,2.31615270446751),.UNSPECIFIED.) ;
#1473 = B_SPLINE_CURVE_WITH_KNOTS('',3,(#73565,#73566,#73567,#73568,#73569,
#73570,#73571,#73572,#73573,#73574,#73575,#73576,#73577,#73578,#73579,#73580,
#73581,#73582,#73583,#73584,#73585,#73586,#73587,#73588,#73589,#73590,#73591,
#73592,#73593,#73594,#73595,#73596,#73597,#73598,#73599,#73600),
 .UNSPECIFIED.,.F.,.F.,(4,2,2,2,2,2,2,2,2,2,2,2,2,2,2,2,2,4),(2.26324251216357,
2.2896302179728,2.33849886420532,2.38628348179271,2.43512592494221,2.48292857175856,
2.5317455424296,2.5795683258518,2.62836058194701,2.67620556889162,2.7249739108993,
2.77284340349392,2.82158867422688,2.86948464897585,2.91820773434636,2.96598983399257,
3.014861761022,3.04133107078369),.UNSPECIFIED.) ;
#1474 = B_SPLINE_CURVE_WITH_KNOTS('',3,(#73601,#73602,#73603,#73604,#73605,
#73606,#73607,#73608,#73609,#73610,#73611,#73612,#73613,#73614,#73615,#73616,
#73617,#73618,#73619,#73620,#73621,#73622,#73623,#73624,#73625,#73626,#73627,
#73628,#73629,#73630,#73631,#73632,#73633,#73634,#73635,#73636),
 .UNSPECIFIED.,.F.,.F.,(4,2,2,2,2,2,2,2,2,2,2,2,2,2,2,2,2,4),(2.31615270446751,
2.35304467118319,2.40139277552237,2.44808152112438,2.49638417176711,2.54304069176822,
2.59129895195733,2.63792511380657,2.68614004325833,2.73273776341155,2.78091041497174,
2.82838060378041,2.87561838875644,2.92303320166402,2.97026178624372,3.01762223630918,
3.06484368446366,3.07757844456771),.UNSPECIFIED.) ;
#1475 = B_SPLINE_CURVE_WITH_KNOTS('',3,(#73641,#73642,#73643,#73644,#73645,
#73646,#73647,#73648,#73649,#73650,#73651,#73652,#73653,#73654,#73655,#73656,
#73657,#73658,#73659,#73660,#73661,#73662,#73663,#73664,#73665,#73666,#73667,
#73668,#73669,#73670,#73671,#73672,#73673,#73674,#73675,#73676),
 .UNSPECIFIED.,.F.,.F.,(4,2,2,2,2,2,2,2,2,2,2,2,2,2,2,2,2,4),(1.4846964099853,
1.5157609729567,1.56486470780561,1.61258494268306,1.66165674452716,1.70937703638255,
1.75841766745033,1.80614033275151,1.85515053221796,1.90287787662182,1.95185836460461,
1.9995926780924,2.04854416046925,2.09628771266648,2.14521088665979,2.19296592239185,
2.24186148284303,2.26324251216357),.UNSPECIFIED.) ;
#1476 = B_SPLINE_CURVE_WITH_KNOTS('',3,(#73677,#73678,#73679,#73680,#73681,
#73682,#73683,#73684,#73685,#73686,#73687,#73688,#73689,#73690,#73691,#73692,
#73693,#73694,#73695,#73696,#73697,#73698,#73699,#73700,#73701,#73702,#73703,
#73704,#73705,#73706,#73707,#73708,#73709,#73710,#73711,#73712),
 .UNSPECIFIED.,.F.,.F.,(4,2,2,2,2,2,2,2,2,2,2,2,2,2,2,2,2,4),(3.07757844456771,
3.11215082170642,3.15936717543428,3.20662208779349,3.25383536010487,3.30103917439352,
3.34825134234439,3.39540522519537,3.44261822307777,3.48972338187794,3.53693909467871,
3.58399677848582,3.63121703572986,3.67822853616582,3.72545510626173,3.7724217583735,
3.81965634357723,3.83617648296158),.UNSPECIFIED.) ;
#1477 = B_SPLINE_CURVE_WITH_KNOTS('',3,(#73717,#73718,#73719,#73720,#73721,
#73722,#73723,#73724,#73725,#73726,#73727,#73728,#73729,#73730,#73731,#73732,
#73733,#73734,#73735,#73736,#73737,#73738,#73739,#73740,#73741,#73742,#73743,
#73744,#73745,#73746,#73747,#73748,#73749,#73750,#73751,#73752),
 .UNSPECIFIED.,.F.,.F.,(4,2,2,2,2,2,2,2,2,2,2,2,2,2,2,2,2,4),(0.704588249065147,
0.739643318471497,0.789033378547931,0.836836191747535,0.886187186262916,
0.933971736098218,0.983284656960893,1.03105316744818,1.08032898034688,1.12808370361566,
1.17732334604404,1.22506655796113,1.27427093778155,1.32200493334144,1.37117492796903,
1.41890201649186,1.46803847277299,1.4846964099853),.UNSPECIFIED.) ;
#1478 = B_SPLINE_CURVE_WITH_KNOTS('',3,(#73753,#73754,#73755,#73756,#73757,
#73758,#73759,#73760,#73761,#73762,#73763,#73764,#73765,#73766,#73767,#73768,
#73769,#73770,#73771,#73772,#73773,#73774,#73775,#73776,#73777,#73778,#73779,
#73780,#73781,#73782,#73783,#73784,#73785,#73786,#73787,#73788),
 .UNSPECIFIED.,.F.,.F.,(4,2,2,2,2,2,2,2,2,2,2,2,2,2,2,2,2,4),(3.83617648296158,
3.86657952665484,3.91382375876177,3.96070489710061,4.00796033396756,4.05480089755955,
4.10206902054539,4.14887052568134,4.1961527380787,4.24291674784165,4.29021437435275,
4.33694249897978,4.38425678626683,4.43095068335512,4.4782828016714,4.5249441762026,
4.57229522208415,4.59332517121579),.UNSPECIFIED.) ;
#1479 = B_SPLINE_CURVE_WITH_KNOTS('',3,(#73795,#73796,#73797,#73798,#73799,
#73800,#73801,#73802,#73803,#73804,#73805,#73806,#73807,#73808,#73809,#73810,
#73811,#73812,#73813,#73814,#73815,#73816,#73817,#73818,#73819,#73820,#73821,
#73822,#73823,#73824,#73825,#73826,#73827,#73828),.UNSPECIFIED.,.F.,.F.,
(4,2,2,2,2,2,2,2,2,2,2,2,2,2,2,2,4),(9.99999993491271E-7,0.0284828516056796,
0.0574221916505215,0.107115030582226,0.155104747126672,0.204751083061182,
0.252708060286527,0.302308985786131,0.350235153921418,0.399791757223437,
0.447689096492581,0.497202458062411,0.545072996594067,0.594544185668009,
0.64238999705136,0.691820068232682,0.704588249065147),.UNSPECIFIED.) ;
#1480 = B_SPLINE_CURVE_WITH_KNOTS('',3,(#73829,#73830,#73831,#73832,#73833,
#73834,#73835,#73836,#73837,#73838,#73839,#73840,#73841,#73842,#73843,#73844,
#73845,#73846,#73847,#73848,#73849,#73850,#73851,#73852,#73853,#73854,#73855,
#73856,#73857,#73858,#73859,#73860,#73861,#73862,#73863,#73864),
 .UNSPECIFIED.,.F.,.F.,(4,2,2,2,2,2,2,2,2,2,2,2,2,2,2,2,2,4),(4.59332517121579,
4.61892582624069,4.66629682621224,4.71289845895872,4.76029037418151,4.80686488058551,
4.85427861235024,4.90082788261854,4.94826427856474,4.99479032010428,5.04225019170015,
5.08875518358285,5.13623929546219,5.18272525768414,5.23023433896211,5.27670333178905,
5.32423808711373,5.35005945872097),.UNSPECIFIED.) ;
#1481 = B_SPLINE_CURVE_WITH_KNOTS('',3,(#73870,#73871,#73872,#73873,#73874,
#73875,#73876,#73877,#73878,#73879,#73880,#73881,#73882,#73883,#73884,#73885,
#73886,#73887,#73888,#73889,#73890,#73891,#73892,#73893),.UNSPECIFIED.,
 .F.,.F.,(4,2,2,2,2,2,2,2,2,2,2,4),(-0.691228479706931,-0.659683515426214,
-0.590402494363344,-0.522681206763571,-0.453350201583115,-0.385661106476045,
-0.316279606507643,-0.248618200834772,-0.179185758627054,-0.111547513813486,
-0.0554456429886268,-9.99999999917733E-7),.UNSPECIFIED.) ;
#1482 = B_SPLINE_CURVE_WITH_KNOTS('',3,(#73896,#73897,#73898,#73899,#73900,
#73901,#73902,#73903,#73904,#73905,#73906,#73907,#73908,#73909,#73910,#73911,
#73912,#73913,#73914,#73915),.UNSPECIFIED.,.F.,.F.,(4,2,2,2,2,2,2,2,2,4),
(-7.84378181003724,-7.77919511183515,-7.71433746063211,-7.64677308418302,
-7.57667425155804,-7.50915779735907,-7.43912043216624,-7.37164984836796,
-7.30167321308063,-7.29122091273785),.UNSPECIFIED.) ;
#1483 = B_SPLINE_CURVE_WITH_KNOTS('',3,(#73920,#73921,#73922,#73923,#73924,
#73925,#73926,#73927,#73928,#73929,#73930,#73931,#73932,#73933,#73934,#73935,
#73936,#73937,#73938,#73939,#73940,#73941,#73942,#73943,#73944,#73945,#73946,
#73947,#73948,#73949,#73950,#73951,#73952,#73953,#73954,#73955),
 .UNSPECIFIED.,.F.,.F.,(4,2,2,2,2,2,2,2,2,2,2,2,2,2,2,2,2,4),(-1.79728453555456,
-1.75567547618576,-1.68676294920706,-1.61863137912338,-1.54967710328783,
-1.4816103119917,-1.41261273732186,-1.34460723868831,-1.27556498377158,
-1.20761709837854,-1.13852894357061,-1.07063481440011,-1.00149969247415,
-0.93365530296354,-0.864472282250888,-0.796673228266311,-0.727441500680126,
-0.691228479706931),.UNSPECIFIED.) ;
#1484 = B_SPLINE_CURVE_WITH_KNOTS('',3,(#73956,#73957,#73958,#73959,#73960,
#73961,#73962,#73963,#73964,#73965,#73966,#73967,#73968,#73969,#73970,#73971,
#73972,#73973,#73974,#73975,#73976,#73977,#73978,#73979,#73980,#73981,#73982,
#73983,#73984,#73985,#73986,#73987,#73988,#73989,#73990,#73991),
 .UNSPECIFIED.,.F.,.F.,(4,2,2,2,2,2,2,2,2,2,2,2,2,2,2,2,2,4),(-7.29122091273785,
-7.23424621011276,-7.16432944604514,-7.09694378135534,-7.02708629245721,
-6.95973951256943,-6.88994058993847,-6.82263007226313,-6.75288902505584,
-6.68561199296562,-6.61592815258376,-6.54868167254206,-6.47905439657241,
-6.4118353764163,-6.34226405216014,-6.27506924073054,-6.20555328814192,
-6.18915326500312),.UNSPECIFIED.) ;
#1485 = B_SPLINE_CURVE_WITH_KNOTS('',3,(#73996,#73997,#73998,#73999,#74000,
#74001,#74002,#74003,#74004,#74005,#74006,#74007,#74008,#74009,#74010,#74011,
#74012,#74013,#74014,#74015,#74016,#74017,#74018,#74019,#74020,#74021,#74022,
#74023,#74024,#74025,#74026,#74027,#74028,#74029,#74030,#74031),
 .UNSPECIFIED.,.F.,.F.,(4,2,2,2,2,2,2,2,2,2,2,2,2,2,2,2,2,4),(-2.90409970887492,
-2.85344626473094,-2.78479167510497,-2.71604260957267,-2.64736463458598,
-2.57870028926952,-2.50999611763196,-2.44141479173892,-2.37268173758173,
-2.30418150908912,-2.23541702550073,-2.16699574561677,-2.0981974363858,
-2.02985272627047,-1.96101835549974,-1.89274760547224,-1.82387510477095,
-1.79728453555456),.UNSPECIFIED.) ;
#1486 = B_SPLINE_CURVE_WITH_KNOTS('',3,(#74032,#74033,#74034,#74035,#74036,
#74037,#74038,#74039,#74040,#74041,#74042,#74043,#74044,#74045,#74046,#74047,
#74048,#74049,#74050,#74051,#74052,#74053,#74054,#74055,#74056,#74057,#74058,
#74059,#74060,#74061,#74062,#74063,#74064,#74065,#74066,#74067),
 .UNSPECIFIED.,.F.,.F.,(4,2,2,2,2,2,2,2,2,2,2,2,2,2,2,2,2,4),(-6.18915326500312,
-6.13837927645232,-6.06891815029146,-6.00176137441837,-5.93235456541957,
-5.86521131128223,-5.79585834613613,-5.72872475630891,-5.65942519626852,
-5.59229727893649,-5.52305071687626,-5.45592435700272,-5.3867304127907,
-5.31960138551605,-5.2504596996016,-5.1833236858355,-5.1142339110082,-5.08964542517064),
 .UNSPECIFIED.) ;
#1487 = B_SPLINE_CURVE_WITH_KNOTS('',3,(#74072,#74073,#74074,#74075,#74076,
#74077,#74078,#74079,#74080,#74081,#74082,#74083,#74084,#74085,#74086,#74087,
#74088,#74089,#74090,#74091,#74092,#74093,#74094,#74095,#74096,#74097,#74098,
#74099,#74100,#74101,#74102,#74103,#74104,#74105,#74106,#74107),
 .UNSPECIFIED.,.F.,.F.,(4,2,2,2,2,2,2,2,2,2,2,2,2,2,2,2,2,4),(-4.01310959987262,
-3.95710163714007,-3.88680966073369,-3.81734501486128,-3.74876820198224,
-3.6793951062838,-3.61081675511574,-3.54153490121183,-3.47295177522944,
-3.40376072516744,-3.33516959884117,-3.26606877167578,-3.19746644656107,
-3.128455104976,-3.05983842638392,-2.99091566358799,-2.92228153757466,-2.90409970887492),
 .UNSPECIFIED.) ;
#1488 = B_SPLINE_CURVE_WITH_KNOTS('',3,(#74108,#74109,#74110,#74111,#74112,
#74113,#74114,#74115,#74116,#74117,#74118,#74119,#74120,#74121,#74122,#74123,
#74124,#74125,#74126,#74127,#74128,#74129,#74130,#74131,#74132,#74133,#74134,
#74135,#74136,#74137,#74138,#74139,#74140,#74141,#74142,#74143),
 .UNSPECIFIED.,.F.,.F.,(4,2,2,2,2,2,2,2,2,2,2,2,2,2,2,2,2,4),(-5.08964542517064,
-5.0470865151152,-4.97804830645332,-4.91088507586657,-4.8418980789635,-4.77471452549557,
-4.70577836312752,-4.63856998568399,-4.56968424315711,-4.50244655150175,
-4.43361076098885,-4.36633930016088,-4.29755292440106,-4.2302432993488,
-4.16150571513528,-4.09415361510854,-4.02546409653717,-3.9911154034222),
 .UNSPECIFIED.) ;
#1489 = B_SPLINE_CURVE_WITH_KNOTS('',3,(#74148,#74149,#74150,#74151,#74152,
#74153,#74154,#74155,#74156,#74157,#74158,#74159,#74160,#74161,#74162,#74163,
#74164,#74165,#74166,#74167,#74168,#74169,#74170,#74171,#74172,#74173,#74174,
#74175,#74176,#74177,#74178,#74179,#74180,#74181,#74182,#74183),
 .UNSPECIFIED.,.F.,.F.,(4,2,2,2,2,2,2,2,2,2,2,2,2,2,2,2,2,4),(-5.12619780738417,
-5.06542824424112,-4.99464397936999,-4.92649998313525,-4.85577983905526,
-4.78768784617287,-4.71703108666039,-4.64898928292674,-4.57839516608918,
-4.51040161405816,-4.43986939573268,-4.37192202842994,-4.3014509658916,
-4.23354758073747,-4.16313693667261,-4.09527518973588,-4.02492423641919,
-4.01310959987262),.UNSPECIFIED.) ;
#1490 = B_SPLINE_CURVE_WITH_KNOTS('',3,(#74184,#74185,#74186,#74187,#74188,
#74189,#74190,#74191,#74192,#74193,#74194,#74195,#74196,#74197,#74198,#74199,
#74200,#74201,#74202,#74203,#74204,#74205,#74206,#74207,#74208,#74209,#74210,
#74211,#74212,#74213,#74214,#74215,#74216,#74217,#74218,#74219),
 .UNSPECIFIED.,.F.,.F.,(4,2,2,2,2,2,2,2,2,2,2,2,2,2,2,2,2,4),(-3.9911154034222,
-3.95806517212602,-3.88942286249412,-3.82211773010324,-3.75332596539371,
-3.68605851423656,-3.61721727138992,-3.54998309857507,-3.48109184883234,
-3.41388649428363,-3.34494477649593,-3.27776374758436,-3.20877115196306,
-3.14160994787275,-3.07256610042072,-3.0054202358165,-2.93632478380748,
-2.89252148335294),.UNSPECIFIED.) ;
#1491 = B_SPLINE_CURVE_WITH_KNOTS('',3,(#74224,#74225,#74226,#74227,#74228,
#74229,#74230,#74231,#74232,#74233,#74234,#74235,#74236,#74237,#74238,#74239,
#74240,#74241,#74242,#74243,#74244,#74245,#74246,#74247,#74248,#74249,#74250,
#74251,#74252,#74253,#74254,#74255,#74256,#74257,#74258,#74259),
 .UNSPECIFIED.,.F.,.F.,(4,2,2,2,2,2,2,2,2,2,2,2,2,2,2,2,2,4),(-6.24525857708354,
-6.18130123341136,-6.10997902666339,-6.0413663967305,-5.97011370244159,
-5.90156390629546,-5.83038011470152,-5.76189210067836,-5.69077658140171,
-5.6223492228121,-5.5513013256323,-5.48293341540393,-5.41195247130259,-5.34364271637003,
-5.27272803887387,-5.2044750543344,-5.13362594117844,-5.12619780738417),
 .UNSPECIFIED.) ;
#1492 = B_SPLINE_CURVE_WITH_KNOTS('',3,(#74260,#74261,#74262,#74263,#74264,
#74265,#74266,#74267,#74268,#74269,#74270,#74271,#74272,#74273,#74274,#74275,
#74276,#74277,#74278,#74279,#74280,#74281,#74282,#74283,#74284,#74285,#74286,
#74287,#74288,#74289,#74290,#74291,#74292,#74293,#74294,#74295),
 .UNSPECIFIED.,.F.,.F.,(4,2,2,2,2,2,2,2,2,2,2,2,2,2,2,2,2,4),(-2.89252148335294,
-2.86918981140948,-2.80004241021797,-2.73291394193786,-2.66371424344966,
-2.59658796980102,-2.52733561255909,-2.46020732011817,-2.3909019212844,
-2.32376750804314,-2.25440865718688,-2.18726414570545,-2.1178514003682,
-2.05069294869569,-1.98122583162893,-1.91404974201738,-1.8445277399499,
-1.7927676458979),.UNSPECIFIED.) ;
#1493 = B_SPLINE_CURVE_WITH_KNOTS('',3,(#74300,#74301,#74302,#74303,#74304,
#74305,#74306,#74307,#74308,#74309,#74310,#74311,#74312,#74313,#74314,#74315,
#74316,#74317,#74318,#74319,#74320,#74321,#74322,#74323,#74324,#74325,#74326,
#74327,#74328,#74329,#74330,#74331,#74332,#74333,#74334,#74335),
 .UNSPECIFIED.,.F.,.F.,(4,2,2,2,2,2,2,2,2,2,2,2,2,2,2,2,2,4),(-7.3718042771804,
-7.30571575682601,-7.23381805398239,-7.16467234115743,-7.09284826442791,
-7.02377165232048,-6.95202076013123,-6.88301263647231,-6.81133446730259,
-6.7423941780996,-6.67078824995235,-6.6019150962137,-6.53038090617178,-6.46157414039527,
-6.39011116428207,-6.3213699866964,-6.24997767886145,-6.24525857708354),
 .UNSPECIFIED.) ;
#1494 = B_SPLINE_CURVE_WITH_KNOTS('',3,(#74336,#74337,#74338,#74339,#74340,
#74341,#74342,#74343,#74344,#74345,#74346,#74347,#74348,#74349,#74350,#74351,
#74352,#74353,#74354,#74355,#74356,#74357,#74358,#74359,#74360,#74361,#74362,
#74363,#74364,#74365,#74366,#74367,#74368,#74369,#74370,#74371),
 .UNSPECIFIED.,.F.,.F.,(4,2,2,2,2,2,2,2,2,2,2,2,2,2,2,2,2,4),(-1.7927676458979,
-1.77733046543547,-1.70775302919658,-1.64053117816249,-1.57089772396895,
-1.5036480628367,-1.43395797454286,-1.3666774287613,-1.29693006087219,-1.22961571438907,
-1.1598103956439,-1.09245948905149,-1.02259552639848,-0.955205453945968,
-0.885282136746782,-0.817850442406927,-0.747867046729006,-0.690191867186042),
 .UNSPECIFIED.) ;
#1495 = B_SPLINE_CURVE_WITH_KNOTS('',3,(#74374,#74375,#74376,#74377,#74378,
#74379,#74380,#74381,#74382,#74383,#74384,#74385,#74386,#74387,#74388,#74389,
#74390,#74391,#74392,#74393,#74394,#74395,#74396,#74397),.UNSPECIFIED.,
 .F.,.F.,(4,2,2,2,2,2,2,2,2,2,2,4),(-0.690191867186042,-0.680391433697344,
-0.610347328058405,-0.54282569448384,-0.472720039614924,-0.405150264626143,
-0.334982321666482,-0.267362495862928,-0.197131528611868,-0.129459864241514,
-0.0646142531593531,-9.99996274231307E-7),.UNSPECIFIED.) ;
#1496 = B_SPLINE_CURVE_WITH_KNOTS('',3,(#74401,#74402,#74403,#74404,#74405,
#74406,#74407,#74408,#74409,#74410,#74411,#74412),.UNSPECIFIED.,.F.,.F.,
(4,2,2,2,2,4),(0.,0.0447884204369107,0.0556867274581508,0.0578926554125182,
0.0592288520665145,0.0597188515297013),.UNSPECIFIED.) ;
#1497 = B_SPLINE_CURVE_WITH_KNOTS('',3,(#74413,#74414,#74415,#74416,#74417,
#74418,#74419,#74420,#74421,#74422,#74423,#74424,#74425,#74426,#74427,#74428,
#74429,#74430),.UNSPECIFIED.,.F.,.F.,(4,2,2,2,2,2,2,2,4),(-7.81395263639748,
-7.77230563804403,-7.72971205369717,-7.65759101326273,-7.58823469740948,
-7.5161884943611,-7.44690289514721,-7.37493114396469,-7.3718042771804),
 .UNSPECIFIED.) ;
#1498 = B_SPLINE_CURVE_WITH_KNOTS('',3,(#74433,#74434,#74435,#74436),
 .UNSPECIFIED.,.F.,.F.,(4,4),(5.35005945872097,5.36908038653652),
 .UNSPECIFIED.) ;
#1499 = B_SPLINE_CURVE_WITH_KNOTS('',3,(#74466,#74467,#74468,#74469,#74470,
#74471),.UNSPECIFIED.,.F.,.F.,(4,2,4),(0.,0.0343987133118532,0.0362588513985796),
 .UNSPECIFIED.) ;
#1500 = B_SPLINE_CURVE_WITH_KNOTS('',3,(#74472,#74473,#74474,#74475,#74476,
#74477),.UNSPECIFIED.,.F.,.F.,(4,2,4),(-0.0362588513985796,-0.0343987133118532,
0.),.UNSPECIFIED.) ;
#1501 = B_SPLINE_CURVE_WITH_KNOTS('',3,(#74499,#74500,#74501,#74502),
 .UNSPECIFIED.,.F.,.F.,(4,4),(-0.00945665398132608,0.),.UNSPECIFIED.) ;
#1502 = B_SPLINE_CURVE_WITH_KNOTS('',3,(#74505,#74506,#74507,#74508,#74509,
#74510,#74511,#74512),.UNSPECIFIED.,.F.,.F.,(4,2,2,4),(0.,0.00451226188197751,
0.00913764751162957,0.00945665398132608),.UNSPECIFIED.) ;
#1503 = B_SPLINE_CURVE_WITH_KNOTS('',3,(#74541,#74542,#74543,#74544,#74545),
 .UNSPECIFIED.,.F.,.F.,(4,1,4),(-0.00954394271160891,-0.0040902611621181,
0.),.UNSPECIFIED.) ;
#1504 = B_SPLINE_CURVE_WITH_KNOTS('',3,(#74546,#74547,#74548,#74549,#74550),
 .UNSPECIFIED.,.F.,.F.,(4,1,4),(0.,0.0040902611621181,0.00954394271160891),
 .UNSPECIFIED.) ;
#1505 = B_SPLINE_CURVE_WITH_KNOTS('',3,(#74653,#74654,#74655,#74656,#74657,
#74658,#74659,#74660),.UNSPECIFIED.,.F.,.F.,(4,2,2,4),(-8.07088867651252E-5,
0.00669596786608275,0.0128600360749486,0.0167125787054897),
 .UNSPECIFIED.) ;
#1506 = B_SPLINE_CURVE_WITH_KNOTS('',3,(#74685,#74686,#74687,#74688),
 .UNSPECIFIED.,.F.,.F.,(4,4),(0.107090369358838,0.113521242067949),
 .UNSPECIFIED.) ;
#1507 = B_SPLINE_CURVE_WITH_KNOTS('',3,(#74734,#74735,#74736,#74737,#74738,
#74739,#74740,#74741,#74742,#74743,#74744,#74745,#74746,#74747,#74748,#74749,
#74750,#74751,#74752,#74753),.UNSPECIFIED.,.F.,.F.,(4,2,2,2,2,2,2,2,2,4),
(-0.189691985209992,-0.186922819341822,-0.184515948817362,-0.184153653473652,
-0.18260925271764,-0.181384487605481,-0.18103834187196,-0.180692196138438,
-0.180346050404917,-0.179999904671396),.UNSPECIFIED.) ;
#1508 = B_SPLINE_CURVE_WITH_KNOTS('',3,(#74779,#74780,#74781,#74782,#74783,
#74784),.UNSPECIFIED.,.F.,.F.,(4,2,4),(0.,0.0343987133118529,0.0362588513985796),
 .UNSPECIFIED.) ;
#1509 = B_SPLINE_CURVE_WITH_KNOTS('',3,(#74792,#74793,#74794,#74795,#74796,
#74797),.UNSPECIFIED.,.F.,.F.,(4,2,4),(-0.00186013808672611,0.,0.0343987133118504),
 .UNSPECIFIED.) ;
#1510 = B_SPLINE_CURVE_WITH_KNOTS('',3,(#74804,#74805,#74806,#74807,#74808,
#74809),.UNSPECIFIED.,.F.,.F.,(4,2,4),(-0.00186013808672659,0.,0.0343987133118501),
 .UNSPECIFIED.) ;
#1511 = B_SPLINE_CURVE_WITH_KNOTS('',3,(#74820,#74821,#74822,#74823,#74824),
 .UNSPECIFIED.,.F.,.F.,(4,1,4),(0.,0.00545368154943955,0.00954394271151922),
 .UNSPECIFIED.) ;
#1512 = B_SPLINE_CURVE_WITH_KNOTS('',3,(#74852,#74853,#74854,#74855,#74856,
#74857),.UNSPECIFIED.,.F.,.F.,(4,2,4),(-0.0343987133118501,0.,0.00186013808672659),
 .UNSPECIFIED.) ;
#1513 = B_SPLINE_CURVE_WITH_KNOTS('',3,(#74880,#74881,#74882,#74883),
 .UNSPECIFIED.,.F.,.F.,(4,4),(-0.00945665401173728,-7.96865975725692E-14),
 .UNSPECIFIED.) ;
#1514 = B_SPLINE_CURVE_WITH_KNOTS('',3,(#74884,#74885,#74886,#74887,#74888,
#74889),.UNSPECIFIED.,.F.,.F.,(4,2,4),(7.96865975725692E-14,0.0047494858717794,
0.00945665401173728),.UNSPECIFIED.) ;
#1515 = B_SPLINE_CURVE_WITH_KNOTS('',3,(#74917,#74918,#74919,#74920,#74921),
 .UNSPECIFIED.,.F.,.F.,(4,1,4),(-0.00954394271151922,-0.00545368154943955,
0.),.UNSPECIFIED.) ;
#1516 = B_SPLINE_CURVE_WITH_KNOTS('',3,(#74992,#74993,#74994,#74995,#74996,
#74997,#74998,#74999,#75000,#75001,#75002,#75003,#75004,#75005,#75006,#75007,
#75008,#75009,#75010,#75011,#75012,#75013),.UNSPECIFIED.,.F.,.F.,(4,2,2,
2,2,2,2,2,2,2,4),(0.,0.00178735894887589,0.00328754343915599,0.00522227948307641,
0.00581324616239635,0.0066458744035453,0.00954455547535216,0.00985052209277086,
0.0134309724899257,0.0160797277273677,0.0167952489709647),.UNSPECIFIED.) ;
#1517 = B_SPLINE_CURVE_WITH_KNOTS('',3,(#75041,#75042,#75043,#75044),
 .UNSPECIFIED.,.F.,.F.,(4,4),(0.11352033938527,0.119949480178501),
 .UNSPECIFIED.) ;
#1518 = B_SPLINE_CURVE_WITH_KNOTS('',3,(#75091,#75092,#75093,#75094,#75095,
#75096,#75097,#75098,#75099,#75100,#75101,#75102,#75103,#75104,#75105,#75106,
#75107,#75108,#75109,#75110),.UNSPECIFIED.,.F.,.F.,(4,2,2,2,2,2,2,2,2,4),
(-0.179997619857109,-0.179651531266927,-0.179305442676744,-0.178959354086561,
-0.178613265496379,-0.177069119697205,-0.175844556774918,-0.173438083587768,
-0.170813788147114,-0.170307139331997),.UNSPECIFIED.) ;
#1519 = B_SPLINE_CURVE_WITH_KNOTS('',3,(#75124,#75125,#75126,#75127,#75128),
 .UNSPECIFIED.,.F.,.F.,(4,1,4),(0.,0.013702704196865,0.0319729764593517),
 .UNSPECIFIED.) ;
#1520 = B_SPLINE_CURVE_WITH_KNOTS('',3,(#75155,#75156,#75157,#75158,#75159,
#75160),.UNSPECIFIED.,.F.,.F.,(4,2,4),(-0.0362588513985796,-0.0343987133118529,
0.),.UNSPECIFIED.) ;
#1521 = B_SPLINE_CURVE_WITH_KNOTS('',3,(#75182,#75183,#75184,#75185),
 .UNSPECIFIED.,.F.,.F.,(4,4),(-0.00945665398132565,0.),.UNSPECIFIED.) ;
#1522 = B_SPLINE_CURVE_WITH_KNOTS('',3,(#75188,#75189,#75190,#75191,#75192,
#75193,#75194,#75195),.UNSPECIFIED.,.F.,.F.,(4,2,2,4),(0.,0.00451226188133782,
0.00913764751100092,0.00945665398132565),.UNSPECIFIED.) ;
#1523 = B_SPLINE_CURVE_WITH_KNOTS('',3,(#75224,#75225,#75226,#75227,#75228),
 .UNSPECIFIED.,.F.,.F.,(4,1,4),(-0.00954394271160956,-0.00409026116211842,
-5.7658280050909E-17),.UNSPECIFIED.) ;
#1524 = B_SPLINE_CURVE_WITH_KNOTS('',3,(#75229,#75230,#75231,#75232,#75233),
 .UNSPECIFIED.,.F.,.F.,(4,1,4),(5.7658280050909E-17,0.00409026116211842,
0.00954394271160956),.UNSPECIFIED.) ;
#1525 = B_SPLINE_CURVE_WITH_KNOTS('',3,(#75309,#75310,#75311,#75312,#75313,
#75314,#75315,#75316,#75317,#75318,#75319,#75320,#75321,#75322,#75323,#75324,
#75325,#75326,#75327,#75328,#75329,#75330,#75331,#75332,#75333,#75334,#75335,
#75336,#75337,#75338,#75339,#75340,#75341,#75342,#75343,#75344,#75345,#75346,
#75347,#75348,#75349,#75350,#75351,#75352,#75353,#75354,#75355,#75356,#75357,
#75358,#75359,#75360,#75361,#75362,#75363,#75364,#75365,#75366,#75367,#75368,
#75369),.UNSPECIFIED.,.F.,.F.,(4,3,3,3,3,3,3,3,3,3,3,3,3,3,3,3,3,3,3,3,
4),(-8.09857184636461E-5,0.000317028515094856,0.000374632195319235,0.000383937353632409,
0.000450354935360417,0.000627468486635104,0.00133592269173385,0.00275283110193136,
0.00369743670872969,0.00519672563943589,0.00605516800959267,0.00669601457014209,
0.00784471646450152,0.00899341835886094,0.00962565333192913,0.0112908221475798,
0.0128600542553739,0.0133505813712207,0.0152272244608216,0.0162383352828185,
0.0167125790586438),.UNSPECIFIED.) ;
#1526 = B_SPLINE_CURVE_WITH_KNOTS('',3,(#75394,#75395,#75396,#75397),
 .UNSPECIFIED.,.F.,.F.,(4,4),(0.107092094291284,0.11352518691992),
 .UNSPECIFIED.) ;
#1527 = B_SPLINE_CURVE_WITH_KNOTS('',3,(#75443,#75444,#75445,#75446,#75447,
#75448,#75449,#75450,#75451,#75452,#75453,#75454,#75455,#75456,#75457,#75458,
#75459,#75460),.UNSPECIFIED.,.F.,.F.,(4,2,2,2,2,2,2,2,4),(-0.189691985209994,
-0.186989953236899,-0.185538236407738,-0.183626840293631,-0.182769070539567,
-0.181384487605482,-0.180692196138439,-0.180346050404917,-0.179999904671396),
 .UNSPECIFIED.) ;
#1528 = B_SPLINE_CURVE_WITH_KNOTS('',3,(#75485,#75486,#75487,#75488,#75489),
 .UNSPECIFIED.,.F.,.F.,(4,1,4),(0.,0.00409026116207964,0.00954394271151917),
 .UNSPECIFIED.) ;
#1529 = B_SPLINE_CURVE_WITH_KNOTS('',3,(#75517,#75518,#75519,#75520,#75521,
#75522),.UNSPECIFIED.,.F.,.F.,(4,2,4),(-0.0343987133118504,0.,0.00186013808672611),
 .UNSPECIFIED.) ;
#1530 = B_SPLINE_CURVE_WITH_KNOTS('',3,(#75545,#75546,#75547,#75548),
 .UNSPECIFIED.,.F.,.F.,(4,4),(-0.00945665401173742,-7.97441283497418E-14),
 .UNSPECIFIED.) ;
#1531 = B_SPLINE_CURVE_WITH_KNOTS('',3,(#75549,#75550,#75551,#75552,#75553,
#75554),.UNSPECIFIED.,.F.,.F.,(4,2,4),(7.97441283497418E-14,0.00474948587256806,
0.00945665401173742),.UNSPECIFIED.) ;
#1532 = B_SPLINE_CURVE_WITH_KNOTS('',3,(#75582,#75583,#75584,#75585,#75586),
 .UNSPECIFIED.,.F.,.F.,(4,1,4),(-0.00954394271151917,-0.00409026116207964,
0.),.UNSPECIFIED.) ;
#1533 = B_SPLINE_CURVE_WITH_KNOTS('',3,(#75657,#75658,#75659,#75660,#75661,
#75662,#75663,#75664,#75665,#75666,#75667,#75668,#75669,#75670,#75671,#75672,
#75673,#75674,#75675,#75676,#75677,#75678),.UNSPECIFIED.,.F.,.F.,(4,2,2,
2,2,2,2,2,2,2,4),(0.,0.00178736671760306,0.00328754690174189,0.00522231021806468,
0.00581324616239624,0.00664590032475465,0.0095446545394002,0.00985058182527603,
0.0134311236465911,0.0160798648246182,0.0167952493652102),.UNSPECIFIED.) ;
#1534 = B_SPLINE_CURVE_WITH_KNOTS('',3,(#75706,#75707,#75708,#75709),
 .UNSPECIFIED.,.F.,.F.,(4,4),(0.11353089859696,0.119959972115571),
 .UNSPECIFIED.) ;
#1535 = B_SPLINE_CURVE_WITH_KNOTS('',3,(#75756,#75757,#75758,#75759,#75760,
#75761,#75762,#75763,#75764,#75765,#75766,#75767,#75768,#75769,#75770,#75771,
#75772,#75773,#75774,#75775),.UNSPECIFIED.,.F.,.F.,(4,2,2,2,2,2,2,2,2,4),
(-0.179997619857109,-0.179651531266927,-0.179305442676744,-0.178959354086562,
-0.178613265496379,-0.177069119697188,-0.175844556774918,-0.173438083587785,
-0.170813788147149,-0.170307139331997),.UNSPECIFIED.) ;
#1536 = B_SPLINE_CURVE_WITH_KNOTS('',3,(#75826,#75827,#75828,#75829,#75830,
#75831),.UNSPECIFIED.,.F.,.F.,(4,2,4),(-0.0364117611345324,-0.0361627499148956,
0.),.UNSPECIFIED.) ;
#1537 = B_SPLINE_CURVE_WITH_KNOTS('',3,(#75837,#75838,#75839,#75840),
 .UNSPECIFIED.,.F.,.F.,(4,4),(-0.146371498429592,0.),.UNSPECIFIED.) ;
#1538 = B_SPLINE_CURVE_WITH_KNOTS('',3,(#75877,#75878,#75879,#75880,#75881,
#75882),.UNSPECIFIED.,.F.,.F.,(4,2,4),(0.,0.0361627499148956,0.0364117611345324),
 .UNSPECIFIED.) ;
#1539 = B_SPLINE_CURVE_WITH_KNOTS('',3,(#75929,#75930,#75931,#75932,#75933,
#75934,#75935,#75936),.UNSPECIFIED.,.F.,.F.,(4,2,2,4),(0.,0.0586623890662813,
0.117369996722224,0.146371498429592),.UNSPECIFIED.) ;
#1540 = B_SPLINE_CURVE_WITH_KNOTS('',3,(#75969,#75970,#75971,#75972,#75973,
#75974,#75975,#75976),.UNSPECIFIED.,.F.,.F.,(4,2,2,4),(-0.146371498430696,
-0.0876595232426458,-0.0289914100866822,-8.05248431948221E-13),
 .UNSPECIFIED.) ;
#1541 = B_SPLINE_CURVE_WITH_KNOTS('',3,(#75977,#75978,#75979,#75980),
 .UNSPECIFIED.,.F.,.F.,(4,4),(0.,0.146371498430696),.UNSPECIFIED.) ;
#1542 = B_SPLINE_CURVE_WITH_KNOTS('',3,(#76037,#76038,#76039,#76040,#76041,
#76042),.UNSPECIFIED.,.F.,.F.,(4,2,4),(8.84614312661979E-17,0.0361913306097799,
0.0364133025372201),.UNSPECIFIED.) ;
#1543 = B_SPLINE_CURVE_WITH_KNOTS('',3,(#76043,#76044,#76045,#76046,#76047,
#76048),.UNSPECIFIED.,.F.,.F.,(4,2,4),(-0.0364133025372201,-0.0361913306097799,
-8.84614312661979E-17),.UNSPECIFIED.) ;
#1544 = B_SPLINE_CURVE_WITH_KNOTS('',3,(#76132,#76133,#76134,#76135),
 .UNSPECIFIED.,.F.,.F.,(4,4),(-0.146371498429891,0.),.UNSPECIFIED.) ;
#1545 = B_SPLINE_CURVE_WITH_KNOTS('',3,(#76136,#76137,#76138,#76139,#76140,
#76141,#76142,#76143),.UNSPECIFIED.,.F.,.F.,(4,2,2,4),(0.,0.0586623890660135,
0.117369996721865,0.146371498429891),.UNSPECIFIED.) ;
#1546 = B_SPLINE_CURVE_WITH_KNOTS('',3,(#76200,#76201,#76202,#76203,#76204,
#76205),.UNSPECIFIED.,.F.,.F.,(4,2,4),(0.,0.0361629958429266,0.0364117772057813),
 .UNSPECIFIED.) ;
#1547 = B_SPLINE_CURVE_WITH_KNOTS('',3,(#76206,#76207,#76208,#76209,#76210,
#76211),.UNSPECIFIED.,.F.,.F.,(4,2,4),(-0.0364117772057813,-0.0361629958429266,
0.),.UNSPECIFIED.) ;
#1548 = B_SPLINE_CURVE_WITH_KNOTS('',3,(#76218,#76219,#76220,#76221,#76222,
#76223),.UNSPECIFIED.,.F.,.F.,(4,2,4),(-0.0364133025382447,-0.0361913306296307,
0.),.UNSPECIFIED.) ;
#1549 = B_SPLINE_CURVE_WITH_KNOTS('',3,(#76228,#76229,#76230,#76231,#76232,
#76233,#76234,#76235),.UNSPECIFIED.,.F.,.F.,(4,2,2,4),(-0.146371498429891,
-0.0876595232417657,-0.0289914100858698,0.),.UNSPECIFIED.) ;
#1550 = B_SPLINE_CURVE_WITH_KNOTS('',3,(#76272,#76273,#76274,#76275),
 .UNSPECIFIED.,.F.,.F.,(4,4),(0.,0.146371498429891),.UNSPECIFIED.) ;
#1551 = B_SPLINE_CURVE_WITH_KNOTS('',3,(#76329,#76330,#76331,#76332,#76333,
#76334),.UNSPECIFIED.,.F.,.F.,(4,2,4),(0.,0.0361913306296307,0.0364133025382447),
 .UNSPECIFIED.) ;
#1552 = B_SPLINE_CURVE_WITH_KNOTS('',3,(#76467,#76468,#76469,#76470,#76471,
#76472,#76473,#76474),.UNSPECIFIED.,.F.,.F.,(4,2,2,4),(-0.00449779612828801,
-0.00440391402779913,-0.00244544984037645,-0.000128411811047494),
 .UNSPECIFIED.) ;
#1553 = B_SPLINE_CURVE_WITH_KNOTS('',3,(#76476,#76477,#76478,#76479,#76480,
#76481,#76482,#76483,#76484,#76485),.UNSPECIFIED.,.F.,.F.,(4,2,2,2,4),(-0.326963021080646,
-0.273443015535847,-0.153352882404738,-0.0199317405198332,0.0415869283876659),
 .UNSPECIFIED.) ;
#1554 = B_SPLINE_CURVE_WITH_KNOTS('',3,(#76487,#76488,#76489,#76490,#76491,
#76492,#76493),.UNSPECIFIED.,.F.,.F.,(4,3,4),(-0.00528739892062153,-0.00264209583824454,
-1.05158573648755E-5),.UNSPECIFIED.) ;
#1555 = B_SPLINE_CURVE_WITH_KNOTS('',3,(#76499,#76500,#76501,#76502,#76503,
#76504,#76505,#76506,#76507,#76508,#76509,#76510,#76511,#76512,#76513,#76514,
#76515,#76516),.UNSPECIFIED.,.F.,.F.,(4,2,2,2,2,2,2,2,4),(0.0199485255308491,
0.0405677462825902,0.0613530454994567,0.0817043692001714,0.100854971904388,
0.119363166385794,0.13699176518755,0.153352882404738,0.153410004281816),
 .UNSPECIFIED.) ;
#1556 = B_SPLINE_CURVE_WITH_KNOTS('',3,(#76518,#76519,#76520,#76521,#76522,
#76523,#76524,#76525,#76526,#76527,#76528,#76529,#76530,#76531,#76532,#76533,
#76534,#76535),.UNSPECIFIED.,.F.,.F.,(4,2,2,2,2,2,2,2,4),(0.153410004867272,
0.172771538902472,0.192188682136839,0.210985897145968,0.228496077033556,
0.245368537241394,0.261430894732374,0.273443015535847,0.273454607678092),
 .UNSPECIFIED.) ;
#1557 = B_SPLINE_CURVE_WITH_KNOTS('',3,(#76536,#76537,#76538,#76539,#76540,
#76541,#76542,#76543),.UNSPECIFIED.,.F.,.F.,(4,2,2,4),(0.273454609116393,
0.292643022549525,0.310270283905659,0.327829791007539),.UNSPECIFIED.) ;
#1558 = B_SPLINE_CURVE_WITH_KNOTS('',3,(#76545,#76546,#76547,#76548,#76549,
#76550,#76551,#76552,#76553,#76554,#76555,#76556,#76557,#76558,#76559,#76560,
#76561,#76562),.UNSPECIFIED.,.F.,.F.,(4,2,2,2,2,2,2,2,4),(1.00000407856514E-6,
0.0270461031048522,0.0463717419686661,0.0669688246402426,0.0808296434149286,
0.0869444645666349,0.0890594351739109,0.0898799261523484,0.0905817008981732),
 .UNSPECIFIED.) ;
#1559 = B_SPLINE_CURVE_WITH_KNOTS('',3,(#76565,#76566,#76567,#76568,#76569,
#76570,#76571,#76572,#76573,#76574,#76575,#76576,#76577,#76578,#76579,#76580,
#76581,#76582,#76583,#76584,#76585,#76586,#76587,#76588,#76589,#76590,#76591,
#76592,#76593,#76594,#76595,#76596,#76597,#76598),.UNSPECIFIED.,.F.,.F.,
(4,3,3,3,3,3,3,3,3,3,3,4),(-0.015771486666387,-0.0156499135546454,-0.0132688478173875,
-0.0120178036343787,-0.0117138282636781,-0.00932822941246477,-0.00780237427572918,
-0.00542308690722213,-0.00451600742544575,-0.00389905627547958,-0.00151468045248576,
0.),.UNSPECIFIED.) ;
#1560 = B_SPLINE_CURVE_WITH_KNOTS('',3,(#76669,#76670,#76671,#76672,#76673,
#76674,#76675,#76676,#76677,#76678,#76679,#76680),.UNSPECIFIED.,.F.,.F.,
(4,2,2,2,2,4),(0.000180857407629647,0.00793560140118584,0.0125099257471543,
0.0143669747674358,0.0151422884351474,0.015668827114255),.UNSPECIFIED.) ;
#1561 = B_SPLINE_CURVE_WITH_KNOTS('',3,(#76682,#76683,#76684,#76685),
 .UNSPECIFIED.,.F.,.F.,(4,4),(5.47634473919011E-6,0.094453216066185),
 .UNSPECIFIED.) ;
#1562 = B_SPLINE_CURVE_WITH_KNOTS('',3,(#76687,#76688,#76689,#76690,#76691,
#76692),.UNSPECIFIED.,.F.,.F.,(4,2,4),(0.094453216066185,0.094503731574,
0.215053629751941),.UNSPECIFIED.) ;
#1563 = B_SPLINE_CURVE_WITH_KNOTS('',3,(#76696,#76697,#76698,#76699,#76700,
#76701,#76702,#76703,#76704,#76705),.UNSPECIFIED.,.F.,.F.,(4,2,2,2,4),(-0.408276645255811,
-0.349022909463275,-0.215144182724569,-0.094503731574,-0.0393180761061371),
 .UNSPECIFIED.) ;
#1564 = B_SPLINE_CURVE_WITH_KNOTS('',3,(#77286,#77287,#77288,#77289,#77290,
#77291,#77292,#77293,#77294,#77295,#77296,#77297),.UNSPECIFIED.,.F.,.F.,
(4,2,2,2,2,4),(-0.10355030182359,-0.0894083769331069,-0.0705862367589278,
-0.0476572871556061,-0.0284912878296623,-9.99964373940782E-7),
 .UNSPECIFIED.) ;
#1565 = B_SPLINE_CURVE_WITH_KNOTS('',3,(#77409,#77410,#77411,#77412),
 .UNSPECIFIED.,.F.,.F.,(4,4),(0.00294758963503899,0.0306076446211308),
 .UNSPECIFIED.) ;
#1566 = B_SPLINE_CURVE_WITH_KNOTS('',3,(#77414,#77415,#77416,#77417,#77418,
#77419),.UNSPECIFIED.,.F.,.F.,(4,2,4),(-0.000233218663520837,0.,0.00294758963503899),
 .UNSPECIFIED.) ;
#1567 = B_SPLINE_CURVE_WITH_KNOTS('',3,(#77508,#77509,#77510,#77511),
 .UNSPECIFIED.,.F.,.F.,(4,4),(-0.0306076446211308,-0.00287612766258956),
 .UNSPECIFIED.) ;
#1568 = B_SPLINE_CURVE_WITH_KNOTS('',3,(#77512,#77513,#77514,#77515,#77516,
#77517),.UNSPECIFIED.,.F.,.F.,(4,2,4),(-0.00287612766258956,0.,0.000233218663520837),
 .UNSPECIFIED.) ;
#1569 = B_SPLINE_CURVE_WITH_KNOTS('',3,(#77895,#77896,#77897,#77898),
 .UNSPECIFIED.,.F.,.F.,(4,4),(0.0029475896360751,0.0306076446211596),
 .UNSPECIFIED.) ;
#1570 = B_SPLINE_CURVE_WITH_KNOTS('',3,(#77900,#77901,#77902,#77903,#77904,
#77905),.UNSPECIFIED.,.F.,.F.,(4,2,4),(-0.0002332186634917,0.,0.0029475896360751),
 .UNSPECIFIED.) ;
#1571 = B_SPLINE_CURVE_WITH_KNOTS('',3,(#77994,#77995,#77996,#77997),
 .UNSPECIFIED.,.F.,.F.,(4,4),(-0.0306076446211596,-0.00287612766194185),
 .UNSPECIFIED.) ;
#1572 = B_SPLINE_CURVE_WITH_KNOTS('',3,(#77998,#77999,#78000,#78001,#78002,
#78003),.UNSPECIFIED.,.F.,.F.,(4,2,4),(-0.00287612766194185,0.,0.0002332186634917),
 .UNSPECIFIED.) ;
#1573 = B_SPLINE_CURVE_WITH_KNOTS('',3,(#78199,#78200,#78201,#78202,#78203),
 .UNSPECIFIED.,.F.,.F.,(4,1,4),(1.29610738810862E-16,0.0182702569606054,
0.0319729496810593),.UNSPECIFIED.) ;
#1574 = B_SPLINE_CURVE_WITH_KNOTS('',3,(#78280,#78281,#78282,#78283),
 .UNSPECIFIED.,.F.,.F.,(4,4),(0.,0.0319729496810593),.UNSPECIFIED.) ;
#1575 = B_SPLINE_CURVE_WITH_KNOTS('',3,(#78317,#78318,#78319,#78320),
 .UNSPECIFIED.,.F.,.F.,(4,4),(0.,0.0319729764593517),.UNSPECIFIED.) ;
#1576 = B_SPLINE_CURVE_WITH_KNOTS('',3,(#78358,#78359,#78360,#78361,#78362,
#78363,#78364,#78365,#78366,#78367,#78368,#78369,#78370,#78371,#78372,#78373),
 .UNSPECIFIED.,.F.,.F.,(4,2,2,2,2,2,2,4),(-0.0319729764593517,-0.026487794895197,
-0.0210191260320854,-0.0155681323168053,-0.013702704196865,-0.00853358219385316,
-0.00336875022758298,0.),.UNSPECIFIED.) ;
#1577 = B_SPLINE_CURVE_WITH_KNOTS('',3,(#78412,#78413,#78414,#78415,#78416,
#78417,#78418,#78419,#78420,#78421,#78422,#78423,#78424,#78425,#78426,#78427),
 .UNSPECIFIED.,.F.,.F.,(4,2,2,2,2,2,2,4),(-0.0319729496810593,-0.0268019298577068,
-0.0216243054581297,-0.0182702569606054,-0.0128223821098292,-0.00736410383994217,
-0.00188441434238895,-1.29610738810862E-16),.UNSPECIFIED.) ;
#1578 = B_SPLINE_CURVE_WITH_KNOTS('',3,(#78437,#78438,#78439,#78440,#78441,
#78442,#78443,#78444,#78445,#78446,#78447,#78448,#78449,#78450,#78451,#78452,
#78453,#78454,#78455,#78456),.UNSPECIFIED.,.F.,.F.,(4,2,2,2,2,2,2,2,2,4),
(2.44073605373652,2.65599013224616,2.99553615799378,3.69719379632858,4.0424469091546,
4.7496870461374,5.56463964981499,6.33322372310358,6.72166834008255,7.2429082378436),
 .UNSPECIFIED.) ;
#1579 = B_SPLINE_CURVE_WITH_KNOTS('',3,(#78460,#78461,#78462,#78463,#78464,
#78465,#78466,#78467,#78468,#78469,#78470,#78471,#78472,#78473,#78474,#78475,
#78476,#78477,#78478,#78479,#78480,#78481,#78482,#78483),.UNSPECIFIED.,
 .F.,.F.,(4,2,2,2,2,2,2,2,2,2,2,4),(0.,0.046946185965169,0.0949502462023891,
0.166325664716851,0.266616518174325,0.400158134448206,0.59170384360669,
0.83908927216011,1.1747465058088,1.58388496113465,2.07198027474184,2.44073605373652),
 .UNSPECIFIED.) ;
#1580 = B_SPLINE_CURVE_WITH_KNOTS('',3,(#78793,#78794,#78795,#78796,#78797,
#78798,#78799,#78800,#78801,#78802,#78803,#78804,#78805,#78806,#78807,#78808),
 .UNSPECIFIED.,.F.,.F.,(4,2,2,2,2,2,2,4),(3.73678905355268,3.77583604564174,
3.84429316886454,3.9117839455625,3.98028517515954,4.04771812918815,4.09356285357691,
4.13893020482044),.UNSPECIFIED.) ;
#1581 = B_SPLINE_CURVE_WITH_KNOTS('',3,(#78811,#78812,#78813,#78814,#78815,
#78816,#78817,#78818,#78819,#78820,#78821,#78822,#78823,#78824,#78825,#78826,
#78827,#78828,#78829,#78830),.UNSPECIFIED.,.F.,.F.,(4,2,2,2,2,2,2,2,2,4),
(1.00000010744283E-6,0.0499431784479235,0.100287210935025,0.168054642610065,
0.237494946806667,0.305292985567466,0.374683046548786,0.442516172111994,
0.51185655028286,0.544247303702404),.UNSPECIFIED.) ;
#1582 = B_SPLINE_CURVE_WITH_KNOTS('',3,(#78835,#78836,#78837,#78838,#78839,
#78840,#78841,#78842,#78843,#78844,#78845,#78846,#78847,#78848,#78849,#78850,
#78851,#78852,#78853,#78854,#78855,#78856,#78857,#78858,#78859,#78860,#78861,
#78862,#78863,#78864,#78865,#78866,#78867,#78868,#78869,#78870),
 .UNSPECIFIED.,.F.,.F.,(4,2,2,2,2,2,2,2,2,2,2,2,2,2,2,2,2,4),(2.63879249403916,
2.68716207519284,2.75533111613759,2.82339735412774,2.89159459627009,2.95958001185233,
3.02780800755272,3.09571469311715,3.1639758471015,3.23180612291199,3.30010268233795,
3.36785909776552,3.43619314464488,3.50387847678256,3.57225192300491,3.63986917252862,
3.70828375765117,3.73678905355268),.UNSPECIFIED.) ;
#1583 = B_SPLINE_CURVE_WITH_KNOTS('',3,(#78871,#78872,#78873,#78874,#78875,
#78876,#78877,#78878,#78879,#78880,#78881,#78882,#78883,#78884,#78885,#78886,
#78887,#78888,#78889,#78890,#78891,#78892,#78893,#78894,#78895,#78896,#78897,
#78898,#78899,#78900,#78901,#78902,#78903,#78904,#78905,#78906),
 .UNSPECIFIED.,.F.,.F.,(4,2,2,2,2,2,2,2,2,2,2,2,2,2,2,2,2,4),(0.544247303702404,
0.579729241383105,0.649020714981666,0.71693728891309,0.786180492040209,
0.854145311540051,0.923341134445988,0.991358342360499,1.06050780118652,
1.12858131963186,1.19768557917167,1.26581915872125,1.33487954264344,1.40307674572091,
1.47209474432328,1.54035893111266,1.6093362063892,1.65177826841052),
 .UNSPECIFIED.) ;
#1584 = B_SPLINE_CURVE_WITH_KNOTS('',3,(#78911,#78912,#78913,#78914,#78915,
#78916,#78917,#78918,#78919,#78920,#78921,#78922,#78923,#78924,#78925,#78926,
#78927,#78928,#78929,#78930,#78931,#78932,#78933,#78934,#78935,#78936,#78937,
#78938,#78939,#78940,#78941,#78942,#78943,#78944,#78945,#78946),
 .UNSPECIFIED.,.F.,.F.,(4,2,2,2,2,2,2,2,2,2,2,2,2,2,2,2,2,4),(1.5389994522091,
1.59333149801295,1.66297884651135,1.7301821776633,1.79977280875785,1.86694772145314,
1.93648225696496,2.00363195036966,2.07311098033212,2.14160511265088,2.20968937196864,
2.27809543856464,2.34619647664059,2.41451552535451,2.48263634985671,2.55086961886095,
2.61901314661333,2.63879249403916),.UNSPECIFIED.) ;
#1585 = B_SPLINE_CURVE_WITH_KNOTS('',3,(#78947,#78948,#78949,#78950,#78951,
#78952,#78953,#78954,#78955,#78956,#78957,#78958,#78959,#78960,#78961,#78962,
#78963,#78964,#78965,#78966,#78967,#78968,#78969,#78970,#78971,#78972,#78973,
#78974,#78975,#78976,#78977,#78978,#78979,#78980,#78981,#78982),
 .UNSPECIFIED.,.F.,.F.,(4,2,2,2,2,2,2,2,2,2,2,2,2,2,2,2,2,4),(1.65177826841052,
1.6776705234471,1.7466089112996,1.81501628298846,1.8839177925435,1.95240091532547,
2.02126772540027,2.08982906495714,2.15959253692843,2.22727314697463,2.29708965878139,
2.36477169799653,2.43464163209697,2.50232925343889,2.57225301932284,2.63995025192664,
2.70992829083685,2.76015985424245),.UNSPECIFIED.) ;
#1586 = B_SPLINE_CURVE_WITH_KNOTS('',3,(#78988,#78989,#78990,#78991,#78992,
#78993,#78994,#78995,#78996,#78997,#78998,#78999,#79000,#79001),
 .UNSPECIFIED.,.F.,.F.,(4,2,2,2,2,2,4),(3.87088446641146,3.88207110309913,
3.95256288258768,4.02054495054698,4.09109719843181,4.13081697342442,4.16975042780213),
 .UNSPECIFIED.) ;
#1587 = B_SPLINE_CURVE_WITH_KNOTS('',3,(#79004,#79005,#79006,#79007,#79008,
#79009,#79010,#79011,#79012,#79013,#79014,#79015,#79016,#79017,#79018,#79019,
#79020,#79021),.UNSPECIFIED.,.F.,.F.,(4,2,2,2,2,2,2,2,4),(9.99925951688718E-7,
0.0402770593329322,0.0813965593939245,0.151714020497245,0.219397414529146,
0.289650306659335,0.357279908909674,0.427468950574574,0.435597230048873),
 .UNSPECIFIED.) ;
#1588 = B_SPLINE_CURVE_WITH_KNOTS('',3,(#79027,#79028,#79029,#79030,#79031,
#79032,#79033,#79034,#79035,#79036),.UNSPECIFIED.,.F.,.F.,(4,2,2,2,4),(-0.1667127750087,
-0.142097710392982,-0.0825624075964315,-0.0415013685793908,-1.00000012634438E-6),
 .UNSPECIFIED.) ;
#1589 = B_SPLINE_CURVE_WITH_KNOTS('',3,(#79039,#79040,#79041,#79042,#79043,
#79044,#79045,#79046,#79047,#79048,#79049,#79050,#79051,#79052,#79053,#79054,
#79055,#79056,#79057,#79058,#79059,#79060,#79061,#79062,#79063,#79064),
 .UNSPECIFIED.,.F.,.F.,(4,2,2,2,2,2,2,2,2,2,2,2,4),(-3.52511524228821,-3.4879111620666,
-3.45147286206197,-3.39356408207001,-3.33588355377615,-3.27799407259938,
-3.22024929076642,-3.16237686440599,-3.10456617477217,-3.04670845322558,
-2.98883032321556,-2.9309848603785,-2.88876551162052),.UNSPECIFIED.) ;
#1590 = B_SPLINE_CURVE_WITH_KNOTS('',3,(#79069,#79070,#79071,#79072,#79073,
#79074,#79075,#79076,#79077,#79078,#79079,#79080,#79081,#79082,#79083,#79084,
#79085,#79086,#79087,#79088,#79089,#79090,#79091,#79092,#79093,#79094,#79095,
#79096,#79097,#79098,#79099,#79100,#79101,#79102,#79103,#79104),
 .UNSPECIFIED.,.F.,.F.,(4,2,2,2,2,2,2,2,2,2,2,2,2,2,2,2,2,4),(-1.1147036297923,
-1.08234127378787,-1.0231056786126,-0.964814237103067,-0.905544180711381,
-0.847294503532792,-0.787988947858243,-0.729777999922997,-0.670436005006492,
-0.612260463830717,-0.552881168011551,-0.494737717697047,-0.435320348351732,
-0.377205696945116,-0.317749544705521,-0.259660335123111,-0.200164740500403,
-0.1667127750087),.UNSPECIFIED.) ;
#1591 = B_SPLINE_CURVE_WITH_KNOTS('',3,(#79105,#79106,#79107,#79108,#79109,
#79110,#79111,#79112,#79113,#79114,#79115,#79116,#79117,#79118,#79119,#79120,
#79121,#79122,#79123,#79124,#79125,#79126,#79127,#79128,#79129,#79130,#79131,
#79132,#79133,#79134,#79135,#79136,#79137,#79138,#79139,#79140),
 .UNSPECIFIED.,.F.,.F.,(4,2,2,2,2,2,2,2,2,2,2,2,2,2,2,2,2,4),(-2.88876551162052,
-2.8730378509001,-2.81520202632923,-2.75718479476445,-2.69935609300128,
-2.64126751092778,-2.58344326618254,-2.52528224276112,-2.46745974068091,
-2.40922528204208,-2.35140177232791,-2.2930929756667,-2.23526568453019,
-2.17688173210656,-2.1190478743858,-2.06058802751593,-2.00274481828321,
-1.95515401212426),.UNSPECIFIED.) ;
#1592 = B_SPLINE_CURVE_WITH_KNOTS('',3,(#79145,#79146,#79147,#79148,#79149,
#79150,#79151,#79152,#79153,#79154,#79155,#79156,#79157,#79158,#79159,#79160,
#79161,#79162,#79163,#79164,#79165,#79166,#79167,#79168,#79169,#79170,#79171,
#79172,#79173,#79174,#79175,#79176,#79177,#79178,#79179,#79180),
 .UNSPECIFIED.,.F.,.F.,(4,2,2,2,2,2,2,2,2,2,2,2,2,2,2,2,2,4),(-2.06310075398818,
-2.02342933420803,-1.96363930695818,-1.90563613528142,-1.8458898927228,
-1.78788604802015,-1.72882872991433,-1.6702291728422,-1.61114617975511,
-1.5526042180681,-1.49349375729761,-1.43500706290225,-1.37586747600671,
-1.31743359143829,-1.25826335363796,-1.19987969503678,-1.1406774124604,
-1.1147036297923),.UNSPECIFIED.) ;
#1593 = B_SPLINE_CURVE_WITH_KNOTS('',3,(#79181,#79182,#79183,#79184,#79185,
#79186,#79187,#79188,#79189,#79190,#79191,#79192,#79193,#79194,#79195,#79196,
#79197,#79198,#79199,#79200,#79201,#79202,#79203,#79204,#79205,#79206,#79207,
#79208,#79209,#79210,#79211,#79212,#79213,#79214,#79215,#79216),
 .UNSPECIFIED.,.F.,.F.,(4,2,2,2,2,2,2,2,2,2,2,2,2,2,2,2,2,4),(-1.95515401212426,
-1.94420841138501,-1.88635307691628,-1.82773951167999,-1.76986929968893,
-1.71260942538492,-1.65318316629389,-1.59587567208381,-1.53639019675408,
-1.47903330179993,-1.41948762790906,-1.36207963998264,-1.3024728018388,
-1.24501211437446,-1.18534316543117,-1.12782825442788,-1.06809626943629,
-1.01710396538768),.UNSPECIFIED.) ;
#1594 = B_SPLINE_CURVE_WITH_KNOTS('',3,(#79222,#79223,#79224,#79225,#79226,
#79227,#79228,#79229),.UNSPECIFIED.,.F.,.F.,(4,2,2,4),(-0.0724080849059257,
-0.0675792623524678,-0.0340552227594196,-9.99999997836065E-7),
 .UNSPECIFIED.) ;
#1595 = B_SPLINE_CURVE_WITH_KNOTS('',3,(#79232,#79233,#79234,#79235,#79236,
#79237,#79238,#79239,#79240,#79241,#79242,#79243,#79244,#79245,#79246,#79247,
#79248,#79249,#79250,#79251,#79252,#79253,#79254,#79255),.UNSPECIFIED.,
 .F.,.F.,(4,2,2,2,2,2,2,2,2,2,2,4),(-3.56932824666088,-3.53449866700443,
-3.50005253731909,-3.44177237096352,-3.38139391611913,-3.32315169324715,
-3.26282744772412,-3.2046207539918,-3.14434969751453,-3.08617601623974,
-3.02595714369959,-3.01323089524153),.UNSPECIFIED.) ;
#1596 = B_SPLINE_CURVE_WITH_KNOTS('',3,(#79257,#79258,#79259,#79260,#79261,
#79262,#79263,#79264,#79265,#79266,#79267,#79268,#79269,#79270,#79271,#79272,
#79273,#79274,#79275,#79276,#79277,#79278,#79279,#79280,#79281,#79282,#79283,
#79284,#79285,#79286,#79287,#79288,#79289,#79290,#79291,#79292),
 .UNSPECIFIED.,.F.,.F.,(4,2,2,2,2,2,2,2,2,2,2,2,2,2,2,2,2,4),(-3.01323089524153,
-2.96781377424098,-2.90764599157684,-2.84953027391211,-2.78941272895961,
-2.73132186836034,-2.67125362853938,-2.61318471166392,-2.55316487653164,
-2.49511489832779,-2.43514260265038,-2.37710847123879,-2.31718288727562,
-2.2591614298491,-2.19928176867963,-2.14126973842676,-2.08143525016407,
-2.06310075398818),.UNSPECIFIED.) ;
#1597 = B_SPLINE_CURVE_WITH_KNOTS('',3,(#79293,#79294,#79295,#79296,#79297,
#79298,#79299,#79300,#79301,#79302,#79303,#79304,#79305,#79306,#79307,#79308,
#79309,#79310,#79311,#79312,#79313,#79314,#79315,#79316,#79317,#79318,#79319,
#79320,#79321,#79322,#79323,#79324,#79325,#79326,#79327,#79328),
 .UNSPECIFIED.,.F.,.F.,(4,2,2,2,2,2,2,2,2,2,2,2,2,2,2,2,2,4),(-1.01710396538768,
-1.01052569025312,-0.95072976706705,-0.893102151152008,-0.833241412200572,
-0.77555546378878,-0.715629057236816,-0.657883550045956,-0.597890650662598,
-0.540084424611622,-0.480024234372677,-0.422156192345284,-0.362027940792846,
-0.304097045462937,-0.243899989848112,-0.185905260581977,-0.125638685815469,
-0.0724080849059257),.UNSPECIFIED.) ;
#1598 = B_SPLINE_CURVE_WITH_KNOTS('',3,(#79330,#79331,#79332,#79333,#79334,
#79335,#79336,#79337,#79338,#79339,#79340,#79341,#79342,#79343,#79344,#79345,
#79346,#79347,#79348,#79349,#79350,#79351,#79352,#79353,#79354,#79355,#79356,
#79357,#79358,#79359,#79360,#79361,#79362,#79363,#79364,#79365),
 .UNSPECIFIED.,.F.,.F.,(4,2,2,2,2,2,2,2,2,2,2,2,2,2,2,2,2,4),(0.435597230048873,
0.495046546283641,0.565172626519024,0.632699860466232,0.702763552831684,
0.770242289348338,0.840244331880487,0.907676580521343,0.977617711024885,
1.04500561401596,1.11488656619888,1.18223240425633,1.25205390364054,1.31936010136934,
1.38912286105409,1.4563919917789,1.52609670814966,1.5389994522091),
 .UNSPECIFIED.) ;
#1599 = B_SPLINE_CURVE_WITH_KNOTS('',3,(#79366,#79367,#79368,#79369,#79370,
#79371,#79372,#79373,#79374,#79375,#79376,#79377,#79378,#79379,#79380,#79381,
#79382,#79383,#79384,#79385,#79386,#79387,#79388,#79389,#79390,#79391,#79392,
#79393,#79394,#79395,#79396,#79397,#79398,#79399,#79400,#79401),
 .UNSPECIFIED.,.F.,.F.,(4,2,2,2,2,2,2,2,2,2,2,2,2,2,2,2,2,4),(2.76015985424245,
2.77763902868009,2.84767181663405,2.91539980943377,2.98548785867969,3.05323670495124,
3.12338056402631,3.1911537061991,3.26135395879188,3.32915468023334,3.39941194304139,
3.46724336682288,3.53755828661268,3.60542337583455,3.67579662590241,3.74369818538195,
3.81413046159021,3.87088446641146),.UNSPECIFIED.) ;
#1600 = B_SPLINE_CURVE_WITH_KNOTS('',3,(#79532,#79533,#79534,#79535),
 .UNSPECIFIED.,.F.,.F.,(4,4),(0.,0.00842756229585243),.UNSPECIFIED.) ;
#1601 = B_SPLINE_CURVE_WITH_KNOTS('',3,(#79538,#79539,#79540,#79541),
 .UNSPECIFIED.,.F.,.F.,(4,4),(0.0790172234209096,0.0874447857167618),
 .UNSPECIFIED.) ;
#1602 = B_SPLINE_CURVE_WITH_KNOTS('',3,(#79588,#79589,#79590,#79591),
 .UNSPECIFIED.,.F.,.F.,(4,4),(0.,0.00842756229585143),.UNSPECIFIED.) ;
#1603 = B_SPLINE_CURVE_WITH_KNOTS('',3,(#79595,#79596,#79597,#79598),
 .UNSPECIFIED.,.F.,.F.,(4,4),(0.0790172234209045,0.0874447857167594),
 .UNSPECIFIED.) ;
#1604 = B_SPLINE_CURVE_WITH_KNOTS('',3,(#79639,#79640,#79641,#79642,#79643,
#79644,#79645,#79646,#79647,#79648,#79649,#79650),.UNSPECIFIED.,.F.,.F.,
(4,2,2,2,2,4),(1.00000007519743E-6,0.0421735173272767,0.08211256883264,
0.109687200675272,0.164822029616579,0.245179037282195),.UNSPECIFIED.) ;
#1605 = B_SPLINE_CURVE_WITH_KNOTS('',3,(#79651,#79652,#79653,#79654,#79655,
#79656,#79657,#79658,#79659,#79660),.UNSPECIFIED.,.F.,.F.,(4,2,2,2,4),(1.0000001480151E-6,
0.0490152958922886,0.0835871661537387,0.106392725679102,0.131008894822419),
 .UNSPECIFIED.) ;
#1606 = B_SPLINE_CURVE_WITH_KNOTS('',3,(#79669,#79670,#79671,#79672,#79673,
#79674,#79675,#79676,#79677,#79678,#79679,#79680),.UNSPECIFIED.,.F.,.F.,
(4,2,2,2,2,4),(-0.00017826200870649,0.,0.0030884165059787,0.00619403925206626,
0.0112943329275738,0.0143635991137086),.UNSPECIFIED.) ;
#1607 = B_SPLINE_CURVE_WITH_KNOTS('',3,(#79682,#79683,#79684,#79685,#79686,
#79687,#79688,#79689,#79690,#79691,#79692,#79693),.UNSPECIFIED.,.F.,.F.,
(4,2,2,2,2,4),(0.0308002519686446,0.0338695181549982,0.0389698118306942,
0.0420754345767631,0.0451638510827407,0.045342113091339),.UNSPECIFIED.) ;
#1608 = B_SPLINE_CURVE_WITH_KNOTS('',3,(#79697,#79698,#79699,#79700,#79701,
#79702,#79703,#79704,#79705,#79706,#79707,#79708),.UNSPECIFIED.,.F.,.F.,
(4,2,2,2,2,4),(0.0308002519713024,0.0338695181576853,0.0389698118335861,
0.0420754345799843,0.0451638510866813,0.0453421130955797),.UNSPECIFIED.) ;
#1609 = B_SPLINE_CURVE_WITH_KNOTS('',3,(#79711,#79712,#79713,#79714,#79715,
#79716,#79717,#79718,#79719,#79720,#79721,#79722),.UNSPECIFIED.,.F.,.F.,
(4,2,2,2,2,4),(-0.000178262008688658,2.5170620795989E-14,0.00308841650593589,
0.00619403925194464,0.0112943329278571,0.0143635991142711),
 .UNSPECIFIED.) ;
#1610 = B_SPLINE_CURVE_WITH_KNOTS('',3,(#79903,#79904,#79905,#79906,#79907,
#79908,#79909,#79910,#79911,#79912),.UNSPECIFIED.,.F.,.F.,(4,2,2,2,4),(1.00000014819981E-6,
0.0516668726729712,0.117271294398376,0.174520707500308,0.234084768444643),
 .UNSPECIFIED.) ;
#1611 = B_SPLINE_CURVE_WITH_KNOTS('',3,(#79913,#79914,#79915,#79916,#79917,
#79918,#79919,#79920,#79921,#79922),.UNSPECIFIED.,.F.,.F.,(4,2,2,2,4),(9.99997439055519E-7,
0.0477521616236099,0.0878727120265759,0.124072211679175,0.147007126409162),
 .UNSPECIFIED.) ;
#1612 = B_SPLINE_CURVE_WITH_KNOTS('',3,(#80833,#80834,#80835,#80836,#80837,
#80838),.UNSPECIFIED.,.F.,.F.,(4,2,4),(-0.0629976158763524,-0.0314993212424117,
-1.00009004573627E-6),.UNSPECIFIED.) ;
#1613 = B_SPLINE_CURVE_WITH_KNOTS('',3,(#80842,#80843,#80844,#80845),
 .UNSPECIFIED.,.F.,.F.,(4,4),(0.65,1.3),.UNSPECIFIED.) ;
#1614 = B_SPLINE_CURVE_WITH_KNOTS('',3,(#80876,#80877,#80878,#80879,#80880,
#80881),.UNSPECIFIED.,.F.,.F.,(4,2,4),(-0.0629976151793818,-0.0314998208710405,
-9.99993644668074E-7),.UNSPECIFIED.) ;
#1615 = B_SPLINE_CURVE_WITH_KNOTS('',3,(#80885,#80886,#80887,#80888,#80889,
#80890),.UNSPECIFIED.,.F.,.F.,(4,2,4),(-0.0749709647986248,-0.0374848715520891,
0.),.UNSPECIFIED.) ;
#1616 = B_SPLINE_CURVE_WITH_KNOTS('',3,(#80922,#80923,#80924,#80925,#80926,
#80927),.UNSPECIFIED.,.F.,.F.,(4,2,4),(-0.0749708491846415,-0.0374854095897592,
0.),.UNSPECIFIED.) ;
#1617 = B_SPLINE_CURVE_WITH_KNOTS('',3,(#80958,#80959,#80960,#80961,#80962,
#80963),.UNSPECIFIED.,.F.,.F.,(4,2,4),(-0.0629976151789191,-0.0314993208821172,
-9.999936648616E-7),.UNSPECIFIED.) ;
#1618 = B_SPLINE_CURVE_WITH_KNOTS('',3,(#80967,#80968,#80969,#80970,#80971,
#80972),.UNSPECIFIED.,.F.,.F.,(4,2,4),(-0.074970850289862,-0.0374860052740206,
0.),.UNSPECIFIED.) ;
#1619 = B_SPLINE_CURVE_WITH_KNOTS('',3,(#81003,#81004,#81005,#81006,#81007,
#81008),.UNSPECIFIED.,.F.,.F.,(4,2,4),(-0.0629976791811074,-0.0314988521171933,
-9.99993650290977E-7),.UNSPECIFIED.) ;
#1620 = B_SPLINE_CURVE_WITH_KNOTS('',3,(#81012,#81013,#81014,#81015,#81016,
#81017),.UNSPECIFIED.,.F.,.F.,(4,2,4),(-0.0749709647978269,-0.0374854665776717,
0.),.UNSPECIFIED.) ;
#1621 = B_SPLINE_CURVE_WITH_KNOTS('',3,(#81459,#81460,#81461,#81462,#81463,
#81464),.UNSPECIFIED.,.F.,.F.,(4,2,4),(9.99986190228668E-7,0.0314993519488164,
0.0629976787086803),.UNSPECIFIED.) ;
#1622 = B_SPLINE_CURVE_WITH_KNOTS('',3,(#81465,#81466,#81467,#81468,#81469,
#81470),.UNSPECIFIED.,.F.,.F.,(4,2,4),(0.,0.0374854669831317,0.0749709656293669),
 .UNSPECIFIED.) ;
#1623 = B_SPLINE_CURVE_WITH_KNOTS('',3,(#81505,#81506,#81507,#81508,#81509,
#81510),.UNSPECIFIED.,.F.,.F.,(4,2,4),(9.99986130257806E-7,0.0314993519482237,
0.0629976787077657),.UNSPECIFIED.) ;
#1624 = B_SPLINE_CURVE_WITH_KNOTS('',3,(#81511,#81512,#81513,#81514,#81515,
#81516),.UNSPECIFIED.,.F.,.F.,(4,2,4),(0.,0.0374854669835134,0.0749709656299367),
 .UNSPECIFIED.) ;
#1625 = B_SPLINE_CURVE_WITH_KNOTS('',3,(#81551,#81552,#81553,#81554,#81555,
#81556),.UNSPECIFIED.,.F.,.F.,(4,2,4),(9.99897261200662E-7,0.0314993517939326,
0.0629976784770454),.UNSPECIFIED.) ;
#1626 = B_SPLINE_CURVE_WITH_KNOTS('',3,(#81557,#81558,#81559,#81560),
 .UNSPECIFIED.,.F.,.F.,(4,4),(0.65,1.3),.UNSPECIFIED.) ;
#1627 = B_SPLINE_CURVE_WITH_KNOTS('',3,(#81590,#81591,#81592,#81593,#81594,
#81595),.UNSPECIFIED.,.F.,.F.,(4,2,4),(0.,0.0374854671857389,0.0749709659305387),
 .UNSPECIFIED.) ;
#1628 = B_SPLINE_CURVE_WITH_KNOTS('',3,(#81630,#81631,#81632,#81633,#81634,
#81635),.UNSPECIFIED.,.F.,.F.,(4,2,4),(9.99986221142887E-7,0.0314993519490406,
0.0629976787097528),.UNSPECIFIED.) ;
#1629 = B_SPLINE_CURVE_WITH_KNOTS('',3,(#81636,#81637,#81638,#81639,#81640,
#81641),.UNSPECIFIED.,.F.,.F.,(4,2,4),(0.,0.0374854669835796,0.0749709656310599),
 .UNSPECIFIED.) ;
#1630 = B_SPLINE_CURVE_WITH_KNOTS('',3,(#81802,#81803,#81804,#81805,#81806,
#81807,#81808,#81809,#81810,#81811,#81812,#81813,#81814,#81815,#81816,#81817,
#81818,#81819,#81820,#81821,#81822,#81823,#81824,#81825),.UNSPECIFIED.,
 .F.,.F.,(4,2,2,2,2,2,2,2,2,2,2,4),(13.8867005186057,13.9350474908693,13.9924855972126,
14.0524156344104,14.1100718512641,14.16910817166,14.2282720252749,14.2852973565917,
14.3449598229184,14.4034785115834,14.4576795870239,14.5137172238172),
 .UNSPECIFIED.) ;
#1631 = B_SPLINE_CURVE_WITH_KNOTS('',3,(#81828,#81829,#81830,#81831,#81832,
#81833,#81834,#81835,#81836,#81837,#81838,#81839,#81840,#81841,#81842,#81843,
#81844,#81845,#81846,#81847,#81848,#81849),.UNSPECIFIED.,.F.,.F.,(4,2,2,
2,2,2,2,2,2,2,4),(9.99999999983386E-7,0.0304626053349231,0.0610090759544533,
0.120167775309188,0.177705880467965,0.237495432414644,0.295507829943808,
0.353719522676528,0.41351508898739,0.47065222200038,0.508205581620669),
 .UNSPECIFIED.) ;
#1632 = B_SPLINE_CURVE_WITH_KNOTS('',3,(#81854,#81855,#81856,#81857,#81858,
#81859,#81860,#81861,#81862,#81863,#81864,#81865,#81866,#81867,#81868,#81869,
#81870,#81871,#81872,#81873,#81874,#81875,#81876,#81877,#81878,#81879,#81880,
#81881,#81882,#81883,#81884,#81885,#81886,#81887,#81888,#81889),
 .UNSPECIFIED.,.F.,.F.,(4,2,2,2,2,2,2,2,2,2,2,2,2,2,2,2,2,4),(12.9412330053418,
12.998236214922,13.0563572589213,13.1159524118842,13.1733090635897,13.2329612974308,
13.2917792811559,13.3487577815587,13.4084196690731,13.4665880264056,13.5243074655242,
13.584060767217,13.6415584764723,13.7011457577954,13.7601194030082,13.8170733726563,
13.8767213491233,13.8867005186057),.UNSPECIFIED.) ;
#1633 = B_SPLINE_CURVE_WITH_KNOTS('',3,(#81890,#81891,#81892,#81893,#81894,
#81895,#81896,#81897,#81898,#81899,#81900,#81901,#81902,#81903,#81904,#81905,
#81906,#81907,#81908,#81909,#81910,#81911,#81912,#81913,#81914,#81915,#81916,
#81917,#81918,#81919,#81920,#81921,#81922,#81923,#81924,#81925),
 .UNSPECIFIED.,.F.,.F.,(4,2,2,2,2,2,2,2,2,2,2,2,2,2,2,2,2,4),(0.508205581620669,
0.529516158689829,0.589294709689451,0.64670174785647,0.706343830502454,
0.764822728260175,0.822910164017873,0.883310219729821,0.940608465203719,
0.999371393345501,1.0591764292834,1.11640397895033,1.17581182275485,1.23468547612338,
1.29256543862931,1.35273576560654,1.41016590071693,1.45610265637391),
 .UNSPECIFIED.) ;
#1634 = B_SPLINE_CURVE_WITH_KNOTS('',3,(#81930,#81931,#81932,#81933,#81934,
#81935,#81936,#81937,#81938,#81939,#81940,#81941,#81942,#81943,#81944,#81945,
#81946,#81947,#81948,#81949,#81950,#81951,#81952,#81953,#81954,#81955,#81956,
#81957,#81958,#81959,#81960,#81961,#81962,#81963,#81964,#81965,#81966,#81967),
 .UNSPECIFIED.,.F.,.F.,(4,2,2,2,2,2,2,2,2,2,2,2,2,2,2,2,2,2,4),(11.9961952508726,
12.0042837462161,12.0618845196288,12.1208623533056,12.1799693778926,12.2369397423948,
12.2965444576751,12.3550069487343,12.4121989388398,12.4722827355704,12.5300739275151,
12.5885939955338,12.6479201143845,12.7050601300443,12.7647104833383,12.8233948532171,
12.880498390127,12.9402044488287,12.9412330053418),.UNSPECIFIED.) ;
#1635 = B_SPLINE_CURVE_WITH_KNOTS('',3,(#81968,#81969,#81970,#81971,#81972,
#81973,#81974,#81975,#81976,#81977,#81978,#81979,#81980,#81981,#81982,#81983,
#81984,#81985,#81986,#81987,#81988,#81989,#81990,#81991,#81992,#81993,#81994,
#81995,#81996,#81997,#81998,#81999,#82000,#82001,#82002,#82003),
 .UNSPECIFIED.,.F.,.F.,(4,2,2,2,2,2,2,2,2,2,2,2,2,2,2,2,2,4),(1.45610265637391,
1.46871800860693,1.52849061803271,1.58558862544678,1.64478817475386,1.70416297781245,
1.76186476207488,1.82183697097415,1.879497358742,1.93787034129416,1.99764047850571,
2.0547078195011,2.11373042452122,2.17368686543178,2.23124440123845,2.29105539109935,
2.34902981745396,2.40334819810103),.UNSPECIFIED.) ;
#1636 = B_SPLINE_CURVE_WITH_KNOTS('',3,(#82008,#82009,#82010,#82011,#82012,
#82013,#82014,#82015,#82016,#82017,#82018,#82019,#82020,#82021,#82022,#82023,
#82024,#82025,#82026,#82027,#82028,#82029,#82030,#82031,#82032,#82033,#82034,
#82035,#82036,#82037,#82038,#82039,#82040,#82041,#82042,#82043),
 .UNSPECIFIED.,.F.,.F.,(4,2,2,2,2,2,2,2,2,2,2,2,2,2,2,2,2,4),(11.0517238864306,
11.0681655496399,11.1254856558836,11.1856249155873,11.2443861394716,11.3013091538836,
11.3609130535846,11.4190252875331,11.4766878949276,11.5363835817554,11.593825824283,
11.6533537955196,11.7122706230244,11.769169357543,11.8287594281516,11.8870294631155,
11.9444113071521,11.9961952508726),.UNSPECIFIED.) ;
#1637 = B_SPLINE_CURVE_WITH_KNOTS('',3,(#82044,#82045,#82046,#82047,#82048,
#82049,#82050,#82051,#82052,#82053,#82054,#82055,#82056,#82057,#82058,#82059,
#82060,#82061,#82062,#82063,#82064,#82065,#82066,#82067,#82068,#82069,#82070,
#82071,#82072,#82073,#82074,#82075,#82076,#82077,#82078,#82079,#82080,#82081),
 .UNSPECIFIED.,.F.,.F.,(4,2,2,2,2,2,2,2,2,2,2,2,2,2,2,2,2,2,4),(2.40334819810103,
2.4072605468042,2.46705591833339,2.52418455061912,2.58306722119116,2.64284703329508,
2.7002709712672,2.75993178087289,2.81835849049791,2.87646189303058,2.93688032948389,
2.99415810892388,3.05293740878363,3.11273682802953,3.16997581814349,3.22939954900085,
3.28820658472353,3.34609923977367,3.35114202110295),.UNSPECIFIED.) ;
#1638 = B_SPLINE_CURVE_WITH_KNOTS('',3,(#82086,#82087,#82088,#82089,#82090,
#82091,#82092,#82093,#82094,#82095,#82096,#82097,#82098,#82099,#82100,#82101,
#82102,#82103,#82104,#82105,#82106,#82107,#82108,#82109,#82110,#82111,#82112,
#82113,#82114,#82115,#82116,#82117,#82118,#82119,#82120,#82121),
 .UNSPECIFIED.,.F.,.F.,(4,2,2,2,2,2,2,2,2,2,2,2,2,2,2,2,2,4),(10.1061328943984,
10.1319344713036,10.1889836828643,10.248657015031,10.3072111047501,10.3644467073206,
10.4246264128683,10.4825080245906,10.5410374571557,10.6004592838386,10.6576583140244,
10.7172803345211,10.7759257359241,10.8329561804325,10.8926005512979,10.9505943726261,
11.0086070054143,11.0517238864306),.UNSPECIFIED.) ;
#1639 = B_SPLINE_CURVE_WITH_KNOTS('',3,(#82122,#82123,#82124,#82125,#82126,
#82127,#82128,#82129,#82130,#82131,#82132,#82133,#82134,#82135,#82136,#82137,
#82138,#82139,#82140,#82141,#82142,#82143,#82144,#82145,#82146,#82147,#82148,
#82149,#82150,#82151,#82152,#82153,#82154,#82155,#82156,#82157),
 .UNSPECIFIED.,.F.,.F.,(4,2,2,2,2,2,2,2,2,2,2,2,2,2,2,2,2,4),(3.35114202110295,
3.40628444731813,3.46368137332275,3.52224634036856,3.58200944812486,3.63910679195477,
3.6983187890776,3.75761489908632,3.81532554132471,3.87530847359802,3.93292407555114,
3.99130574702326,4.05106281670436,4.10811742404662,4.16714832201972,4.22701774069037,
4.28457972163558,4.2982223769055),.UNSPECIFIED.) ;
#1640 = B_SPLINE_CURVE_WITH_KNOTS('',3,(#82162,#82163,#82164,#82165,#82166,
#82167,#82168,#82169,#82170,#82171,#82172,#82173,#82174,#82175,#82176,#82177,
#82178,#82179,#82180,#82181,#82182,#82183,#82184,#82185,#82186,#82187,#82188,
#82189,#82190,#82191,#82192,#82193,#82194,#82195,#82196,#82197),
 .UNSPECIFIED.,.F.,.F.,(4,2,2,2,2,2,2,2,2,2,2,2,2,2,2,2,2,4),(9.16068336219022,
9.19538360180203,9.25235946726598,9.31202418801378,9.37021833087523,9.4279003321042,
9.48768220706314,9.54520591189467,9.60471899739655,9.66372331785842,9.72068736339293,
9.78034198576824,9.83869910931437,9.89611140398129,9.95607523366671,10.013762247429,
10.0727354918934,10.1061328943984),.UNSPECIFIED.) ;
#1641 = B_SPLINE_CURVE_WITH_KNOTS('',3,(#82198,#82199,#82200,#82201,#82202,
#82203,#82204,#82205,#82206,#82207,#82208,#82209,#82210,#82211,#82212,#82213,
#82214,#82215,#82216,#82217,#82218,#82219,#82220,#82221,#82222,#82223,#82224,
#82225,#82226,#82227,#82228,#82229,#82230,#82231,#82232,#82233),
 .UNSPECIFIED.,.F.,.F.,(4,2,2,2,2,2,2,2,2,2,2,2,2,2,2,2,2,4),(4.2982223769055,
4.34439663186739,4.40231707582145,4.46055170597777,4.52033067706177,4.57743592485621,
4.63632205749593,4.69608715005503,4.75351317167067,4.81317737256235,4.87153538562735,
4.92963978294915,4.99006111696204,5.04730335700837,5.10608391044735,5.16586145253212,
5.22309807562595,5.2457892592979),.UNSPECIFIED.) ;
#1642 = B_SPLINE_CURVE_WITH_KNOTS('',3,(#82238,#82239,#82240,#82241,#82242,
#82243,#82244,#82245,#82246,#82247,#82248,#82249,#82250,#82251,#82252,#82253,
#82254,#82255,#82256,#82257,#82258,#82259,#82260,#82261,#82262,#82263,#82264,
#82265,#82266,#82267,#82268,#82269,#82270,#82271,#82272,#82273),
 .UNSPECIFIED.,.F.,.F.,(4,2,2,2,2,2,2,2,2,2,2,2,2,2,2,2,2,4),(8.21436505857019,
8.25733956019176,8.31460502469798,8.37486191077879,8.43281602299387,8.4913430031965,
8.55084190230918,8.60811398753954,8.66779474291512,8.72651665970665,8.78358981574751,
8.84329151668778,8.90136153830009,8.9593861037039,9.01902504997052,9.07642130387137,
9.13654008132794,9.16068336219022),.UNSPECIFIED.) ;
#1643 = B_SPLINE_CURVE_WITH_KNOTS('',3,(#82274,#82275,#82276,#82277,#82278,
#82279,#82280,#82281,#82282,#82283,#82284,#82285,#82286,#82287,#82288,#82289,
#82290,#82291,#82292,#82293,#82294,#82295,#82296,#82297,#82298,#82299,#82300,
#82301,#82302,#82303,#82304,#82305,#82306,#82307,#82308,#82309),
 .UNSPECIFIED.,.F.,.F.,(4,2,2,2,2,2,2,2,2,2,2,2,2,2,2,2,2,4),(5.2457892592979,
5.28252236343818,5.34124533948901,5.39913569519271,5.45932029051008,5.51666828733251,
5.57523098093596,5.63496811679614,5.69205059527559,5.75125970307787,5.8104586001455,
5.86816306502341,5.92814118700423,5.98569549667876,6.04407067666668,6.10379801346566,
6.16082506805814,6.19252875602354),.UNSPECIFIED.) ;
#1644 = B_SPLINE_CURVE_WITH_KNOTS('',3,(#82314,#82315,#82316,#82317,#82318,
#82319,#82320,#82321,#82322,#82323,#82324,#82325,#82326,#82327,#82328,#82329,
#82330,#82331,#82332,#82333,#82334,#82335,#82336,#82337,#82338,#82339,#82340,
#82341,#82342,#82343,#82344,#82345,#82346,#82347,#82348,#82349),
 .UNSPECIFIED.,.F.,.F.,(4,2,2,2,2,2,2,2,2,2,2,2,2,2,2,2,2,4),(7.26810373508885,
7.31959226080252,7.37728070535416,7.43713087514446,7.49471888210049,7.55420561942568,
7.61327955037669,7.67029385961975,7.72999626093379,7.78842276307307,7.84585231980428,
7.90588921391058,7.96364491307247,8.02260214152301,8.08187479149579,8.13898700097499,
8.19871197935205,8.21436505857019),.UNSPECIFIED.) ;
#1645 = B_SPLINE_CURVE_WITH_KNOTS('',3,(#82350,#82351,#82352,#82353,#82354,
#82355,#82356,#82357,#82358,#82359,#82360,#82361,#82362,#82363,#82364,#82365,
#82366,#82367,#82368,#82369,#82370,#82371,#82372,#82373,#82374,#82375,#82376,
#82377,#82378,#82379,#82380,#82381,#82382,#82383,#82384,#82385),
 .UNSPECIFIED.,.F.,.F.,(4,2,2,2,2,2,2,2,2,2,2,2,2,2,2,2,2,4),(6.19252875602354,
6.21984888247365,6.2796116781406,6.33716298617571,6.39697019465541,6.45481923300649,
6.51304248460271,6.57278820928456,6.62985451075959,6.68872863482653,6.74846230883204,
6.80587530622558,6.86552729196779,6.92379822165874,6.98188832681,7.04229679654806,
7.09948736675755,7.13949123074078),.UNSPECIFIED.) ;
#1646 = B_SPLINE_CURVE_WITH_KNOTS('',3,(#82390,#82391,#82392,#82393,#82394,
#82395,#82396,#82397,#82398,#82399,#82400,#82401,#82402,#82403,#82404,#82405,
#82406,#82407,#82408,#82409,#82410,#82411,#82412,#82413,#82414,#82415,#82416,
#82417,#82418,#82419,#82420,#82421,#82422,#82423,#82424,#82425,#82426,#82427),
 .UNSPECIFIED.,.F.,.F.,(4,2,2,2,2,2,2,2,2,2,2,2,2,2,2,2,2,2,4),(6.32170606963374,
6.32400468955437,6.38370211924148,6.44076735369172,6.4994918136059,6.55916879534269,
6.61644284739015,6.67594418833338,6.73444756181926,6.79240320162889,6.85266228462122,
6.90991547332821,6.9685446550446,7.02826345535349,7.08537458801367,7.14464864112866,
7.20357745851197,7.26133349550517,7.26810373508885),.UNSPECIFIED.) ;
#1647 = B_SPLINE_CURVE_WITH_KNOTS('',3,(#82428,#82429,#82430,#82431,#82432,
#82433,#82434,#82435,#82436,#82437,#82438,#82439,#82440,#82441,#82442,#82443,
#82444,#82445,#82446,#82447,#82448,#82449,#82450,#82451,#82452,#82453,#82454,
#82455,#82456,#82457,#82458,#82459,#82460,#82461,#82462,#82463),
 .UNSPECIFIED.,.F.,.F.,(4,2,2,2,2,2,2,2,2,2,2,2,2,2,2,2,2,4),(7.13949123074078,
7.15825374460888,7.2179922538912,7.27521247887906,7.33403878159532,7.39109870458423,
7.45082647635778,7.50900171095632,7.56689066611655,7.62664565486306,7.68414864972785,
7.7440004506624,7.80296907884385,7.85997329598635,7.9196775938442,7.9779974472315,
8.03557740903284,8.08585791009537),.UNSPECIFIED.) ;
#1648 = B_SPLINE_CURVE_WITH_KNOTS('',3,(#82468,#82469,#82470,#82471,#82472,
#82473,#82474,#82475,#82476,#82477,#82478,#82479,#82480,#82481,#82482,#82483,
#82484,#82485,#82486,#82487,#82488,#82489,#82490,#82491,#82492,#82493,#82494,
#82495,#82496,#82497,#82498,#82499,#82500,#82501,#82502,#82503),
 .UNSPECIFIED.,.F.,.F.,(4,2,2,2,2,2,2,2,2,2,2,2,2,2,2,2,2,4),(5.37622687183942,
5.38702250960326,5.44667528576275,5.50363907047652,5.56264942463801,5.62213453916844,
5.67966286689129,5.73945005988841,5.79711619501117,5.85531485867278,5.91497648508351,
5.97194790610636,6.03079582310035,6.09088439256072,6.14828357290543,6.20792599150807,
6.26593197674811,6.32170606963374),.UNSPECIFIED.) ;
#1649 = B_SPLINE_CURVE_WITH_KNOTS('',3,(#82504,#82505,#82506,#82507,#82508,
#82509,#82510,#82511,#82512,#82513,#82514,#82515,#82516,#82517,#82518,#82519,
#82520,#82521,#82522,#82523,#82524,#82525,#82526,#82527,#82528,#82529,#82530,
#82531,#82532,#82533,#82534,#82535,#82536,#82537,#82538,#82539),
 .UNSPECIFIED.,.F.,.F.,(4,2,2,2,2,2,2,2,2,2,2,2,2,2,2,2,2,4),(8.08585791009537,
8.09549597218786,8.15314538334764,8.21242039989169,8.27156797612537,8.32860911320981,
8.38831773648552,8.44681872385912,8.50417468441307,8.56429334890911,8.62212277167029,
8.68090338297569,8.74026085247203,8.79743772848003,8.85718076728487,8.91589420882259,
8.97312504989025,9.032439876577),.UNSPECIFIED.) ;
#1650 = B_SPLINE_CURVE_WITH_KNOTS('',3,(#82544,#82545,#82546,#82547,#82548,
#82549,#82550,#82551,#82552,#82553,#82554,#82555,#82556,#82557,#82558,#82559,
#82560,#82561,#82562,#82563,#82564,#82565,#82566,#82567,#82568,#82569,#82570,
#82571,#82572,#82573,#82574,#82575,#82576,#82577,#82578,#82579),
 .UNSPECIFIED.,.F.,.F.,(4,2,2,2,2,2,2,2,2,2,2,2,2,2,2,2,2,4),(4.43047895939197,
4.45007522884968,4.50969926510265,4.5669061270457,4.62633650352384,4.68484659374169,
4.74273561983522,4.80292366691765,4.86015173224413,4.9187133717519,4.97838620834566,
5.03543961578679,5.09464600810578,5.15359503132235,5.21128816879447,5.27125894855187,
5.3286592324085,5.37622687183942),.UNSPECIFIED.) ;
#1651 = B_SPLINE_CURVE_WITH_KNOTS('',3,(#82580,#82581,#82582,#82583,#82584,
#82585,#82586,#82587,#82588,#82589,#82590,#82591,#82592,#82593,#82594,#82595,
#82596,#82597,#82598,#82599,#82600,#82601,#82602,#82603,#82604,#82605,#82606,
#82607,#82608,#82609,#82610,#82611,#82612,#82613,#82614,#82615,#82616,#82617),
 .UNSPECIFIED.,.F.,.F.,(4,2,2,2,2,2,2,2,2,2,2,2,2,2,2,2,2,2,4),(9.032439876577,
9.03347505180903,9.09151345897655,9.1499072073473,9.20950017382282,9.26685935009706,
9.32657952091107,9.38539515694615,9.44247136996037,9.50220784047952,9.56037205525028,
9.61830724947866,9.67804902641785,9.73554052963516,9.79547082649963,9.85442397084414,
9.91143409586645,9.97114381916621,9.97904550765146),.UNSPECIFIED.) ;
#1652 = B_SPLINE_CURVE_WITH_KNOTS('',3,(#82622,#82623,#82624,#82625,#82626,
#82627,#82628,#82629,#82630,#82631,#82632,#82633,#82634,#82635,#82636,#82637,
#82638,#82639,#82640,#82641,#82642,#82643,#82644,#82645,#82646,#82647,#82648,
#82649,#82650,#82651,#82652,#82653,#82654,#82655,#82656,#82657),
 .UNSPECIFIED.,.F.,.F.,(4,2,2,2,2,2,2,2,2,2,2,2,2,2,2,2,2,4),(3.48575023797641,
3.51399594028383,3.5734997701978,3.63095276691785,3.69066016886127,3.74831136852578,
3.80643429791633,3.86604096895959,3.92296464805189,3.98173649994462,4.04184951588525,
4.09917852154368,4.15874676311374,4.21674528680338,4.27474780856614,4.33439370231729,
4.39142122162925,4.43047895939197),.UNSPECIFIED.) ;
#1653 = B_SPLINE_CURVE_WITH_KNOTS('',3,(#82658,#82659,#82660,#82661,#82662,
#82663,#82664,#82665,#82666,#82667,#82668,#82669,#82670,#82671,#82672,#82673,
#82674,#82675,#82676,#82677,#82678,#82679,#82680,#82681,#82682,#82683,#82684,
#82685,#82686,#82687,#82688,#82689,#82690,#82691,#82692,#82693),
 .UNSPECIFIED.,.F.,.F.,(4,2,2,2,2,2,2,2,2,2,2,2,2,2,2,2,2,4),(9.97904550765146,
10.0294478805367,10.0870653156411,10.1469658748943,10.2045993921111,10.2639450069181,
10.3230729369084,10.3801081197963,10.4398186669585,10.4982996881472,10.5556817539635,
10.6157782501837,10.6735879401908,10.7324274869952,10.7917618523947,10.8489207802873,
10.908661926968,10.9254729108197),.UNSPECIFIED.) ;
#1654 = B_SPLINE_CURVE_WITH_KNOTS('',3,(#82698,#82699,#82700,#82701,#82702,
#82703,#82704,#82705,#82706,#82707,#82708,#82709,#82710,#82711,#82712,#82713,
#82714,#82715,#82716,#82717,#82718,#82719,#82720,#82721,#82722,#82723,#82724,
#82725,#82726,#82727,#82728,#82729,#82730,#82731,#82732,#82733),
 .UNSPECIFIED.,.F.,.F.,(4,2,2,2,2,2,2,2,2,2,2,2,2,2,2,2,2,4),(2.5410263785329,
2.57866932478977,2.63717406289675,2.69497909645909,2.75507795688919,2.81226721150962,
2.87074374700886,2.93035398974217,2.98733419714063,3.04645519099512,3.10541264329701,
3.16302582590397,3.22291178102946,3.28028618337226,3.33856871206754,3.39816287801024,
3.45506667880724,3.48575023797641),.UNSPECIFIED.) ;
#1655 = B_SPLINE_CURVE_WITH_KNOTS('',3,(#82734,#82735,#82736,#82737,#82738,
#82739,#82740,#82741,#82742,#82743,#82744,#82745,#82746,#82747,#82748,#82749,
#82750,#82751,#82752,#82753,#82754,#82755,#82756,#82757,#82758,#82759,#82760,
#82761,#82762,#82763,#82764,#82765,#82766,#82767,#82768,#82769),
 .UNSPECIFIED.,.F.,.F.,(4,2,2,2,2,2,2,2,2,2,2,2,2,2,2,2,2,4),(10.9254729108197,
10.9673518741525,11.0245962962134,11.0849206118767,11.1429360001134,11.2013745918176,
11.2609415930954,11.3182768845568,11.3779883710219,11.436778174129,11.4938561844441,
11.5535855030256,11.6117237029001,11.6696898328819,11.7294030058459,11.7868681658494,
11.846860602723,11.8722070730006),.UNSPECIFIED.) ;
#1656 = B_SPLINE_CURVE_WITH_KNOTS('',3,(#82774,#82775,#82776,#82777,#82778,
#82779,#82780,#82781,#82782,#82783,#82784,#82785,#82786,#82787,#82788,#82789,
#82790,#82791,#82792,#82793,#82794,#82795,#82796,#82797,#82798,#82799,#82800,
#82801,#82802,#82803,#82804,#82805,#82806,#82807,#82808,#82809),
 .UNSPECIFIED.,.F.,.F.,(4,2,2,2,2,2,2,2,2,2,2,2,2,2,2,2,2,4),(1.59524381008426,
1.64219928555692,1.69995479960911,1.75811654543929,1.81778735648274,1.87477859220045,
1.93359025056505,1.99385447979138,2.05122669579738,2.1108385062818,2.16894963367187,
2.22699679299248,2.2867105859981,2.34381635052473,2.40251607132118,2.46217352123779,
2.51932796376252,2.5410263785329),.UNSPECIFIED.) ;
#1657 = B_SPLINE_CURVE_WITH_KNOTS('',3,(#82810,#82811,#82812,#82813,#82814,
#82815,#82816,#82817,#82818,#82819,#82820,#82821,#82822,#82823,#82824,#82825,
#82826,#82827,#82828,#82829,#82830,#82831,#82832,#82833,#82834,#82835,#82836,
#82837,#82838,#82839,#82840,#82841,#82842,#82843,#82844,#82845),
 .UNSPECIFIED.,.F.,.F.,(4,2,2,2,2,2,2,2,2,2,2,2,2,2,2,2,2,4),(11.8722070730006,
11.9057830423993,11.9627849572883,12.0224843188238,12.080757543489,12.1383977592506,
12.1982648617393,12.2558675785037,12.3152681844023,12.3743611588062,12.4313765000627,
12.4910732525112,12.5495191814863,12.6069130219924,12.6669718088517,12.7247467828119,
12.783630310924,12.8183169223007),.UNSPECIFIED.) ;
#1658 = B_SPLINE_CURVE_WITH_KNOTS('',3,(#82850,#82851,#82852,#82853,#82854,
#82855,#82856,#82857,#82858,#82859,#82860,#82861,#82862,#82863,#82864,#82865,
#82866,#82867,#82868,#82869,#82870,#82871,#82872,#82873,#82874,#82875,#82876,
#82877,#82878,#82879,#82880,#82881,#82882,#82883,#82884,#82885),
 .UNSPECIFIED.,.F.,.F.,(4,2,2,2,2,2,2,2,2,2,2,2,2,2,2,2,2,4),(0.649736777376371,
0.705689678240313,0.762957073707775,0.821462804205472,0.88112900735365,
0.938149594548792,0.9973007844438,1.0563910421508,1.11403726413225,1.17395573242052,
1.23142244431764,1.28973859070027,1.34939294812008,1.40635125485932,1.46531509515816,
1.52496337930765,1.58245418488598,1.59524381008426),.UNSPECIFIED.) ;
#1659 = B_SPLINE_CURVE_WITH_KNOTS('',3,(#82886,#82887,#82888,#82889,#82890,
#82891,#82892,#82893,#82894,#82895,#82896,#82897,#82898,#82899,#82900,#82901,
#82902,#82903,#82904,#82905,#82906,#82907,#82908,#82909,#82910,#82911,#82912,
#82913,#82914,#82915,#82916,#82917,#82918,#82919,#82920,#82921),
 .UNSPECIFIED.,.F.,.F.,(4,2,2,2,2,2,2,2,2,2,2,2,2,2,2,2,2,4),(12.8183169223007,
12.8429261623028,12.9000532843054,12.9597768932427,13.0184281247438,13.0756720407192,
13.1359550292795,13.1939323314564,13.2524012731139,13.3119268030521,13.3692232666448,
13.4289104836939,13.4876590852451,13.5447247490731,13.6044312671098,13.6625282462393,
13.7205109861668,13.764829475703),.UNSPECIFIED.) ;
#1660 = B_SPLINE_CURVE_WITH_KNOTS('',3,(#82927,#82928,#82929,#82930,#82931,
#82932,#82933,#82934,#82935,#82936,#82937,#82938,#82939,#82940,#82941,#82942,
#82943,#82944,#82945,#82946,#82947,#82948,#82949,#82950,#82951,#82952,#82953,
#82954,#82955,#82956,#82957,#82958),.UNSPECIFIED.,.F.,.F.,(4,2,2,2,2,2,
2,2,2,2,2,2,2,2,2,4),(-0.604482102223105,-0.604472052630673,-0.558816604903575,
-0.512995341988544,-0.466125939830108,-0.421016120560909,-0.374090744720571,
-0.327859265800465,-0.283024906762521,-0.23608761475075,-0.190362394357742,
-0.144876688170418,-0.0979214349660129,-0.0527340847053595,-0.0268491614321842,
-9.99999981043942E-7),.UNSPECIFIED.) ;
#1661 = B_SPLINE_CURVE_WITH_KNOTS('',3,(#82962,#82963,#82964,#82965,#82966,
#82967,#82968,#82969,#82970,#82971,#82972,#82973,#82974,#82975,#82976,#82977,
#82978,#82979,#82980,#82981,#82982,#82983,#82984,#82985,#82986,#82987,#82988,
#82989,#82990,#82991,#82992,#82993,#82994,#82995,#82996,#82997,#82998,#82999,
#83000,#83001,#83002,#83003,#83004,#83005,#83006,#83007,#83008,#83009,#83010,
#83011,#83012,#83013,#83014,#83015,#83016,#83017,#83018,#83019,#83020,#83021,
#83022,#83023,#83024,#83025,#83026,#83027,#83028,#83029,#83030,#83031,#83032,
#83033,#83034,#83035,#83036,#83037,#83038,#83039,#83040,#83041,#83042,#83043,
#83044,#83045,#83046,#83047,#83048,#83049,#83050,#83051,#83052,#83053,#83054,
#83055,#83056,#83057,#83058),.UNSPECIFIED.,.F.,.F.,(4,3,3,3,3,3,3,3,3,3,
3,3,3,3,3,3,3,3,3,3,3,3,3,3,3,3,3,3,3,3,3,3,4),(0.,0.0325197560323793,0.0361754347737445,
0.0545181792551618,0.0665073209256394,0.0701985195194899,0.0715839281444508,
0.0766179496429377,0.0876742174549116,0.0986799106067661,0.109623686050927,
0.117049763338473,0.128531172361757,0.151540610100312,0.160999394201887,
0.165201627662936,0.175477096788014,0.185820644734618,0.196164192681223,
0.200180615978208,0.204045205104025,0.206337708125956,0.208347839550571,
0.224387966023407,0.244962280061539,0.253570253824267,0.257129272275443,
0.282960548052419,0.285773414391098,0.289578563004044,0.292679154477924,
0.309399625992716,0.323847468004356),.UNSPECIFIED.) ;
#1662 = B_SPLINE_CURVE_WITH_KNOTS('',3,(#83059,#83060,#83061,#83062,#83063,
#83064,#83065,#83066,#83067,#83068,#83069,#83070),.UNSPECIFIED.,.F.,.F.,
(4,2,2,2,2,4),(-11.5393310976055,-11.5013731957114,-11.4621334340822,-11.4153480751354,
-11.370429899528,-11.3541155477015),.UNSPECIFIED.) ;
#1663 = B_SPLINE_CURVE_WITH_KNOTS('',3,(#83075,#83076,#83077,#83078,#83079,
#83080,#83081,#83082,#83083,#83084,#83085,#83086,#83087,#83088,#83089,#83090,
#83091,#83092,#83093,#83094,#83095,#83096,#83097,#83098,#83099,#83100,#83101,
#83102,#83103,#83104,#83105,#83106,#83107,#83108,#83109,#83110),
 .UNSPECIFIED.,.F.,.F.,(4,2,2,2,2,2,2,2,2,2,2,2,2,2,2,2,2,4),(-1.34731169092089,
-1.3412018153619,-1.29589168841991,-1.24955082083875,-1.20306965837919,
-1.15826389470243,-1.11138171165322,-1.06538584417928,-1.02039676291541,
-0.973136021319122,-0.927670180887149,-0.881634272236604,-0.834974620519227,
-0.790022224945155,-0.743078246417081,-0.696892986888225,-0.651937532555577,
-0.604482102223105),.UNSPECIFIED.) ;
#1664 = B_SPLINE_CURVE_WITH_KNOTS('',3,(#83111,#83112,#83113,#83114,#83115,
#83116,#83117,#83118,#83119,#83120,#83121,#83122,#83123,#83124,#83125,#83126,
#83127,#83128,#83129,#83130,#83131,#83132,#83133,#83134,#83135,#83136,#83137,
#83138,#83139,#83140,#83141,#83142,#83143,#83144,#83145,#83146),
 .UNSPECIFIED.,.F.,.F.,(4,2,2,2,2,2,2,2,2,2,2,2,2,2,2,2,2,4),(-11.3541155477015,
-11.3237621770439,-11.2778677119073,-11.2323992784145,-11.1851333428345,
-11.1402220975301,-11.0942245020397,-11.0473852179779,-11.002595542972,
-10.9561167440097,-10.9099470224542,-10.8646457619258,-10.8175607661819,
-10.7725610586643,-10.7267296728004,-10.6799275400698,-10.6352322960093,
-10.6125286589702),.UNSPECIFIED.) ;
#1665 = B_SPLINE_CURVE_WITH_KNOTS('',3,(#83151,#83152,#83153,#83154,#83155,
#83156,#83157,#83158,#83159,#83160,#83161,#83162,#83163,#83164,#83165,#83166,
#83167,#83168,#83169,#83170,#83171,#83172,#83173,#83174,#83175,#83176,#83177,
#83178,#83179,#83180,#83181,#83182,#83183,#83184,#83185,#83186),
 .UNSPECIFIED.,.F.,.F.,(4,2,2,2,2,2,2,2,2,2,2,2,2,2,2,2,2,4),(-2.08931556787976,
-2.07717317487852,-2.03206502854522,-1.98490565151034,-1.93867897462963,
-1.89393154733524,-1.8470655465658,-1.8013407535219,-1.75604490428414,-1.70908360063356,
-1.66389336498396,-1.61717126675813,-1.57083532596603,-1.5260973037643,
-1.47924023671116,-1.43339866758495,-1.38829377159172,-1.34731169092089),
 .UNSPECIFIED.) ;
#1666 = B_SPLINE_CURVE_WITH_KNOTS('',3,(#83187,#83188,#83189,#83190,#83191,
#83192,#83193,#83194,#83195,#83196,#83197,#83198,#83199,#83200,#83201,#83202,
#83203,#83204,#83205,#83206,#83207,#83208,#83209,#83210,#83211,#83212,#83213,
#83214,#83215,#83216,#83217,#83218,#83219,#83220,#83221,#83222),
 .UNSPECIFIED.,.F.,.F.,(4,2,2,2,2,2,2,2,2,2,2,2,2,2,2,2,2,4),(-10.6125286589702,
-10.5889100367047,-10.5423832940755,-10.4972140874325,-10.4502727021239,
-10.4051066814913,-10.3594048645256,-10.3126050385905,-10.267925831595,
-10.2217251541091,-10.174778107769,-10.1297038549222,-10.0828665268164,
-10.0374670241972,-9.99185573135441,-9.94502566253314,-9.9002901133366,
-9.87140270043892),.UNSPECIFIED.) ;
#1667 = B_SPLINE_CURVE_WITH_KNOTS('',3,(#83227,#83228,#83229,#83230,#83231,
#83232,#83233,#83234,#83235,#83236,#83237,#83238,#83239,#83240,#83241,#83242,
#83243,#83244,#83245,#83246,#83247,#83248,#83249,#83250,#83251,#83252,#83253,
#83254,#83255,#83256,#83257,#83258,#83259,#83260,#83261,#83262),
 .UNSPECIFIED.,.F.,.F.,(4,2,2,2,2,2,2,2,2,2,2,2,2,2,2,2,2,4),(-2.83245463856665,
-2.81370343304387,-2.76880307515479,-2.72186916108506,-2.67574833193176,
-2.63076864197808,-2.58337370011299,-2.53778287170268,-2.49186092435614,
-2.44506390373703,-2.40002203430969,-2.35312926746393,-2.30697313780473,
-2.26214711373248,-2.21524024196913,-2.16959241343306,-2.12404413386628,
-2.08931556787976),.UNSPECIFIED.) ;
#1668 = B_SPLINE_CURVE_WITH_KNOTS('',3,(#83263,#83264,#83265,#83266,#83267,
#83268,#83269,#83270,#83271,#83272,#83273,#83274,#83275,#83276,#83277,#83278,
#83279,#83280,#83281,#83282,#83283,#83284,#83285,#83286,#83287,#83288,#83289,
#83290,#83291,#83292,#83293,#83294,#83295,#83296,#83297,#83298),
 .UNSPECIFIED.,.F.,.F.,(4,2,2,2,2,2,2,2,2,2,2,2,2,2,2,2,2,4),(-9.87140270043892,
-9.85417324171317,-9.80735552697951,-9.76235647797716,-9.71560253017239,
-9.66986064457499,-9.62431652276782,-9.57696752511082,-9.53210483846283,
-9.48603207223652,-9.43919136581251,-9.39434694969904,-9.34779975847588,
-9.30183561623833,-9.25647793175298,-9.20933024089469,-9.16442679755697,
-9.12966134408518),.UNSPECIFIED.) ;
#1669 = B_SPLINE_CURVE_WITH_KNOTS('',3,(#83303,#83304,#83305,#83306,#83307,
#83308,#83309,#83310,#83311,#83312,#83313,#83314,#83315,#83316,#83317,#83318,
#83319,#83320,#83321,#83322,#83323,#83324,#83325,#83326,#83327,#83328,#83329,
#83330,#83331,#83332,#83333,#83334,#83335,#83336,#83337,#83338),
 .UNSPECIFIED.,.F.,.F.,(4,2,2,2,2,2,2,2,2,2,2,2,2,2,2,2,2,4),(-3.57487681123277,
-3.54968647514162,-3.50493349970735,-3.45805565860227,-3.41224821672189,
-3.36705025131333,-3.31999785751033,-3.27472319297991,-3.22820685407033,
-3.18177117344887,-3.13698401394248,-3.09009589679917,-3.04414982511993,
-2.9991008402324,-2.95189561122699,-2.90648023451509,-2.86030375025126,
-2.83245463856665),.UNSPECIFIED.) ;
#1670 = B_SPLINE_CURVE_WITH_KNOTS('',3,(#83339,#83340,#83341,#83342,#83343,
#83344,#83345,#83346,#83347,#83348,#83349,#83350,#83351,#83352,#83353,#83354,
#83355,#83356,#83357,#83358,#83359,#83360,#83361,#83362,#83363,#83364,#83365,
#83366,#83367,#83368,#83369,#83370,#83371,#83372,#83373,#83374),
 .UNSPECIFIED.,.F.,.F.,(4,2,2,2,2,2,2,2,2,2,2,2,2,2,2,2,2,4),(-9.12966134408518,
-9.11854010652168,-9.07175780388743,-9.02705303938877,-8.98068119937531,
-8.93440550666307,-8.88920021314424,-8.8422177708298,-8.79719195681835,
-8.75145611879147,-8.70469585620383,-8.66005189617882,-8.61382199987997,
-8.56716018383391,-8.52207136168262,-8.47521592007197,-8.42999357961432,
-8.38917606320042),.UNSPECIFIED.) ;
#1671 = B_SPLINE_CURVE_WITH_KNOTS('',3,(#83379,#83380,#83381,#83382,#83383,
#83384,#83385,#83386,#83387,#83388,#83389,#83390,#83391,#83392,#83393,#83394,
#83395,#83396,#83397,#83398,#83399,#83400,#83401,#83402,#83403,#83404,#83405,
#83406,#83407,#83408,#83409,#83410,#83411,#83412,#83413,#83414),
 .UNSPECIFIED.,.F.,.F.,(4,2,2,2,2,2,2,2,2,2,2,2,2,2,2,2,2,4),(-4.31766659413976,
-4.28659846302871,-4.24170055646562,-4.19474588369237,-4.1490979597056,
-4.10340702113605,-4.0565409612618,-4.01143575579773,-3.96405683387488,
-3.91784449462356,-3.87305125486111,-3.82615059506103,-3.78044321036394,
-3.73502561909169,-3.68808695293045,-3.64291630589686,-3.59599189048964,
-3.57487681123277),.UNSPECIFIED.) ;
#1672 = B_SPLINE_CURVE_WITH_KNOTS('',3,(#83415,#83416,#83417,#83418,#83419,
#83420,#83421,#83422,#83423,#83424,#83425,#83426,#83427,#83428,#83429,#83430,
#83431,#83432,#83433,#83434,#83435,#83436,#83437,#83438,#83439,#83440,#83441,
#83442,#83443,#83444,#83445,#83446,#83447,#83448,#83449,#83450,#83451,#83452),
 .UNSPECIFIED.,.F.,.F.,(4,2,2,2,2,2,2,2,2,2,2,2,2,2,2,2,2,2,4),(-8.38917606320042,
-8.38437093820375,-8.33759893938715,-8.29293925621511,-8.24681517513577,
-8.199713215607,-8.15470298046625,-8.10793414450284,-8.06245545585829,-8.01690611295866,
-7.97009066411063,-7.92534712298602,-7.87929000553699,-7.83248902005484,
-7.78754258654849,-7.74084506106679,-7.69498578432255,-7.64949066614786,
-7.64797087659483),.UNSPECIFIED.) ;
#1673 = B_SPLINE_CURVE_WITH_KNOTS('',3,(#83457,#83458,#83459,#83460,#83461,
#83462,#83463,#83464,#83465,#83466,#83467,#83468,#83469,#83470,#83471,#83472,
#83473,#83474,#83475,#83476,#83477,#83478,#83479,#83480,#83481,#83482,#83483,
#83484,#83485,#83486,#83487,#83488,#83489,#83490,#83491,#83492),
 .UNSPECIFIED.,.F.,.F.,(4,2,2,2,2,2,2,2,2,2,2,2,2,2,2,2,2,4),(-5.06189018830862,
-5.0246914476009,-4.97950438607291,-4.93227395428298,-4.88683167766163,
-4.8404383466902,-4.79381815898027,-4.74888605317594,-4.70188421904935,
-4.65574875023561,-4.61066410116121,-4.56325818761082,-4.51765389759663,
-4.47155159378806,-4.424747023233,-4.3796963332284,-4.33275745326406,-4.31766659413976),
 .UNSPECIFIED.) ;
#1674 = B_SPLINE_CURVE_WITH_KNOTS('',3,(#83493,#83494,#83495,#83496,#83497,
#83498,#83499,#83500,#83501,#83502,#83503,#83504,#83505,#83506,#83507,#83508,
#83509,#83510,#83511,#83512,#83513,#83514,#83515,#83516,#83517,#83518,#83519,
#83520,#83521,#83522,#83523,#83524,#83525,#83526,#83527,#83528),
 .UNSPECIFIED.,.F.,.F.,(4,2,2,2,2,2,2,2,2,2,2,2,2,2,2,2,2,4),(-7.64797087659483,
-7.60219585475731,-7.55729228392319,-7.51126807237905,-7.46442153868907,
-7.41961221540445,-7.37310843911013,-7.32698746884331,-7.28166466461712,
-7.23455623843522,-7.18957659516422,-7.14372391229961,-7.09692002617542,
-7.05221709702265,-7.0058749010068,-6.95940823504211,-6.91422291151097,
-6.90653741160255),.UNSPECIFIED.) ;
#1675 = B_SPLINE_CURVE_WITH_KNOTS('',3,(#83533,#83534,#83535,#83536,#83537,
#83538,#83539,#83540,#83541,#83542,#83543,#83544,#83545,#83546,#83547,#83548,
#83549,#83550,#83551,#83552,#83553,#83554,#83555,#83556,#83557,#83558,#83559,
#83560,#83561,#83562,#83563,#83564,#83565,#83566,#83567,#83568),
 .UNSPECIFIED.,.F.,.F.,(4,2,2,2,2,2,2,2,2,2,2,2,2,2,2,2,2,4),(-5.80568588485352,
-5.76254620022904,-5.71693605613462,-5.66994085357101,-5.62471389566346,
-5.57751982231786,-5.53116693801469,-5.4863196315096,-5.43934574413778,
-5.39349474889934,-5.34812844394237,-5.30103565386192,-5.25571981922943,
-5.20895608059552,-5.16248732504782,-5.11763667173845,-5.07066608480533,
-5.06189018830862),.UNSPECIFIED.) ;
#1676 = B_SPLINE_CURVE_WITH_KNOTS('',3,(#83569,#83570,#83571,#83572,#83573,
#83574,#83575,#83576,#83577,#83578,#83579,#83580,#83581,#83582,#83583,#83584,
#83585,#83586,#83587,#83588,#83589,#83590,#83591,#83592,#83593,#83594,#83595,
#83596,#83597,#83598,#83599,#83600,#83601,#83602,#83603,#83604),
 .UNSPECIFIED.,.F.,.F.,(4,2,2,2,2,2,2,2,2,2,2,2,2,2,2,2,2,4),(-6.90653741160255,
-6.86726387513544,-6.82212926045643,-6.77641183790277,-6.72961536262379,
-6.68494008118346,-6.63872492763704,-6.59184615335233,-6.54676151251456,
-6.49991264254877,-6.45455352979052,-6.40893266759151,-6.3621107437088,
-6.31738944954778,-6.27126398027799,-6.22445353975894,-6.17944803528691,
-6.16535718549382),.UNSPECIFIED.) ;
#1677 = B_SPLINE_CURVE_WITH_KNOTS('',3,(#83609,#83610,#83611,#83612,#83613,
#83614,#83615,#83616,#83617,#83618,#83619,#83620,#83621,#83622,#83623,#83624,
#83625,#83626,#83627,#83628,#83629,#83630,#83631,#83632,#83633,#83634,#83635,
#83636,#83637,#83638,#83639,#83640,#83641,#83642,#83643,#83644,#83645,#83646),
 .UNSPECIFIED.,.F.,.F.,(4,2,2,2,2,2,2,2,2,2,2,2,2,2,2,2,2,2,4),(-6.5485693399367,
-6.54469452430869,-6.4978255135919,-6.45306354789751,-6.40687923124368,
-6.35954447090233,-6.31446735523363,-6.26763036535901,-6.22197751540764,
-6.1763582302673,-6.12943610112621,-6.08457118639726,-6.03844133336597,
-5.99153489517415,-5.94651305142779,-5.90023767360354,-5.85532263233972,
-5.80831310746145,-5.80568588485352),.UNSPECIFIED.) ;
#1678 = B_SPLINE_CURVE_WITH_KNOTS('',3,(#83647,#83648,#83649,#83650,#83651,
#83652,#83653,#83654,#83655,#83656,#83657,#83658,#83659,#83660,#83661,#83662,
#83663,#83664,#83665,#83666,#83667,#83668,#83669,#83670,#83671,#83672,#83673,
#83674,#83675,#83676,#83677,#83678,#83679,#83680,#83681,#83682),
 .UNSPECIFIED.,.F.,.F.,(4,2,2,2,2,2,2,2,2,2,2,2,2,2,2,2,2,4),(-6.16535718549382,
-6.13268670498756,-6.08699929169078,-6.04145007032189,-5.99409453761209,
-5.94925789990988,-5.90318034616918,-5.85635525600001,-5.81150873241543,
-5.76495891990493,-5.72024348147513,-5.67344467205068,-5.62788672168556,
-5.58247359644929,-5.53569334689852,-5.49067310216224,-5.44367706639317,
-5.4240172864351),.UNSPECIFIED.) ;
#1679 = B_SPLINE_CURVE_WITH_KNOTS('',3,(#83687,#83688,#83689,#83690,#83691,
#83692,#83693,#83694,#83695,#83696,#83697,#83698,#83699,#83700,#83701,#83702,
#83703,#83704,#83705,#83706,#83707,#83708,#83709,#83710,#83711,#83712,#83713,
#83714,#83715,#83716,#83717,#83718,#83719,#83720,#83721,#83722),
 .UNSPECIFIED.,.F.,.F.,(4,2,2,2,2,2,2,2,2,2,2,2,2,2,2,2,2,4),(-7.2903982875493,
-7.28026237605557,-7.23340402376256,-7.18864394453266,-7.14223433209178,
-7.09575895219682,-7.05051031092062,-7.00348478836652,-6.95832150536336,
-6.91254051700472,-6.86569340257366,-6.82096968707691,-6.77469126511584,
-6.72780971778659,-6.68266609136878,-6.63575535824411,-6.59037439851765,
-6.5485693399367),.UNSPECIFIED.) ;
#1680 = B_SPLINE_CURVE_WITH_KNOTS('',3,(#83723,#83724,#83725,#83726,#83727,
#83728,#83729,#83730,#83731,#83732,#83733,#83734,#83735,#83736,#83737,#83738,
#83739,#83740,#83741,#83742,#83743,#83744,#83745,#83746,#83747,#83748,#83749,
#83750,#83751,#83752,#83753,#83754,#83755,#83756,#83757,#83758),
 .UNSPECIFIED.,.F.,.F.,(4,2,2,2,2,2,2,2,2,2,2,2,2,2,2,2,2,4),(-5.4240172864351,
-5.39753691479611,-5.3528911128382,-5.30612883532888,-5.26048854219916,
-5.21532000638465,-5.16844399254702,-5.12333656913247,-5.07677055162506,
-5.03051629773879,-4.98586970138458,-4.93911182979272,-4.89334974740763,
-4.84836207585291,-4.80135035441491,-4.75611829156816,-4.70992336812542,
-4.68362193225928),.UNSPECIFIED.) ;
#1681 = B_SPLINE_CURVE_WITH_KNOTS('',3,(#83763,#83764,#83765,#83766,#83767,
#83768,#83769,#83770,#83771,#83772,#83773,#83774,#83775,#83776,#83777,#83778,
#83779,#83780,#83781,#83782,#83783,#83784,#83785,#83786,#83787,#83788,#83789,
#83790,#83791,#83792,#83793,#83794,#83795,#83796,#83797,#83798),
 .UNSPECIFIED.,.F.,.F.,(4,2,2,2,2,2,2,2,2,2,2,2,2,2,2,2,2,4),(-8.03313136846868,
-8.01678752022364,-7.96992196508481,-7.92490377627534,-7.87813124306105,
-7.83224506796249,-7.78667850411988,-7.73930857188702,-7.694358942822,-7.64826272925189,
-7.60135756548507,-7.55648212666153,-7.50990705070329,-7.46376909578636,
-7.41837882573787,-7.37119949443887,-7.32618295935356,-7.2903982875493),
 .UNSPECIFIED.) ;
#1682 = B_SPLINE_CURVE_WITH_KNOTS('',3,(#83799,#83800,#83801,#83802,#83803,
#83804,#83805,#83806,#83807,#83808,#83809,#83810,#83811,#83812,#83813,#83814,
#83815,#83816,#83817,#83818,#83819,#83820,#83821,#83822,#83823,#83824,#83825,
#83826,#83827,#83828,#83829,#83830,#83831,#83832,#83833,#83834),
 .UNSPECIFIED.,.F.,.F.,(4,2,2,2,2,2,2,2,2,2,2,2,2,2,2,2,2,4),(-4.68362193225928,
-4.66351951710304,-4.61879451160515,-4.57200673789761,-4.52608576131031,
-4.48120275436424,-4.43401758077193,-4.38862540199452,-4.34272311312387,
-4.29613678696753,-4.25125494346797,-4.20440028285465,-4.15828570684597,
-4.11342482121262,-4.06603060008173,-4.02044463673821,-3.97474347018052,
-3.94185895807078),.UNSPECIFIED.) ;
#1683 = B_SPLINE_CURVE_WITH_KNOTS('',3,(#83839,#83840,#83841,#83842,#83843,
#83844,#83845,#83846,#83847,#83848,#83849,#83850,#83851,#83852,#83853,#83854,
#83855,#83856,#83857,#83858,#83859,#83860,#83861,#83862,#83863,#83864,#83865,
#83866,#83867,#83868,#83869,#83870,#83871,#83872,#83873,#83874),
 .UNSPECIFIED.,.F.,.F.,(4,2,2,2,2,2,2,2,2,2,2,2,2,2,2,2,2,4),(-8.77491333060422,
-8.75231389418036,-8.70562932404755,-8.66046095430428,-8.61352221281336,
-8.56825768216331,-8.5225551658115,-8.47571560127791,-8.43099402430489,
-8.38479009824252,-8.33766978968508,-8.29258457966775,-8.2457373223502,
-8.20022201624112,-8.15459759623412,-8.10771807906936,-8.06291978776965,
-8.03313136846868),.UNSPECIFIED.) ;
#1684 = B_SPLINE_CURVE_WITH_KNOTS('',3,(#83875,#83876,#83877,#83878,#83879,
#83880,#83881,#83882,#83883,#83884,#83885,#83886,#83887,#83888,#83889,#83890,
#83891,#83892,#83893,#83894,#83895,#83896,#83897,#83898,#83899,#83900,#83901,
#83902,#83903,#83904,#83905,#83906,#83907,#83908,#83909,#83910),
 .UNSPECIFIED.,.F.,.F.,(4,2,2,2,2,2,2,2,2,2,2,2,2,2,2,2,2,4),(-3.94185895807078,
-3.92794359307557,-3.88290124803901,-3.83605797395444,-3.78989399397843,
-3.74514397062485,-3.698289555497,-3.65263018309304,-3.60725206137288,-3.56036298328301,
-3.5152399334815,-3.46835185771871,-3.42209586200823,-3.37738781550701,
-3.33055699830715,-3.28479866434645,-3.23964153573233,-3.20015024205927),
 .UNSPECIFIED.) ;
#1685 = B_SPLINE_CURVE_WITH_KNOTS('',3,(#83915,#83916,#83917,#83918,#83919,
#83920,#83921,#83922,#83923,#83924,#83925,#83926,#83927,#83928,#83929,#83930,
#83931,#83932,#83933,#83934,#83935,#83936,#83937,#83938,#83939,#83940,#83941,
#83942,#83943,#83944,#83945,#83946,#83947,#83948,#83949,#83950),
 .UNSPECIFIED.,.F.,.F.,(4,2,2,2,2,2,2,2,2,2,2,2,2,2,2,2,2,4),(-9.51681717340635,
-9.48746469526357,-9.44146155525688,-9.39601566694291,-9.34877545441454,
-9.30381320687154,-9.25783760349915,-9.21097989719694,-9.16619559342027,
-9.11973524996446,-9.07342976330784,-9.02814050699756,-8.98107005349904,
-8.93599434700291,-8.89017400244873,-8.84334241713347,-8.79862810084481,
-8.77491333060422),.UNSPECIFIED.) ;
#1686 = B_SPLINE_CURVE_WITH_KNOTS('',3,(#83951,#83952,#83953,#83954,#83955,
#83956,#83957,#83958,#83959,#83960,#83961,#83962,#83963,#83964,#83965,#83966,
#83967,#83968,#83969,#83970,#83971,#83972,#83973,#83974,#83975,#83976,#83977,
#83978,#83979,#83980,#83981,#83982,#83983,#83984,#83985,#83986),
 .UNSPECIFIED.,.F.,.F.,(4,2,2,2,2,2,2,2,2,2,2,2,2,2,2,2,2,4),(-3.20015024205927,
-3.19263985153786,-3.14741383327045,-3.10093486301163,-3.05454962939341,
-3.00980937954436,-2.9629691524755,-2.91707326441536,-2.87206684967415,
-2.82491343575938,-2.77954774098522,-2.73341022654117,-2.68686135074236,
-2.64200999664347,-2.59512494148472,-2.54905534698971,-2.50412022980151,
-2.45812360193803),.UNSPECIFIED.) ;
#1687 = B_SPLINE_CURVE_WITH_KNOTS('',3,(#83991,#83992,#83993,#83994,#83995,
#83996,#83997,#83998,#83999,#84000,#84001,#84002,#84003,#84004,#84005,#84006,
#84007,#84008,#84009,#84010,#84011,#84012,#84013,#84014,#84015,#84016,#84017,
#84018,#84019,#84020,#84021,#84022,#84023,#84024,#84025,#84026),
 .UNSPECIFIED.,.F.,.F.,(4,2,2,2,2,2,2,2,2,2,2,2,2,2,2,2,2,4),(-10.2599619460435,
-10.2238795993298,-10.1784210421296,-10.1327140734422,-10.0857987625166,
-10.0409865492377,-9.99477371905538,-9.94787016080768,-9.90277888516916,
-9.85592862759665,-9.81013720350877,-9.76450078117451,-9.71705493603555,
-9.67212388099948,-9.6259580110907,-9.57903744350876,-9.53410435631313,
-9.51681717340635),.UNSPECIFIED.) ;
#1688 = B_SPLINE_CURVE_WITH_KNOTS('',3,(#84027,#84028,#84029,#84030,#84031,
#84032,#84033,#84034,#84035,#84036,#84037,#84038,#84039,#84040,#84041,#84042,
#84043,#84044,#84045,#84046,#84047,#84048,#84049,#84050,#84051,#84052,#84053,
#84054,#84055,#84056,#84057,#84058,#84059,#84060,#84061,#84062,#84063,#84064),
 .UNSPECIFIED.,.F.,.F.,(4,2,2,2,2,2,2,2,2,2,2,2,2,2,2,2,2,2,4),(-2.45812360193803,
-2.45677819111201,-2.41123806917093,-2.36535712296393,-2.31861252364742,
-2.27362101086785,-2.22677840151894,-2.18067423534073,-2.13589460996303,
-2.08903779312993,-2.04344152483191,-1.99793613709164,-1.95111841743952,
-1.9060613966591,-1.85894205246388,-1.81276844099364,-1.76806895369967,
-1.72125375882939,-1.71626027993097),.UNSPECIFIED.) ;
#1689 = B_SPLINE_CURVE_WITH_KNOTS('',3,(#84069,#84070,#84071,#84072,#84073,
#84074,#84075,#84076,#84077,#84078,#84079,#84080,#84081,#84082,#84083,#84084,
#84085,#84086,#84087,#84088,#84089,#84090,#84091,#84092,#84093,#84094,#84095,
#84096,#84097,#84098,#84099,#84100,#84101,#84102,#84103,#84104),
 .UNSPECIFIED.,.F.,.F.,(4,2,2,2,2,2,2,2,2,2,2,2,2,2,2,2,2,4),(-11.0024392821081,
-10.9599663286644,-10.9148936873785,-10.8689576925085,-10.8220632122557,
-10.7772755291895,-10.7308486859947,-10.6842749853735,-10.6390062126163,
-10.5919607038823,-10.5467296415202,-10.5009275958716,-10.4540391183822,
-10.4092759003239,-10.3629748375851,-10.3159858990373,-10.2708164187479,
-10.2599619460435),.UNSPECIFIED.) ;
#1690 = B_SPLINE_CURVE_WITH_KNOTS('',3,(#84105,#84106,#84107,#84108,#84109,
#84110,#84111,#84112,#84113,#84114,#84115,#84116,#84117,#84118,#84119,#84120,
#84121,#84122,#84123,#84124,#84125,#84126,#84127,#84128,#84129,#84130,#84131,
#84132,#84133,#84134,#84135,#84136,#84137,#84138,#84139,#84140),
 .UNSPECIFIED.,.F.,.F.,(4,2,2,2,2,2,2,2,2,2,2,2,2,2,2,2,2,4),(-1.71626027993097,
-1.67558165604805,-1.63032975843029,-1.58342285229462,-1.53828482577707,
-1.49160342090406,-1.44532162530017,-1.40063343013664,-1.35382800245341,
-1.30804024643797,-1.2629808833479,-1.21594447590769,-1.17068763509309,
-1.12438875183991,-1.07796278093185,-1.03320894854416,-0.986379336876156,
-0.975053485488691),.UNSPECIFIED.) ;
#1691 = B_SPLINE_CURVE_WITH_KNOTS('',3,(#84145,#84146,#84147,#84148,#84149,
#84150,#84151,#84152,#84153,#84154,#84155,#84156,#84157,#84158,#84159,#84160,
#84161,#84162,#84163,#84164,#84165,#84166,#84167,#84168,#84169,#84170,#84171,
#84172,#84173,#84174,#84175,#84176,#84177,#84178,#84179,#84180,#84181,#84182),
 .UNSPECIFIED.,.F.,.F.,(4,2,2,2,2,2,2,2,2,2,2,2,2,2,2,2,2,2,4),(-11.745553964402,
-11.7437796313797,-11.6968771639769,-11.6520478978994,-11.6059097355514,
-11.5590219451859,-11.5139958135559,-11.4672156546915,-11.4212575032449,
-11.3756812580484,-11.328302426854,-11.2833094575338,-11.2372030713339,
-11.1902673929136,-11.1453764273601,-11.0987890831327,-11.0525649378165,
-11.0071599187327,-11.0024392821081),.UNSPECIFIED.) ;
#1692 = B_SPLINE_CURVE_WITH_KNOTS('',3,(#84183,#84184,#84185,#84186,#84187,
#84188,#84189,#84190,#84191,#84192,#84193,#84194,#84195,#84196,#84197,#84198,
#84199,#84200,#84201,#84202,#84203,#84204,#84205,#84206,#84207,#84208,#84209,
#84210,#84211,#84212,#84213,#84214,#84215,#84216,#84217,#84218),
 .UNSPECIFIED.,.F.,.F.,(4,2,2,2,2,2,2,2,2,2,2,2,2,2,2,2,2,4),(-0.975053485488691,
-0.940438383434336,-0.895496741425073,-0.848292684069909,-0.802881195188261,
-0.756889100969424,-0.710285662172893,-0.665387348006602,-0.618496985028334,
-0.572367719394815,-0.527461816105139,-0.480054142080902,-0.434454029561906,
-0.388678699600084,-0.341866450150363,-0.296811533381677,-0.249941016724657,
-0.232520228075875),.UNSPECIFIED.) ;
#1693 = B_SPLINE_CURVE_WITH_KNOTS('',3,(#84224,#84225,#84226,#84227,#84228,
#84229,#84230,#84231,#84232,#84233,#84234,#84235),.UNSPECIFIED.,.F.,.F.,
(4,2,2,2,2,4),(-0.597330195429814,-0.544079370208448,-0.490056450117875,
-0.432782108807466,-0.373472117043514,-0.370559454039791),.UNSPECIFIED.) ;
#1694 = B_SPLINE_CURVE_WITH_KNOTS('',3,(#84236,#84237,#84238,#84239,#84240,
#84241,#84242,#84243,#84244,#84245,#84246,#84247,#84248,#84249,#84250,#84251,
#84252,#84253,#84254,#84255),.UNSPECIFIED.,.F.,.F.,(4,2,2,2,2,2,2,2,2,4),
(-0.649716652274618,-0.564337691326781,-0.481346182278479,-0.363784182044033,
-0.257506122927,-0.162647153734189,-0.114596047443497,-0.051841763469862,
-0.0257254202730378,0.),.UNSPECIFIED.) ;
#1695 = B_SPLINE_CURVE_WITH_KNOTS('',3,(#84259,#84260,#84261,#84262,#84263,
#84264,#84265,#84266,#84267,#84268,#84269,#84270),.UNSPECIFIED.,.F.,.F.,
(4,2,2,2,2,4),(0.,0.0418293556303661,0.0810203615126183,0.121024586302138,
0.157958985747223,0.188938551649128),.UNSPECIFIED.) ;
#1696 = B_SPLINE_CURVE_WITH_KNOTS('',3,(#84271,#84272,#84273,#84274,#84275,
#84276,#84277,#84278,#84279,#84280,#84281,#84282,#84283,#84284),
 .UNSPECIFIED.,.F.,.F.,(4,2,2,2,2,2,4),(-0.370559454039791,-0.314596141147387,
-0.247797040916131,-0.17177268662274,-0.0929222455585059,-0.0416908555263841,
-9.99999990425327E-7),.UNSPECIFIED.) ;
#1697 = B_SPLINE_CURVE_WITH_KNOTS('',3,(#84287,#84288,#84289,#84290,#84291,
#84292,#84293,#84294,#84295,#84296,#84297,#84298,#84299,#84300),
 .UNSPECIFIED.,.F.,.F.,(4,2,2,2,2,2,4),(-0.232520228075875,-0.203766248810284,
-0.158983315267675,-0.112100958247863,-0.0664320735278172,-0.0337545420634901,
-9.9999999686462E-7),.UNSPECIFIED.) ;
#1698 = B_SPLINE_CURVE_WITH_KNOTS('',3,(#84303,#84304,#84305,#84306,#84307,
#84308,#84309,#84310,#84311,#84312),.UNSPECIFIED.,.F.,.F.,(4,2,2,2,4),(-11.8840105514171,
-11.8593886360263,-11.834981196036,-11.789408525476,-11.745553964402),
 .UNSPECIFIED.) ;
#1699 = B_SPLINE_CURVE_WITH_KNOTS('',3,(#84315,#84316,#84317,#84318,#84319,
#84320,#84321,#84322,#84323,#84324,#84325,#84326,#84327,#84328,#84329,#84330,
#84331,#84332,#84333,#84334,#84335,#84336,#84337,#84338,#84339,#84340,#84341,
#84342,#84343,#84344),.UNSPECIFIED.,.F.,.F.,(4,2,2,2,2,2,2,2,2,2,2,2,2,
2,4),(13.764829475703,13.7801798863136,13.8376035555737,13.897643352408,
13.956519485524,14.0134991405525,14.073172406556,14.1313993619064,14.189048326989,
14.2488660827664,14.3064227017816,14.3658641164806,14.4249063546466,14.4790961696761,
14.5339228824178),.UNSPECIFIED.) ;
#1700 = B_SPLINE_CURVE_WITH_KNOTS('',3,(#84347,#84348,#84349,#84350,#84351,
#84352,#84353,#84354,#84355,#84356,#84357,#84358,#84359,#84360,#84361,#84362,
#84363,#84364,#84365,#84366,#84367,#84368,#84369,#84370,#84371,#84372,#84373,
#84374),.UNSPECIFIED.,.F.,.F.,(4,2,2,2,2,2,2,2,2,2,2,2,2,4),(9.99999998019281E-7,
0.0303227215428037,0.0604117772912196,0.118540071650349,0.176589582480443,
0.236954853625382,0.294123775847925,0.352848945254168,0.412557664472652,
0.469738883770964,0.529106788707932,0.587728785588294,0.645562701786344,
0.649736777376371),.UNSPECIFIED.) ;
#1701 = B_SPLINE_CURVE_WITH_KNOTS('',3,(#84455,#84456,#84457,#84458,#84459,
#84460,#84461,#84462,#84463,#84464,#84465,#84466,#84467,#84468,#84469,#84470),
 .UNSPECIFIED.,.F.,.F.,(4,2,2,2,2,2,2,4),(-0.393680344589454,-0.341967463828253,
-0.280075465042844,-0.199030941955768,-0.120297878012763,-0.0601931247465125,
-0.0292201673629089,0.),.UNSPECIFIED.) ;
#1702 = B_SPLINE_CURVE_WITH_KNOTS('',3,(#84471,#84472,#84473,#84474,#84475,
#84476,#84477,#84478,#84479,#84480,#84481,#84482,#84483,#84484,#84485,#84486),
 .UNSPECIFIED.,.F.,.F.,(4,2,2,2,2,2,2,4),(-0.334612951676255,-0.279460360491098,
-0.2151903907044,-0.163552299907468,-0.123594611698629,-0.0765880757042877,
-0.0381084216339553,-1.00000011143964E-6),.UNSPECIFIED.) ;
#1703 = B_SPLINE_CURVE_WITH_KNOTS('',3,(#85513,#85514,#85515,#85516,#85517,
#85518,#85519,#85520,#85521,#85522,#85523,#85524,#85525,#85526,#85527,#85528,
#85529,#85530,#85531,#85532,#85533,#85534,#85535,#85536,#85537,#85538,#85539,
#85540,#85541,#85542,#85543,#85544,#85545,#85546,#85547,#85548,#85549,#85550,
#85551,#85552,#85553,#85554,#85555,#85556,#85557,#85558,#85559,#85560,#85561,
#85562,#85563,#85564,#85565,#85566,#85567,#85568,#85569,#85570,#85571,#85572,
#85573,#85574,#85575,#85576,#85577,#85578,#85579,#85580,#85581,#85582,#85583,
#85584,#85585,#85586,#85587,#85588,#85589,#85590,#85591,#85592,#85593,#85594,
#85595,#85596,#85597,#85598,#85599,#85600,#85601,#85602,#85603,#85604,#85605,
#85606,#85607,#85608,#85609,#85610,#85611,#85612,#85613,#85614,#85615,#85616,
#85617,#85618,#85619,#85620,#85621,#85622,#85623,#85624,#85625,#85626,#85627,
#85628,#85629,#85630,#85631,#85632,#85633,#85634,#85635,#85636,#85637,#85638,
#85639,#85640,#85641,#85642,#85643,#85644,#85645,#85646,#85647,#85648,#85649,
#85650,#85651,#85652,#85653,#85654,#85655,#85656,#85657,#85658,#85659,#85660,
#85661,#85662,#85663,#85664,#85665,#85666,#85667,#85668,#85669,#85670,#85671,
#85672,#85673,#85674,#85675,#85676,#85677,#85678,#85679,#85680,#85681,#85682,
#85683,#85684,#85685,#85686,#85687,#85688,#85689,#85690,#85691,#85692,#85693,
#85694,#85695,#85696,#85697,#85698,#85699,#85700,#85701,#85702,#85703,#85704,
#85705,#85706,#85707,#85708,#85709,#85710,#85711,#85712,#85713,#85714,#85715,
#85716,#85717,#85718,#85719,#85720,#85721,#85722,#85723,#85724,#85725,#85726,
#85727,#85728,#85729,#85730,#85731,#85732,#85733,#85734,#85735,#85736,#85737,
#85738,#85739,#85740,#85741,#85742,#85743,#85744,#85745,#85746,#85747,#85748,
#85749,#85750,#85751,#85752,#85753),.UNSPECIFIED.,.F.,.F.,(4,3,3,3,3,3,
3,3,3,3,3,3,3,3,3,3,3,3,3,3,3,3,3,3,3,3,3,3,3,3,3,3,3,3,3,3,3,3,3,3,3,3,
3,3,3,3,3,3,3,3,3,3,3,3,3,3,3,3,3,3,3,3,3,3,3,3,3,3,3,3,3,3,3,3,3,3,3,3,
3,3,4),(0.,0.012505555813569,0.0249230581963485,0.0374326759220017,0.0497312868613704,
0.0620126665492352,0.0742948718990828,0.0869711539247056,0.0993397367790628,
0.112169868390318,0.125000000001574,0.137505555815144,0.149923058197916,
0.16243267592357,0.174731286862939,0.187012666550806,0.199294871900654,
0.211971153926278,0.224339736780635,0.237169868391891,0.250000000003148,
0.26250555581671,0.274923058199489,0.287432675925143,0.299731286864511,
0.312012666552378,0.324294871902227,0.336971153927851,0.349339736782208,
0.362169868393464,0.375000000004721,0.387505555818293,0.399923058201069,
0.412432675926722,0.42473128686609,0.437012666553957,0.449294871903807,
0.461971153929429,0.474339736783788,0.487169868395042,0.500000000006295,
0.512505555819864,0.52492305820266,0.537432675928311,0.549731286867678,
0.562012666555544,0.574294871905386,0.586971153931007,0.599339736785364,
0.612169868396617,0.625000000007869,0.63750555582144,0.64992305820421,0.662432675929864,
0.674731286869233,0.687012666557099,0.699294871906943,0.711971153932568,
0.724339736786926,0.737169868398184,0.750000000009443,0.762505555823011,
0.774923058205782,0.787432675931436,0.799731286870803,0.812012666558669,
0.824294871908519,0.836971153934144,0.849339736788504,0.862169868399761,
0.875000000011017,0.887510054669295,0.900295972101501,0.912631393721422,
0.924929982354673,0.93720989642673,0.949489203700992,0.961808005151189,
0.974159538537179,0.986588161028193,0.98979739412694),.UNSPECIFIED.) ;
#1704 = B_SPLINE_CURVE_WITH_KNOTS('',3,(#85754,#85755,#85756,#85757,#85758,
#85759,#85760,#85761,#85762,#85763,#85764,#85765,#85766,#85767,#85768,#85769,
#85770,#85771,#85772,#85773,#85774,#85775,#85776,#85777,#85778,#85779,#85780,
#85781,#85782,#85783,#85784,#85785,#85786,#85787,#85788,#85789,#85790,#85791,
#85792,#85793,#85794,#85795,#85796,#85797,#85798,#85799,#85800,#85801,#85802,
#85803,#85804,#85805,#85806,#85807,#85808,#85809,#85810,#85811,#85812,#85813,
#85814,#85815,#85816,#85817,#85818,#85819,#85820,#85821,#85822,#85823,#85824,
#85825,#85826,#85827,#85828,#85829,#85830,#85831,#85832,#85833,#85834,#85835,
#85836,#85837,#85838,#85839,#85840,#85841,#85842,#85843,#85844,#85845,#85846,
#85847,#85848,#85849,#85850,#85851,#85852,#85853,#85854,#85855,#85856,#85857,
#85858,#85859,#85860,#85861,#85862,#85863,#85864,#85865,#85866,#85867,#85868,
#85869,#85870,#85871,#85872,#85873,#85874,#85875,#85876,#85877,#85878,#85879,
#85880,#85881,#85882,#85883,#85884,#85885,#85886,#85887,#85888,#85889,#85890,
#85891,#85892,#85893,#85894,#85895,#85896,#85897,#85898,#85899,#85900),
 .UNSPECIFIED.,.F.,.F.,(4,2,2,2,2,2,2,2,2,2,2,2,2,2,2,2,2,2,2,2,2,2,2,2,
2,2,2,2,2,2,2,2,2,2,2,2,2,2,2,2,2,2,2,2,2,2,2,2,2,2,2,2,2,2,2,2,2,2,2,2,
2,2,2,2,2,2,2,2,2,2,2,2,1,4),(0.,0.0143071334539869,0.028474245317343,0.0425776897392449,
0.0566436916612223,0.0706981180304496,0.0848024667917353,0.0989449686784511,
0.113213785447835,0.126288471502626,0.140595604956613,0.154762716819969,
0.168866161241871,0.18293216316385,0.196986589533071,0.211090938294356,
0.225233440181069,0.239502256950454,0.252576943005252,0.266884076459241,
0.281051188322597,0.2951546327445,0.309220634666477,0.323275061035697,0.337379409796983,
0.351521911683701,0.365790728453086,0.378865414507879,0.393172547961876,
0.407339659825232,0.421443104247129,0.435509106169106,0.449563532538323,
0.463667881299609,0.477810383186328,0.492079199955711,0.505153886010505,
0.519461019464478,0.533628131327833,0.54773157574974,0.561797577671727,
0.575852004040961,0.589956352802245,0.604098854688955,0.618367671458334,
0.631442357513131,0.645749490967132,0.659916602830487,0.674020047252389,
0.688086049174363,0.702140475543579,0.716244824304864,0.730387326191586,
0.744656142960965,0.757730829015757,0.772037962469715,0.786205074333073,
0.800308518754975,0.814374520676947,0.828428947046167,0.842533295807452,
0.85667579769416,0.870944614463543,0.884019300518384,0.898516614138413,
0.912686930054781,0.92679168641128,0.9408571728242,0.955642331987805,0.969733244122183,
0.983861047480448,0.99808103302288,0.999998904734446,1.),.UNSPECIFIED.) ;
#1705 = B_SPLINE_CURVE_WITH_KNOTS('',3,(#85902,#85903,#85904,#85905,#85906,
#85907,#85908,#85909,#85910,#85911,#85912,#85913,#85914,#85915,#85916,#85917,
#85918,#85919,#85920,#85921,#85922,#85923,#85924,#85925,#85926,#85927,#85928,
#85929,#85930,#85931,#85932,#85933,#85934,#85935,#85936,#85937,#85938,#85939,
#85940,#85941,#85942,#85943,#85944,#85945,#85946,#85947,#85948,#85949,#85950,
#85951,#85952,#85953,#85954,#85955,#85956,#85957,#85958,#85959,#85960,#85961,
#85962,#85963,#85964,#85965,#85966,#85967,#85968,#85969,#85970,#85971,#85972,
#85973,#85974,#85975,#85976,#85977,#85978,#85979,#85980,#85981,#85982,#85983,
#85984,#85985,#85986,#85987,#85988,#85989,#85990,#85991,#85992,#85993,#85994,
#85995,#85996,#85997,#85998,#85999,#86000,#86001,#86002,#86003,#86004,#86005,
#86006,#86007,#86008,#86009,#86010,#86011,#86012,#86013,#86014,#86015,#86016,
#86017,#86018,#86019,#86020,#86021,#86022,#86023,#86024,#86025,#86026,#86027,
#86028,#86029,#86030,#86031,#86032,#86033,#86034,#86035,#86036,#86037,#86038,
#86039,#86040,#86041,#86042,#86043,#86044,#86045,#86046,#86047,#86048,#86049,
#86050,#86051,#86052,#86053,#86054,#86055,#86056,#86057,#86058,#86059,#86060,
#86061,#86062,#86063,#86064,#86065,#86066,#86067,#86068,#86069,#86070,#86071,
#86072,#86073,#86074,#86075,#86076,#86077,#86078,#86079,#86080,#86081,#86082,
#86083,#86084,#86085,#86086,#86087,#86088,#86089,#86090,#86091,#86092,#86093,
#86094,#86095,#86096,#86097,#86098,#86099,#86100,#86101,#86102,#86103,#86104,
#86105,#86106,#86107,#86108,#86109,#86110,#86111,#86112,#86113,#86114,#86115,
#86116,#86117,#86118,#86119,#86120,#86121,#86122,#86123,#86124,#86125,#86126,
#86127,#86128,#86129,#86130,#86131,#86132,#86133,#86134,#86135,#86136,#86137,
#86138,#86139,#86140,#86141,#86142),.UNSPECIFIED.,.F.,.F.,(4,3,3,3,3,3,
3,3,3,3,3,3,3,3,3,3,3,3,3,3,3,3,3,3,3,3,3,3,3,3,3,3,3,3,3,3,3,3,3,3,3,3,
3,3,3,3,3,3,3,3,3,3,3,3,3,3,3,3,3,3,3,3,3,3,3,3,3,3,3,3,3,3,3,3,3,3,3,3,
3,3,4),(0.,0.0126344879087828,0.0251800145560018,0.0378186062548132,0.0502440156905314,
0.0626520162199399,0.0750608509262703,0.087867825231326,0.100363927990737,
0.113326338068615,0.126288748146493,0.138923236055458,0.151468762702297,
0.164107354401133,0.176532763837236,0.188940764367353,0.201349599072213,
0.214156573377406,0.226652676136431,0.239615086214709,0.252577496292986,
0.265211984200475,0.2777575108485,0.290396102547373,0.302821511981297,0.315229512513409,
0.327638347215868,0.34044532152177,0.35294142428118,0.365903834360329,0.378866244439479,
0.391500732347696,0.404046258994235,0.416684850693202,0.429110260128054,
0.441518260657293,0.453927095363529,0.46673406966914,0.479230172428468,
0.49219258250722,0.505154992585972,0.5177894804948,0.530335007143577,0.542973598842188,
0.55539900827921,0.567807008809323,0.580215843512492,0.593022817817485,
0.605518920576294,0.618481330654379,0.631443740732464,0.644078228638788,
0.656623755284755,0.66926234698403,0.681687756419411,0.694095756948902,
0.706504591653536,0.719311565959891,0.731807668720805,0.744770078799881,
0.757732488878957,0.770366976786588,0.782912503436521,0.795551095135137,
0.807976504570989,0.820384505101515,0.832793339806436,0.84560031411119,
0.8580964168697,0.871058826947575,0.88402123702545,0.896661248545381,0.909182555765295,
0.921646976956805,0.934073048117458,0.946479128094685,0.959048489802928,
0.971489276870397,0.984122925899028,0.996756574927659,1.),.UNSPECIFIED.) ;
#1706 = PLANE('',#32777) ;
#1707 = PLANE('',#32832) ;
#1708 = PLANE('',#32846) ;
#1709 = PLANE('',#32847) ;
#1710 = PLANE('',#32861) ;
#1711 = PLANE('',#32862) ;
#1712 = PLANE('',#32875) ;
#1713 = PLANE('',#32877) ;
#1714 = PLANE('',#32881) ;
#1715 = PLANE('',#32882) ;
#1716 = PLANE('',#32931) ;
#1717 = PLANE('',#32941) ;
#1718 = PLANE('',#32956) ;
#1719 = PLANE('',#32959) ;
#1720 = PLANE('',#32964) ;
#1721 = PLANE('',#32965) ;
#1722 = PLANE('',#32969) ;
#1723 = PLANE('',#32973) ;
#1724 = PLANE('',#32975) ;
#1725 = PLANE('',#32977) ;
#1726 = PLANE('',#32980) ;
#1727 = PLANE('',#32982) ;
#1728 = PLANE('',#32985) ;
#1729 = PLANE('',#32987) ;
#1730 = PLANE('',#32990) ;
#1731 = PLANE('',#32992) ;
#1732 = PLANE('',#32994) ;
#1733 = PLANE('',#32997) ;
#1734 = PLANE('',#32999) ;
#1735 = PLANE('',#33000) ;
#1736 = PLANE('',#33003) ;
#1737 = PLANE('',#33012) ;
#1738 = PLANE('',#33013) ;
#1739 = PLANE('',#33019) ;
#1740 = PLANE('',#33021) ;
#1741 = PLANE('',#33023) ;
#1742 = PLANE('',#33025) ;
#1743 = PLANE('',#33027) ;
#1744 = PLANE('',#33029) ;
#1745 = PLANE('',#33031) ;
#1746 = PLANE('',#33033) ;
#1747 = PLANE('',#33035) ;
#1748 = PLANE('',#33037) ;
#1749 = PLANE('',#33039) ;
#1750 = PLANE('',#33041) ;
#1751 = PLANE('',#33043) ;
#1752 = PLANE('',#33090) ;
#1753 = PLANE('',#33096) ;
#1754 = PLANE('',#33097) ;
#1755 = PLANE('',#33098) ;
#1756 = PLANE('',#33099) ;
#1757 = PLANE('',#33100) ;
#1758 = PLANE('',#33101) ;
#1759 = PLANE('',#33102) ;
#1760 = PLANE('',#33152) ;
#1761 = PLANE('',#33174) ;
#1762 = PLANE('',#33175) ;
#1763 = PLANE('',#33176) ;
#1764 = PLANE('',#33177) ;
#1765 = PLANE('',#33178) ;
#1766 = PLANE('',#33179) ;
#1767 = PLANE('',#33180) ;
#1768 = PLANE('',#33181) ;
#1769 = PLANE('',#33182) ;
#1770 = PLANE('',#33183) ;
#1771 = PLANE('',#33184) ;
#1772 = PLANE('',#33188) ;
#1773 = PLANE('',#33189) ;
#1774 = PLANE('',#33190) ;
#1775 = PLANE('',#33191) ;
#1776 = PLANE('',#33192) ;
#1777 = PLANE('',#33193) ;
#1778 = PLANE('',#33194) ;
#1779 = PLANE('',#33320) ;
#1780 = PLANE('',#33330) ;
#1781 = PLANE('',#33340) ;
#1782 = PLANE('',#33353) ;
#1783 = PLANE('',#33360) ;
#1784 = PLANE('',#33373) ;
#1785 = PLANE('',#33375) ;
#1786 = PLANE('',#33385) ;
#1787 = PLANE('',#33386) ;
#1788 = PLANE('',#33387) ;
#1789 = PLANE('',#33388) ;
#1790 = PLANE('',#33389) ;
#1791 = PLANE('',#33390) ;
#1792 = PLANE('',#33392) ;
#1793 = PLANE('',#33393) ;
#1794 = PLANE('',#33394) ;
#1795 = PLANE('',#33395) ;
#1796 = PLANE('',#33399) ;
#1797 = PLANE('',#33413) ;
#1798 = PLANE('',#33416) ;
#1799 = PLANE('',#33419) ;
#1800 = PLANE('',#33433) ;
#1801 = PLANE('',#33436) ;
#1802 = PLANE('',#33439) ;
#1803 = PLANE('',#33440) ;
#1804 = PLANE('',#33441) ;
#1805 = PLANE('',#33442) ;
#1806 = PLANE('',#33443) ;
#1807 = PLANE('',#33444) ;
#1808 = PLANE('',#33445) ;
#1809 = PLANE('',#33446) ;
#1810 = PLANE('',#33447) ;
#1811 = PLANE('',#33448) ;
#1812 = PLANE('',#33449) ;
#1813 = PLANE('',#33450) ;
#1814 = PLANE('',#33451) ;
#1815 = PLANE('',#33452) ;
#1816 = PLANE('',#33453) ;
#1817 = PLANE('',#33468) ;
#1818 = PLANE('',#33478) ;
#1819 = PLANE('',#33480) ;
#1820 = PLANE('',#33515) ;
#1821 = PLANE('',#33517) ;
#1822 = PLANE('',#33518) ;
#1823 = PLANE('',#33519) ;
#1824 = PLANE('',#33520) ;
#1825 = PLANE('',#33521) ;
#1826 = PLANE('',#33522) ;
#1827 = PLANE('',#33523) ;
#1828 = PLANE('',#33524) ;
#1829 = PLANE('',#33525) ;
#1830 = PLANE('',#33526) ;
#1831 = PLANE('',#33527) ;
#1832 = PLANE('',#33528) ;
#1833 = PLANE('',#33529) ;
#1834 = PLANE('',#33531) ;
#1835 = PLANE('',#33532) ;
#1836 = PLANE('',#33533) ;
#1837 = PLANE('',#33534) ;
#1838 = PLANE('',#33535) ;
#1839 = PLANE('',#33537) ;
#1840 = PLANE('',#33543) ;
#1841 = PLANE('',#33553) ;
#1842 = PLANE('',#33554) ;
#1843 = PLANE('',#33555) ;
#1844 = PLANE('',#33556) ;
#1845 = PLANE('',#33557) ;
#1846 = PLANE('',#33564) ;
#1847 = PLANE('',#33587) ;
#1848 = PLANE('',#33588) ;
#1849 = PLANE('',#33590) ;
#1850 = PLANE('',#33592) ;
#1851 = PLANE('',#33594) ;
#1852 = PLANE('',#33595) ;
#1853 = PLANE('',#33596) ;
#1854 = PLANE('',#33597) ;
#1855 = PLANE('',#33598) ;
#1856 = PLANE('',#33599) ;
#1857 = PLANE('',#33602) ;
#1858 = PLANE('',#33603) ;
#1859 = PLANE('',#33606) ;
#1860 = PLANE('',#33607) ;
#1861 = PLANE('',#33608) ;
#1862 = PLANE('',#33609) ;
#1863 = PLANE('',#33610) ;
#1864 = PLANE('',#33611) ;
#1865 = PLANE('',#33612) ;
#1866 = PLANE('',#33613) ;
#1867 = PLANE('',#33623) ;
#1868 = PLANE('',#33626) ;
#1869 = PLANE('',#33631) ;
#1870 = PLANE('',#33636) ;
#1871 = PLANE('',#33637) ;
#1872 = PLANE('',#33638) ;
#1873 = PLANE('',#33639) ;
#1874 = PLANE('',#33664) ;
#1875 = PLANE('',#33667) ;
#1876 = PLANE('',#33671) ;
#1877 = PLANE('',#33678) ;
#1878 = PLANE('',#33684) ;
#1879 = PLANE('',#33692) ;
#1880 = PLANE('',#33693) ;
#1881 = PLANE('',#33694) ;
#1882 = PLANE('',#33695) ;
#1883 = PLANE('',#33696) ;
#1884 = PLANE('',#33697) ;
#1885 = PLANE('',#33698) ;
#1886 = PLANE('',#33699) ;
#1887 = PLANE('',#33700) ;
#1888 = PLANE('',#33701) ;
#1889 = PLANE('',#33702) ;
#1890 = PLANE('',#33703) ;
#1891 = PLANE('',#33704) ;
#1892 = PLANE('',#33705) ;
#1893 = PLANE('',#33706) ;
#1894 = PLANE('',#33707) ;
#1895 = PLANE('',#33708) ;
#1896 = PLANE('',#33709) ;
#1897 = PLANE('',#33710) ;
#1898 = PLANE('',#33711) ;
#1899 = PLANE('',#33719) ;
#1900 = PLANE('',#33720) ;
#1901 = PLANE('',#33721) ;
#1902 = PLANE('',#33722) ;
#1903 = PLANE('',#33723) ;
#1904 = PLANE('',#33724) ;
#1905 = PLANE('',#33725) ;
#1906 = PLANE('',#33726) ;
#1907 = PLANE('',#33727) ;
#1908 = PLANE('',#33728) ;
#1909 = PLANE('',#33729) ;
#1910 = PLANE('',#33730) ;
#1911 = PLANE('',#33731) ;
#1912 = PLANE('',#33732) ;
#1913 = PLANE('',#33733) ;
#1914 = PLANE('',#33734) ;
#1915 = PLANE('',#33735) ;
#1916 = PLANE('',#33736) ;
#1917 = PLANE('',#33737) ;
#1918 = PLANE('',#33738) ;
#1919 = PLANE('',#33739) ;
#1920 = PLANE('',#33740) ;
#1921 = PLANE('',#33741) ;
#1922 = PLANE('',#33742) ;
#1923 = PLANE('',#33743) ;
#1924 = PLANE('',#33744) ;
#1925 = PLANE('',#33745) ;
#1926 = PLANE('',#33746) ;
#1927 = PLANE('',#33747) ;
#1928 = PLANE('',#33748) ;
#1929 = PLANE('',#33749) ;
#1930 = PLANE('',#33750) ;
#1931 = PLANE('',#33751) ;
#1932 = PLANE('',#33752) ;
#1933 = PLANE('',#33753) ;
#1934 = PLANE('',#33754) ;
#1935 = PLANE('',#33755) ;
#1936 = PLANE('',#33762) ;
#1937 = PLANE('',#33773) ;
#1938 = PLANE('',#33784) ;
#1939 = PLANE('',#33795) ;
#1940 = PLANE('',#33806) ;
#1941 = PLANE('',#33817) ;
#1942 = PLANE('',#33828) ;
#1943 = PLANE('',#33839) ;
#1944 = PLANE('',#33848) ;
#1945 = PLANE('',#33855) ;
#1946 = PLANE('',#33857) ;
#1947 = PLANE('',#33859) ;
#1948 = PLANE('',#33861) ;
#1949 = PLANE('',#33863) ;
#1950 = PLANE('',#33865) ;
#1951 = PLANE('',#33867) ;
#1952 = PLANE('',#33869) ;
#1953 = PLANE('',#33893) ;
#1954 = PLANE('',#33898) ;
#1955 = PLANE('',#33921) ;
#1956 = PLANE('',#33926) ;
#1957 = PLANE('',#33949) ;
#1958 = PLANE('',#33954) ;
#1959 = PLANE('',#33977) ;
#1960 = PLANE('',#33982) ;
#1961 = PLANE('',#34005) ;
#1962 = PLANE('',#34010) ;
#1963 = PLANE('',#34033) ;
#1964 = PLANE('',#34038) ;
#1965 = PLANE('',#34061) ;
#1966 = PLANE('',#34066) ;
#1967 = PLANE('',#34089) ;
#1968 = PLANE('',#34094) ;
#1969 = PLANE('',#34117) ;
#1970 = PLANE('',#34122) ;
#1971 = PLANE('',#34149) ;
#1972 = PLANE('',#34152) ;
#1973 = PLANE('',#34179) ;
#1974 = PLANE('',#34182) ;
#1975 = PLANE('',#34209) ;
#1976 = PLANE('',#34212) ;
#1977 = PLANE('',#34239) ;
#1978 = PLANE('',#34242) ;
#1979 = PLANE('',#34269) ;
#1980 = PLANE('',#34272) ;
#1981 = PLANE('',#34299) ;
#1982 = PLANE('',#34302) ;
#1983 = PLANE('',#34329) ;
#1984 = PLANE('',#34332) ;
#1985 = PLANE('',#34359) ;
#1986 = PLANE('',#34362) ;
#1987 = PLANE('',#34389) ;
#1988 = PLANE('',#34394) ;
#1989 = PLANE('',#34421) ;
#1990 = PLANE('',#34426) ;
#1991 = PLANE('',#34453) ;
#1992 = PLANE('',#34458) ;
#1993 = PLANE('',#34485) ;
#1994 = PLANE('',#34490) ;
#1995 = PLANE('',#34517) ;
#1996 = PLANE('',#34522) ;
#1997 = PLANE('',#34549) ;
#1998 = PLANE('',#34554) ;
#1999 = PLANE('',#34581) ;
#2000 = PLANE('',#34586) ;
#2001 = PLANE('',#34613) ;
#2002 = PLANE('',#34618) ;
#2003 = PLANE('',#34645) ;
#2004 = PLANE('',#34648) ;
#2005 = PLANE('',#34649) ;
#2006 = PLANE('',#34677) ;
#2007 = PLANE('',#34682) ;
#2008 = PLANE('',#34683) ;
#2009 = PLANE('',#34688) ;
#2010 = PLANE('',#34693) ;
#2011 = PLANE('',#34694) ;
#2012 = PLANE('',#34732) ;
#2013 = PLANE('',#34733) ;
#2014 = PLANE('',#34734) ;
#2015 = PLANE('',#34735) ;
#2016 = PLANE('',#34790) ;
#2017 = PLANE('',#34791) ;
#2018 = PLANE('',#34792) ;
#2019 = PLANE('',#34793) ;
#2020 = PLANE('',#34850) ;
#2021 = PLANE('',#34851) ;
#2022 = PLANE('',#34852) ;
#2023 = PLANE('',#34853) ;
#2024 = PLANE('',#34910) ;
#2025 = PLANE('',#34911) ;
#2026 = PLANE('',#34912) ;
#2027 = PLANE('',#34913) ;
#2028 = PLANE('',#34970) ;
#2029 = PLANE('',#34971) ;
#2030 = PLANE('',#34972) ;
#2031 = PLANE('',#34973) ;
#2032 = PLANE('',#35030) ;
#2033 = PLANE('',#35031) ;
#2034 = PLANE('',#35032) ;
#2035 = PLANE('',#35033) ;
#2036 = PLANE('',#35090) ;
#2037 = PLANE('',#35091) ;
#2038 = PLANE('',#35092) ;
#2039 = PLANE('',#35093) ;
#2040 = PLANE('',#35150) ;
#2041 = PLANE('',#35151) ;
#2042 = PLANE('',#35152) ;
#2043 = PLANE('',#35153) ;
#2044 = PLANE('',#35210) ;
#2045 = PLANE('',#35211) ;
#2046 = PLANE('',#35212) ;
#2047 = PLANE('',#35213) ;
#2048 = PLANE('',#35232) ;
#2049 = PLANE('',#35233) ;
#2050 = PLANE('',#35234) ;
#2051 = PLANE('',#35235) ;
#2052 = PLANE('',#35236) ;
#2053 = PLANE('',#35237) ;
#2054 = PLANE('',#35238) ;
#2055 = PLANE('',#35239) ;
#2056 = PLANE('',#35240) ;
#2057 = PLANE('',#35241) ;
#2058 = PLANE('',#35242) ;
#2059 = PLANE('',#35243) ;
#2060 = PLANE('',#35244) ;
#2061 = PLANE('',#35245) ;
#2062 = PLANE('',#35246) ;
#2063 = PLANE('',#35247) ;
#2064 = PLANE('',#35248) ;
#2065 = PLANE('',#35249) ;
#2066 = PLANE('',#35250) ;
#2067 = PLANE('',#35251) ;
#2068 = PLANE('',#35252) ;
#2069 = PLANE('',#35253) ;
#2070 = PLANE('',#35254) ;
#2071 = PLANE('',#35255) ;
#2072 = PLANE('',#35256) ;
#2073 = PLANE('',#35257) ;
#2074 = PLANE('',#35258) ;
#2075 = PLANE('',#35259) ;
#2076 = PLANE('',#35263) ;
#2077 = PLANE('',#35288) ;
#2078 = PLANE('',#35292) ;
#2079 = PLANE('',#35293) ;
#2080 = PLANE('',#35294) ;
#2081 = PLANE('',#35295) ;
#2082 = PLANE('',#35296) ;
#2083 = PLANE('',#35297) ;
#2084 = PLANE('',#35298) ;
#2085 = PLANE('',#35299) ;
#2086 = PLANE('',#35300) ;
#2087 = PLANE('',#35301) ;
#2088 = PLANE('',#35302) ;
#2089 = PLANE('',#35303) ;
#2090 = PLANE('',#35304) ;
#2091 = PLANE('',#35305) ;
#2092 = PLANE('',#35306) ;
#2093 = PLANE('',#35307) ;
#2094 = PLANE('',#35308) ;
#2095 = PLANE('',#35309) ;
#2096 = PLANE('',#35310) ;
#2097 = PLANE('',#35311) ;
#2098 = PLANE('',#35312) ;
#2099 = PLANE('',#35313) ;
#2100 = PLANE('',#35314) ;
#2101 = PLANE('',#35315) ;
#2102 = PLANE('',#35316) ;
#2103 = PLANE('',#35317) ;
#2104 = PLANE('',#35318) ;
#2105 = PLANE('',#35319) ;
#2106 = PLANE('',#35320) ;
#2107 = PLANE('',#35321) ;
#2108 = PLANE('',#35322) ;
#2109 = PLANE('',#35323) ;
#2110 = PLANE('',#35324) ;
#2111 = PLANE('',#35325) ;
#2112 = PLANE('',#35326) ;
#2113 = PLANE('',#35327) ;
#2114 = PLANE('',#35328) ;
#2115 = PLANE('',#35338) ;
#2116 = PLANE('',#35340) ;
#2117 = PLANE('',#35350) ;
#2118 = PLANE('',#35352) ;
#2119 = PLANE('',#35362) ;
#2120 = PLANE('',#35364) ;
#2121 = PLANE('',#35374) ;
#2122 = PLANE('',#35376) ;
#2123 = PLANE('',#35386) ;
#2124 = PLANE('',#35388) ;
#2125 = PLANE('',#35398) ;
#2126 = PLANE('',#35400) ;
#2127 = PLANE('',#35410) ;
#2128 = PLANE('',#35412) ;
#2129 = PLANE('',#35422) ;
#2130 = PLANE('',#35432) ;
#2131 = PLANE('',#35433) ;
#2132 = PLANE('',#35435) ;
#2133 = PLANE('',#35437) ;
#2134 = PLANE('',#35440) ;
#2135 = PLANE('',#35442) ;
#2136 = PLANE('',#35445) ;
#2137 = PLANE('',#35447) ;
#2138 = PLANE('',#35450) ;
#2139 = PLANE('',#35452) ;
#2140 = PLANE('',#35455) ;
#2141 = PLANE('',#35457) ;
#2142 = PLANE('',#35460) ;
#2143 = PLANE('',#35462) ;
#2144 = PLANE('',#35465) ;
#2145 = PLANE('',#35467) ;
#2146 = PLANE('',#35470) ;
#2147 = PLANE('',#35472) ;
#2148 = PLANE('',#35531) ;
#2149 = PLANE('',#35555) ;
#2150 = PLANE('',#35569) ;
#2151 = PLANE('',#35591) ;
#2152 = PLANE('',#35600) ;
#2153 = PLANE('',#35634) ;
#2154 = PLANE('',#35643) ;
#2155 = PLANE('',#35655) ;
#2156 = PLANE('',#35665) ;
#2157 = PLANE('',#35680) ;
#2158 = PLANE('',#35696) ;
#2159 = PLANE('',#35699) ;
#2160 = PLANE('',#35717) ;
#2161 = PLANE('',#35745) ;
#2162 = PLANE('',#35748) ;
#2163 = PLANE('',#35775) ;
#2164 = PLANE('',#35791) ;
#2165 = PLANE('',#35794) ;
#2166 = PLANE('',#35814) ;
#2167 = PLANE('',#35822) ;
#2168 = PLANE('',#35843) ;
#2169 = PLANE('',#35844) ;
#2170 = PLANE('',#35864) ;
#2171 = PLANE('',#35867) ;
#2172 = PLANE('',#35901) ;
#2173 = PLANE('',#35985) ;
#2174 = PLANE('',#35988) ;
#2175 = PLANE('',#35991) ;
#2176 = PLANE('',#35992) ;
#2177 = PLANE('',#35993) ;
#2178 = PLANE('',#35994) ;
#2179 = PLANE('',#36000) ;
#2180 = PLANE('',#36003) ;
#2181 = PLANE('',#36004) ;
#2182 = PLANE('',#36005) ;
#2183 = PLANE('',#36006) ;
#2184 = PLANE('',#36009) ;
#2185 = PLANE('',#36018) ;
#2186 = PLANE('',#36022) ;
#2187 = PLANE('',#36025) ;
#2188 = PLANE('',#36031) ;
#2189 = PLANE('',#36126) ;
#2190 = PLANE('',#36133) ;
#2191 = PLANE('',#36158) ;
#2192 = PLANE('',#36163) ;
#2193 = PLANE('',#36165) ;
#2194 = PLANE('',#36167) ;
#2195 = PLANE('',#36169) ;
#2196 = PLANE('',#36195) ;
#2197 = PLANE('',#36196) ;
#2198 = PLANE('',#36206) ;
#2199 = PLANE('',#36207) ;
#2200 = PLANE('',#36216) ;
#2201 = PLANE('',#36217) ;
#2202 = PLANE('',#36227) ;
#2203 = PLANE('',#36228) ;
#2204 = PLANE('',#36247) ;
#2205 = PLANE('',#36249) ;
#2206 = PLANE('',#36250) ;
#2207 = PLANE('',#36261) ;
#2208 = PLANE('',#36263) ;
#2209 = PLANE('',#36264) ;
#2210 = PLANE('',#36275) ;
#2211 = PLANE('',#36277) ;
#2212 = PLANE('',#36278) ;
#2213 = PLANE('',#36289) ;
#2214 = PLANE('',#36291) ;
#2215 = PLANE('',#36292) ;
#2216 = PLANE('',#36303) ;
#2217 = PLANE('',#36304) ;
#2218 = PLANE('',#36305) ;
#2219 = PLANE('',#36306) ;
#2220 = PLANE('',#36307) ;
#2221 = PLANE('',#36314) ;
#2222 = PLANE('',#36315) ;
#2223 = PLANE('',#36317) ;
#2224 = PLANE('',#36318) ;
#2225 = PLANE('',#36321) ;
#2226 = PLANE('',#36322) ;
#2227 = PLANE('',#36324) ;
#2228 = PLANE('',#36325) ;
#2229 = PLANE('',#36344) ;
#2230 = PLANE('',#36345) ;
#2231 = PLANE('',#36346) ;
#2232 = PLANE('',#36347) ;
#2233 = PLANE('',#36348) ;
#2234 = PLANE('',#36349) ;
#2235 = PLANE('',#36350) ;
#2236 = PLANE('',#36351) ;
#2237 = PLANE('',#36352) ;
#2238 = PLANE('',#36353) ;
#2239 = PLANE('',#36354) ;
#2240 = PLANE('',#36355) ;
#2241 = PLANE('',#36356) ;
#2242 = PLANE('',#36362) ;
#2243 = PLANE('',#36368) ;
#2244 = PLANE('',#36369) ;
#2245 = PLANE('',#36370) ;
#2246 = PLANE('',#36371) ;
#2247 = PLANE('',#36459) ;
#2248 = PLANE('',#36460) ;
#2249 = PLANE('',#36463) ;
#2250 = PLANE('',#36464) ;
#2251 = PLANE('',#36465) ;
#2252 = PLANE('',#36466) ;
#2253 = PLANE('',#36467) ;
#2254 = PLANE('',#36469) ;
#2255 = PLANE('',#36470) ;
#2256 = PLANE('',#36471) ;
#2257 = PLANE('',#36472) ;
#2258 = PLANE('',#36473) ;
#2259 = PLANE('',#36474) ;
#2260 = PLANE('',#36475) ;
#2261 = PLANE('',#36476) ;
#2262 = PLANE('',#36478) ;
#2263 = PLANE('',#36479) ;
#2264 = PLANE('',#36480) ;
#2265 = PLANE('',#36481) ;
#2266 = PLANE('',#36483) ;
#2267 = PLANE('',#36484) ;
#2268 = PLANE('',#36495) ;
#2269 = PLANE('',#36500) ;
#2270 = FACE_OUTER_BOUND('',#4158,.T.) ;
#2271 = FACE_OUTER_BOUND('',#4159,.T.) ;
#2272 = FACE_OUTER_BOUND('',#4180,.T.) ;
#2273 = FACE_OUTER_BOUND('',#4181,.T.) ;
#2274 = FACE_OUTER_BOUND('',#4182,.T.) ;
#2275 = FACE_OUTER_BOUND('',#4185,.T.) ;
#2276 = FACE_OUTER_BOUND('',#4186,.T.) ;
#2277 = FACE_OUTER_BOUND('',#4187,.T.) ;
#2278 = FACE_OUTER_BOUND('',#4190,.T.) ;
#2279 = FACE_OUTER_BOUND('',#4191,.T.) ;
#2280 = FACE_OUTER_BOUND('',#4192,.T.) ;
#2281 = FACE_OUTER_BOUND('',#4195,.T.) ;
#2282 = FACE_OUTER_BOUND('',#4196,.T.) ;
#2283 = FACE_OUTER_BOUND('',#4197,.T.) ;
#2284 = FACE_OUTER_BOUND('',#4198,.T.) ;
#2285 = FACE_OUTER_BOUND('',#4199,.T.) ;
#2286 = FACE_OUTER_BOUND('',#4200,.T.) ;
#2287 = FACE_OUTER_BOUND('',#4201,.T.) ;
#2288 = FACE_OUTER_BOUND('',#4222,.T.) ;
#2289 = FACE_OUTER_BOUND('',#4225,.T.) ;
#2290 = FACE_OUTER_BOUND('',#4226,.T.) ;
#2291 = FACE_OUTER_BOUND('',#4227,.T.) ;
#2292 = FACE_OUTER_BOUND('',#4228,.T.) ;
#2293 = FACE_OUTER_BOUND('',#4229,.T.) ;
#2294 = FACE_OUTER_BOUND('',#4230,.T.) ;
#2295 = FACE_OUTER_BOUND('',#4231,.T.) ;
#2296 = FACE_OUTER_BOUND('',#4232,.T.) ;
#2297 = FACE_OUTER_BOUND('',#4233,.T.) ;
#2298 = FACE_OUTER_BOUND('',#4234,.T.) ;
#2299 = FACE_OUTER_BOUND('',#4235,.T.) ;
#2300 = FACE_OUTER_BOUND('',#4236,.T.) ;
#2301 = FACE_OUTER_BOUND('',#4237,.T.) ;
#2302 = FACE_OUTER_BOUND('',#4238,.T.) ;
#2303 = FACE_OUTER_BOUND('',#4239,.T.) ;
#2304 = FACE_OUTER_BOUND('',#4240,.T.) ;
#2305 = FACE_OUTER_BOUND('',#4241,.T.) ;
#2306 = FACE_OUTER_BOUND('',#4242,.T.) ;
#2307 = FACE_OUTER_BOUND('',#4243,.T.) ;
#2308 = FACE_OUTER_BOUND('',#4244,.T.) ;
#2309 = FACE_OUTER_BOUND('',#4245,.T.) ;
#2310 = FACE_OUTER_BOUND('',#4246,.T.) ;
#2311 = FACE_OUTER_BOUND('',#4247,.T.) ;
#2312 = FACE_OUTER_BOUND('',#4248,.T.) ;
#2313 = FACE_OUTER_BOUND('',#4249,.T.) ;
#2314 = FACE_OUTER_BOUND('',#4250,.T.) ;
#2315 = FACE_OUTER_BOUND('',#4251,.T.) ;
#2316 = FACE_OUTER_BOUND('',#4252,.T.) ;
#2317 = FACE_OUTER_BOUND('',#4253,.T.) ;
#2318 = FACE_OUTER_BOUND('',#4254,.T.) ;
#2319 = FACE_OUTER_BOUND('',#4255,.T.) ;
#2320 = FACE_OUTER_BOUND('',#4256,.T.) ;
#2321 = FACE_OUTER_BOUND('',#4257,.T.) ;
#2322 = FACE_OUTER_BOUND('',#4258,.T.) ;
#2323 = FACE_OUTER_BOUND('',#4259,.T.) ;
#2324 = FACE_OUTER_BOUND('',#4260,.T.) ;
#2325 = FACE_OUTER_BOUND('',#4261,.T.) ;
#2326 = FACE_OUTER_BOUND('',#4262,.T.) ;
#2327 = FACE_OUTER_BOUND('',#4263,.T.) ;
#2328 = FACE_OUTER_BOUND('',#4264,.T.) ;
#2329 = FACE_OUTER_BOUND('',#4265,.T.) ;
#2330 = FACE_OUTER_BOUND('',#4266,.T.) ;
#2331 = FACE_OUTER_BOUND('',#4267,.T.) ;
#2332 = FACE_OUTER_BOUND('',#4268,.T.) ;
#2333 = FACE_OUTER_BOUND('',#4269,.T.) ;
#2334 = FACE_OUTER_BOUND('',#4270,.T.) ;
#2335 = FACE_OUTER_BOUND('',#4271,.T.) ;
#2336 = FACE_OUTER_BOUND('',#4272,.T.) ;
#2337 = FACE_OUTER_BOUND('',#4273,.T.) ;
#2338 = FACE_OUTER_BOUND('',#4274,.T.) ;
#2339 = FACE_OUTER_BOUND('',#4275,.T.) ;
#2340 = FACE_OUTER_BOUND('',#4276,.T.) ;
#2341 = FACE_OUTER_BOUND('',#4277,.T.) ;
#2342 = FACE_OUTER_BOUND('',#4278,.T.) ;
#2343 = FACE_OUTER_BOUND('',#4279,.T.) ;
#2344 = FACE_OUTER_BOUND('',#4280,.T.) ;
#2345 = FACE_OUTER_BOUND('',#4281,.T.) ;
#2346 = FACE_OUTER_BOUND('',#4282,.T.) ;
#2347 = FACE_OUTER_BOUND('',#4283,.T.) ;
#2348 = FACE_OUTER_BOUND('',#4284,.T.) ;
#2349 = FACE_OUTER_BOUND('',#4285,.T.) ;
#2350 = FACE_OUTER_BOUND('',#4286,.T.) ;
#2351 = FACE_OUTER_BOUND('',#4287,.T.) ;
#2352 = FACE_OUTER_BOUND('',#4288,.T.) ;
#2353 = FACE_OUTER_BOUND('',#4289,.T.) ;
#2354 = FACE_OUTER_BOUND('',#4290,.T.) ;
#2355 = FACE_OUTER_BOUND('',#4291,.T.) ;
#2356 = FACE_OUTER_BOUND('',#4292,.T.) ;
#2357 = FACE_OUTER_BOUND('',#4293,.T.) ;
#2358 = FACE_OUTER_BOUND('',#4294,.T.) ;
#2359 = FACE_OUTER_BOUND('',#4295,.T.) ;
#2360 = FACE_OUTER_BOUND('',#4296,.T.) ;
#2361 = FACE_OUTER_BOUND('',#4297,.T.) ;
#2362 = FACE_OUTER_BOUND('',#4298,.T.) ;
#2363 = FACE_OUTER_BOUND('',#4299,.T.) ;
#2364 = FACE_OUTER_BOUND('',#4300,.T.) ;
#2365 = FACE_OUTER_BOUND('',#4301,.T.) ;
#2366 = FACE_OUTER_BOUND('',#4302,.T.) ;
#2367 = FACE_OUTER_BOUND('',#4303,.T.) ;
#2368 = FACE_OUTER_BOUND('',#4304,.T.) ;
#2369 = FACE_OUTER_BOUND('',#4305,.T.) ;
#2370 = FACE_OUTER_BOUND('',#4306,.T.) ;
#2371 = FACE_OUTER_BOUND('',#4307,.T.) ;
#2372 = FACE_OUTER_BOUND('',#4308,.T.) ;
#2373 = FACE_OUTER_BOUND('',#4309,.T.) ;
#2374 = FACE_OUTER_BOUND('',#4310,.T.) ;
#2375 = FACE_OUTER_BOUND('',#4311,.T.) ;
#2376 = FACE_OUTER_BOUND('',#4312,.T.) ;
#2377 = FACE_OUTER_BOUND('',#4313,.T.) ;
#2378 = FACE_OUTER_BOUND('',#4314,.T.) ;
#2379 = FACE_OUTER_BOUND('',#4315,.T.) ;
#2380 = FACE_OUTER_BOUND('',#4316,.T.) ;
#2381 = FACE_OUTER_BOUND('',#4317,.T.) ;
#2382 = FACE_OUTER_BOUND('',#4318,.T.) ;
#2383 = FACE_OUTER_BOUND('',#4319,.T.) ;
#2384 = FACE_OUTER_BOUND('',#4320,.T.) ;
#2385 = FACE_OUTER_BOUND('',#4321,.T.) ;
#2386 = FACE_OUTER_BOUND('',#4322,.T.) ;
#2387 = FACE_OUTER_BOUND('',#4323,.T.) ;
#2388 = FACE_OUTER_BOUND('',#4324,.T.) ;
#2389 = FACE_OUTER_BOUND('',#4325,.T.) ;
#2390 = FACE_OUTER_BOUND('',#4326,.T.) ;
#2391 = FACE_OUTER_BOUND('',#4327,.T.) ;
#2392 = FACE_OUTER_BOUND('',#4328,.T.) ;
#2393 = FACE_OUTER_BOUND('',#4329,.T.) ;
#2394 = FACE_OUTER_BOUND('',#4330,.T.) ;
#2395 = FACE_OUTER_BOUND('',#4331,.T.) ;
#2396 = FACE_OUTER_BOUND('',#4332,.T.) ;
#2397 = FACE_OUTER_BOUND('',#4333,.T.) ;
#2398 = FACE_OUTER_BOUND('',#4334,.T.) ;
#2399 = FACE_OUTER_BOUND('',#4335,.T.) ;
#2400 = FACE_OUTER_BOUND('',#4336,.T.) ;
#2401 = FACE_OUTER_BOUND('',#4337,.T.) ;
#2402 = FACE_OUTER_BOUND('',#4338,.T.) ;
#2403 = FACE_OUTER_BOUND('',#4339,.T.) ;
#2404 = FACE_OUTER_BOUND('',#4340,.T.) ;
#2405 = FACE_OUTER_BOUND('',#4341,.T.) ;
#2406 = FACE_OUTER_BOUND('',#4342,.T.) ;
#2407 = FACE_OUTER_BOUND('',#4343,.T.) ;
#2408 = FACE_OUTER_BOUND('',#4344,.T.) ;
#2409 = FACE_OUTER_BOUND('',#4345,.T.) ;
#2410 = FACE_OUTER_BOUND('',#4346,.T.) ;
#2411 = FACE_OUTER_BOUND('',#4347,.T.) ;
#2412 = FACE_OUTER_BOUND('',#4348,.T.) ;
#2413 = FACE_OUTER_BOUND('',#4349,.T.) ;
#2414 = FACE_OUTER_BOUND('',#4350,.T.) ;
#2415 = FACE_OUTER_BOUND('',#4351,.T.) ;
#2416 = FACE_OUTER_BOUND('',#4352,.T.) ;
#2417 = FACE_OUTER_BOUND('',#4353,.T.) ;
#2418 = FACE_OUTER_BOUND('',#4354,.T.) ;
#2419 = FACE_OUTER_BOUND('',#4355,.T.) ;
#2420 = FACE_OUTER_BOUND('',#4357,.T.) ;
#2421 = FACE_OUTER_BOUND('',#4358,.T.) ;
#2422 = FACE_OUTER_BOUND('',#4359,.T.) ;
#2423 = FACE_OUTER_BOUND('',#4360,.T.) ;
#2424 = FACE_OUTER_BOUND('',#4361,.T.) ;
#2425 = FACE_OUTER_BOUND('',#4362,.T.) ;
#2426 = FACE_OUTER_BOUND('',#4363,.T.) ;
#2427 = FACE_OUTER_BOUND('',#4365,.T.) ;
#2428 = FACE_OUTER_BOUND('',#4366,.T.) ;
#2429 = FACE_OUTER_BOUND('',#4367,.T.) ;
#2430 = FACE_OUTER_BOUND('',#4368,.T.) ;
#2431 = FACE_OUTER_BOUND('',#4369,.T.) ;
#2432 = FACE_OUTER_BOUND('',#4370,.T.) ;
#2433 = FACE_OUTER_BOUND('',#4371,.T.) ;
#2434 = FACE_OUTER_BOUND('',#4372,.T.) ;
#2435 = FACE_OUTER_BOUND('',#4373,.T.) ;
#2436 = FACE_OUTER_BOUND('',#4374,.T.) ;
#2437 = FACE_OUTER_BOUND('',#4375,.T.) ;
#2438 = FACE_OUTER_BOUND('',#4376,.T.) ;
#2439 = FACE_OUTER_BOUND('',#4377,.T.) ;
#2440 = FACE_OUTER_BOUND('',#4378,.T.) ;
#2441 = FACE_OUTER_BOUND('',#4379,.T.) ;
#2442 = FACE_OUTER_BOUND('',#4380,.T.) ;
#2443 = FACE_OUTER_BOUND('',#4381,.T.) ;
#2444 = FACE_OUTER_BOUND('',#4382,.T.) ;
#2445 = FACE_OUTER_BOUND('',#4383,.T.) ;
#2446 = FACE_OUTER_BOUND('',#4384,.T.) ;
#2447 = FACE_OUTER_BOUND('',#4385,.T.) ;
#2448 = FACE_OUTER_BOUND('',#4386,.T.) ;
#2449 = FACE_OUTER_BOUND('',#4387,.T.) ;
#2450 = FACE_OUTER_BOUND('',#4388,.T.) ;
#2451 = FACE_OUTER_BOUND('',#4389,.T.) ;
#2452 = FACE_OUTER_BOUND('',#4390,.T.) ;
#2453 = FACE_OUTER_BOUND('',#4392,.T.) ;
#2454 = FACE_OUTER_BOUND('',#4393,.T.) ;
#2455 = FACE_OUTER_BOUND('',#4394,.T.) ;
#2456 = FACE_OUTER_BOUND('',#4395,.T.) ;
#2457 = FACE_OUTER_BOUND('',#4396,.T.) ;
#2458 = FACE_OUTER_BOUND('',#4397,.T.) ;
#2459 = FACE_OUTER_BOUND('',#4398,.T.) ;
#2460 = FACE_OUTER_BOUND('',#4399,.T.) ;
#2461 = FACE_OUTER_BOUND('',#4400,.T.) ;
#2462 = FACE_OUTER_BOUND('',#4401,.T.) ;
#2463 = FACE_OUTER_BOUND('',#4402,.T.) ;
#2464 = FACE_OUTER_BOUND('',#4403,.T.) ;
#2465 = FACE_OUTER_BOUND('',#4404,.T.) ;
#2466 = FACE_OUTER_BOUND('',#4405,.T.) ;
#2467 = FACE_OUTER_BOUND('',#4406,.T.) ;
#2468 = FACE_OUTER_BOUND('',#4407,.T.) ;
#2469 = FACE_OUTER_BOUND('',#4408,.T.) ;
#2470 = FACE_OUTER_BOUND('',#4409,.T.) ;
#2471 = FACE_OUTER_BOUND('',#4410,.T.) ;
#2472 = FACE_OUTER_BOUND('',#4411,.T.) ;
#2473 = FACE_OUTER_BOUND('',#4412,.T.) ;
#2474 = FACE_OUTER_BOUND('',#4413,.T.) ;
#2475 = FACE_OUTER_BOUND('',#4414,.T.) ;
#2476 = FACE_OUTER_BOUND('',#4415,.T.) ;
#2477 = FACE_OUTER_BOUND('',#4416,.T.) ;
#2478 = FACE_OUTER_BOUND('',#4417,.T.) ;
#2479 = FACE_OUTER_BOUND('',#4418,.T.) ;
#2480 = FACE_OUTER_BOUND('',#4419,.T.) ;
#2481 = FACE_OUTER_BOUND('',#4420,.T.) ;
#2482 = FACE_OUTER_BOUND('',#4421,.T.) ;
#2483 = FACE_OUTER_BOUND('',#4422,.T.) ;
#2484 = FACE_OUTER_BOUND('',#4423,.T.) ;
#2485 = FACE_OUTER_BOUND('',#4424,.T.) ;
#2486 = FACE_OUTER_BOUND('',#4425,.T.) ;
#2487 = FACE_OUTER_BOUND('',#4426,.T.) ;
#2488 = FACE_OUTER_BOUND('',#4427,.T.) ;
#2489 = FACE_OUTER_BOUND('',#4428,.T.) ;
#2490 = FACE_OUTER_BOUND('',#4429,.T.) ;
#2491 = FACE_OUTER_BOUND('',#4430,.T.) ;
#2492 = FACE_OUTER_BOUND('',#4431,.T.) ;
#2493 = FACE_OUTER_BOUND('',#4432,.T.) ;
#2494 = FACE_OUTER_BOUND('',#4433,.T.) ;
#2495 = FACE_OUTER_BOUND('',#4434,.T.) ;
#2496 = FACE_OUTER_BOUND('',#4435,.T.) ;
#2497 = FACE_OUTER_BOUND('',#4436,.T.) ;
#2498 = FACE_OUTER_BOUND('',#4437,.T.) ;
#2499 = FACE_OUTER_BOUND('',#4438,.T.) ;
#2500 = FACE_OUTER_BOUND('',#4439,.T.) ;
#2501 = FACE_OUTER_BOUND('',#4440,.T.) ;
#2502 = FACE_OUTER_BOUND('',#4441,.T.) ;
#2503 = FACE_OUTER_BOUND('',#4442,.T.) ;
#2504 = FACE_OUTER_BOUND('',#4443,.T.) ;
#2505 = FACE_OUTER_BOUND('',#4444,.T.) ;
#2506 = FACE_OUTER_BOUND('',#4445,.T.) ;
#2507 = FACE_OUTER_BOUND('',#4446,.T.) ;
#2508 = FACE_OUTER_BOUND('',#4447,.T.) ;
#2509 = FACE_OUTER_BOUND('',#4448,.T.) ;
#2510 = FACE_OUTER_BOUND('',#4449,.T.) ;
#2511 = FACE_OUTER_BOUND('',#4450,.T.) ;
#2512 = FACE_OUTER_BOUND('',#4451,.T.) ;
#2513 = FACE_OUTER_BOUND('',#4452,.T.) ;
#2514 = FACE_OUTER_BOUND('',#4453,.T.) ;
#2515 = FACE_OUTER_BOUND('',#4454,.T.) ;
#2516 = FACE_OUTER_BOUND('',#4455,.T.) ;
#2517 = FACE_OUTER_BOUND('',#4456,.T.) ;
#2518 = FACE_OUTER_BOUND('',#4457,.T.) ;
#2519 = FACE_OUTER_BOUND('',#4458,.T.) ;
#2520 = FACE_OUTER_BOUND('',#4459,.T.) ;
#2521 = FACE_OUTER_BOUND('',#4460,.T.) ;
#2522 = FACE_OUTER_BOUND('',#4461,.T.) ;
#2523 = FACE_OUTER_BOUND('',#4462,.T.) ;
#2524 = FACE_OUTER_BOUND('',#4463,.T.) ;
#2525 = FACE_OUTER_BOUND('',#4464,.T.) ;
#2526 = FACE_OUTER_BOUND('',#4465,.T.) ;
#2527 = FACE_OUTER_BOUND('',#4466,.T.) ;
#2528 = FACE_OUTER_BOUND('',#4467,.T.) ;
#2529 = FACE_OUTER_BOUND('',#4468,.T.) ;
#2530 = FACE_OUTER_BOUND('',#4469,.T.) ;
#2531 = FACE_OUTER_BOUND('',#4470,.T.) ;
#2532 = FACE_OUTER_BOUND('',#4471,.T.) ;
#2533 = FACE_OUTER_BOUND('',#4472,.T.) ;
#2534 = FACE_OUTER_BOUND('',#4473,.T.) ;
#2535 = FACE_OUTER_BOUND('',#4474,.T.) ;
#2536 = FACE_OUTER_BOUND('',#4475,.T.) ;
#2537 = FACE_OUTER_BOUND('',#4476,.T.) ;
#2538 = FACE_OUTER_BOUND('',#4477,.T.) ;
#2539 = FACE_OUTER_BOUND('',#4478,.T.) ;
#2540 = FACE_OUTER_BOUND('',#4479,.T.) ;
#2541 = FACE_OUTER_BOUND('',#4480,.T.) ;
#2542 = FACE_OUTER_BOUND('',#4481,.T.) ;
#2543 = FACE_OUTER_BOUND('',#4482,.T.) ;
#2544 = FACE_OUTER_BOUND('',#4483,.T.) ;
#2545 = FACE_OUTER_BOUND('',#4484,.T.) ;
#2546 = FACE_OUTER_BOUND('',#4485,.T.) ;
#2547 = FACE_OUTER_BOUND('',#4486,.T.) ;
#2548 = FACE_OUTER_BOUND('',#4487,.T.) ;
#2549 = FACE_OUTER_BOUND('',#4488,.T.) ;
#2550 = FACE_OUTER_BOUND('',#4489,.T.) ;
#2551 = FACE_OUTER_BOUND('',#4490,.T.) ;
#2552 = FACE_OUTER_BOUND('',#4499,.T.) ;
#2553 = FACE_OUTER_BOUND('',#4500,.T.) ;
#2554 = FACE_OUTER_BOUND('',#4511,.T.) ;
#2555 = FACE_OUTER_BOUND('',#4520,.T.) ;
#2556 = FACE_OUTER_BOUND('',#4531,.T.) ;
#2557 = FACE_OUTER_BOUND('',#4532,.T.) ;
#2558 = FACE_OUTER_BOUND('',#4533,.T.) ;
#2559 = FACE_OUTER_BOUND('',#4534,.T.) ;
#2560 = FACE_OUTER_BOUND('',#4535,.T.) ;
#2561 = FACE_OUTER_BOUND('',#4536,.T.) ;
#2562 = FACE_OUTER_BOUND('',#4537,.T.) ;
#2563 = FACE_OUTER_BOUND('',#4538,.T.) ;
#2564 = FACE_OUTER_BOUND('',#4539,.T.) ;
#2565 = FACE_OUTER_BOUND('',#4540,.T.) ;
#2566 = FACE_OUTER_BOUND('',#4541,.T.) ;
#2567 = FACE_OUTER_BOUND('',#4542,.T.) ;
#2568 = FACE_OUTER_BOUND('',#4543,.T.) ;
#2569 = FACE_OUTER_BOUND('',#4544,.T.) ;
#2570 = FACE_OUTER_BOUND('',#4545,.T.) ;
#2571 = FACE_OUTER_BOUND('',#4546,.T.) ;
#2572 = FACE_OUTER_BOUND('',#4547,.T.) ;
#2573 = FACE_OUTER_BOUND('',#4548,.T.) ;
#2574 = FACE_OUTER_BOUND('',#4549,.T.) ;
#2575 = FACE_OUTER_BOUND('',#4550,.T.) ;
#2576 = FACE_OUTER_BOUND('',#4551,.T.) ;
#2577 = FACE_OUTER_BOUND('',#4552,.T.) ;
#2578 = FACE_OUTER_BOUND('',#4553,.T.) ;
#2579 = FACE_OUTER_BOUND('',#4554,.T.) ;
#2580 = FACE_OUTER_BOUND('',#4555,.T.) ;
#2581 = FACE_OUTER_BOUND('',#4556,.T.) ;
#2582 = FACE_OUTER_BOUND('',#4557,.T.) ;
#2583 = FACE_OUTER_BOUND('',#4558,.T.) ;
#2584 = FACE_OUTER_BOUND('',#4559,.T.) ;
#2585 = FACE_OUTER_BOUND('',#4560,.T.) ;
#2586 = FACE_OUTER_BOUND('',#4561,.T.) ;
#2587 = FACE_OUTER_BOUND('',#4562,.T.) ;
#2588 = FACE_OUTER_BOUND('',#4563,.T.) ;
#2589 = FACE_OUTER_BOUND('',#4564,.T.) ;
#2590 = FACE_OUTER_BOUND('',#4565,.T.) ;
#2591 = FACE_OUTER_BOUND('',#4566,.T.) ;
#2592 = FACE_OUTER_BOUND('',#4567,.T.) ;
#2593 = FACE_OUTER_BOUND('',#4568,.T.) ;
#2594 = FACE_OUTER_BOUND('',#4569,.T.) ;
#2595 = FACE_OUTER_BOUND('',#4570,.T.) ;
#2596 = FACE_OUTER_BOUND('',#4571,.T.) ;
#2597 = FACE_OUTER_BOUND('',#4572,.T.) ;
#2598 = FACE_OUTER_BOUND('',#4573,.T.) ;
#2599 = FACE_OUTER_BOUND('',#4574,.T.) ;
#2600 = FACE_OUTER_BOUND('',#4575,.T.) ;
#2601 = FACE_OUTER_BOUND('',#4576,.T.) ;
#2602 = FACE_OUTER_BOUND('',#4577,.T.) ;
#2603 = FACE_OUTER_BOUND('',#4578,.T.) ;
#2604 = FACE_OUTER_BOUND('',#4579,.T.) ;
#2605 = FACE_OUTER_BOUND('',#4580,.T.) ;
#2606 = FACE_OUTER_BOUND('',#4581,.T.) ;
#2607 = FACE_OUTER_BOUND('',#4582,.T.) ;
#2608 = FACE_OUTER_BOUND('',#4583,.T.) ;
#2609 = FACE_OUTER_BOUND('',#4584,.T.) ;
#2610 = FACE_OUTER_BOUND('',#4585,.T.) ;
#2611 = FACE_OUTER_BOUND('',#4586,.T.) ;
#2612 = FACE_OUTER_BOUND('',#4587,.T.) ;
#2613 = FACE_OUTER_BOUND('',#4588,.T.) ;
#2614 = FACE_OUTER_BOUND('',#4589,.T.) ;
#2615 = FACE_OUTER_BOUND('',#4590,.T.) ;
#2616 = FACE_OUTER_BOUND('',#4591,.T.) ;
#2617 = FACE_OUTER_BOUND('',#4592,.T.) ;
#2618 = FACE_OUTER_BOUND('',#4593,.T.) ;
#2619 = FACE_OUTER_BOUND('',#4594,.T.) ;
#2620 = FACE_OUTER_BOUND('',#4595,.T.) ;
#2621 = FACE_OUTER_BOUND('',#4596,.T.) ;
#2622 = FACE_OUTER_BOUND('',#4597,.T.) ;
#2623 = FACE_OUTER_BOUND('',#4598,.T.) ;
#2624 = FACE_OUTER_BOUND('',#4599,.T.) ;
#2625 = FACE_OUTER_BOUND('',#4600,.T.) ;
#2626 = FACE_OUTER_BOUND('',#4601,.T.) ;
#2627 = FACE_OUTER_BOUND('',#4602,.T.) ;
#2628 = FACE_OUTER_BOUND('',#4603,.T.) ;
#2629 = FACE_OUTER_BOUND('',#4604,.T.) ;
#2630 = FACE_OUTER_BOUND('',#4605,.T.) ;
#2631 = FACE_OUTER_BOUND('',#4606,.T.) ;
#2632 = FACE_OUTER_BOUND('',#4607,.T.) ;
#2633 = FACE_OUTER_BOUND('',#4608,.T.) ;
#2634 = FACE_OUTER_BOUND('',#4609,.T.) ;
#2635 = FACE_OUTER_BOUND('',#4610,.T.) ;
#2636 = FACE_OUTER_BOUND('',#4611,.T.) ;
#2637 = FACE_OUTER_BOUND('',#4612,.T.) ;
#2638 = FACE_OUTER_BOUND('',#4613,.T.) ;
#2639 = FACE_OUTER_BOUND('',#4614,.T.) ;
#2640 = FACE_OUTER_BOUND('',#4615,.T.) ;
#2641 = FACE_OUTER_BOUND('',#4616,.T.) ;
#2642 = FACE_OUTER_BOUND('',#4617,.T.) ;
#2643 = FACE_OUTER_BOUND('',#4618,.T.) ;
#2644 = FACE_OUTER_BOUND('',#4619,.T.) ;
#2645 = FACE_OUTER_BOUND('',#4620,.T.) ;
#2646 = FACE_OUTER_BOUND('',#4621,.T.) ;
#2647 = FACE_OUTER_BOUND('',#4622,.T.) ;
#2648 = FACE_OUTER_BOUND('',#4623,.T.) ;
#2649 = FACE_OUTER_BOUND('',#4624,.T.) ;
#2650 = FACE_OUTER_BOUND('',#4625,.T.) ;
#2651 = FACE_OUTER_BOUND('',#4626,.T.) ;
#2652 = FACE_OUTER_BOUND('',#4627,.T.) ;
#2653 = FACE_OUTER_BOUND('',#4628,.T.) ;
#2654 = FACE_OUTER_BOUND('',#4629,.T.) ;
#2655 = FACE_OUTER_BOUND('',#4630,.T.) ;
#2656 = FACE_OUTER_BOUND('',#4631,.T.) ;
#2657 = FACE_OUTER_BOUND('',#4632,.T.) ;
#2658 = FACE_OUTER_BOUND('',#4633,.T.) ;
#2659 = FACE_OUTER_BOUND('',#4634,.T.) ;
#2660 = FACE_OUTER_BOUND('',#4635,.T.) ;
#2661 = FACE_OUTER_BOUND('',#4636,.T.) ;
#2662 = FACE_OUTER_BOUND('',#4637,.T.) ;
#2663 = FACE_OUTER_BOUND('',#4638,.T.) ;
#2664 = FACE_OUTER_BOUND('',#4639,.T.) ;
#2665 = FACE_OUTER_BOUND('',#4640,.T.) ;
#2666 = FACE_OUTER_BOUND('',#4641,.T.) ;
#2667 = FACE_OUTER_BOUND('',#4642,.T.) ;
#2668 = FACE_OUTER_BOUND('',#4643,.T.) ;
#2669 = FACE_OUTER_BOUND('',#4648,.T.) ;
#2670 = FACE_OUTER_BOUND('',#4649,.T.) ;
#2671 = FACE_OUTER_BOUND('',#4650,.T.) ;
#2672 = FACE_OUTER_BOUND('',#4651,.T.) ;
#2673 = FACE_OUTER_BOUND('',#4652,.T.) ;
#2674 = FACE_OUTER_BOUND('',#4653,.T.) ;
#2675 = FACE_OUTER_BOUND('',#4654,.T.) ;
#2676 = FACE_OUTER_BOUND('',#4655,.T.) ;
#2677 = FACE_OUTER_BOUND('',#4656,.T.) ;
#2678 = FACE_OUTER_BOUND('',#4657,.T.) ;
#2679 = FACE_OUTER_BOUND('',#4658,.T.) ;
#2680 = FACE_OUTER_BOUND('',#4659,.T.) ;
#2681 = FACE_OUTER_BOUND('',#4660,.T.) ;
#2682 = FACE_OUTER_BOUND('',#4661,.T.) ;
#2683 = FACE_OUTER_BOUND('',#4662,.T.) ;
#2684 = FACE_OUTER_BOUND('',#4663,.T.) ;
#2685 = FACE_OUTER_BOUND('',#4664,.T.) ;
#2686 = FACE_OUTER_BOUND('',#4665,.T.) ;
#2687 = FACE_OUTER_BOUND('',#4666,.T.) ;
#2688 = FACE_OUTER_BOUND('',#4667,.T.) ;
#2689 = FACE_OUTER_BOUND('',#4668,.T.) ;
#2690 = FACE_OUTER_BOUND('',#4669,.T.) ;
#2691 = FACE_OUTER_BOUND('',#4670,.T.) ;
#2692 = FACE_OUTER_BOUND('',#4671,.T.) ;
#2693 = FACE_OUTER_BOUND('',#4672,.T.) ;
#2694 = FACE_OUTER_BOUND('',#4673,.T.) ;
#2695 = FACE_OUTER_BOUND('',#4674,.T.) ;
#2696 = FACE_OUTER_BOUND('',#4675,.T.) ;
#2697 = FACE_OUTER_BOUND('',#4676,.T.) ;
#2698 = FACE_OUTER_BOUND('',#4677,.T.) ;
#2699 = FACE_OUTER_BOUND('',#4678,.T.) ;
#2700 = FACE_OUTER_BOUND('',#4679,.T.) ;
#2701 = FACE_OUTER_BOUND('',#4680,.T.) ;
#2702 = FACE_OUTER_BOUND('',#4681,.T.) ;
#2703 = FACE_OUTER_BOUND('',#4682,.T.) ;
#2704 = FACE_OUTER_BOUND('',#4683,.T.) ;
#2705 = FACE_OUTER_BOUND('',#4684,.T.) ;
#2706 = FACE_OUTER_BOUND('',#4685,.T.) ;
#2707 = FACE_OUTER_BOUND('',#4686,.T.) ;
#2708 = FACE_OUTER_BOUND('',#4687,.T.) ;
#2709 = FACE_OUTER_BOUND('',#4688,.T.) ;
#2710 = FACE_OUTER_BOUND('',#4690,.T.) ;
#2711 = FACE_OUTER_BOUND('',#4691,.T.) ;
#2712 = FACE_OUTER_BOUND('',#4692,.T.) ;
#2713 = FACE_OUTER_BOUND('',#4693,.T.) ;
#2714 = FACE_OUTER_BOUND('',#4694,.T.) ;
#2715 = FACE_OUTER_BOUND('',#4695,.T.) ;
#2716 = FACE_OUTER_BOUND('',#4696,.T.) ;
#2717 = FACE_OUTER_BOUND('',#4697,.T.) ;
#2718 = FACE_OUTER_BOUND('',#4698,.T.) ;
#2719 = FACE_OUTER_BOUND('',#4699,.T.) ;
#2720 = FACE_OUTER_BOUND('',#4700,.T.) ;
#2721 = FACE_OUTER_BOUND('',#4701,.T.) ;
#2722 = FACE_OUTER_BOUND('',#4702,.T.) ;
#2723 = FACE_OUTER_BOUND('',#4703,.T.) ;
#2724 = FACE_OUTER_BOUND('',#4704,.T.) ;
#2725 = FACE_OUTER_BOUND('',#4705,.T.) ;
#2726 = FACE_OUTER_BOUND('',#4706,.T.) ;
#2727 = FACE_OUTER_BOUND('',#4707,.T.) ;
#2728 = FACE_OUTER_BOUND('',#4708,.T.) ;
#2729 = FACE_OUTER_BOUND('',#4709,.T.) ;
#2730 = FACE_OUTER_BOUND('',#4710,.T.) ;
#2731 = FACE_OUTER_BOUND('',#4711,.T.) ;
#2732 = FACE_OUTER_BOUND('',#4712,.T.) ;
#2733 = FACE_OUTER_BOUND('',#4713,.T.) ;
#2734 = FACE_OUTER_BOUND('',#4714,.T.) ;
#2735 = FACE_OUTER_BOUND('',#4715,.T.) ;
#2736 = FACE_OUTER_BOUND('',#4716,.T.) ;
#2737 = FACE_OUTER_BOUND('',#4717,.T.) ;
#2738 = FACE_OUTER_BOUND('',#4718,.T.) ;
#2739 = FACE_OUTER_BOUND('',#4719,.T.) ;
#2740 = FACE_OUTER_BOUND('',#4720,.T.) ;
#2741 = FACE_OUTER_BOUND('',#4721,.T.) ;
#2742 = FACE_OUTER_BOUND('',#4722,.T.) ;
#2743 = FACE_OUTER_BOUND('',#4723,.T.) ;
#2744 = FACE_OUTER_BOUND('',#4728,.T.) ;
#2745 = FACE_OUTER_BOUND('',#4729,.T.) ;
#2746 = FACE_OUTER_BOUND('',#4730,.T.) ;
#2747 = FACE_OUTER_BOUND('',#4731,.T.) ;
#2748 = FACE_OUTER_BOUND('',#4733,.T.) ;
#2749 = FACE_OUTER_BOUND('',#4734,.T.) ;
#2750 = FACE_OUTER_BOUND('',#4735,.T.) ;
#2751 = FACE_OUTER_BOUND('',#4736,.T.) ;
#2752 = FACE_OUTER_BOUND('',#4737,.T.) ;
#2753 = FACE_OUTER_BOUND('',#4738,.T.) ;
#2754 = FACE_OUTER_BOUND('',#4739,.T.) ;
#2755 = FACE_OUTER_BOUND('',#4740,.T.) ;
#2756 = FACE_OUTER_BOUND('',#4741,.T.) ;
#2757 = FACE_OUTER_BOUND('',#4742,.T.) ;
#2758 = FACE_OUTER_BOUND('',#4743,.T.) ;
#2759 = FACE_OUTER_BOUND('',#4753,.T.) ;
#2760 = FACE_OUTER_BOUND('',#4754,.T.) ;
#2761 = FACE_OUTER_BOUND('',#4755,.T.) ;
#2762 = FACE_OUTER_BOUND('',#4756,.T.) ;
#2763 = FACE_OUTER_BOUND('',#4757,.T.) ;
#2764 = FACE_OUTER_BOUND('',#4758,.T.) ;
#2765 = FACE_OUTER_BOUND('',#4759,.T.) ;
#2766 = FACE_OUTER_BOUND('',#4760,.T.) ;
#2767 = FACE_OUTER_BOUND('',#4761,.T.) ;
#2768 = FACE_OUTER_BOUND('',#4762,.T.) ;
#2769 = FACE_OUTER_BOUND('',#4763,.T.) ;
#2770 = FACE_OUTER_BOUND('',#4764,.T.) ;
#2771 = FACE_OUTER_BOUND('',#4765,.T.) ;
#2772 = FACE_OUTER_BOUND('',#4766,.T.) ;
#2773 = FACE_OUTER_BOUND('',#4767,.T.) ;
#2774 = FACE_OUTER_BOUND('',#4777,.T.) ;
#2775 = FACE_OUTER_BOUND('',#4778,.T.) ;
#2776 = FACE_OUTER_BOUND('',#4779,.T.) ;
#2777 = FACE_OUTER_BOUND('',#4780,.T.) ;
#2778 = FACE_OUTER_BOUND('',#4781,.T.) ;
#2779 = FACE_OUTER_BOUND('',#4782,.T.) ;
#2780 = FACE_OUTER_BOUND('',#4783,.T.) ;
#2781 = FACE_OUTER_BOUND('',#4784,.T.) ;
#2782 = FACE_OUTER_BOUND('',#4785,.T.) ;
#2783 = FACE_OUTER_BOUND('',#4786,.T.) ;
#2784 = FACE_OUTER_BOUND('',#4787,.T.) ;
#2785 = FACE_OUTER_BOUND('',#4788,.T.) ;
#2786 = FACE_OUTER_BOUND('',#4789,.T.) ;
#2787 = FACE_OUTER_BOUND('',#4790,.T.) ;
#2788 = FACE_OUTER_BOUND('',#4791,.T.) ;
#2789 = FACE_OUTER_BOUND('',#4792,.T.) ;
#2790 = FACE_OUTER_BOUND('',#4793,.T.) ;
#2791 = FACE_OUTER_BOUND('',#4794,.T.) ;
#2792 = FACE_OUTER_BOUND('',#4795,.T.) ;
#2793 = FACE_OUTER_BOUND('',#4796,.T.) ;
#2794 = FACE_OUTER_BOUND('',#4797,.T.) ;
#2795 = FACE_OUTER_BOUND('',#4798,.T.) ;
#2796 = FACE_OUTER_BOUND('',#4799,.T.) ;
#2797 = FACE_OUTER_BOUND('',#4800,.T.) ;
#2798 = FACE_OUTER_BOUND('',#4801,.T.) ;
#2799 = FACE_OUTER_BOUND('',#4802,.T.) ;
#2800 = FACE_OUTER_BOUND('',#4803,.T.) ;
#2801 = FACE_OUTER_BOUND('',#4804,.T.) ;
#2802 = FACE_OUTER_BOUND('',#4805,.T.) ;
#2803 = FACE_OUTER_BOUND('',#4806,.T.) ;
#2804 = FACE_OUTER_BOUND('',#4807,.T.) ;
#2805 = FACE_OUTER_BOUND('',#4808,.T.) ;
#2806 = FACE_OUTER_BOUND('',#4809,.T.) ;
#2807 = FACE_OUTER_BOUND('',#4810,.T.) ;
#2808 = FACE_OUTER_BOUND('',#4811,.T.) ;
#2809 = FACE_OUTER_BOUND('',#4812,.T.) ;
#2810 = FACE_OUTER_BOUND('',#4813,.T.) ;
#2811 = FACE_OUTER_BOUND('',#4814,.T.) ;
#2812 = FACE_OUTER_BOUND('',#4815,.T.) ;
#2813 = FACE_OUTER_BOUND('',#4816,.T.) ;
#2814 = FACE_OUTER_BOUND('',#4817,.T.) ;
#2815 = FACE_OUTER_BOUND('',#4818,.T.) ;
#2816 = FACE_OUTER_BOUND('',#4819,.T.) ;
#2817 = FACE_OUTER_BOUND('',#4820,.T.) ;
#2818 = FACE_OUTER_BOUND('',#4821,.T.) ;
#2819 = FACE_OUTER_BOUND('',#4822,.T.) ;
#2820 = FACE_OUTER_BOUND('',#4825,.T.) ;
#2821 = FACE_OUTER_BOUND('',#4826,.T.) ;
#2822 = FACE_OUTER_BOUND('',#4827,.T.) ;
#2823 = FACE_OUTER_BOUND('',#4830,.T.) ;
#2824 = FACE_OUTER_BOUND('',#4831,.T.) ;
#2825 = FACE_OUTER_BOUND('',#4832,.T.) ;
#2826 = FACE_OUTER_BOUND('',#4835,.T.) ;
#2827 = FACE_OUTER_BOUND('',#4836,.T.) ;
#2828 = FACE_OUTER_BOUND('',#4837,.T.) ;
#2829 = FACE_OUTER_BOUND('',#4840,.T.) ;
#2830 = FACE_OUTER_BOUND('',#4841,.T.) ;
#2831 = FACE_OUTER_BOUND('',#4842,.T.) ;
#2832 = FACE_OUTER_BOUND('',#4845,.T.) ;
#2833 = FACE_OUTER_BOUND('',#4846,.T.) ;
#2834 = FACE_OUTER_BOUND('',#4847,.T.) ;
#2835 = FACE_OUTER_BOUND('',#4850,.T.) ;
#2836 = FACE_OUTER_BOUND('',#4851,.T.) ;
#2837 = FACE_OUTER_BOUND('',#4852,.T.) ;
#2838 = FACE_OUTER_BOUND('',#4855,.T.) ;
#2839 = FACE_OUTER_BOUND('',#4856,.T.) ;
#2840 = FACE_OUTER_BOUND('',#4857,.T.) ;
#2841 = FACE_OUTER_BOUND('',#4860,.T.) ;
#2842 = FACE_OUTER_BOUND('',#4861,.T.) ;
#2843 = FACE_OUTER_BOUND('',#4864,.T.) ;
#2844 = FACE_OUTER_BOUND('',#4865,.T.) ;
#2845 = FACE_OUTER_BOUND('',#4867,.T.) ;
#2846 = FACE_OUTER_BOUND('',#4869,.T.) ;
#2847 = FACE_OUTER_BOUND('',#4871,.T.) ;
#2848 = FACE_OUTER_BOUND('',#4873,.T.) ;
#2849 = FACE_OUTER_BOUND('',#4875,.T.) ;
#2850 = FACE_OUTER_BOUND('',#4877,.T.) ;
#2851 = FACE_OUTER_BOUND('',#4879,.T.) ;
#2852 = FACE_OUTER_BOUND('',#4881,.T.) ;
#2853 = FACE_OUTER_BOUND('',#4882,.T.) ;
#2854 = FACE_OUTER_BOUND('',#4883,.T.) ;
#2855 = FACE_OUTER_BOUND('',#4884,.T.) ;
#2856 = FACE_OUTER_BOUND('',#4885,.T.) ;
#2857 = FACE_OUTER_BOUND('',#4886,.T.) ;
#2858 = FACE_OUTER_BOUND('',#4887,.T.) ;
#2859 = FACE_OUTER_BOUND('',#4888,.T.) ;
#2860 = FACE_OUTER_BOUND('',#4889,.T.) ;
#2861 = FACE_OUTER_BOUND('',#4890,.T.) ;
#2862 = FACE_OUTER_BOUND('',#4891,.T.) ;
#2863 = FACE_OUTER_BOUND('',#4892,.T.) ;
#2864 = FACE_OUTER_BOUND('',#4893,.T.) ;
#2865 = FACE_OUTER_BOUND('',#4894,.T.) ;
#2866 = FACE_OUTER_BOUND('',#4895,.T.) ;
#2867 = FACE_OUTER_BOUND('',#4896,.T.) ;
#2868 = FACE_OUTER_BOUND('',#4897,.T.) ;
#2869 = FACE_OUTER_BOUND('',#4898,.T.) ;
#2870 = FACE_OUTER_BOUND('',#4899,.T.) ;
#2871 = FACE_OUTER_BOUND('',#4900,.T.) ;
#2872 = FACE_OUTER_BOUND('',#4901,.T.) ;
#2873 = FACE_OUTER_BOUND('',#4902,.T.) ;
#2874 = FACE_OUTER_BOUND('',#4903,.T.) ;
#2875 = FACE_OUTER_BOUND('',#4904,.T.) ;
#2876 = FACE_OUTER_BOUND('',#4905,.T.) ;
#2877 = FACE_OUTER_BOUND('',#4906,.T.) ;
#2878 = FACE_OUTER_BOUND('',#4907,.T.) ;
#2879 = FACE_OUTER_BOUND('',#4908,.T.) ;
#2880 = FACE_OUTER_BOUND('',#4909,.T.) ;
#2881 = FACE_OUTER_BOUND('',#4910,.T.) ;
#2882 = FACE_OUTER_BOUND('',#4911,.T.) ;
#2883 = FACE_OUTER_BOUND('',#4912,.T.) ;
#2884 = FACE_OUTER_BOUND('',#4913,.T.) ;
#2885 = FACE_OUTER_BOUND('',#4914,.T.) ;
#2886 = FACE_OUTER_BOUND('',#4915,.T.) ;
#2887 = FACE_OUTER_BOUND('',#4916,.T.) ;
#2888 = FACE_OUTER_BOUND('',#4917,.T.) ;
#2889 = FACE_OUTER_BOUND('',#4918,.T.) ;
#2890 = FACE_OUTER_BOUND('',#4919,.T.) ;
#2891 = FACE_OUTER_BOUND('',#4920,.T.) ;
#2892 = FACE_OUTER_BOUND('',#4921,.T.) ;
#2893 = FACE_OUTER_BOUND('',#4922,.T.) ;
#2894 = FACE_OUTER_BOUND('',#4923,.T.) ;
#2895 = FACE_OUTER_BOUND('',#4924,.T.) ;
#2896 = FACE_OUTER_BOUND('',#4925,.T.) ;
#2897 = FACE_OUTER_BOUND('',#4926,.T.) ;
#2898 = FACE_OUTER_BOUND('',#4927,.T.) ;
#2899 = FACE_OUTER_BOUND('',#4928,.T.) ;
#2900 = FACE_OUTER_BOUND('',#4929,.T.) ;
#2901 = FACE_OUTER_BOUND('',#4930,.T.) ;
#2902 = FACE_OUTER_BOUND('',#4931,.T.) ;
#2903 = FACE_OUTER_BOUND('',#4932,.T.) ;
#2904 = FACE_OUTER_BOUND('',#4933,.T.) ;
#2905 = FACE_OUTER_BOUND('',#4934,.T.) ;
#2906 = FACE_OUTER_BOUND('',#4935,.T.) ;
#2907 = FACE_OUTER_BOUND('',#4936,.T.) ;
#2908 = FACE_OUTER_BOUND('',#4937,.T.) ;
#2909 = FACE_OUTER_BOUND('',#4938,.T.) ;
#2910 = FACE_OUTER_BOUND('',#4939,.T.) ;
#2911 = FACE_OUTER_BOUND('',#4940,.T.) ;
#2912 = FACE_OUTER_BOUND('',#4941,.T.) ;
#2913 = FACE_OUTER_BOUND('',#4942,.T.) ;
#2914 = FACE_OUTER_BOUND('',#4943,.T.) ;
#2915 = FACE_OUTER_BOUND('',#4944,.T.) ;
#2916 = FACE_OUTER_BOUND('',#4945,.T.) ;
#2917 = FACE_OUTER_BOUND('',#4946,.T.) ;
#2918 = FACE_OUTER_BOUND('',#4947,.T.) ;
#2919 = FACE_OUTER_BOUND('',#4948,.T.) ;
#2920 = FACE_OUTER_BOUND('',#4949,.T.) ;
#2921 = FACE_OUTER_BOUND('',#4950,.T.) ;
#2922 = FACE_OUTER_BOUND('',#4951,.T.) ;
#2923 = FACE_OUTER_BOUND('',#4952,.T.) ;
#2924 = FACE_OUTER_BOUND('',#4953,.T.) ;
#2925 = FACE_OUTER_BOUND('',#4954,.T.) ;
#2926 = FACE_OUTER_BOUND('',#4955,.T.) ;
#2927 = FACE_OUTER_BOUND('',#4956,.T.) ;
#2928 = FACE_OUTER_BOUND('',#4957,.T.) ;
#2929 = FACE_OUTER_BOUND('',#4958,.T.) ;
#2930 = FACE_OUTER_BOUND('',#4959,.T.) ;
#2931 = FACE_OUTER_BOUND('',#4960,.T.) ;
#2932 = FACE_OUTER_BOUND('',#4961,.T.) ;
#2933 = FACE_OUTER_BOUND('',#4962,.T.) ;
#2934 = FACE_OUTER_BOUND('',#4963,.T.) ;
#2935 = FACE_OUTER_BOUND('',#4964,.T.) ;
#2936 = FACE_OUTER_BOUND('',#4965,.T.) ;
#2937 = FACE_OUTER_BOUND('',#4966,.T.) ;
#2938 = FACE_OUTER_BOUND('',#4967,.T.) ;
#2939 = FACE_OUTER_BOUND('',#4968,.T.) ;
#2940 = FACE_OUTER_BOUND('',#4969,.T.) ;
#2941 = FACE_OUTER_BOUND('',#4970,.T.) ;
#2942 = FACE_OUTER_BOUND('',#4971,.T.) ;
#2943 = FACE_OUTER_BOUND('',#4972,.T.) ;
#2944 = FACE_OUTER_BOUND('',#4973,.T.) ;
#2945 = FACE_OUTER_BOUND('',#4974,.T.) ;
#2946 = FACE_OUTER_BOUND('',#4975,.T.) ;
#2947 = FACE_OUTER_BOUND('',#4976,.T.) ;
#2948 = FACE_OUTER_BOUND('',#4977,.T.) ;
#2949 = FACE_OUTER_BOUND('',#4978,.T.) ;
#2950 = FACE_OUTER_BOUND('',#4979,.T.) ;
#2951 = FACE_OUTER_BOUND('',#4980,.T.) ;
#2952 = FACE_OUTER_BOUND('',#4981,.T.) ;
#2953 = FACE_OUTER_BOUND('',#4982,.T.) ;
#2954 = FACE_OUTER_BOUND('',#4983,.T.) ;
#2955 = FACE_OUTER_BOUND('',#4984,.T.) ;
#2956 = FACE_OUTER_BOUND('',#4985,.T.) ;
#2957 = FACE_OUTER_BOUND('',#4986,.T.) ;
#2958 = FACE_OUTER_BOUND('',#4987,.T.) ;
#2959 = FACE_OUTER_BOUND('',#4988,.T.) ;
#2960 = FACE_OUTER_BOUND('',#4989,.T.) ;
#2961 = FACE_OUTER_BOUND('',#4990,.T.) ;
#2962 = FACE_OUTER_BOUND('',#4991,.T.) ;
#2963 = FACE_OUTER_BOUND('',#4992,.T.) ;
#2964 = FACE_OUTER_BOUND('',#4993,.T.) ;
#2965 = FACE_OUTER_BOUND('',#4994,.T.) ;
#2966 = FACE_OUTER_BOUND('',#4995,.T.) ;
#2967 = FACE_OUTER_BOUND('',#4996,.T.) ;
#2968 = FACE_OUTER_BOUND('',#4997,.T.) ;
#2969 = FACE_OUTER_BOUND('',#4998,.T.) ;
#2970 = FACE_OUTER_BOUND('',#4999,.T.) ;
#2971 = FACE_OUTER_BOUND('',#5000,.T.) ;
#2972 = FACE_OUTER_BOUND('',#5001,.T.) ;
#2973 = FACE_OUTER_BOUND('',#5002,.T.) ;
#2974 = FACE_OUTER_BOUND('',#5003,.T.) ;
#2975 = FACE_OUTER_BOUND('',#5004,.T.) ;
#2976 = FACE_OUTER_BOUND('',#5005,.T.) ;
#2977 = FACE_OUTER_BOUND('',#5006,.T.) ;
#2978 = FACE_OUTER_BOUND('',#5007,.T.) ;
#2979 = FACE_OUTER_BOUND('',#5008,.T.) ;
#2980 = FACE_OUTER_BOUND('',#5009,.T.) ;
#2981 = FACE_OUTER_BOUND('',#5010,.T.) ;
#2982 = FACE_OUTER_BOUND('',#5011,.T.) ;
#2983 = FACE_OUTER_BOUND('',#5012,.T.) ;
#2984 = FACE_OUTER_BOUND('',#5013,.T.) ;
#2985 = FACE_OUTER_BOUND('',#5014,.T.) ;
#2986 = FACE_OUTER_BOUND('',#5015,.T.) ;
#2987 = FACE_OUTER_BOUND('',#5016,.T.) ;
#2988 = FACE_OUTER_BOUND('',#5017,.T.) ;
#2989 = FACE_OUTER_BOUND('',#5018,.T.) ;
#2990 = FACE_OUTER_BOUND('',#5019,.T.) ;
#2991 = FACE_OUTER_BOUND('',#5020,.T.) ;
#2992 = FACE_OUTER_BOUND('',#5021,.T.) ;
#2993 = FACE_OUTER_BOUND('',#5022,.T.) ;
#2994 = FACE_OUTER_BOUND('',#5023,.T.) ;
#2995 = FACE_OUTER_BOUND('',#5024,.T.) ;
#2996 = FACE_OUTER_BOUND('',#5025,.T.) ;
#2997 = FACE_OUTER_BOUND('',#5026,.T.) ;
#2998 = FACE_OUTER_BOUND('',#5027,.T.) ;
#2999 = FACE_OUTER_BOUND('',#5028,.T.) ;
#3000 = FACE_OUTER_BOUND('',#5029,.T.) ;
#3001 = FACE_OUTER_BOUND('',#5030,.T.) ;
#3002 = FACE_OUTER_BOUND('',#5031,.T.) ;
#3003 = FACE_OUTER_BOUND('',#5032,.T.) ;
#3004 = FACE_OUTER_BOUND('',#5033,.T.) ;
#3005 = FACE_OUTER_BOUND('',#5034,.T.) ;
#3006 = FACE_OUTER_BOUND('',#5035,.T.) ;
#3007 = FACE_OUTER_BOUND('',#5036,.T.) ;
#3008 = FACE_OUTER_BOUND('',#5037,.T.) ;
#3009 = FACE_OUTER_BOUND('',#5038,.T.) ;
#3010 = FACE_OUTER_BOUND('',#5039,.T.) ;
#3011 = FACE_OUTER_BOUND('',#5040,.T.) ;
#3012 = FACE_OUTER_BOUND('',#5041,.T.) ;
#3013 = FACE_OUTER_BOUND('',#5042,.T.) ;
#3014 = FACE_OUTER_BOUND('',#5043,.T.) ;
#3015 = FACE_OUTER_BOUND('',#5044,.T.) ;
#3016 = FACE_OUTER_BOUND('',#5045,.T.) ;
#3017 = FACE_OUTER_BOUND('',#5046,.T.) ;
#3018 = FACE_OUTER_BOUND('',#5047,.T.) ;
#3019 = FACE_OUTER_BOUND('',#5048,.T.) ;
#3020 = FACE_OUTER_BOUND('',#5049,.T.) ;
#3021 = FACE_OUTER_BOUND('',#5050,.T.) ;
#3022 = FACE_OUTER_BOUND('',#5051,.T.) ;
#3023 = FACE_OUTER_BOUND('',#5052,.T.) ;
#3024 = FACE_OUTER_BOUND('',#5053,.T.) ;
#3025 = FACE_OUTER_BOUND('',#5054,.T.) ;
#3026 = FACE_OUTER_BOUND('',#5055,.T.) ;
#3027 = FACE_OUTER_BOUND('',#5056,.T.) ;
#3028 = FACE_OUTER_BOUND('',#5057,.T.) ;
#3029 = FACE_OUTER_BOUND('',#5058,.T.) ;
#3030 = FACE_OUTER_BOUND('',#5059,.T.) ;
#3031 = FACE_OUTER_BOUND('',#5060,.T.) ;
#3032 = FACE_OUTER_BOUND('',#5061,.T.) ;
#3033 = FACE_OUTER_BOUND('',#5062,.T.) ;
#3034 = FACE_OUTER_BOUND('',#5063,.T.) ;
#3035 = FACE_OUTER_BOUND('',#5064,.T.) ;
#3036 = FACE_OUTER_BOUND('',#5065,.T.) ;
#3037 = FACE_OUTER_BOUND('',#5066,.T.) ;
#3038 = FACE_OUTER_BOUND('',#5067,.T.) ;
#3039 = FACE_OUTER_BOUND('',#5068,.T.) ;
#3040 = FACE_OUTER_BOUND('',#5069,.T.) ;
#3041 = FACE_OUTER_BOUND('',#5070,.T.) ;
#3042 = FACE_OUTER_BOUND('',#5071,.T.) ;
#3043 = FACE_OUTER_BOUND('',#5072,.T.) ;
#3044 = FACE_OUTER_BOUND('',#5073,.T.) ;
#3045 = FACE_OUTER_BOUND('',#5074,.T.) ;
#3046 = FACE_OUTER_BOUND('',#5075,.T.) ;
#3047 = FACE_OUTER_BOUND('',#5076,.T.) ;
#3048 = FACE_OUTER_BOUND('',#5077,.T.) ;
#3049 = FACE_OUTER_BOUND('',#5078,.T.) ;
#3050 = FACE_OUTER_BOUND('',#5079,.T.) ;
#3051 = FACE_OUTER_BOUND('',#5080,.T.) ;
#3052 = FACE_OUTER_BOUND('',#5081,.T.) ;
#3053 = FACE_OUTER_BOUND('',#5082,.T.) ;
#3054 = FACE_OUTER_BOUND('',#5083,.T.) ;
#3055 = FACE_OUTER_BOUND('',#5084,.T.) ;
#3056 = FACE_OUTER_BOUND('',#5085,.T.) ;
#3057 = FACE_OUTER_BOUND('',#5086,.T.) ;
#3058 = FACE_OUTER_BOUND('',#5087,.T.) ;
#3059 = FACE_OUTER_BOUND('',#5088,.T.) ;
#3060 = FACE_OUTER_BOUND('',#5089,.T.) ;
#3061 = FACE_OUTER_BOUND('',#5090,.T.) ;
#3062 = FACE_OUTER_BOUND('',#5091,.T.) ;
#3063 = FACE_OUTER_BOUND('',#5092,.T.) ;
#3064 = FACE_OUTER_BOUND('',#5093,.T.) ;
#3065 = FACE_OUTER_BOUND('',#5094,.T.) ;
#3066 = FACE_OUTER_BOUND('',#5095,.T.) ;
#3067 = FACE_OUTER_BOUND('',#5096,.T.) ;
#3068 = FACE_OUTER_BOUND('',#5097,.T.) ;
#3069 = FACE_OUTER_BOUND('',#5098,.T.) ;
#3070 = FACE_OUTER_BOUND('',#5099,.T.) ;
#3071 = FACE_OUTER_BOUND('',#5100,.T.) ;
#3072 = FACE_OUTER_BOUND('',#5101,.T.) ;
#3073 = FACE_OUTER_BOUND('',#5102,.T.) ;
#3074 = FACE_OUTER_BOUND('',#5103,.T.) ;
#3075 = FACE_OUTER_BOUND('',#5104,.T.) ;
#3076 = FACE_OUTER_BOUND('',#5105,.T.) ;
#3077 = FACE_OUTER_BOUND('',#5106,.T.) ;
#3078 = FACE_OUTER_BOUND('',#5107,.T.) ;
#3079 = FACE_OUTER_BOUND('',#5108,.T.) ;
#3080 = FACE_OUTER_BOUND('',#5109,.T.) ;
#3081 = FACE_OUTER_BOUND('',#5110,.T.) ;
#3082 = FACE_OUTER_BOUND('',#5111,.T.) ;
#3083 = FACE_OUTER_BOUND('',#5112,.T.) ;
#3084 = FACE_OUTER_BOUND('',#5113,.T.) ;
#3085 = FACE_OUTER_BOUND('',#5114,.T.) ;
#3086 = FACE_OUTER_BOUND('',#5115,.T.) ;
#3087 = FACE_OUTER_BOUND('',#5116,.T.) ;
#3088 = FACE_OUTER_BOUND('',#5117,.T.) ;
#3089 = FACE_OUTER_BOUND('',#5118,.T.) ;
#3090 = FACE_OUTER_BOUND('',#5119,.T.) ;
#3091 = FACE_OUTER_BOUND('',#5120,.T.) ;
#3092 = FACE_OUTER_BOUND('',#5121,.T.) ;
#3093 = FACE_OUTER_BOUND('',#5122,.T.) ;
#3094 = FACE_OUTER_BOUND('',#5123,.T.) ;
#3095 = FACE_OUTER_BOUND('',#5124,.T.) ;
#3096 = FACE_OUTER_BOUND('',#5125,.T.) ;
#3097 = FACE_OUTER_BOUND('',#5126,.T.) ;
#3098 = FACE_OUTER_BOUND('',#5127,.T.) ;
#3099 = FACE_OUTER_BOUND('',#5128,.T.) ;
#3100 = FACE_OUTER_BOUND('',#5129,.T.) ;
#3101 = FACE_OUTER_BOUND('',#5130,.T.) ;
#3102 = FACE_OUTER_BOUND('',#5131,.T.) ;
#3103 = FACE_OUTER_BOUND('',#5132,.T.) ;
#3104 = FACE_OUTER_BOUND('',#5133,.T.) ;
#3105 = FACE_OUTER_BOUND('',#5134,.T.) ;
#3106 = FACE_OUTER_BOUND('',#5135,.T.) ;
#3107 = FACE_OUTER_BOUND('',#5136,.T.) ;
#3108 = FACE_OUTER_BOUND('',#5137,.T.) ;
#3109 = FACE_OUTER_BOUND('',#5138,.T.) ;
#3110 = FACE_OUTER_BOUND('',#5139,.T.) ;
#3111 = FACE_OUTER_BOUND('',#5140,.T.) ;
#3112 = FACE_OUTER_BOUND('',#5141,.T.) ;
#3113 = FACE_OUTER_BOUND('',#5142,.T.) ;
#3114 = FACE_OUTER_BOUND('',#5143,.T.) ;
#3115 = FACE_OUTER_BOUND('',#5144,.T.) ;
#3116 = FACE_OUTER_BOUND('',#5145,.T.) ;
#3117 = FACE_OUTER_BOUND('',#5146,.T.) ;
#3118 = FACE_OUTER_BOUND('',#5147,.T.) ;
#3119 = FACE_OUTER_BOUND('',#5148,.T.) ;
#3120 = FACE_OUTER_BOUND('',#5149,.T.) ;
#3121 = FACE_OUTER_BOUND('',#5150,.T.) ;
#3122 = FACE_OUTER_BOUND('',#5151,.T.) ;
#3123 = FACE_OUTER_BOUND('',#5152,.T.) ;
#3124 = FACE_OUTER_BOUND('',#5153,.T.) ;
#3125 = FACE_OUTER_BOUND('',#5154,.T.) ;
#3126 = FACE_OUTER_BOUND('',#5155,.T.) ;
#3127 = FACE_OUTER_BOUND('',#5156,.T.) ;
#3128 = FACE_OUTER_BOUND('',#5157,.T.) ;
#3129 = FACE_OUTER_BOUND('',#5158,.T.) ;
#3130 = FACE_OUTER_BOUND('',#5159,.T.) ;
#3131 = FACE_OUTER_BOUND('',#5160,.T.) ;
#3132 = FACE_OUTER_BOUND('',#5161,.T.) ;
#3133 = FACE_OUTER_BOUND('',#5162,.T.) ;
#3134 = FACE_OUTER_BOUND('',#5163,.T.) ;
#3135 = FACE_OUTER_BOUND('',#5164,.T.) ;
#3136 = FACE_OUTER_BOUND('',#5165,.T.) ;
#3137 = FACE_OUTER_BOUND('',#5166,.T.) ;
#3138 = FACE_OUTER_BOUND('',#5167,.T.) ;
#3139 = FACE_OUTER_BOUND('',#5168,.T.) ;
#3140 = FACE_OUTER_BOUND('',#5169,.T.) ;
#3141 = FACE_OUTER_BOUND('',#5170,.T.) ;
#3142 = FACE_OUTER_BOUND('',#5171,.T.) ;
#3143 = FACE_OUTER_BOUND('',#5172,.T.) ;
#3144 = FACE_OUTER_BOUND('',#5173,.T.) ;
#3145 = FACE_OUTER_BOUND('',#5174,.T.) ;
#3146 = FACE_OUTER_BOUND('',#5175,.T.) ;
#3147 = FACE_OUTER_BOUND('',#5176,.T.) ;
#3148 = FACE_OUTER_BOUND('',#5177,.T.) ;
#3149 = FACE_OUTER_BOUND('',#5178,.T.) ;
#3150 = FACE_OUTER_BOUND('',#5179,.T.) ;
#3151 = FACE_OUTER_BOUND('',#5180,.T.) ;
#3152 = FACE_OUTER_BOUND('',#5181,.T.) ;
#3153 = FACE_OUTER_BOUND('',#5182,.T.) ;
#3154 = FACE_OUTER_BOUND('',#5183,.T.) ;
#3155 = FACE_OUTER_BOUND('',#5184,.T.) ;
#3156 = FACE_OUTER_BOUND('',#5185,.T.) ;
#3157 = FACE_OUTER_BOUND('',#5186,.T.) ;
#3158 = FACE_OUTER_BOUND('',#5187,.T.) ;
#3159 = FACE_OUTER_BOUND('',#5188,.T.) ;
#3160 = FACE_OUTER_BOUND('',#5189,.T.) ;
#3161 = FACE_OUTER_BOUND('',#5190,.T.) ;
#3162 = FACE_OUTER_BOUND('',#5191,.T.) ;
#3163 = FACE_OUTER_BOUND('',#5192,.T.) ;
#3164 = FACE_OUTER_BOUND('',#5193,.T.) ;
#3165 = FACE_OUTER_BOUND('',#5197,.T.) ;
#3166 = FACE_OUTER_BOUND('',#5198,.T.) ;
#3167 = FACE_OUTER_BOUND('',#5199,.T.) ;
#3168 = FACE_OUTER_BOUND('',#5200,.T.) ;
#3169 = FACE_OUTER_BOUND('',#5201,.T.) ;
#3170 = FACE_OUTER_BOUND('',#5202,.T.) ;
#3171 = FACE_OUTER_BOUND('',#5203,.T.) ;
#3172 = FACE_OUTER_BOUND('',#5204,.T.) ;
#3173 = FACE_OUTER_BOUND('',#5205,.T.) ;
#3174 = FACE_OUTER_BOUND('',#5206,.T.) ;
#3175 = FACE_OUTER_BOUND('',#5207,.T.) ;
#3176 = FACE_OUTER_BOUND('',#5208,.T.) ;
#3177 = FACE_OUTER_BOUND('',#5209,.T.) ;
#3178 = FACE_OUTER_BOUND('',#5210,.T.) ;
#3179 = FACE_OUTER_BOUND('',#5211,.T.) ;
#3180 = FACE_OUTER_BOUND('',#5212,.T.) ;
#3181 = FACE_OUTER_BOUND('',#5213,.T.) ;
#3182 = FACE_OUTER_BOUND('',#5214,.T.) ;
#3183 = FACE_OUTER_BOUND('',#5215,.T.) ;
#3184 = FACE_OUTER_BOUND('',#5216,.T.) ;
#3185 = FACE_OUTER_BOUND('',#5218,.T.) ;
#3186 = FACE_OUTER_BOUND('',#5219,.T.) ;
#3187 = FACE_OUTER_BOUND('',#5220,.T.) ;
#3188 = FACE_OUTER_BOUND('',#5221,.T.) ;
#3189 = FACE_OUTER_BOUND('',#5222,.T.) ;
#3190 = FACE_OUTER_BOUND('',#5223,.T.) ;
#3191 = FACE_OUTER_BOUND('',#5224,.T.) ;
#3192 = FACE_OUTER_BOUND('',#5225,.T.) ;
#3193 = FACE_OUTER_BOUND('',#5226,.T.) ;
#3194 = FACE_OUTER_BOUND('',#5227,.T.) ;
#3195 = FACE_OUTER_BOUND('',#5228,.T.) ;
#3196 = FACE_OUTER_BOUND('',#5229,.T.) ;
#3197 = FACE_OUTER_BOUND('',#5230,.T.) ;
#3198 = FACE_OUTER_BOUND('',#5231,.T.) ;
#3199 = FACE_OUTER_BOUND('',#5232,.T.) ;
#3200 = FACE_OUTER_BOUND('',#5233,.T.) ;
#3201 = FACE_OUTER_BOUND('',#5234,.T.) ;
#3202 = FACE_OUTER_BOUND('',#5235,.T.) ;
#3203 = FACE_OUTER_BOUND('',#5236,.T.) ;
#3204 = FACE_OUTER_BOUND('',#5237,.T.) ;
#3205 = FACE_OUTER_BOUND('',#5238,.T.) ;
#3206 = FACE_OUTER_BOUND('',#5239,.T.) ;
#3207 = FACE_OUTER_BOUND('',#5240,.T.) ;
#3208 = FACE_OUTER_BOUND('',#5241,.T.) ;
#3209 = FACE_OUTER_BOUND('',#5242,.T.) ;
#3210 = FACE_OUTER_BOUND('',#5243,.T.) ;
#3211 = FACE_OUTER_BOUND('',#5244,.T.) ;
#3212 = FACE_OUTER_BOUND('',#5245,.T.) ;
#3213 = FACE_OUTER_BOUND('',#5246,.T.) ;
#3214 = FACE_OUTER_BOUND('',#5247,.T.) ;
#3215 = FACE_OUTER_BOUND('',#5248,.T.) ;
#3216 = FACE_OUTER_BOUND('',#5249,.T.) ;
#3217 = FACE_OUTER_BOUND('',#5250,.T.) ;
#3218 = FACE_OUTER_BOUND('',#5251,.T.) ;
#3219 = FACE_OUTER_BOUND('',#5252,.T.) ;
#3220 = FACE_OUTER_BOUND('',#5253,.T.) ;
#3221 = FACE_OUTER_BOUND('',#5254,.T.) ;
#3222 = FACE_OUTER_BOUND('',#5255,.T.) ;
#3223 = FACE_OUTER_BOUND('',#5256,.T.) ;
#3224 = FACE_OUTER_BOUND('',#5257,.T.) ;
#3225 = FACE_OUTER_BOUND('',#5258,.T.) ;
#3226 = FACE_OUTER_BOUND('',#5259,.T.) ;
#3227 = FACE_OUTER_BOUND('',#5260,.T.) ;
#3228 = FACE_OUTER_BOUND('',#5261,.T.) ;
#3229 = FACE_OUTER_BOUND('',#5262,.T.) ;
#3230 = FACE_OUTER_BOUND('',#5263,.T.) ;
#3231 = FACE_OUTER_BOUND('',#5264,.T.) ;
#3232 = FACE_OUTER_BOUND('',#5265,.T.) ;
#3233 = FACE_OUTER_BOUND('',#5266,.T.) ;
#3234 = FACE_OUTER_BOUND('',#5267,.T.) ;
#3235 = FACE_OUTER_BOUND('',#5268,.T.) ;
#3236 = FACE_OUTER_BOUND('',#5269,.T.) ;
#3237 = FACE_OUTER_BOUND('',#5270,.T.) ;
#3238 = FACE_OUTER_BOUND('',#5271,.T.) ;
#3239 = FACE_OUTER_BOUND('',#5272,.T.) ;
#3240 = FACE_OUTER_BOUND('',#5273,.T.) ;
#3241 = FACE_OUTER_BOUND('',#5274,.T.) ;
#3242 = FACE_OUTER_BOUND('',#5275,.T.) ;
#3243 = FACE_OUTER_BOUND('',#5276,.T.) ;
#3244 = FACE_OUTER_BOUND('',#5277,.T.) ;
#3245 = FACE_OUTER_BOUND('',#5278,.T.) ;
#3246 = FACE_OUTER_BOUND('',#5279,.T.) ;
#3247 = FACE_OUTER_BOUND('',#5280,.T.) ;
#3248 = FACE_OUTER_BOUND('',#5281,.T.) ;
#3249 = FACE_OUTER_BOUND('',#5282,.T.) ;
#3250 = FACE_OUTER_BOUND('',#5283,.T.) ;
#3251 = FACE_OUTER_BOUND('',#5284,.T.) ;
#3252 = FACE_OUTER_BOUND('',#5285,.T.) ;
#3253 = FACE_OUTER_BOUND('',#5286,.T.) ;
#3254 = FACE_OUTER_BOUND('',#5287,.T.) ;
#3255 = FACE_OUTER_BOUND('',#5288,.T.) ;
#3256 = FACE_OUTER_BOUND('',#5289,.T.) ;
#3257 = FACE_OUTER_BOUND('',#5290,.T.) ;
#3258 = FACE_OUTER_BOUND('',#5291,.T.) ;
#3259 = FACE_OUTER_BOUND('',#5292,.T.) ;
#3260 = FACE_OUTER_BOUND('',#5293,.T.) ;
#3261 = FACE_OUTER_BOUND('',#5294,.T.) ;
#3262 = FACE_OUTER_BOUND('',#5295,.T.) ;
#3263 = FACE_OUTER_BOUND('',#5296,.T.) ;
#3264 = FACE_OUTER_BOUND('',#5297,.T.) ;
#3265 = FACE_OUTER_BOUND('',#5298,.T.) ;
#3266 = FACE_OUTER_BOUND('',#5299,.T.) ;
#3267 = FACE_OUTER_BOUND('',#5300,.T.) ;
#3268 = FACE_OUTER_BOUND('',#5301,.T.) ;
#3269 = FACE_OUTER_BOUND('',#5302,.T.) ;
#3270 = FACE_OUTER_BOUND('',#5303,.T.) ;
#3271 = FACE_OUTER_BOUND('',#5304,.T.) ;
#3272 = FACE_OUTER_BOUND('',#5305,.T.) ;
#3273 = FACE_OUTER_BOUND('',#5306,.T.) ;
#3274 = FACE_OUTER_BOUND('',#5307,.T.) ;
#3275 = FACE_OUTER_BOUND('',#5308,.T.) ;
#3276 = FACE_OUTER_BOUND('',#5309,.T.) ;
#3277 = FACE_OUTER_BOUND('',#5310,.T.) ;
#3278 = FACE_OUTER_BOUND('',#5311,.T.) ;
#3279 = FACE_OUTER_BOUND('',#5312,.T.) ;
#3280 = FACE_OUTER_BOUND('',#5313,.T.) ;
#3281 = FACE_OUTER_BOUND('',#5314,.T.) ;
#3282 = FACE_OUTER_BOUND('',#5315,.T.) ;
#3283 = FACE_OUTER_BOUND('',#5316,.T.) ;
#3284 = FACE_OUTER_BOUND('',#5317,.T.) ;
#3285 = FACE_OUTER_BOUND('',#5318,.T.) ;
#3286 = FACE_OUTER_BOUND('',#5319,.T.) ;
#3287 = FACE_OUTER_BOUND('',#5320,.T.) ;
#3288 = FACE_OUTER_BOUND('',#5321,.T.) ;
#3289 = FACE_OUTER_BOUND('',#5322,.T.) ;
#3290 = FACE_OUTER_BOUND('',#5323,.T.) ;
#3291 = FACE_OUTER_BOUND('',#5324,.T.) ;
#3292 = FACE_OUTER_BOUND('',#5325,.T.) ;
#3293 = FACE_OUTER_BOUND('',#5326,.T.) ;
#3294 = FACE_OUTER_BOUND('',#5327,.T.) ;
#3295 = FACE_OUTER_BOUND('',#5328,.T.) ;
#3296 = FACE_OUTER_BOUND('',#5329,.T.) ;
#3297 = FACE_OUTER_BOUND('',#5330,.T.) ;
#3298 = FACE_OUTER_BOUND('',#5331,.T.) ;
#3299 = FACE_OUTER_BOUND('',#5332,.T.) ;
#3300 = FACE_OUTER_BOUND('',#5333,.T.) ;
#3301 = FACE_OUTER_BOUND('',#5334,.T.) ;
#3302 = FACE_OUTER_BOUND('',#5335,.T.) ;
#3303 = FACE_OUTER_BOUND('',#5336,.T.) ;
#3304 = FACE_OUTER_BOUND('',#5337,.T.) ;
#3305 = FACE_OUTER_BOUND('',#5338,.T.) ;
#3306 = FACE_OUTER_BOUND('',#5339,.T.) ;
#3307 = FACE_OUTER_BOUND('',#5340,.T.) ;
#3308 = FACE_OUTER_BOUND('',#5341,.T.) ;
#3309 = FACE_OUTER_BOUND('',#5342,.T.) ;
#3310 = FACE_OUTER_BOUND('',#5343,.T.) ;
#3311 = FACE_OUTER_BOUND('',#5344,.T.) ;
#3312 = FACE_OUTER_BOUND('',#5345,.T.) ;
#3313 = FACE_OUTER_BOUND('',#5346,.T.) ;
#3314 = FACE_OUTER_BOUND('',#5347,.T.) ;
#3315 = FACE_OUTER_BOUND('',#5348,.T.) ;
#3316 = FACE_OUTER_BOUND('',#5349,.T.) ;
#3317 = FACE_OUTER_BOUND('',#5350,.T.) ;
#3318 = FACE_OUTER_BOUND('',#5351,.T.) ;
#3319 = FACE_OUTER_BOUND('',#5352,.T.) ;
#3320 = FACE_OUTER_BOUND('',#5353,.T.) ;
#3321 = FACE_OUTER_BOUND('',#5354,.T.) ;
#3322 = FACE_OUTER_BOUND('',#5355,.T.) ;
#3323 = FACE_OUTER_BOUND('',#5356,.T.) ;
#3324 = FACE_OUTER_BOUND('',#5357,.T.) ;
#3325 = FACE_OUTER_BOUND('',#5358,.T.) ;
#3326 = FACE_OUTER_BOUND('',#5359,.T.) ;
#3327 = FACE_OUTER_BOUND('',#5360,.T.) ;
#3328 = FACE_OUTER_BOUND('',#5361,.T.) ;
#3329 = FACE_OUTER_BOUND('',#5362,.T.) ;
#3330 = FACE_OUTER_BOUND('',#5363,.T.) ;
#3331 = FACE_OUTER_BOUND('',#5364,.T.) ;
#3332 = FACE_OUTER_BOUND('',#5365,.T.) ;
#3333 = FACE_OUTER_BOUND('',#5366,.T.) ;
#3334 = FACE_OUTER_BOUND('',#5367,.T.) ;
#3335 = FACE_OUTER_BOUND('',#5368,.T.) ;
#3336 = FACE_OUTER_BOUND('',#5369,.T.) ;
#3337 = FACE_OUTER_BOUND('',#5370,.T.) ;
#3338 = FACE_OUTER_BOUND('',#5371,.T.) ;
#3339 = FACE_OUTER_BOUND('',#5372,.T.) ;
#3340 = FACE_OUTER_BOUND('',#5373,.T.) ;
#3341 = FACE_OUTER_BOUND('',#5374,.T.) ;
#3342 = FACE_OUTER_BOUND('',#5375,.T.) ;
#3343 = FACE_OUTER_BOUND('',#5376,.T.) ;
#3344 = FACE_OUTER_BOUND('',#5377,.T.) ;
#3345 = FACE_OUTER_BOUND('',#5378,.T.) ;
#3346 = FACE_OUTER_BOUND('',#5379,.T.) ;
#3347 = FACE_OUTER_BOUND('',#5380,.T.) ;
#3348 = FACE_OUTER_BOUND('',#5381,.T.) ;
#3349 = FACE_OUTER_BOUND('',#5382,.T.) ;
#3350 = FACE_OUTER_BOUND('',#5383,.T.) ;
#3351 = FACE_OUTER_BOUND('',#5384,.T.) ;
#3352 = FACE_OUTER_BOUND('',#5385,.T.) ;
#3353 = FACE_OUTER_BOUND('',#5386,.T.) ;
#3354 = FACE_OUTER_BOUND('',#5387,.T.) ;
#3355 = FACE_OUTER_BOUND('',#5388,.T.) ;
#3356 = FACE_OUTER_BOUND('',#5389,.T.) ;
#3357 = FACE_OUTER_BOUND('',#5390,.T.) ;
#3358 = FACE_OUTER_BOUND('',#5391,.T.) ;
#3359 = FACE_OUTER_BOUND('',#5392,.T.) ;
#3360 = FACE_OUTER_BOUND('',#5393,.T.) ;
#3361 = FACE_OUTER_BOUND('',#5394,.T.) ;
#3362 = FACE_OUTER_BOUND('',#5395,.T.) ;
#3363 = FACE_OUTER_BOUND('',#5396,.T.) ;
#3364 = FACE_OUTER_BOUND('',#5397,.T.) ;
#3365 = FACE_OUTER_BOUND('',#5398,.T.) ;
#3366 = FACE_OUTER_BOUND('',#5399,.T.) ;
#3367 = FACE_OUTER_BOUND('',#5400,.T.) ;
#3368 = FACE_OUTER_BOUND('',#5401,.T.) ;
#3369 = FACE_OUTER_BOUND('',#5402,.T.) ;
#3370 = FACE_OUTER_BOUND('',#5403,.T.) ;
#3371 = FACE_OUTER_BOUND('',#5404,.T.) ;
#3372 = FACE_OUTER_BOUND('',#5405,.T.) ;
#3373 = FACE_OUTER_BOUND('',#5406,.T.) ;
#3374 = FACE_OUTER_BOUND('',#5407,.T.) ;
#3375 = FACE_OUTER_BOUND('',#5408,.T.) ;
#3376 = FACE_OUTER_BOUND('',#5409,.T.) ;
#3377 = FACE_OUTER_BOUND('',#5410,.T.) ;
#3378 = FACE_OUTER_BOUND('',#5411,.T.) ;
#3379 = FACE_OUTER_BOUND('',#5412,.T.) ;
#3380 = FACE_OUTER_BOUND('',#5413,.T.) ;
#3381 = FACE_OUTER_BOUND('',#5414,.T.) ;
#3382 = FACE_OUTER_BOUND('',#5415,.T.) ;
#3383 = FACE_OUTER_BOUND('',#5416,.T.) ;
#3384 = FACE_OUTER_BOUND('',#5417,.T.) ;
#3385 = FACE_OUTER_BOUND('',#5418,.T.) ;
#3386 = FACE_OUTER_BOUND('',#5419,.T.) ;
#3387 = FACE_OUTER_BOUND('',#5420,.T.) ;
#3388 = FACE_OUTER_BOUND('',#5421,.T.) ;
#3389 = FACE_OUTER_BOUND('',#5422,.T.) ;
#3390 = FACE_OUTER_BOUND('',#5423,.T.) ;
#3391 = FACE_OUTER_BOUND('',#5424,.T.) ;
#3392 = FACE_OUTER_BOUND('',#5425,.T.) ;
#3393 = FACE_OUTER_BOUND('',#5426,.T.) ;
#3394 = FACE_OUTER_BOUND('',#5427,.T.) ;
#3395 = FACE_OUTER_BOUND('',#5428,.T.) ;
#3396 = FACE_OUTER_BOUND('',#5429,.T.) ;
#3397 = FACE_OUTER_BOUND('',#5430,.T.) ;
#3398 = FACE_OUTER_BOUND('',#5431,.T.) ;
#3399 = FACE_OUTER_BOUND('',#5432,.T.) ;
#3400 = FACE_OUTER_BOUND('',#5433,.T.) ;
#3401 = FACE_OUTER_BOUND('',#5434,.T.) ;
#3402 = FACE_OUTER_BOUND('',#5435,.T.) ;
#3403 = FACE_OUTER_BOUND('',#5436,.T.) ;
#3404 = FACE_OUTER_BOUND('',#5437,.T.) ;
#3405 = FACE_OUTER_BOUND('',#5438,.T.) ;
#3406 = FACE_OUTER_BOUND('',#5439,.T.) ;
#3407 = FACE_OUTER_BOUND('',#5440,.T.) ;
#3408 = FACE_OUTER_BOUND('',#5441,.T.) ;
#3409 = FACE_OUTER_BOUND('',#5442,.T.) ;
#3410 = FACE_OUTER_BOUND('',#5443,.T.) ;
#3411 = FACE_OUTER_BOUND('',#5444,.T.) ;
#3412 = FACE_OUTER_BOUND('',#5445,.T.) ;
#3413 = FACE_OUTER_BOUND('',#5446,.T.) ;
#3414 = FACE_OUTER_BOUND('',#5447,.T.) ;
#3415 = FACE_OUTER_BOUND('',#5448,.T.) ;
#3416 = FACE_OUTER_BOUND('',#5449,.T.) ;
#3417 = FACE_OUTER_BOUND('',#5450,.T.) ;
#3418 = FACE_OUTER_BOUND('',#5451,.T.) ;
#3419 = FACE_OUTER_BOUND('',#5452,.T.) ;
#3420 = FACE_OUTER_BOUND('',#5453,.T.) ;
#3421 = FACE_OUTER_BOUND('',#5454,.T.) ;
#3422 = FACE_OUTER_BOUND('',#5455,.T.) ;
#3423 = FACE_OUTER_BOUND('',#5456,.T.) ;
#3424 = FACE_OUTER_BOUND('',#5457,.T.) ;
#3425 = FACE_OUTER_BOUND('',#5458,.T.) ;
#3426 = FACE_OUTER_BOUND('',#5459,.T.) ;
#3427 = FACE_OUTER_BOUND('',#5460,.T.) ;
#3428 = FACE_OUTER_BOUND('',#5461,.T.) ;
#3429 = FACE_OUTER_BOUND('',#5462,.T.) ;
#3430 = FACE_OUTER_BOUND('',#5463,.T.) ;
#3431 = FACE_OUTER_BOUND('',#5464,.T.) ;
#3432 = FACE_OUTER_BOUND('',#5465,.T.) ;
#3433 = FACE_OUTER_BOUND('',#5466,.T.) ;
#3434 = FACE_OUTER_BOUND('',#5467,.T.) ;
#3435 = FACE_OUTER_BOUND('',#5468,.T.) ;
#3436 = FACE_OUTER_BOUND('',#5469,.T.) ;
#3437 = FACE_OUTER_BOUND('',#5470,.T.) ;
#3438 = FACE_OUTER_BOUND('',#5471,.T.) ;
#3439 = FACE_OUTER_BOUND('',#5472,.T.) ;
#3440 = FACE_OUTER_BOUND('',#5473,.T.) ;
#3441 = FACE_OUTER_BOUND('',#5474,.T.) ;
#3442 = FACE_OUTER_BOUND('',#5475,.T.) ;
#3443 = FACE_OUTER_BOUND('',#5476,.T.) ;
#3444 = FACE_OUTER_BOUND('',#5477,.T.) ;
#3445 = FACE_OUTER_BOUND('',#5478,.T.) ;
#3446 = FACE_OUTER_BOUND('',#5479,.T.) ;
#3447 = FACE_OUTER_BOUND('',#5480,.T.) ;
#3448 = FACE_OUTER_BOUND('',#5481,.T.) ;
#3449 = FACE_OUTER_BOUND('',#5482,.T.) ;
#3450 = FACE_OUTER_BOUND('',#5483,.T.) ;
#3451 = FACE_OUTER_BOUND('',#5484,.T.) ;
#3452 = FACE_OUTER_BOUND('',#5485,.T.) ;
#3453 = FACE_OUTER_BOUND('',#5486,.T.) ;
#3454 = FACE_OUTER_BOUND('',#5487,.T.) ;
#3455 = FACE_OUTER_BOUND('',#5488,.T.) ;
#3456 = FACE_OUTER_BOUND('',#5489,.T.) ;
#3457 = FACE_OUTER_BOUND('',#5490,.T.) ;
#3458 = FACE_OUTER_BOUND('',#5491,.T.) ;
#3459 = FACE_OUTER_BOUND('',#5492,.T.) ;
#3460 = FACE_OUTER_BOUND('',#5493,.T.) ;
#3461 = FACE_OUTER_BOUND('',#5494,.T.) ;
#3462 = FACE_OUTER_BOUND('',#5495,.T.) ;
#3463 = FACE_OUTER_BOUND('',#5496,.T.) ;
#3464 = FACE_OUTER_BOUND('',#5497,.T.) ;
#3465 = FACE_OUTER_BOUND('',#5498,.T.) ;
#3466 = FACE_OUTER_BOUND('',#5499,.T.) ;
#3467 = FACE_OUTER_BOUND('',#5500,.T.) ;
#3468 = FACE_OUTER_BOUND('',#5501,.T.) ;
#3469 = FACE_OUTER_BOUND('',#5502,.T.) ;
#3470 = FACE_OUTER_BOUND('',#5503,.T.) ;
#3471 = FACE_OUTER_BOUND('',#5504,.T.) ;
#3472 = FACE_OUTER_BOUND('',#5505,.T.) ;
#3473 = FACE_OUTER_BOUND('',#5506,.T.) ;
#3474 = FACE_OUTER_BOUND('',#5507,.T.) ;
#3475 = FACE_OUTER_BOUND('',#5508,.T.) ;
#3476 = FACE_OUTER_BOUND('',#5509,.T.) ;
#3477 = FACE_OUTER_BOUND('',#5510,.T.) ;
#3478 = FACE_OUTER_BOUND('',#5511,.T.) ;
#3479 = FACE_OUTER_BOUND('',#5512,.T.) ;
#3480 = FACE_OUTER_BOUND('',#5513,.T.) ;
#3481 = FACE_OUTER_BOUND('',#5514,.T.) ;
#3482 = FACE_OUTER_BOUND('',#5515,.T.) ;
#3483 = FACE_OUTER_BOUND('',#5516,.T.) ;
#3484 = FACE_OUTER_BOUND('',#5517,.T.) ;
#3485 = FACE_OUTER_BOUND('',#5518,.T.) ;
#3486 = FACE_OUTER_BOUND('',#5519,.T.) ;
#3487 = FACE_OUTER_BOUND('',#5520,.T.) ;
#3488 = FACE_OUTER_BOUND('',#5521,.T.) ;
#3489 = FACE_OUTER_BOUND('',#5522,.T.) ;
#3490 = FACE_OUTER_BOUND('',#5523,.T.) ;
#3491 = FACE_OUTER_BOUND('',#5524,.T.) ;
#3492 = FACE_OUTER_BOUND('',#5525,.T.) ;
#3493 = FACE_OUTER_BOUND('',#5526,.T.) ;
#3494 = FACE_OUTER_BOUND('',#5527,.T.) ;
#3495 = FACE_OUTER_BOUND('',#5528,.T.) ;
#3496 = FACE_OUTER_BOUND('',#5529,.T.) ;
#3497 = FACE_OUTER_BOUND('',#5530,.T.) ;
#3498 = FACE_OUTER_BOUND('',#5531,.T.) ;
#3499 = FACE_OUTER_BOUND('',#5532,.T.) ;
#3500 = FACE_OUTER_BOUND('',#5533,.T.) ;
#3501 = FACE_OUTER_BOUND('',#5534,.T.) ;
#3502 = FACE_OUTER_BOUND('',#5535,.T.) ;
#3503 = FACE_OUTER_BOUND('',#5536,.T.) ;
#3504 = FACE_OUTER_BOUND('',#5537,.T.) ;
#3505 = FACE_OUTER_BOUND('',#5538,.T.) ;
#3506 = FACE_OUTER_BOUND('',#5539,.T.) ;
#3507 = FACE_OUTER_BOUND('',#5540,.T.) ;
#3508 = FACE_OUTER_BOUND('',#5541,.T.) ;
#3509 = FACE_OUTER_BOUND('',#5542,.T.) ;
#3510 = FACE_OUTER_BOUND('',#5543,.T.) ;
#3511 = FACE_OUTER_BOUND('',#5544,.T.) ;
#3512 = FACE_OUTER_BOUND('',#5545,.T.) ;
#3513 = FACE_OUTER_BOUND('',#5546,.T.) ;
#3514 = FACE_OUTER_BOUND('',#5547,.T.) ;
#3515 = FACE_OUTER_BOUND('',#5548,.T.) ;
#3516 = FACE_OUTER_BOUND('',#5549,.T.) ;
#3517 = FACE_OUTER_BOUND('',#5550,.T.) ;
#3518 = FACE_OUTER_BOUND('',#5551,.T.) ;
#3519 = FACE_OUTER_BOUND('',#5552,.T.) ;
#3520 = FACE_OUTER_BOUND('',#5553,.T.) ;
#3521 = FACE_OUTER_BOUND('',#5554,.T.) ;
#3522 = FACE_OUTER_BOUND('',#5555,.T.) ;
#3523 = FACE_OUTER_BOUND('',#5556,.T.) ;
#3524 = FACE_OUTER_BOUND('',#5557,.T.) ;
#3525 = FACE_OUTER_BOUND('',#5558,.T.) ;
#3526 = FACE_OUTER_BOUND('',#5559,.T.) ;
#3527 = FACE_OUTER_BOUND('',#5560,.T.) ;
#3528 = FACE_OUTER_BOUND('',#5561,.T.) ;
#3529 = FACE_OUTER_BOUND('',#5562,.T.) ;
#3530 = FACE_OUTER_BOUND('',#5563,.T.) ;
#3531 = FACE_OUTER_BOUND('',#5564,.T.) ;
#3532 = FACE_OUTER_BOUND('',#5568,.T.) ;
#3533 = FACE_OUTER_BOUND('',#5569,.T.) ;
#3534 = FACE_OUTER_BOUND('',#5570,.T.) ;
#3535 = FACE_OUTER_BOUND('',#5571,.T.) ;
#3536 = FACE_OUTER_BOUND('',#5572,.T.) ;
#3537 = FACE_OUTER_BOUND('',#5573,.T.) ;
#3538 = FACE_OUTER_BOUND('',#5577,.T.) ;
#3539 = FACE_OUTER_BOUND('',#5578,.T.) ;
#3540 = FACE_OUTER_BOUND('',#5579,.T.) ;
#3541 = FACE_OUTER_BOUND('',#5580,.T.) ;
#3542 = FACE_OUTER_BOUND('',#5581,.T.) ;
#3543 = FACE_OUTER_BOUND('',#5582,.T.) ;
#3544 = FACE_OUTER_BOUND('',#5586,.T.) ;
#3545 = FACE_OUTER_BOUND('',#5587,.T.) ;
#3546 = FACE_OUTER_BOUND('',#5588,.T.) ;
#3547 = FACE_OUTER_BOUND('',#5589,.T.) ;
#3548 = FACE_OUTER_BOUND('',#5590,.T.) ;
#3549 = FACE_OUTER_BOUND('',#5591,.T.) ;
#3550 = FACE_OUTER_BOUND('',#5595,.T.) ;
#3551 = FACE_OUTER_BOUND('',#5596,.T.) ;
#3552 = FACE_OUTER_BOUND('',#5597,.T.) ;
#3553 = FACE_OUTER_BOUND('',#5598,.T.) ;
#3554 = FACE_OUTER_BOUND('',#5599,.T.) ;
#3555 = FACE_OUTER_BOUND('',#5600,.T.) ;
#3556 = FACE_OUTER_BOUND('',#5604,.T.) ;
#3557 = FACE_OUTER_BOUND('',#5605,.T.) ;
#3558 = FACE_OUTER_BOUND('',#5606,.T.) ;
#3559 = FACE_OUTER_BOUND('',#5607,.T.) ;
#3560 = FACE_OUTER_BOUND('',#5608,.T.) ;
#3561 = FACE_OUTER_BOUND('',#5609,.T.) ;
#3562 = FACE_OUTER_BOUND('',#5613,.T.) ;
#3563 = FACE_OUTER_BOUND('',#5614,.T.) ;
#3564 = FACE_OUTER_BOUND('',#5615,.T.) ;
#3565 = FACE_OUTER_BOUND('',#5616,.T.) ;
#3566 = FACE_OUTER_BOUND('',#5617,.T.) ;
#3567 = FACE_OUTER_BOUND('',#5618,.T.) ;
#3568 = FACE_OUTER_BOUND('',#5622,.T.) ;
#3569 = FACE_OUTER_BOUND('',#5623,.T.) ;
#3570 = FACE_OUTER_BOUND('',#5624,.T.) ;
#3571 = FACE_OUTER_BOUND('',#5625,.T.) ;
#3572 = FACE_OUTER_BOUND('',#5626,.T.) ;
#3573 = FACE_OUTER_BOUND('',#5627,.T.) ;
#3574 = FACE_OUTER_BOUND('',#5631,.T.) ;
#3575 = FACE_OUTER_BOUND('',#5632,.T.) ;
#3576 = FACE_OUTER_BOUND('',#5633,.T.) ;
#3577 = FACE_OUTER_BOUND('',#5634,.T.) ;
#3578 = FACE_OUTER_BOUND('',#5635,.T.) ;
#3579 = FACE_OUTER_BOUND('',#5636,.T.) ;
#3580 = FACE_OUTER_BOUND('',#5637,.T.) ;
#3581 = FACE_OUTER_BOUND('',#5638,.T.) ;
#3582 = FACE_OUTER_BOUND('',#5639,.T.) ;
#3583 = FACE_OUTER_BOUND('',#5640,.T.) ;
#3584 = FACE_OUTER_BOUND('',#5641,.T.) ;
#3585 = FACE_OUTER_BOUND('',#5642,.T.) ;
#3586 = FACE_OUTER_BOUND('',#5643,.T.) ;
#3587 = FACE_OUTER_BOUND('',#5644,.T.) ;
#3588 = FACE_OUTER_BOUND('',#5645,.T.) ;
#3589 = FACE_OUTER_BOUND('',#5646,.T.) ;
#3590 = FACE_OUTER_BOUND('',#5647,.T.) ;
#3591 = FACE_OUTER_BOUND('',#5648,.T.) ;
#3592 = FACE_OUTER_BOUND('',#5649,.T.) ;
#3593 = FACE_OUTER_BOUND('',#5650,.T.) ;
#3594 = FACE_OUTER_BOUND('',#5651,.T.) ;
#3595 = FACE_OUTER_BOUND('',#5652,.T.) ;
#3596 = FACE_OUTER_BOUND('',#5653,.T.) ;
#3597 = FACE_OUTER_BOUND('',#5654,.T.) ;
#3598 = FACE_OUTER_BOUND('',#5655,.T.) ;
#3599 = FACE_OUTER_BOUND('',#5656,.T.) ;
#3600 = FACE_OUTER_BOUND('',#5657,.T.) ;
#3601 = FACE_OUTER_BOUND('',#5658,.T.) ;
#3602 = FACE_OUTER_BOUND('',#5659,.T.) ;
#3603 = FACE_OUTER_BOUND('',#5660,.T.) ;
#3604 = FACE_OUTER_BOUND('',#5661,.T.) ;
#3605 = FACE_OUTER_BOUND('',#5662,.T.) ;
#3606 = FACE_OUTER_BOUND('',#5663,.T.) ;
#3607 = FACE_OUTER_BOUND('',#5664,.T.) ;
#3608 = FACE_OUTER_BOUND('',#5665,.T.) ;
#3609 = FACE_OUTER_BOUND('',#5666,.T.) ;
#3610 = FACE_OUTER_BOUND('',#5667,.T.) ;
#3611 = FACE_OUTER_BOUND('',#5668,.T.) ;
#3612 = FACE_OUTER_BOUND('',#5669,.T.) ;
#3613 = FACE_OUTER_BOUND('',#5670,.T.) ;
#3614 = FACE_OUTER_BOUND('',#5671,.T.) ;
#3615 = FACE_OUTER_BOUND('',#5672,.T.) ;
#3616 = FACE_OUTER_BOUND('',#5673,.T.) ;
#3617 = FACE_OUTER_BOUND('',#5674,.T.) ;
#3618 = FACE_OUTER_BOUND('',#5675,.T.) ;
#3619 = FACE_OUTER_BOUND('',#5676,.T.) ;
#3620 = FACE_OUTER_BOUND('',#5677,.T.) ;
#3621 = FACE_OUTER_BOUND('',#5678,.T.) ;
#3622 = FACE_OUTER_BOUND('',#5679,.T.) ;
#3623 = FACE_OUTER_BOUND('',#5680,.T.) ;
#3624 = FACE_OUTER_BOUND('',#5681,.T.) ;
#3625 = FACE_OUTER_BOUND('',#5682,.T.) ;
#3626 = FACE_OUTER_BOUND('',#5683,.T.) ;
#3627 = FACE_OUTER_BOUND('',#5684,.T.) ;
#3628 = FACE_OUTER_BOUND('',#5685,.T.) ;
#3629 = FACE_OUTER_BOUND('',#5686,.T.) ;
#3630 = FACE_OUTER_BOUND('',#5687,.T.) ;
#3631 = FACE_OUTER_BOUND('',#5688,.T.) ;
#3632 = FACE_OUTER_BOUND('',#5689,.T.) ;
#3633 = FACE_OUTER_BOUND('',#5690,.T.) ;
#3634 = FACE_OUTER_BOUND('',#5691,.T.) ;
#3635 = FACE_OUTER_BOUND('',#5692,.T.) ;
#3636 = FACE_OUTER_BOUND('',#5693,.T.) ;
#3637 = FACE_OUTER_BOUND('',#5694,.T.) ;
#3638 = FACE_OUTER_BOUND('',#5695,.T.) ;
#3639 = FACE_OUTER_BOUND('',#5696,.T.) ;
#3640 = FACE_OUTER_BOUND('',#5697,.T.) ;
#3641 = FACE_OUTER_BOUND('',#5698,.T.) ;
#3642 = FACE_OUTER_BOUND('',#5699,.T.) ;
#3643 = FACE_OUTER_BOUND('',#5700,.T.) ;
#3644 = FACE_OUTER_BOUND('',#5701,.T.) ;
#3645 = FACE_OUTER_BOUND('',#5702,.T.) ;
#3646 = FACE_OUTER_BOUND('',#5703,.T.) ;
#3647 = FACE_OUTER_BOUND('',#5704,.T.) ;
#3648 = FACE_OUTER_BOUND('',#5705,.T.) ;
#3649 = FACE_OUTER_BOUND('',#5706,.T.) ;
#3650 = FACE_OUTER_BOUND('',#5707,.T.) ;
#3651 = FACE_OUTER_BOUND('',#5708,.T.) ;
#3652 = FACE_OUTER_BOUND('',#5709,.T.) ;
#3653 = FACE_OUTER_BOUND('',#5710,.T.) ;
#3654 = FACE_OUTER_BOUND('',#5711,.T.) ;
#3655 = FACE_OUTER_BOUND('',#5712,.T.) ;
#3656 = FACE_OUTER_BOUND('',#5713,.T.) ;
#3657 = FACE_OUTER_BOUND('',#5714,.T.) ;
#3658 = FACE_OUTER_BOUND('',#5715,.T.) ;
#3659 = FACE_OUTER_BOUND('',#5716,.T.) ;
#3660 = FACE_OUTER_BOUND('',#5717,.T.) ;
#3661 = FACE_OUTER_BOUND('',#5718,.T.) ;
#3662 = FACE_OUTER_BOUND('',#5719,.T.) ;
#3663 = FACE_OUTER_BOUND('',#5720,.T.) ;
#3664 = FACE_OUTER_BOUND('',#5721,.T.) ;
#3665 = FACE_OUTER_BOUND('',#5722,.T.) ;
#3666 = FACE_OUTER_BOUND('',#5723,.T.) ;
#3667 = FACE_OUTER_BOUND('',#5724,.T.) ;
#3668 = FACE_OUTER_BOUND('',#5725,.T.) ;
#3669 = FACE_OUTER_BOUND('',#5726,.T.) ;
#3670 = FACE_OUTER_BOUND('',#5727,.T.) ;
#3671 = FACE_OUTER_BOUND('',#5728,.T.) ;
#3672 = FACE_OUTER_BOUND('',#5729,.T.) ;
#3673 = FACE_OUTER_BOUND('',#5730,.T.) ;
#3674 = FACE_OUTER_BOUND('',#5731,.T.) ;
#3675 = FACE_OUTER_BOUND('',#5732,.T.) ;
#3676 = FACE_OUTER_BOUND('',#5733,.T.) ;
#3677 = FACE_OUTER_BOUND('',#5734,.T.) ;
#3678 = FACE_OUTER_BOUND('',#5735,.T.) ;
#3679 = FACE_OUTER_BOUND('',#5736,.T.) ;
#3680 = FACE_OUTER_BOUND('',#5737,.T.) ;
#3681 = FACE_OUTER_BOUND('',#5738,.T.) ;
#3682 = FACE_OUTER_BOUND('',#5739,.T.) ;
#3683 = FACE_OUTER_BOUND('',#5740,.T.) ;
#3684 = FACE_OUTER_BOUND('',#5741,.T.) ;
#3685 = FACE_OUTER_BOUND('',#5742,.T.) ;
#3686 = FACE_OUTER_BOUND('',#5743,.T.) ;
#3687 = FACE_OUTER_BOUND('',#5744,.T.) ;
#3688 = FACE_OUTER_BOUND('',#5745,.T.) ;
#3689 = FACE_OUTER_BOUND('',#5746,.T.) ;
#3690 = FACE_OUTER_BOUND('',#5747,.T.) ;
#3691 = FACE_OUTER_BOUND('',#5748,.T.) ;
#3692 = FACE_OUTER_BOUND('',#5749,.T.) ;
#3693 = FACE_OUTER_BOUND('',#5750,.T.) ;
#3694 = FACE_OUTER_BOUND('',#5751,.T.) ;
#3695 = FACE_OUTER_BOUND('',#5752,.T.) ;
#3696 = FACE_OUTER_BOUND('',#5753,.T.) ;
#3697 = FACE_OUTER_BOUND('',#5754,.T.) ;
#3698 = FACE_OUTER_BOUND('',#5755,.T.) ;
#3699 = FACE_OUTER_BOUND('',#5756,.T.) ;
#3700 = FACE_OUTER_BOUND('',#5757,.T.) ;
#3701 = FACE_OUTER_BOUND('',#5758,.T.) ;
#3702 = FACE_OUTER_BOUND('',#5759,.T.) ;
#3703 = FACE_OUTER_BOUND('',#5760,.T.) ;
#3704 = FACE_OUTER_BOUND('',#5761,.T.) ;
#3705 = FACE_OUTER_BOUND('',#5762,.T.) ;
#3706 = FACE_OUTER_BOUND('',#5763,.T.) ;
#3707 = FACE_OUTER_BOUND('',#5764,.T.) ;
#3708 = FACE_OUTER_BOUND('',#5765,.T.) ;
#3709 = FACE_OUTER_BOUND('',#5766,.T.) ;
#3710 = FACE_OUTER_BOUND('',#5767,.T.) ;
#3711 = FACE_OUTER_BOUND('',#5768,.T.) ;
#3712 = FACE_OUTER_BOUND('',#5769,.T.) ;
#3713 = FACE_OUTER_BOUND('',#5770,.T.) ;
#3714 = FACE_OUTER_BOUND('',#5771,.T.) ;
#3715 = FACE_OUTER_BOUND('',#5772,.T.) ;
#3716 = FACE_OUTER_BOUND('',#5773,.T.) ;
#3717 = FACE_OUTER_BOUND('',#5774,.T.) ;
#3718 = FACE_OUTER_BOUND('',#5775,.T.) ;
#3719 = FACE_OUTER_BOUND('',#5776,.T.) ;
#3720 = FACE_OUTER_BOUND('',#5777,.T.) ;
#3721 = FACE_OUTER_BOUND('',#5778,.T.) ;
#3722 = FACE_OUTER_BOUND('',#5779,.T.) ;
#3723 = FACE_OUTER_BOUND('',#5780,.T.) ;
#3724 = FACE_OUTER_BOUND('',#5781,.T.) ;
#3725 = FACE_OUTER_BOUND('',#5782,.T.) ;
#3726 = FACE_OUTER_BOUND('',#5783,.T.) ;
#3727 = FACE_OUTER_BOUND('',#5784,.T.) ;
#3728 = FACE_OUTER_BOUND('',#5785,.T.) ;
#3729 = FACE_OUTER_BOUND('',#5786,.T.) ;
#3730 = FACE_OUTER_BOUND('',#5788,.T.) ;
#3731 = FACE_OUTER_BOUND('',#5789,.T.) ;
#3732 = FACE_OUTER_BOUND('',#5790,.T.) ;
#3733 = FACE_OUTER_BOUND('',#5791,.T.) ;
#3734 = FACE_OUTER_BOUND('',#5792,.T.) ;
#3735 = FACE_OUTER_BOUND('',#5793,.T.) ;
#3736 = FACE_OUTER_BOUND('',#5794,.T.) ;
#3737 = FACE_OUTER_BOUND('',#5795,.T.) ;
#3738 = FACE_OUTER_BOUND('',#5796,.T.) ;
#3739 = FACE_OUTER_BOUND('',#5797,.T.) ;
#3740 = FACE_OUTER_BOUND('',#5798,.T.) ;
#3741 = FACE_OUTER_BOUND('',#5799,.T.) ;
#3742 = FACE_OUTER_BOUND('',#5800,.T.) ;
#3743 = FACE_OUTER_BOUND('',#5801,.T.) ;
#3744 = FACE_OUTER_BOUND('',#5802,.T.) ;
#3745 = FACE_OUTER_BOUND('',#5803,.T.) ;
#3746 = FACE_OUTER_BOUND('',#5804,.T.) ;
#3747 = FACE_OUTER_BOUND('',#5805,.T.) ;
#3748 = FACE_OUTER_BOUND('',#5806,.T.) ;
#3749 = FACE_OUTER_BOUND('',#5807,.T.) ;
#3750 = FACE_OUTER_BOUND('',#5808,.T.) ;
#3751 = FACE_OUTER_BOUND('',#5809,.T.) ;
#3752 = FACE_OUTER_BOUND('',#5810,.T.) ;
#3753 = FACE_OUTER_BOUND('',#5811,.T.) ;
#3754 = FACE_OUTER_BOUND('',#5812,.T.) ;
#3755 = FACE_OUTER_BOUND('',#5813,.T.) ;
#3756 = FACE_OUTER_BOUND('',#5814,.T.) ;
#3757 = FACE_OUTER_BOUND('',#5815,.T.) ;
#3758 = FACE_OUTER_BOUND('',#5816,.T.) ;
#3759 = FACE_OUTER_BOUND('',#5817,.T.) ;
#3760 = FACE_OUTER_BOUND('',#5818,.T.) ;
#3761 = FACE_OUTER_BOUND('',#5819,.T.) ;
#3762 = FACE_OUTER_BOUND('',#5820,.T.) ;
#3763 = FACE_OUTER_BOUND('',#5821,.T.) ;
#3764 = FACE_OUTER_BOUND('',#5822,.T.) ;
#3765 = FACE_OUTER_BOUND('',#5823,.T.) ;
#3766 = FACE_OUTER_BOUND('',#5824,.T.) ;
#3767 = FACE_OUTER_BOUND('',#5825,.T.) ;
#3768 = FACE_OUTER_BOUND('',#5826,.T.) ;
#3769 = FACE_OUTER_BOUND('',#5827,.T.) ;
#3770 = FACE_OUTER_BOUND('',#5828,.T.) ;
#3771 = FACE_OUTER_BOUND('',#5829,.T.) ;
#3772 = FACE_OUTER_BOUND('',#5830,.T.) ;
#3773 = FACE_OUTER_BOUND('',#5831,.T.) ;
#3774 = FACE_OUTER_BOUND('',#5832,.T.) ;
#3775 = FACE_OUTER_BOUND('',#5833,.T.) ;
#3776 = FACE_OUTER_BOUND('',#5834,.T.) ;
#3777 = FACE_OUTER_BOUND('',#5835,.T.) ;
#3778 = FACE_OUTER_BOUND('',#5836,.T.) ;
#3779 = FACE_OUTER_BOUND('',#5837,.T.) ;
#3780 = FACE_OUTER_BOUND('',#5838,.T.) ;
#3781 = FACE_OUTER_BOUND('',#5839,.T.) ;
#3782 = FACE_OUTER_BOUND('',#5840,.T.) ;
#3783 = FACE_OUTER_BOUND('',#5841,.T.) ;
#3784 = FACE_OUTER_BOUND('',#5842,.T.) ;
#3785 = FACE_OUTER_BOUND('',#5843,.T.) ;
#3786 = FACE_OUTER_BOUND('',#5844,.T.) ;
#3787 = FACE_OUTER_BOUND('',#5845,.T.) ;
#3788 = FACE_OUTER_BOUND('',#5846,.T.) ;
#3789 = FACE_OUTER_BOUND('',#5847,.T.) ;
#3790 = FACE_OUTER_BOUND('',#5848,.T.) ;
#3791 = FACE_OUTER_BOUND('',#5849,.T.) ;
#3792 = FACE_OUTER_BOUND('',#5850,.T.) ;
#3793 = FACE_OUTER_BOUND('',#5851,.T.) ;
#3794 = FACE_OUTER_BOUND('',#5852,.T.) ;
#3795 = FACE_OUTER_BOUND('',#5853,.T.) ;
#3796 = FACE_OUTER_BOUND('',#5854,.T.) ;
#3797 = FACE_OUTER_BOUND('',#5855,.T.) ;
#3798 = FACE_OUTER_BOUND('',#5856,.T.) ;
#3799 = FACE_OUTER_BOUND('',#5857,.T.) ;
#3800 = FACE_OUTER_BOUND('',#5858,.T.) ;
#3801 = FACE_OUTER_BOUND('',#5859,.T.) ;
#3802 = FACE_OUTER_BOUND('',#5860,.T.) ;
#3803 = FACE_OUTER_BOUND('',#5861,.T.) ;
#3804 = FACE_OUTER_BOUND('',#5862,.T.) ;
#3805 = FACE_OUTER_BOUND('',#5863,.T.) ;
#3806 = FACE_OUTER_BOUND('',#5864,.T.) ;
#3807 = FACE_OUTER_BOUND('',#5865,.T.) ;
#3808 = FACE_OUTER_BOUND('',#5866,.T.) ;
#3809 = FACE_OUTER_BOUND('',#5867,.T.) ;
#3810 = FACE_OUTER_BOUND('',#5868,.T.) ;
#3811 = FACE_OUTER_BOUND('',#5869,.T.) ;
#3812 = FACE_OUTER_BOUND('',#5870,.T.) ;
#3813 = FACE_OUTER_BOUND('',#5871,.T.) ;
#3814 = FACE_OUTER_BOUND('',#5872,.T.) ;
#3815 = FACE_OUTER_BOUND('',#5873,.T.) ;
#3816 = FACE_OUTER_BOUND('',#5874,.T.) ;
#3817 = FACE_OUTER_BOUND('',#5875,.T.) ;
#3818 = FACE_OUTER_BOUND('',#5876,.T.) ;
#3819 = FACE_OUTER_BOUND('',#5877,.T.) ;
#3820 = FACE_OUTER_BOUND('',#5878,.T.) ;
#3821 = FACE_OUTER_BOUND('',#5879,.T.) ;
#3822 = FACE_OUTER_BOUND('',#5880,.T.) ;
#3823 = FACE_OUTER_BOUND('',#5881,.T.) ;
#3824 = FACE_OUTER_BOUND('',#5882,.T.) ;
#3825 = FACE_OUTER_BOUND('',#5883,.T.) ;
#3826 = FACE_OUTER_BOUND('',#5884,.T.) ;
#3827 = FACE_OUTER_BOUND('',#5885,.T.) ;
#3828 = FACE_OUTER_BOUND('',#5886,.T.) ;
#3829 = FACE_OUTER_BOUND('',#5887,.T.) ;
#3830 = FACE_OUTER_BOUND('',#5888,.T.) ;
#3831 = FACE_OUTER_BOUND('',#5889,.T.) ;
#3832 = FACE_OUTER_BOUND('',#5890,.T.) ;
#3833 = FACE_OUTER_BOUND('',#5891,.T.) ;
#3834 = FACE_OUTER_BOUND('',#5892,.T.) ;
#3835 = FACE_OUTER_BOUND('',#5893,.T.) ;
#3836 = FACE_OUTER_BOUND('',#5894,.T.) ;
#3837 = FACE_OUTER_BOUND('',#5895,.T.) ;
#3838 = FACE_OUTER_BOUND('',#5896,.T.) ;
#3839 = FACE_OUTER_BOUND('',#5897,.T.) ;
#3840 = FACE_OUTER_BOUND('',#5898,.T.) ;
#3841 = FACE_OUTER_BOUND('',#5899,.T.) ;
#3842 = FACE_OUTER_BOUND('',#5900,.T.) ;
#3843 = FACE_OUTER_BOUND('',#5901,.T.) ;
#3844 = FACE_OUTER_BOUND('',#5902,.T.) ;
#3845 = FACE_OUTER_BOUND('',#5903,.T.) ;
#3846 = FACE_OUTER_BOUND('',#5904,.T.) ;
#3847 = FACE_OUTER_BOUND('',#5905,.T.) ;
#3848 = FACE_OUTER_BOUND('',#5906,.T.) ;
#3849 = FACE_OUTER_BOUND('',#5907,.T.) ;
#3850 = FACE_OUTER_BOUND('',#5908,.T.) ;
#3851 = FACE_OUTER_BOUND('',#5909,.T.) ;
#3852 = FACE_OUTER_BOUND('',#5910,.T.) ;
#3853 = FACE_OUTER_BOUND('',#5911,.T.) ;
#3854 = FACE_OUTER_BOUND('',#5912,.T.) ;
#3855 = FACE_OUTER_BOUND('',#5913,.T.) ;
#3856 = FACE_OUTER_BOUND('',#5914,.T.) ;
#3857 = FACE_OUTER_BOUND('',#5915,.T.) ;
#3858 = FACE_OUTER_BOUND('',#5916,.T.) ;
#3859 = FACE_OUTER_BOUND('',#5917,.T.) ;
#3860 = FACE_OUTER_BOUND('',#5918,.T.) ;
#3861 = FACE_OUTER_BOUND('',#5919,.T.) ;
#3862 = FACE_OUTER_BOUND('',#5920,.T.) ;
#3863 = FACE_OUTER_BOUND('',#5921,.T.) ;
#3864 = FACE_OUTER_BOUND('',#5922,.T.) ;
#3865 = FACE_OUTER_BOUND('',#5923,.T.) ;
#3866 = FACE_OUTER_BOUND('',#5924,.T.) ;
#3867 = FACE_OUTER_BOUND('',#5925,.T.) ;
#3868 = FACE_OUTER_BOUND('',#5926,.T.) ;
#3869 = FACE_OUTER_BOUND('',#5927,.T.) ;
#3870 = FACE_OUTER_BOUND('',#5928,.T.) ;
#3871 = FACE_OUTER_BOUND('',#5929,.T.) ;
#3872 = FACE_OUTER_BOUND('',#5930,.T.) ;
#3873 = FACE_OUTER_BOUND('',#5931,.T.) ;
#3874 = FACE_OUTER_BOUND('',#5932,.T.) ;
#3875 = FACE_OUTER_BOUND('',#5933,.T.) ;
#3876 = FACE_OUTER_BOUND('',#5934,.T.) ;
#3877 = FACE_OUTER_BOUND('',#5935,.T.) ;
#3878 = FACE_OUTER_BOUND('',#5936,.T.) ;
#3879 = FACE_OUTER_BOUND('',#5937,.T.) ;
#3880 = FACE_OUTER_BOUND('',#5938,.T.) ;
#3881 = FACE_OUTER_BOUND('',#5939,.T.) ;
#3882 = FACE_OUTER_BOUND('',#5940,.T.) ;
#3883 = FACE_OUTER_BOUND('',#5941,.T.) ;
#3884 = FACE_OUTER_BOUND('',#5942,.T.) ;
#3885 = FACE_OUTER_BOUND('',#5943,.T.) ;
#3886 = FACE_OUTER_BOUND('',#5944,.T.) ;
#3887 = FACE_OUTER_BOUND('',#5945,.T.) ;
#3888 = FACE_OUTER_BOUND('',#5946,.T.) ;
#3889 = FACE_OUTER_BOUND('',#5947,.T.) ;
#3890 = FACE_OUTER_BOUND('',#5948,.T.) ;
#3891 = FACE_OUTER_BOUND('',#5949,.T.) ;
#3892 = FACE_OUTER_BOUND('',#5950,.T.) ;
#3893 = FACE_OUTER_BOUND('',#5951,.T.) ;
#3894 = FACE_OUTER_BOUND('',#5952,.T.) ;
#3895 = FACE_OUTER_BOUND('',#5953,.T.) ;
#3896 = FACE_OUTER_BOUND('',#5954,.T.) ;
#3897 = FACE_OUTER_BOUND('',#5955,.T.) ;
#3898 = FACE_OUTER_BOUND('',#5956,.T.) ;
#3899 = FACE_OUTER_BOUND('',#5957,.T.) ;
#3900 = FACE_OUTER_BOUND('',#5958,.T.) ;
#3901 = FACE_OUTER_BOUND('',#5959,.T.) ;
#3902 = FACE_OUTER_BOUND('',#5961,.T.) ;
#3903 = FACE_OUTER_BOUND('',#5962,.T.) ;
#3904 = FACE_OUTER_BOUND('',#5963,.T.) ;
#3905 = FACE_OUTER_BOUND('',#5964,.T.) ;
#3906 = FACE_OUTER_BOUND('',#5965,.T.) ;
#3907 = FACE_OUTER_BOUND('',#5966,.T.) ;
#3908 = FACE_OUTER_BOUND('',#5967,.T.) ;
#3909 = FACE_OUTER_BOUND('',#5968,.T.) ;
#3910 = FACE_OUTER_BOUND('',#5969,.T.) ;
#3911 = FACE_OUTER_BOUND('',#5970,.T.) ;
#3912 = FACE_OUTER_BOUND('',#5971,.T.) ;
#3913 = FACE_OUTER_BOUND('',#5972,.T.) ;
#3914 = FACE_OUTER_BOUND('',#5973,.T.) ;
#3915 = FACE_OUTER_BOUND('',#5974,.T.) ;
#3916 = FACE_OUTER_BOUND('',#5975,.T.) ;
#3917 = FACE_OUTER_BOUND('',#5976,.T.) ;
#3918 = FACE_OUTER_BOUND('',#5977,.T.) ;
#3919 = FACE_OUTER_BOUND('',#5978,.T.) ;
#3920 = FACE_OUTER_BOUND('',#5979,.T.) ;
#3921 = FACE_OUTER_BOUND('',#5980,.T.) ;
#3922 = FACE_OUTER_BOUND('',#5981,.T.) ;
#3923 = FACE_OUTER_BOUND('',#5982,.T.) ;
#3924 = FACE_OUTER_BOUND('',#5983,.T.) ;
#3925 = FACE_OUTER_BOUND('',#5984,.T.) ;
#3926 = FACE_OUTER_BOUND('',#5985,.T.) ;
#3927 = FACE_OUTER_BOUND('',#5986,.T.) ;
#3928 = FACE_OUTER_BOUND('',#5987,.T.) ;
#3929 = FACE_OUTER_BOUND('',#5988,.T.) ;
#3930 = FACE_OUTER_BOUND('',#5989,.T.) ;
#3931 = FACE_OUTER_BOUND('',#5990,.T.) ;
#3932 = FACE_OUTER_BOUND('',#5991,.T.) ;
#3933 = FACE_OUTER_BOUND('',#5992,.T.) ;
#3934 = FACE_OUTER_BOUND('',#5993,.T.) ;
#3935 = FACE_OUTER_BOUND('',#5994,.T.) ;
#3936 = FACE_OUTER_BOUND('',#5995,.T.) ;
#3937 = FACE_OUTER_BOUND('',#5996,.T.) ;
#3938 = FACE_OUTER_BOUND('',#5997,.T.) ;
#3939 = FACE_OUTER_BOUND('',#5998,.T.) ;
#3940 = FACE_OUTER_BOUND('',#5999,.T.) ;
#3941 = FACE_OUTER_BOUND('',#6000,.T.) ;
#3942 = FACE_OUTER_BOUND('',#6001,.T.) ;
#3943 = FACE_OUTER_BOUND('',#6002,.T.) ;
#3944 = FACE_OUTER_BOUND('',#6003,.T.) ;
#3945 = FACE_OUTER_BOUND('',#6004,.T.) ;
#3946 = FACE_OUTER_BOUND('',#6005,.T.) ;
#3947 = FACE_OUTER_BOUND('',#6006,.T.) ;
#3948 = FACE_OUTER_BOUND('',#6007,.T.) ;
#3949 = FACE_OUTER_BOUND('',#6008,.T.) ;
#3950 = FACE_OUTER_BOUND('',#6009,.T.) ;
#3951 = FACE_OUTER_BOUND('',#6010,.T.) ;
#3952 = FACE_OUTER_BOUND('',#6011,.T.) ;
#3953 = FACE_OUTER_BOUND('',#6012,.T.) ;
#3954 = FACE_OUTER_BOUND('',#6013,.T.) ;
#3955 = FACE_OUTER_BOUND('',#6014,.T.) ;
#3956 = FACE_OUTER_BOUND('',#6016,.T.) ;
#3957 = FACE_OUTER_BOUND('',#6017,.T.) ;
#3958 = FACE_OUTER_BOUND('',#6018,.T.) ;
#3959 = FACE_OUTER_BOUND('',#6020,.T.) ;
#3960 = FACE_OUTER_BOUND('',#6021,.T.) ;
#3961 = FACE_OUTER_BOUND('',#6022,.T.) ;
#3962 = FACE_OUTER_BOUND('',#6023,.T.) ;
#3963 = FACE_OUTER_BOUND('',#6024,.T.) ;
#3964 = FACE_OUTER_BOUND('',#6025,.T.) ;
#3965 = FACE_OUTER_BOUND('',#6026,.T.) ;
#3966 = FACE_OUTER_BOUND('',#6027,.T.) ;
#3967 = FACE_OUTER_BOUND('',#6028,.T.) ;
#3968 = FACE_OUTER_BOUND('',#6030,.T.) ;
#3969 = FACE_OUTER_BOUND('',#6031,.T.) ;
#3970 = FACE_OUTER_BOUND('',#6032,.T.) ;
#3971 = FACE_OUTER_BOUND('',#6033,.T.) ;
#3972 = FACE_OUTER_BOUND('',#6034,.T.) ;
#3973 = FACE_OUTER_BOUND('',#6035,.T.) ;
#3974 = FACE_OUTER_BOUND('',#6036,.T.) ;
#3975 = FACE_OUTER_BOUND('',#6037,.T.) ;
#3976 = FACE_OUTER_BOUND('',#6038,.T.) ;
#3977 = FACE_OUTER_BOUND('',#6039,.T.) ;
#3978 = FACE_OUTER_BOUND('',#6040,.T.) ;
#3979 = FACE_OUTER_BOUND('',#6041,.T.) ;
#3980 = FACE_OUTER_BOUND('',#6042,.T.) ;
#3981 = FACE_OUTER_BOUND('',#6043,.T.) ;
#3982 = FACE_OUTER_BOUND('',#6044,.T.) ;
#3983 = FACE_OUTER_BOUND('',#6045,.T.) ;
#3984 = FACE_OUTER_BOUND('',#6046,.T.) ;
#3985 = FACE_OUTER_BOUND('',#6047,.T.) ;
#3986 = FACE_OUTER_BOUND('',#6048,.T.) ;
#3987 = FACE_OUTER_BOUND('',#6049,.T.) ;
#3988 = FACE_OUTER_BOUND('',#6050,.T.) ;
#3989 = FACE_OUTER_BOUND('',#6051,.T.) ;
#3990 = FACE_OUTER_BOUND('',#6052,.T.) ;
#3991 = FACE_OUTER_BOUND('',#6053,.T.) ;
#3992 = FACE_OUTER_BOUND('',#6054,.T.) ;
#3993 = FACE_OUTER_BOUND('',#6055,.T.) ;
#3994 = FACE_OUTER_BOUND('',#6056,.T.) ;
#3995 = FACE_OUTER_BOUND('',#6057,.T.) ;
#3996 = FACE_OUTER_BOUND('',#6058,.T.) ;
#3997 = FACE_OUTER_BOUND('',#6059,.T.) ;
#3998 = FACE_OUTER_BOUND('',#6060,.T.) ;
#3999 = FACE_OUTER_BOUND('',#6061,.T.) ;
#4000 = FACE_OUTER_BOUND('',#6062,.T.) ;
#4001 = FACE_OUTER_BOUND('',#6063,.T.) ;
#4002 = FACE_OUTER_BOUND('',#6064,.T.) ;
#4003 = FACE_OUTER_BOUND('',#6065,.T.) ;
#4004 = FACE_OUTER_BOUND('',#6066,.T.) ;
#4005 = FACE_OUTER_BOUND('',#6067,.T.) ;
#4006 = FACE_OUTER_BOUND('',#6068,.T.) ;
#4007 = FACE_OUTER_BOUND('',#6069,.T.) ;
#4008 = FACE_OUTER_BOUND('',#6070,.T.) ;
#4009 = FACE_OUTER_BOUND('',#6071,.T.) ;
#4010 = FACE_OUTER_BOUND('',#6072,.T.) ;
#4011 = FACE_OUTER_BOUND('',#6073,.T.) ;
#4012 = FACE_OUTER_BOUND('',#6074,.T.) ;
#4013 = FACE_OUTER_BOUND('',#6075,.T.) ;
#4014 = FACE_OUTER_BOUND('',#6076,.T.) ;
#4015 = FACE_OUTER_BOUND('',#6077,.T.) ;
#4016 = FACE_OUTER_BOUND('',#6078,.T.) ;
#4017 = FACE_OUTER_BOUND('',#6079,.T.) ;
#4018 = FACE_OUTER_BOUND('',#6080,.T.) ;
#4019 = FACE_OUTER_BOUND('',#6081,.T.) ;
#4020 = FACE_OUTER_BOUND('',#6082,.T.) ;
#4021 = FACE_OUTER_BOUND('',#6083,.T.) ;
#4022 = FACE_OUTER_BOUND('',#6084,.T.) ;
#4023 = FACE_OUTER_BOUND('',#6085,.T.) ;
#4024 = FACE_OUTER_BOUND('',#6086,.T.) ;
#4025 = FACE_OUTER_BOUND('',#6087,.T.) ;
#4026 = FACE_OUTER_BOUND('',#6088,.T.) ;
#4027 = FACE_OUTER_BOUND('',#6089,.T.) ;
#4028 = FACE_OUTER_BOUND('',#6090,.T.) ;
#4029 = FACE_OUTER_BOUND('',#6091,.T.) ;
#4030 = FACE_OUTER_BOUND('',#6092,.T.) ;
#4031 = FACE_OUTER_BOUND('',#6093,.T.) ;
#4032 = FACE_OUTER_BOUND('',#6094,.T.) ;
#4033 = FACE_OUTER_BOUND('',#6095,.T.) ;
#4034 = FACE_OUTER_BOUND('',#6096,.T.) ;
#4035 = FACE_OUTER_BOUND('',#6097,.T.) ;
#4036 = FACE_OUTER_BOUND('',#6098,.T.) ;
#4037 = FACE_OUTER_BOUND('',#6099,.T.) ;
#4038 = FACE_OUTER_BOUND('',#6100,.T.) ;
#4039 = FACE_OUTER_BOUND('',#6101,.T.) ;
#4040 = FACE_OUTER_BOUND('',#6102,.T.) ;
#4041 = FACE_OUTER_BOUND('',#6104,.T.) ;
#4042 = FACE_OUTER_BOUND('',#6105,.T.) ;
#4043 = FACE_OUTER_BOUND('',#6106,.T.) ;
#4044 = FACE_OUTER_BOUND('',#6107,.T.) ;
#4045 = FACE_OUTER_BOUND('',#6108,.T.) ;
#4046 = FACE_OUTER_BOUND('',#6109,.T.) ;
#4047 = FACE_OUTER_BOUND('',#6110,.T.) ;
#4048 = FACE_OUTER_BOUND('',#6111,.T.) ;
#4049 = FACE_OUTER_BOUND('',#6112,.T.) ;
#4050 = FACE_OUTER_BOUND('',#6113,.T.) ;
#4051 = FACE_OUTER_BOUND('',#6114,.T.) ;
#4052 = FACE_OUTER_BOUND('',#6115,.T.) ;
#4053 = FACE_OUTER_BOUND('',#6116,.T.) ;
#4054 = FACE_OUTER_BOUND('',#6117,.T.) ;
#4055 = FACE_OUTER_BOUND('',#6118,.T.) ;
#4056 = FACE_OUTER_BOUND('',#6119,.T.) ;
#4057 = FACE_OUTER_BOUND('',#6120,.T.) ;
#4058 = FACE_OUTER_BOUND('',#6121,.T.) ;
#4059 = FACE_OUTER_BOUND('',#6122,.T.) ;
#4060 = FACE_OUTER_BOUND('',#6123,.T.) ;
#4061 = FACE_OUTER_BOUND('',#6124,.T.) ;
#4062 = FACE_OUTER_BOUND('',#6125,.T.) ;
#4063 = FACE_OUTER_BOUND('',#6126,.T.) ;
#4064 = FACE_OUTER_BOUND('',#6127,.T.) ;
#4065 = FACE_OUTER_BOUND('',#6128,.T.) ;
#4066 = FACE_OUTER_BOUND('',#6129,.T.) ;
#4067 = FACE_OUTER_BOUND('',#6130,.T.) ;
#4068 = FACE_OUTER_BOUND('',#6131,.T.) ;
#4069 = FACE_OUTER_BOUND('',#6132,.T.) ;
#4070 = FACE_OUTER_BOUND('',#6133,.T.) ;
#4071 = FACE_OUTER_BOUND('',#6139,.T.) ;
#4072 = FACE_OUTER_BOUND('',#6145,.T.) ;
#4073 = FACE_OUTER_BOUND('',#6146,.T.) ;
#4074 = FACE_OUTER_BOUND('',#6147,.T.) ;
#4075 = FACE_OUTER_BOUND('',#6148,.T.) ;
#4076 = FACE_OUTER_BOUND('',#6149,.T.) ;
#4077 = FACE_OUTER_BOUND('',#6150,.T.) ;
#4078 = FACE_OUTER_BOUND('',#6151,.T.) ;
#4079 = FACE_OUTER_BOUND('',#6152,.T.) ;
#4080 = FACE_OUTER_BOUND('',#6153,.T.) ;
#4081 = FACE_OUTER_BOUND('',#6154,.T.) ;
#4082 = FACE_OUTER_BOUND('',#6155,.T.) ;
#4083 = FACE_OUTER_BOUND('',#6156,.T.) ;
#4084 = FACE_OUTER_BOUND('',#6157,.T.) ;
#4085 = FACE_OUTER_BOUND('',#6158,.T.) ;
#4086 = FACE_OUTER_BOUND('',#6159,.T.) ;
#4087 = FACE_OUTER_BOUND('',#6160,.T.) ;
#4088 = FACE_OUTER_BOUND('',#6161,.T.) ;
#4089 = FACE_OUTER_BOUND('',#6162,.T.) ;
#4090 = FACE_OUTER_BOUND('',#6163,.T.) ;
#4091 = FACE_OUTER_BOUND('',#6164,.T.) ;
#4092 = FACE_OUTER_BOUND('',#6165,.T.) ;
#4093 = FACE_OUTER_BOUND('',#6166,.T.) ;
#4094 = FACE_OUTER_BOUND('',#6167,.T.) ;
#4095 = FACE_OUTER_BOUND('',#6168,.T.) ;
#4096 = FACE_OUTER_BOUND('',#6169,.T.) ;
#4097 = FACE_OUTER_BOUND('',#6170,.T.) ;
#4098 = FACE_OUTER_BOUND('',#6171,.T.) ;
#4099 = FACE_OUTER_BOUND('',#6172,.T.) ;
#4100 = FACE_OUTER_BOUND('',#6173,.T.) ;
#4101 = FACE_OUTER_BOUND('',#6174,.T.) ;
#4102 = FACE_OUTER_BOUND('',#6175,.T.) ;
#4103 = FACE_OUTER_BOUND('',#6176,.T.) ;
#4104 = FACE_OUTER_BOUND('',#6177,.T.) ;
#4105 = FACE_OUTER_BOUND('',#6178,.T.) ;
#4106 = FACE_OUTER_BOUND('',#6179,.T.) ;
#4107 = FACE_OUTER_BOUND('',#6180,.T.) ;
#4108 = FACE_OUTER_BOUND('',#6181,.T.) ;
#4109 = FACE_OUTER_BOUND('',#6182,.T.) ;
#4110 = FACE_OUTER_BOUND('',#6183,.T.) ;
#4111 = FACE_OUTER_BOUND('',#6184,.T.) ;
#4112 = FACE_OUTER_BOUND('',#6185,.T.) ;
#4113 = FACE_OUTER_BOUND('',#6186,.T.) ;
#4114 = FACE_OUTER_BOUND('',#6187,.T.) ;
#4115 = FACE_OUTER_BOUND('',#6188,.T.) ;
#4116 = FACE_OUTER_BOUND('',#6189,.T.) ;
#4117 = FACE_OUTER_BOUND('',#6190,.T.) ;
#4118 = FACE_OUTER_BOUND('',#6191,.T.) ;
#4119 = FACE_OUTER_BOUND('',#6192,.T.) ;
#4120 = FACE_OUTER_BOUND('',#6194,.T.) ;
#4121 = FACE_OUTER_BOUND('',#6195,.T.) ;
#4122 = FACE_OUTER_BOUND('',#6196,.T.) ;
#4123 = FACE_OUTER_BOUND('',#6198,.T.) ;
#4124 = FACE_OUTER_BOUND('',#6199,.T.) ;
#4125 = FACE_OUTER_BOUND('',#6200,.T.) ;
#4126 = FACE_OUTER_BOUND('',#6201,.T.) ;
#4127 = FACE_OUTER_BOUND('',#6202,.T.) ;
#4128 = FACE_OUTER_BOUND('',#6203,.T.) ;
#4129 = FACE_OUTER_BOUND('',#6204,.T.) ;
#4130 = FACE_OUTER_BOUND('',#6205,.T.) ;
#4131 = FACE_OUTER_BOUND('',#6206,.T.) ;
#4132 = FACE_OUTER_BOUND('',#6207,.T.) ;
#4133 = FACE_OUTER_BOUND('',#6208,.T.) ;
#4134 = FACE_OUTER_BOUND('',#6209,.T.) ;
#4135 = FACE_OUTER_BOUND('',#6210,.T.) ;
#4136 = FACE_OUTER_BOUND('',#6211,.T.) ;
#4137 = FACE_OUTER_BOUND('',#6212,.T.) ;
#4138 = FACE_OUTER_BOUND('',#6213,.T.) ;
#4139 = FACE_OUTER_BOUND('',#6214,.T.) ;
#4140 = FACE_OUTER_BOUND('',#6215,.T.) ;
#4141 = FACE_OUTER_BOUND('',#6216,.T.) ;
#4142 = FACE_OUTER_BOUND('',#6217,.T.) ;
#4143 = FACE_OUTER_BOUND('',#6218,.T.) ;
#4144 = FACE_OUTER_BOUND('',#6219,.T.) ;
#4145 = FACE_OUTER_BOUND('',#6220,.T.) ;
#4146 = FACE_OUTER_BOUND('',#6221,.T.) ;
#4147 = FACE_OUTER_BOUND('',#6222,.T.) ;
#4148 = FACE_OUTER_BOUND('',#6223,.T.) ;
#4149 = FACE_OUTER_BOUND('',#6224,.T.) ;
#4150 = FACE_OUTER_BOUND('',#6225,.T.) ;
#4151 = FACE_OUTER_BOUND('',#6226,.T.) ;
#4152 = FACE_OUTER_BOUND('',#6227,.T.) ;
#4153 = FACE_OUTER_BOUND('',#6228,.T.) ;
#4154 = FACE_OUTER_BOUND('',#6229,.T.) ;
#4155 = FACE_OUTER_BOUND('',#6231,.T.) ;
#4156 = FACE_OUTER_BOUND('',#6232,.T.) ;
#4157 = FACE_OUTER_BOUND('',#6234,.T.) ;
#4158 = EDGE_LOOP('',(#20380,#20381,#20382,#20383)) ;
#4159 = EDGE_LOOP('',(#20384,#20385,#20386,#20387,#20388,#20389)) ;
#4160 = EDGE_LOOP('',(#20390,#20391,#20392,#20393)) ;
#4161 = EDGE_LOOP('',(#20394,#20395,#20396,#20397)) ;
#4162 = EDGE_LOOP('',(#20398,#20399,#20400,#20401)) ;
#4163 = EDGE_LOOP('',(#20402,#20403,#20404,#20405)) ;
#4164 = EDGE_LOOP('',(#20406,#20407,#20408,#20409)) ;
#4165 = EDGE_LOOP('',(#20410,#20411,#20412,#20413)) ;
#4166 = EDGE_LOOP('',(#20414,#20415,#20416,#20417)) ;
#4167 = EDGE_LOOP('',(#20418,#20419,#20420,#20421)) ;
#4168 = EDGE_LOOP('',(#20422,#20423,#20424,#20425)) ;
#4169 = EDGE_LOOP('',(#20426,#20427,#20428,#20429)) ;
#4170 = EDGE_LOOP('',(#20430)) ;
#4171 = EDGE_LOOP('',(#20431)) ;
#4172 = EDGE_LOOP('',(#20432)) ;
#4173 = EDGE_LOOP('',(#20433)) ;
#4174 = EDGE_LOOP('',(#20434)) ;
#4175 = EDGE_LOOP('',(#20435)) ;
#4176 = EDGE_LOOP('',(#20436,#20437,#20438,#20439)) ;
#4177 = EDGE_LOOP('',(#20440,#20441,#20442,#20443)) ;
#4178 = EDGE_LOOP('',(#20444,#20445,#20446,#20447)) ;
#4179 = EDGE_LOOP('',(#20448,#20449,#20450,#20451)) ;
#4180 = EDGE_LOOP('',(#20452,#20453,#20454,#20455)) ;
#4181 = EDGE_LOOP('',(#20456,#20457,#20458,#20459)) ;
#4182 = EDGE_LOOP('',(#20460,#20461,#20462,#20463,#20464,#20465,#20466,#20467,
#20468,#20469,#20470,#20471,#20472,#20473,#20474,#20475,#20476,#20477)) ;
#4183 = EDGE_LOOP('',(#20478)) ;
#4184 = EDGE_LOOP('',(#20479)) ;
#4185 = EDGE_LOOP('',(#20480,#20481,#20482,#20483)) ;
#4186 = EDGE_LOOP('',(#20484,#20485,#20486,#20487,#20488,#20489,#20490,#20491)) ;
#4187 = EDGE_LOOP('',(#20492,#20493,#20494,#20495,#20496,#20497,#20498,#20499,
#20500,#20501,#20502,#20503,#20504,#20505,#20506,#20507,#20508,#20509)) ;
#4188 = EDGE_LOOP('',(#20510)) ;
#4189 = EDGE_LOOP('',(#20511)) ;
#4190 = EDGE_LOOP('',(#20512,#20513,#20514,#20515)) ;
#4191 = EDGE_LOOP('',(#20516,#20517,#20518,#20519,#20520,#20521,#20522)) ;
#4192 = EDGE_LOOP('',(#20523,#20524,#20525,#20526,#20527,#20528,#20529,#20530,
#20531,#20532,#20533,#20534,#20535,#20536,#20537,#20538,#20539,#20540)) ;
#4193 = EDGE_LOOP('',(#20541)) ;
#4194 = EDGE_LOOP('',(#20542)) ;
#4195 = EDGE_LOOP('',(#20543,#20544,#20545,#20546)) ;
#4196 = EDGE_LOOP('',(#20547,#20548,#20549,#20550)) ;
#4197 = EDGE_LOOP('',(#20551,#20552,#20553,#20554)) ;
#4198 = EDGE_LOOP('',(#20555,#20556,#20557,#20558)) ;
#4199 = EDGE_LOOP('',(#20559,#20560,#20561,#20562)) ;
#4200 = EDGE_LOOP('',(#20563,#20564,#20565,#20566,#20567,#20568,#20569)) ;
#4201 = EDGE_LOOP('',(#20570,#20571,#20572,#20573,#20574,#20575,#20576,#20577,
#20578,#20579,#20580,#20581)) ;
#4202 = EDGE_LOOP('',(#20582,#20583,#20584,#20585)) ;
#4203 = EDGE_LOOP('',(#20586)) ;
#4204 = EDGE_LOOP('',(#20587)) ;
#4205 = EDGE_LOOP('',(#20588,#20589,#20590,#20591)) ;
#4206 = EDGE_LOOP('',(#20592,#20593,#20594,#20595)) ;
#4207 = EDGE_LOOP('',(#20596,#20597,#20598,#20599)) ;
#4208 = EDGE_LOOP('',(#20600,#20601,#20602,#20603)) ;
#4209 = EDGE_LOOP('',(#20604,#20605,#20606,#20607)) ;
#4210 = EDGE_LOOP('',(#20608,#20609,#20610,#20611)) ;
#4211 = EDGE_LOOP('',(#20612)) ;
#4212 = EDGE_LOOP('',(#20613)) ;
#4213 = EDGE_LOOP('',(#20614)) ;
#4214 = EDGE_LOOP('',(#20615)) ;
#4215 = EDGE_LOOP('',(#20616,#20617,#20618,#20619)) ;
#4216 = EDGE_LOOP('',(#20620,#20621,#20622,#20623)) ;
#4217 = EDGE_LOOP('',(#20624,#20625,#20626,#20627)) ;
#4218 = EDGE_LOOP('',(#20628,#20629,#20630,#20631)) ;
#4219 = EDGE_LOOP('',(#20632,#20633,#20634,#20635)) ;
#4220 = EDGE_LOOP('',(#20636,#20637,#20638,#20639)) ;
#4221 = EDGE_LOOP('',(#20640,#20641,#20642,#20643)) ;
#4222 = EDGE_LOOP('',(#20644,#20645,#20646,#20647,#20648,#20649,#20650,#20651,
#20652,#20653,#20654,#20655,#20656,#20657,#20658,#20659,#20660,#20661)) ;
#4223 = EDGE_LOOP('',(#20662)) ;
#4224 = EDGE_LOOP('',(#20663)) ;
#4225 = EDGE_LOOP('',(#20664,#20665,#20666,#20667,#20668,#20669)) ;
#4226 = EDGE_LOOP('',(#20670,#20671,#20672,#20673)) ;
#4227 = EDGE_LOOP('',(#20674,#20675,#20676,#20677)) ;
#4228 = EDGE_LOOP('',(#20678,#20679,#20680,#20681)) ;
#4229 = EDGE_LOOP('',(#20682,#20683,#20684,#20685)) ;
#4230 = EDGE_LOOP('',(#20686,#20687,#20688,#20689)) ;
#4231 = EDGE_LOOP('',(#20690,#20691,#20692,#20693)) ;
#4232 = EDGE_LOOP('',(#20694,#20695,#20696,#20697)) ;
#4233 = EDGE_LOOP('',(#20698,#20699,#20700,#20701)) ;
#4234 = EDGE_LOOP('',(#20702,#20703,#20704,#20705)) ;
#4235 = EDGE_LOOP('',(#20706,#20707,#20708,#20709)) ;
#4236 = EDGE_LOOP('',(#20710,#20711,#20712,#20713)) ;
#4237 = EDGE_LOOP('',(#20714,#20715,#20716,#20717)) ;
#4238 = EDGE_LOOP('',(#20718,#20719,#20720,#20721)) ;
#4239 = EDGE_LOOP('',(#20722,#20723,#20724,#20725)) ;
#4240 = EDGE_LOOP('',(#20726,#20727,#20728,#20729)) ;
#4241 = EDGE_LOOP('',(#20730,#20731,#20732,#20733,#20734,#20735,#20736)) ;
#4242 = EDGE_LOOP('',(#20737,#20738,#20739,#20740)) ;
#4243 = EDGE_LOOP('',(#20741,#20742,#20743,#20744)) ;
#4244 = EDGE_LOOP('',(#20745,#20746,#20747,#20748)) ;
#4245 = EDGE_LOOP('',(#20749,#20750,#20751,#20752,#20753,#20754)) ;
#4246 = EDGE_LOOP('',(#20755,#20756,#20757,#20758)) ;
#4247 = EDGE_LOOP('',(#20759,#20760,#20761,#20762,#20763,#20764,#20765)) ;
#4248 = EDGE_LOOP('',(#20766,#20767,#20768,#20769)) ;
#4249 = EDGE_LOOP('',(#20770,#20771,#20772,#20773,#20774,#20775,#20776)) ;
#4250 = EDGE_LOOP('',(#20777,#20778,#20779,#20780)) ;
#4251 = EDGE_LOOP('',(#20781,#20782,#20783,#20784)) ;
#4252 = EDGE_LOOP('',(#20785,#20786,#20787,#20788)) ;
#4253 = EDGE_LOOP('',(#20789,#20790,#20791,#20792)) ;
#4254 = EDGE_LOOP('',(#20793,#20794,#20795,#20796)) ;
#4255 = EDGE_LOOP('',(#20797,#20798,#20799,#20800)) ;
#4256 = EDGE_LOOP('',(#20801,#20802,#20803,#20804)) ;
#4257 = EDGE_LOOP('',(#20805,#20806,#20807,#20808)) ;
#4258 = EDGE_LOOP('',(#20809,#20810,#20811,#20812)) ;
#4259 = EDGE_LOOP('',(#20813,#20814,#20815,#20816)) ;
#4260 = EDGE_LOOP('',(#20817,#20818,#20819,#20820)) ;
#4261 = EDGE_LOOP('',(#20821,#20822,#20823,#20824)) ;
#4262 = EDGE_LOOP('',(#20825,#20826,#20827,#20828)) ;
#4263 = EDGE_LOOP('',(#20829,#20830,#20831,#20832)) ;
#4264 = EDGE_LOOP('',(#20833,#20834,#20835,#20836)) ;
#4265 = EDGE_LOOP('',(#20837,#20838,#20839,#20840)) ;
#4266 = EDGE_LOOP('',(#20841,#20842,#20843,#20844)) ;
#4267 = EDGE_LOOP('',(#20845,#20846,#20847,#20848)) ;
#4268 = EDGE_LOOP('',(#20849,#20850,#20851,#20852)) ;
#4269 = EDGE_LOOP('',(#20853,#20854,#20855,#20856)) ;
#4270 = EDGE_LOOP('',(#20857,#20858,#20859,#20860)) ;
#4271 = EDGE_LOOP('',(#20861,#20862,#20863,#20864)) ;
#4272 = EDGE_LOOP('',(#20865,#20866,#20867,#20868,#20869,#20870,#20871)) ;
#4273 = EDGE_LOOP('',(#20872,#20873,#20874,#20875,#20876,#20877,#20878,#20879)) ;
#4274 = EDGE_LOOP('',(#20880,#20881,#20882,#20883)) ;
#4275 = EDGE_LOOP('',(#20884,#20885,#20886,#20887)) ;
#4276 = EDGE_LOOP('',(#20888,#20889,#20890,#20891)) ;
#4277 = EDGE_LOOP('',(#20892,#20893,#20894,#20895)) ;
#4278 = EDGE_LOOP('',(#20896,#20897,#20898,#20899)) ;
#4279 = EDGE_LOOP('',(#20900,#20901,#20902,#20903)) ;
#4280 = EDGE_LOOP('',(#20904,#20905,#20906,#20907)) ;
#4281 = EDGE_LOOP('',(#20908,#20909,#20910,#20911)) ;
#4282 = EDGE_LOOP('',(#20912,#20913,#20914,#20915)) ;
#4283 = EDGE_LOOP('',(#20916,#20917,#20918,#20919)) ;
#4284 = EDGE_LOOP('',(#20920,#20921,#20922,#20923)) ;
#4285 = EDGE_LOOP('',(#20924,#20925,#20926,#20927)) ;
#4286 = EDGE_LOOP('',(#20928,#20929,#20930,#20931)) ;
#4287 = EDGE_LOOP('',(#20932,#20933,#20934,#20935,#20936,#20937)) ;
#4288 = EDGE_LOOP('',(#20938,#20939,#20940,#20941)) ;
#4289 = EDGE_LOOP('',(#20942,#20943,#20944,#20945)) ;
#4290 = EDGE_LOOP('',(#20946,#20947,#20948,#20949)) ;
#4291 = EDGE_LOOP('',(#20950,#20951,#20952,#20953)) ;
#4292 = EDGE_LOOP('',(#20954,#20955,#20956,#20957)) ;
#4293 = EDGE_LOOP('',(#20958,#20959,#20960,#20961)) ;
#4294 = EDGE_LOOP('',(#20962,#20963,#20964,#20965)) ;
#4295 = EDGE_LOOP('',(#20966,#20967,#20968,#20969)) ;
#4296 = EDGE_LOOP('',(#20970,#20971,#20972,#20973)) ;
#4297 = EDGE_LOOP('',(#20974,#20975,#20976,#20977)) ;
#4298 = EDGE_LOOP('',(#20978,#20979,#20980,#20981)) ;
#4299 = EDGE_LOOP('',(#20982,#20983,#20984,#20985)) ;
#4300 = EDGE_LOOP('',(#20986,#20987,#20988,#20989)) ;
#4301 = EDGE_LOOP('',(#20990,#20991,#20992,#20993)) ;
#4302 = EDGE_LOOP('',(#20994,#20995,#20996,#20997)) ;
#4303 = EDGE_LOOP('',(#20998,#20999,#21000,#21001)) ;
#4304 = EDGE_LOOP('',(#21002,#21003,#21004,#21005)) ;
#4305 = EDGE_LOOP('',(#21006,#21007,#21008,#21009)) ;
#4306 = EDGE_LOOP('',(#21010,#21011,#21012,#21013)) ;
#4307 = EDGE_LOOP('',(#21014,#21015,#21016,#21017)) ;
#4308 = EDGE_LOOP('',(#21018,#21019,#21020,#21021)) ;
#4309 = EDGE_LOOP('',(#21022,#21023,#21024,#21025)) ;
#4310 = EDGE_LOOP('',(#21026,#21027,#21028,#21029)) ;
#4311 = EDGE_LOOP('',(#21030,#21031,#21032,#21033)) ;
#4312 = EDGE_LOOP('',(#21034,#21035,#21036,#21037)) ;
#4313 = EDGE_LOOP('',(#21038,#21039,#21040,#21041)) ;
#4314 = EDGE_LOOP('',(#21042,#21043,#21044,#21045)) ;
#4315 = EDGE_LOOP('',(#21046,#21047,#21048,#21049)) ;
#4316 = EDGE_LOOP('',(#21050,#21051,#21052,#21053)) ;
#4317 = EDGE_LOOP('',(#21054,#21055,#21056,#21057,#21058,#21059)) ;
#4318 = EDGE_LOOP('',(#21060,#21061,#21062,#21063)) ;
#4319 = EDGE_LOOP('',(#21064,#21065,#21066,#21067)) ;
#4320 = EDGE_LOOP('',(#21068,#21069,#21070,#21071)) ;
#4321 = EDGE_LOOP('',(#21072,#21073,#21074,#21075)) ;
#4322 = EDGE_LOOP('',(#21076,#21077,#21078,#21079)) ;
#4323 = EDGE_LOOP('',(#21080,#21081,#21082,#21083)) ;
#4324 = EDGE_LOOP('',(#21084,#21085,#21086,#21087)) ;
#4325 = EDGE_LOOP('',(#21088,#21089,#21090,#21091)) ;
#4326 = EDGE_LOOP('',(#21092,#21093,#21094,#21095)) ;
#4327 = EDGE_LOOP('',(#21096,#21097,#21098,#21099)) ;
#4328 = EDGE_LOOP('',(#21100,#21101,#21102,#21103)) ;
#4329 = EDGE_LOOP('',(#21104,#21105,#21106,#21107)) ;
#4330 = EDGE_LOOP('',(#21108,#21109,#21110,#21111)) ;
#4331 = EDGE_LOOP('',(#21112,#21113,#21114,#21115)) ;
#4332 = EDGE_LOOP('',(#21116,#21117,#21118,#21119)) ;
#4333 = EDGE_LOOP('',(#21120,#21121,#21122,#21123)) ;
#4334 = EDGE_LOOP('',(#21124,#21125,#21126,#21127)) ;
#4335 = EDGE_LOOP('',(#21128,#21129,#21130,#21131)) ;
#4336 = EDGE_LOOP('',(#21132,#21133,#21134,#21135)) ;
#4337 = EDGE_LOOP('',(#21136,#21137,#21138,#21139)) ;
#4338 = EDGE_LOOP('',(#21140,#21141,#21142,#21143)) ;
#4339 = EDGE_LOOP('',(#21144,#21145,#21146,#21147)) ;
#4340 = EDGE_LOOP('',(#21148,#21149,#21150,#21151)) ;
#4341 = EDGE_LOOP('',(#21152,#21153,#21154,#21155)) ;
#4342 = EDGE_LOOP('',(#21156,#21157,#21158,#21159)) ;
#4343 = EDGE_LOOP('',(#21160,#21161,#21162,#21163)) ;
#4344 = EDGE_LOOP('',(#21164,#21165,#21166,#21167)) ;
#4345 = EDGE_LOOP('',(#21168,#21169,#21170,#21171)) ;
#4346 = EDGE_LOOP('',(#21172,#21173,#21174,#21175)) ;
#4347 = EDGE_LOOP('',(#21176,#21177,#21178)) ;
#4348 = EDGE_LOOP('',(#21179,#21180,#21181,#21182)) ;
#4349 = EDGE_LOOP('',(#21183,#21184,#21185,#21186)) ;
#4350 = EDGE_LOOP('',(#21187,#21188,#21189,#21190)) ;
#4351 = EDGE_LOOP('',(#21191,#21192,#21193)) ;
#4352 = EDGE_LOOP('',(#21194,#21195,#21196)) ;
#4353 = EDGE_LOOP('',(#21197,#21198,#21199,#21200,#21201,#21202,#21203,#21204,
#21205,#21206,#21207,#21208,#21209,#21210,#21211,#21212)) ;
#4354 = EDGE_LOOP('',(#21213,#21214,#21215,#21216,#21217,#21218,#21219,#21220,
#21221,#21222,#21223,#21224,#21225,#21226,#21227,#21228,#21229)) ;
#4355 = EDGE_LOOP('',(#21230,#21231,#21232,#21233,#21234,#21235)) ;
#4356 = EDGE_LOOP('',(#21236,#21237)) ;
#4357 = EDGE_LOOP('',(#21238,#21239,#21240,#21241,#21242,#21243)) ;
#4358 = EDGE_LOOP('',(#21244,#21245,#21246,#21247,#21248,#21249)) ;
#4359 = EDGE_LOOP('',(#21250,#21251,#21252,#21253,#21254,#21255)) ;
#4360 = EDGE_LOOP('',(#21256,#21257,#21258,#21259,#21260,#21261)) ;
#4361 = EDGE_LOOP('',(#21262,#21263,#21264,#21265,#21266,#21267)) ;
#4362 = EDGE_LOOP('',(#21268,#21269,#21270,#21271,#21272,#21273)) ;
#4363 = EDGE_LOOP('',(#21274,#21275,#21276,#21277,#21278,#21279)) ;
#4364 = EDGE_LOOP('',(#21280,#21281)) ;
#4365 = EDGE_LOOP('',(#21282,#21283,#21284)) ;
#4366 = EDGE_LOOP('',(#21285,#21286,#21287)) ;
#4367 = EDGE_LOOP('',(#21288,#21289,#21290)) ;
#4368 = EDGE_LOOP('',(#21291,#21292,#21293)) ;
#4369 = EDGE_LOOP('',(#21294,#21295,#21296)) ;
#4370 = EDGE_LOOP('',(#21297,#21298,#21299)) ;
#4371 = EDGE_LOOP('',(#21300,#21301,#21302)) ;
#4372 = EDGE_LOOP('',(#21303,#21304,#21305)) ;
#4373 = EDGE_LOOP('',(#21306,#21307,#21308)) ;
#4374 = EDGE_LOOP('',(#21309,#21310,#21311)) ;
#4375 = EDGE_LOOP('',(#21312,#21313,#21314)) ;
#4376 = EDGE_LOOP('',(#21315,#21316,#21317,#21318,#21319)) ;
#4377 = EDGE_LOOP('',(#21320,#21321,#21322,#21323)) ;
#4378 = EDGE_LOOP('',(#21324,#21325,#21326,#21327)) ;
#4379 = EDGE_LOOP('',(#21328,#21329,#21330,#21331)) ;
#4380 = EDGE_LOOP('',(#21332,#21333,#21334,#21335)) ;
#4381 = EDGE_LOOP('',(#21336,#21337,#21338,#21339,#21340,#21341,#21342,#21343,
#21344)) ;
#4382 = EDGE_LOOP('',(#21345,#21346,#21347,#21348)) ;
#4383 = EDGE_LOOP('',(#21349,#21350,#21351,#21352)) ;
#4384 = EDGE_LOOP('',(#21353,#21354,#21355,#21356)) ;
#4385 = EDGE_LOOP('',(#21357,#21358,#21359,#21360)) ;
#4386 = EDGE_LOOP('',(#21361,#21362,#21363,#21364)) ;
#4387 = EDGE_LOOP('',(#21365,#21366,#21367,#21368)) ;
#4388 = EDGE_LOOP('',(#21369,#21370,#21371,#21372,#21373)) ;
#4389 = EDGE_LOOP('',(#21374,#21375,#21376,#21377,#21378,#21379)) ;
#4390 = EDGE_LOOP('',(#21380)) ;
#4391 = EDGE_LOOP('',(#21381,#21382,#21383,#21384,#21385,#21386,#21387,#21388,
#21389,#21390,#21391,#21392,#21393,#21394,#21395,#21396,#21397,#21398,#21399,
#21400)) ;
#4392 = EDGE_LOOP('',(#21401,#21402,#21403,#21404,#21405,#21406,#21407,#21408)) ;
#4393 = EDGE_LOOP('',(#21409,#21410,#21411,#21412,#21413,#21414,#21415,#21416,
#21417,#21418,#21419,#21420,#21421,#21422,#21423,#21424,#21425,#21426,#21427,
#21428,#21429,#21430,#21431)) ;
#4394 = EDGE_LOOP('',(#21432,#21433,#21434,#21435)) ;
#4395 = EDGE_LOOP('',(#21436,#21437,#21438,#21439)) ;
#4396 = EDGE_LOOP('',(#21440,#21441,#21442,#21443)) ;
#4397 = EDGE_LOOP('',(#21444,#21445,#21446,#21447)) ;
#4398 = EDGE_LOOP('',(#21448,#21449,#21450,#21451)) ;
#4399 = EDGE_LOOP('',(#21452,#21453,#21454,#21455)) ;
#4400 = EDGE_LOOP('',(#21456,#21457,#21458,#21459)) ;
#4401 = EDGE_LOOP('',(#21460,#21461,#21462,#21463)) ;
#4402 = EDGE_LOOP('',(#21464,#21465,#21466,#21467)) ;
#4403 = EDGE_LOOP('',(#21468,#21469,#21470,#21471)) ;
#4404 = EDGE_LOOP('',(#21472,#21473,#21474,#21475)) ;
#4405 = EDGE_LOOP('',(#21476,#21477,#21478,#21479)) ;
#4406 = EDGE_LOOP('',(#21480,#21481,#21482,#21483)) ;
#4407 = EDGE_LOOP('',(#21484,#21485,#21486,#21487)) ;
#4408 = EDGE_LOOP('',(#21488,#21489,#21490,#21491,#21492)) ;
#4409 = EDGE_LOOP('',(#21493,#21494,#21495,#21496)) ;
#4410 = EDGE_LOOP('',(#21497,#21498,#21499,#21500)) ;
#4411 = EDGE_LOOP('',(#21501,#21502,#21503,#21504)) ;
#4412 = EDGE_LOOP('',(#21505,#21506,#21507,#21508)) ;
#4413 = EDGE_LOOP('',(#21509,#21510,#21511,#21512)) ;
#4414 = EDGE_LOOP('',(#21513,#21514,#21515,#21516,#21517,#21518)) ;
#4415 = EDGE_LOOP('',(#21519)) ;
#4416 = EDGE_LOOP('',(#21520,#21521,#21522,#21523,#21524,#21525,#21526,#21527,
#21528,#21529,#21530,#21531,#21532,#21533,#21534,#21535)) ;
#4417 = EDGE_LOOP('',(#21536,#21537,#21538,#21539,#21540,#21541,#21542,#21543,
#21544,#21545,#21546,#21547,#21548,#21549)) ;
#4418 = EDGE_LOOP('',(#21550,#21551,#21552,#21553)) ;
#4419 = EDGE_LOOP('',(#21554,#21555,#21556,#21557,#21558)) ;
#4420 = EDGE_LOOP('',(#21559,#21560,#21561,#21562,#21563)) ;
#4421 = EDGE_LOOP('',(#21564,#21565,#21566,#21567)) ;
#4422 = EDGE_LOOP('',(#21568,#21569,#21570,#21571,#21572,#21573)) ;
#4423 = EDGE_LOOP('',(#21574,#21575,#21576,#21577,#21578,#21579,#21580)) ;
#4424 = EDGE_LOOP('',(#21581,#21582,#21583,#21584)) ;
#4425 = EDGE_LOOP('',(#21585,#21586,#21587,#21588,#21589)) ;
#4426 = EDGE_LOOP('',(#21590,#21591,#21592,#21593,#21594,#21595)) ;
#4427 = EDGE_LOOP('',(#21596,#21597,#21598,#21599)) ;
#4428 = EDGE_LOOP('',(#21600,#21601,#21602,#21603,#21604)) ;
#4429 = EDGE_LOOP('',(#21605,#21606,#21607,#21608,#21609)) ;
#4430 = EDGE_LOOP('',(#21610,#21611,#21612)) ;
#4431 = EDGE_LOOP('',(#21613,#21614,#21615,#21616,#21617)) ;
#4432 = EDGE_LOOP('',(#21618,#21619,#21620,#21621,#21622,#21623)) ;
#4433 = EDGE_LOOP('',(#21624,#21625,#21626)) ;
#4434 = EDGE_LOOP('',(#21627,#21628,#21629,#21630,#21631)) ;
#4435 = EDGE_LOOP('',(#21632,#21633,#21634,#21635,#21636,#21637)) ;
#4436 = EDGE_LOOP('',(#21638,#21639,#21640)) ;
#4437 = EDGE_LOOP('',(#21641,#21642,#21643,#21644,#21645)) ;
#4438 = EDGE_LOOP('',(#21646,#21647,#21648,#21649,#21650,#21651)) ;
#4439 = EDGE_LOOP('',(#21652,#21653,#21654)) ;
#4440 = EDGE_LOOP('',(#21655,#21656,#21657,#21658,#21659)) ;
#4441 = EDGE_LOOP('',(#21660,#21661,#21662,#21663,#21664,#21665)) ;
#4442 = EDGE_LOOP('',(#21666,#21667,#21668,#21669)) ;
#4443 = EDGE_LOOP('',(#21670,#21671,#21672,#21673,#21674)) ;
#4444 = EDGE_LOOP('',(#21675,#21676,#21677,#21678,#21679)) ;
#4445 = EDGE_LOOP('',(#21680,#21681,#21682,#21683)) ;
#4446 = EDGE_LOOP('',(#21684,#21685,#21686,#21687,#21688)) ;
#4447 = EDGE_LOOP('',(#21689,#21690,#21691,#21692,#21693,#21694)) ;
#4448 = EDGE_LOOP('',(#21695,#21696,#21697)) ;
#4449 = EDGE_LOOP('',(#21698,#21699,#21700,#21701,#21702)) ;
#4450 = EDGE_LOOP('',(#21703,#21704,#21705,#21706,#21707,#21708)) ;
#4451 = EDGE_LOOP('',(#21709,#21710,#21711)) ;
#4452 = EDGE_LOOP('',(#21712,#21713,#21714,#21715,#21716)) ;
#4453 = EDGE_LOOP('',(#21717,#21718,#21719,#21720,#21721,#21722)) ;
#4454 = EDGE_LOOP('',(#21723,#21724,#21725,#21726)) ;
#4455 = EDGE_LOOP('',(#21727,#21728,#21729,#21730,#21731)) ;
#4456 = EDGE_LOOP('',(#21732,#21733,#21734,#21735,#21736)) ;
#4457 = EDGE_LOOP('',(#21737,#21738,#21739,#21740)) ;
#4458 = EDGE_LOOP('',(#21741,#21742,#21743,#21744,#21745)) ;
#4459 = EDGE_LOOP('',(#21746,#21747,#21748,#21749,#21750)) ;
#4460 = EDGE_LOOP('',(#21751,#21752,#21753)) ;
#4461 = EDGE_LOOP('',(#21754,#21755,#21756,#21757,#21758)) ;
#4462 = EDGE_LOOP('',(#21759,#21760,#21761,#21762,#21763,#21764)) ;
#4463 = EDGE_LOOP('',(#21765,#21766,#21767)) ;
#4464 = EDGE_LOOP('',(#21768,#21769,#21770,#21771,#21772)) ;
#4465 = EDGE_LOOP('',(#21773,#21774,#21775,#21776,#21777,#21778)) ;
#4466 = EDGE_LOOP('',(#21779,#21780,#21781,#21782)) ;
#4467 = EDGE_LOOP('',(#21783,#21784,#21785,#21786)) ;
#4468 = EDGE_LOOP('',(#21787,#21788,#21789,#21790)) ;
#4469 = EDGE_LOOP('',(#21791,#21792,#21793,#21794)) ;
#4470 = EDGE_LOOP('',(#21795,#21796,#21797,#21798)) ;
#4471 = EDGE_LOOP('',(#21799,#21800,#21801,#21802)) ;
#4472 = EDGE_LOOP('',(#21803,#21804,#21805,#21806,#21807)) ;
#4473 = EDGE_LOOP('',(#21808,#21809,#21810,#21811)) ;
#4474 = EDGE_LOOP('',(#21812,#21813,#21814,#21815)) ;
#4475 = EDGE_LOOP('',(#21816,#21817,#21818,#21819)) ;
#4476 = EDGE_LOOP('',(#21820,#21821,#21822,#21823)) ;
#4477 = EDGE_LOOP('',(#21824,#21825,#21826,#21827)) ;
#4478 = EDGE_LOOP('',(#21828,#21829,#21830,#21831)) ;
#4479 = EDGE_LOOP('',(#21832,#21833,#21834,#21835,#21836)) ;
#4480 = EDGE_LOOP('',(#21837,#21838,#21839,#21840)) ;
#4481 = EDGE_LOOP('',(#21841,#21842,#21843,#21844)) ;
#4482 = EDGE_LOOP('',(#21845,#21846,#21847,#21848)) ;
#4483 = EDGE_LOOP('',(#21849,#21850,#21851,#21852)) ;
#4484 = EDGE_LOOP('',(#21853,#21854,#21855,#21856)) ;
#4485 = EDGE_LOOP('',(#21857,#21858,#21859,#21860)) ;
#4486 = EDGE_LOOP('',(#21861,#21862,#21863,#21864)) ;
#4487 = EDGE_LOOP('',(#21865,#21866,#21867,#21868,#21869,#21870,#21871,#21872,
#21873,#21874,#21875,#21876)) ;
#4488 = EDGE_LOOP('',(#21877,#21878,#21879,#21880)) ;
#4489 = EDGE_LOOP('',(#21881,#21882,#21883,#21884)) ;
#4490 = EDGE_LOOP('',(#21885,#21886,#21887,#21888,#21889,#21890,#21891,#21892,
#21893,#21894,#21895,#21896,#21897,#21898,#21899,#21900)) ;
#4491 = EDGE_LOOP('',(#21901,#21902,#21903,#21904,#21905,#21906,#21907,#21908,
#21909,#21910,#21911,#21912,#21913,#21914)) ;
#4492 = EDGE_LOOP('',(#21915,#21916,#21917,#21918,#21919,#21920)) ;
#4493 = EDGE_LOOP('',(#21921,#21922,#21923,#21924,#21925,#21926)) ;
#4494 = EDGE_LOOP('',(#21927)) ;
#4495 = EDGE_LOOP('',(#21928,#21929,#21930,#21931)) ;
#4496 = EDGE_LOOP('',(#21932,#21933,#21934,#21935)) ;
#4497 = EDGE_LOOP('',(#21936,#21937,#21938,#21939)) ;
#4498 = EDGE_LOOP('',(#21940)) ;
#4499 = EDGE_LOOP('',(#21941,#21942,#21943,#21944)) ;
#4500 = EDGE_LOOP('',(#21945,#21946,#21947,#21948,#21949,#21950,#21951,#21952,
#21953,#21954,#21955,#21956,#21957,#21958,#21959,#21960,#21961,#21962,#21963,
#21964,#21965,#21966,#21967,#21968)) ;
#4501 = EDGE_LOOP('',(#21969)) ;
#4502 = EDGE_LOOP('',(#21970,#21971,#21972,#21973)) ;
#4503 = EDGE_LOOP('',(#21974,#21975,#21976,#21977)) ;
#4504 = EDGE_LOOP('',(#21978,#21979,#21980,#21981)) ;
#4505 = EDGE_LOOP('',(#21982,#21983,#21984,#21985)) ;
#4506 = EDGE_LOOP('',(#21986)) ;
#4507 = EDGE_LOOP('',(#21987,#21988,#21989,#21990,#21991,#21992)) ;
#4508 = EDGE_LOOP('',(#21993,#21994,#21995,#21996,#21997,#21998)) ;
#4509 = EDGE_LOOP('',(#21999,#22000,#22001,#22002,#22003,#22004,#22005,#22006)) ;
#4510 = EDGE_LOOP('',(#22007,#22008,#22009,#22010,#22011,#22012,#22013,#22014,
#22015,#22016)) ;
#4511 = EDGE_LOOP('',(#22017,#22018,#22019,#22020,#22021,#22022,#22023,#22024,
#22025,#22026,#22027,#22028,#22029,#22030,#22031,#22032)) ;
#4512 = EDGE_LOOP('',(#22033)) ;
#4513 = EDGE_LOOP('',(#22034,#22035,#22036,#22037)) ;
#4514 = EDGE_LOOP('',(#22038,#22039,#22040,#22041)) ;
#4515 = EDGE_LOOP('',(#22042,#22043,#22044,#22045)) ;
#4516 = EDGE_LOOP('',(#22046,#22047,#22048,#22049,#22050,#22051)) ;
#4517 = EDGE_LOOP('',(#22052)) ;
#4518 = EDGE_LOOP('',(#22053,#22054,#22055,#22056,#22057)) ;
#4519 = EDGE_LOOP('',(#22058,#22059,#22060,#22061,#22062)) ;
#4520 = EDGE_LOOP('',(#22063,#22064,#22065,#22066,#22067,#22068,#22069,#22070,
#22071,#22072,#22073,#22074,#22075,#22076,#22077,#22078,#22079,#22080,#22081,
#22082,#22083,#22084,#22085,#22086)) ;
#4521 = EDGE_LOOP('',(#22087,#22088,#22089,#22090,#22091,#22092,#22093,#22094)) ;
#4522 = EDGE_LOOP('',(#22095,#22096,#22097,#22098,#22099)) ;
#4523 = EDGE_LOOP('',(#22100,#22101,#22102,#22103,#22104)) ;
#4524 = EDGE_LOOP('',(#22105,#22106,#22107,#22108,#22109,#22110)) ;
#4525 = EDGE_LOOP('',(#22111,#22112,#22113,#22114)) ;
#4526 = EDGE_LOOP('',(#22115,#22116,#22117,#22118)) ;
#4527 = EDGE_LOOP('',(#22119,#22120,#22121,#22122)) ;
#4528 = EDGE_LOOP('',(#22123,#22124,#22125,#22126)) ;
#4529 = EDGE_LOOP('',(#22127)) ;
#4530 = EDGE_LOOP('',(#22128)) ;
#4531 = EDGE_LOOP('',(#22129,#22130,#22131,#22132,#22133,#22134,#22135,#22136)) ;
#4532 = EDGE_LOOP('',(#22137,#22138,#22139,#22140,#22141,#22142,#22143,#22144)) ;
#4533 = EDGE_LOOP('',(#22145,#22146,#22147,#22148)) ;
#4534 = EDGE_LOOP('',(#22149,#22150,#22151,#22152)) ;
#4535 = EDGE_LOOP('',(#22153,#22154,#22155,#22156)) ;
#4536 = EDGE_LOOP('',(#22157,#22158,#22159,#22160)) ;
#4537 = EDGE_LOOP('',(#22161,#22162,#22163,#22164)) ;
#4538 = EDGE_LOOP('',(#22165,#22166,#22167,#22168)) ;
#4539 = EDGE_LOOP('',(#22169,#22170,#22171,#22172)) ;
#4540 = EDGE_LOOP('',(#22173,#22174,#22175,#22176)) ;
#4541 = EDGE_LOOP('',(#22177,#22178,#22179,#22180)) ;
#4542 = EDGE_LOOP('',(#22181,#22182,#22183,#22184,#22185,#22186,#22187)) ;
#4543 = EDGE_LOOP('',(#22188,#22189,#22190,#22191,#22192,#22193,#22194,#22195)) ;
#4544 = EDGE_LOOP('',(#22196,#22197,#22198,#22199)) ;
#4545 = EDGE_LOOP('',(#22200,#22201,#22202,#22203)) ;
#4546 = EDGE_LOOP('',(#22204,#22205,#22206,#22207,#22208,#22209,#22210)) ;
#4547 = EDGE_LOOP('',(#22211,#22212,#22213,#22214)) ;
#4548 = EDGE_LOOP('',(#22215,#22216,#22217,#22218)) ;
#4549 = EDGE_LOOP('',(#22219,#22220,#22221,#22222)) ;
#4550 = EDGE_LOOP('',(#22223,#22224,#22225,#22226)) ;
#4551 = EDGE_LOOP('',(#22227,#22228,#22229,#22230)) ;
#4552 = EDGE_LOOP('',(#22231,#22232,#22233,#22234)) ;
#4553 = EDGE_LOOP('',(#22235,#22236,#22237,#22238)) ;
#4554 = EDGE_LOOP('',(#22239,#22240,#22241,#22242)) ;
#4555 = EDGE_LOOP('',(#22243,#22244,#22245,#22246)) ;
#4556 = EDGE_LOOP('',(#22247,#22248,#22249,#22250)) ;
#4557 = EDGE_LOOP('',(#22251,#22252,#22253,#22254)) ;
#4558 = EDGE_LOOP('',(#22255,#22256,#22257,#22258)) ;
#4559 = EDGE_LOOP('',(#22259,#22260,#22261,#22262)) ;
#4560 = EDGE_LOOP('',(#22263,#22264,#22265,#22266)) ;
#4561 = EDGE_LOOP('',(#22267,#22268,#22269,#22270)) ;
#4562 = EDGE_LOOP('',(#22271,#22272,#22273,#22274)) ;
#4563 = EDGE_LOOP('',(#22275,#22276,#22277,#22278)) ;
#4564 = EDGE_LOOP('',(#22279,#22280,#22281,#22282)) ;
#4565 = EDGE_LOOP('',(#22283,#22284,#22285,#22286)) ;
#4566 = EDGE_LOOP('',(#22287,#22288,#22289,#22290)) ;
#4567 = EDGE_LOOP('',(#22291,#22292,#22293,#22294)) ;
#4568 = EDGE_LOOP('',(#22295,#22296,#22297,#22298)) ;
#4569 = EDGE_LOOP('',(#22299,#22300,#22301,#22302)) ;
#4570 = EDGE_LOOP('',(#22303,#22304,#22305,#22306)) ;
#4571 = EDGE_LOOP('',(#22307,#22308,#22309,#22310)) ;
#4572 = EDGE_LOOP('',(#22311,#22312,#22313,#22314)) ;
#4573 = EDGE_LOOP('',(#22315,#22316,#22317,#22318)) ;
#4574 = EDGE_LOOP('',(#22319,#22320,#22321,#22322)) ;
#4575 = EDGE_LOOP('',(#22323,#22324,#22325,#22326)) ;
#4576 = EDGE_LOOP('',(#22327,#22328,#22329,#22330)) ;
#4577 = EDGE_LOOP('',(#22331,#22332,#22333,#22334)) ;
#4578 = EDGE_LOOP('',(#22335,#22336,#22337,#22338)) ;
#4579 = EDGE_LOOP('',(#22339,#22340,#22341,#22342)) ;
#4580 = EDGE_LOOP('',(#22343,#22344,#22345,#22346)) ;
#4581 = EDGE_LOOP('',(#22347,#22348,#22349,#22350)) ;
#4582 = EDGE_LOOP('',(#22351,#22352,#22353,#22354)) ;
#4583 = EDGE_LOOP('',(#22355,#22356,#22357,#22358,#22359,#22360,#22361,#22362)) ;
#4584 = EDGE_LOOP('',(#22363,#22364,#22365,#22366)) ;
#4585 = EDGE_LOOP('',(#22367,#22368,#22369,#22370)) ;
#4586 = EDGE_LOOP('',(#22371,#22372,#22373,#22374)) ;
#4587 = EDGE_LOOP('',(#22375,#22376,#22377,#22378)) ;
#4588 = EDGE_LOOP('',(#22379,#22380,#22381,#22382)) ;
#4589 = EDGE_LOOP('',(#22383,#22384,#22385,#22386,#22387,#22388,#22389,#22390)) ;
#4590 = EDGE_LOOP('',(#22391,#22392,#22393,#22394)) ;
#4591 = EDGE_LOOP('',(#22395,#22396,#22397,#22398)) ;
#4592 = EDGE_LOOP('',(#22399,#22400,#22401,#22402)) ;
#4593 = EDGE_LOOP('',(#22403,#22404,#22405,#22406)) ;
#4594 = EDGE_LOOP('',(#22407,#22408,#22409,#22410)) ;
#4595 = EDGE_LOOP('',(#22411,#22412,#22413,#22414)) ;
#4596 = EDGE_LOOP('',(#22415,#22416,#22417,#22418,#22419)) ;
#4597 = EDGE_LOOP('',(#22420,#22421,#22422,#22423,#22424)) ;
#4598 = EDGE_LOOP('',(#22425,#22426,#22427,#22428,#22429)) ;
#4599 = EDGE_LOOP('',(#22430,#22431,#22432,#22433,#22434)) ;
#4600 = EDGE_LOOP('',(#22435,#22436,#22437,#22438)) ;
#4601 = EDGE_LOOP('',(#22439,#22440,#22441,#22442)) ;
#4602 = EDGE_LOOP('',(#22443,#22444,#22445,#22446)) ;
#4603 = EDGE_LOOP('',(#22447,#22448,#22449,#22450)) ;
#4604 = EDGE_LOOP('',(#22451,#22452,#22453,#22454)) ;
#4605 = EDGE_LOOP('',(#22455,#22456,#22457,#22458)) ;
#4606 = EDGE_LOOP('',(#22459,#22460,#22461,#22462)) ;
#4607 = EDGE_LOOP('',(#22463,#22464,#22465,#22466,#22467,#22468)) ;
#4608 = EDGE_LOOP('',(#22469,#22470,#22471,#22472)) ;
#4609 = EDGE_LOOP('',(#22473,#22474,#22475,#22476)) ;
#4610 = EDGE_LOOP('',(#22477,#22478,#22479,#22480)) ;
#4611 = EDGE_LOOP('',(#22481,#22482,#22483,#22484)) ;
#4612 = EDGE_LOOP('',(#22485,#22486,#22487,#22488)) ;
#4613 = EDGE_LOOP('',(#22489,#22490,#22491,#22492)) ;
#4614 = EDGE_LOOP('',(#22493,#22494,#22495,#22496)) ;
#4615 = EDGE_LOOP('',(#22497,#22498,#22499,#22500)) ;
#4616 = EDGE_LOOP('',(#22501,#22502,#22503,#22504)) ;
#4617 = EDGE_LOOP('',(#22505,#22506,#22507,#22508)) ;
#4618 = EDGE_LOOP('',(#22509,#22510,#22511,#22512)) ;
#4619 = EDGE_LOOP('',(#22513,#22514,#22515,#22516)) ;
#4620 = EDGE_LOOP('',(#22517,#22518,#22519,#22520)) ;
#4621 = EDGE_LOOP('',(#22521,#22522,#22523,#22524)) ;
#4622 = EDGE_LOOP('',(#22525,#22526,#22527,#22528)) ;
#4623 = EDGE_LOOP('',(#22529,#22530,#22531,#22532)) ;
#4624 = EDGE_LOOP('',(#22533,#22534,#22535,#22536)) ;
#4625 = EDGE_LOOP('',(#22537,#22538,#22539,#22540)) ;
#4626 = EDGE_LOOP('',(#22541,#22542,#22543,#22544)) ;
#4627 = EDGE_LOOP('',(#22545,#22546,#22547,#22548)) ;
#4628 = EDGE_LOOP('',(#22549,#22550,#22551,#22552)) ;
#4629 = EDGE_LOOP('',(#22553,#22554,#22555,#22556)) ;
#4630 = EDGE_LOOP('',(#22557,#22558,#22559,#22560,#22561,#22562,#22563,#22564)) ;
#4631 = EDGE_LOOP('',(#22565,#22566,#22567,#22568,#22569,#22570,#22571,#22572)) ;
#4632 = EDGE_LOOP('',(#22573,#22574,#22575,#22576)) ;
#4633 = EDGE_LOOP('',(#22577,#22578,#22579,#22580)) ;
#4634 = EDGE_LOOP('',(#22581,#22582,#22583,#22584,#22585,#22586,#22587,#22588)) ;
#4635 = EDGE_LOOP('',(#22589,#22590,#22591,#22592)) ;
#4636 = EDGE_LOOP('',(#22593,#22594,#22595,#22596)) ;
#4637 = EDGE_LOOP('',(#22597,#22598,#22599,#22600)) ;
#4638 = EDGE_LOOP('',(#22601,#22602,#22603,#22604,#22605,#22606)) ;
#4639 = EDGE_LOOP('',(#22607,#22608,#22609,#22610,#22611,#22612,#22613,#22614)) ;
#4640 = EDGE_LOOP('',(#22615,#22616,#22617,#22618,#22619,#22620,#22621,#22622)) ;
#4641 = EDGE_LOOP('',(#22623,#22624,#22625,#22626,#22627,#22628,#22629,#22630)) ;
#4642 = EDGE_LOOP('',(#22631,#22632,#22633,#22634,#22635,#22636,#22637,#22638)) ;
#4643 = EDGE_LOOP('',(#22639,#22640,#22641,#22642,#22643,#22644,#22645,#22646,
#22647,#22648,#22649,#22650)) ;
#4644 = EDGE_LOOP('',(#22651)) ;
#4645 = EDGE_LOOP('',(#22652)) ;
#4646 = EDGE_LOOP('',(#22653)) ;
#4647 = EDGE_LOOP('',(#22654)) ;
#4648 = EDGE_LOOP('',(#22655,#22656,#22657,#22658)) ;
#4649 = EDGE_LOOP('',(#22659,#22660,#22661,#22662,#22663)) ;
#4650 = EDGE_LOOP('',(#22664,#22665,#22666,#22667,#22668)) ;
#4651 = EDGE_LOOP('',(#22669,#22670,#22671,#22672,#22673)) ;
#4652 = EDGE_LOOP('',(#22674,#22675,#22676,#22677,#22678)) ;
#4653 = EDGE_LOOP('',(#22679,#22680,#22681,#22682,#22683)) ;
#4654 = EDGE_LOOP('',(#22684,#22685,#22686,#22687,#22688)) ;
#4655 = EDGE_LOOP('',(#22689,#22690,#22691,#22692,#22693)) ;
#4656 = EDGE_LOOP('',(#22694,#22695,#22696,#22697,#22698)) ;
#4657 = EDGE_LOOP('',(#22699,#22700,#22701,#22702)) ;
#4658 = EDGE_LOOP('',(#22703,#22704,#22705,#22706,#22707)) ;
#4659 = EDGE_LOOP('',(#22708,#22709,#22710,#22711,#22712)) ;
#4660 = EDGE_LOOP('',(#22713,#22714,#22715,#22716,#22717,#22718,#22719,#22720)) ;
#4661 = EDGE_LOOP('',(#22721,#22722,#22723,#22724,#22725,#22726,#22727,#22728)) ;
#4662 = EDGE_LOOP('',(#22729,#22730,#22731,#22732)) ;
#4663 = EDGE_LOOP('',(#22733,#22734,#22735,#22736)) ;
#4664 = EDGE_LOOP('',(#22737,#22738,#22739,#22740)) ;
#4665 = EDGE_LOOP('',(#22741,#22742,#22743,#22744)) ;
#4666 = EDGE_LOOP('',(#22745,#22746,#22747,#22748)) ;
#4667 = EDGE_LOOP('',(#22749,#22750,#22751,#22752)) ;
#4668 = EDGE_LOOP('',(#22753,#22754,#22755,#22756)) ;
#4669 = EDGE_LOOP('',(#22757,#22758,#22759,#22760)) ;
#4670 = EDGE_LOOP('',(#22761,#22762,#22763,#22764)) ;
#4671 = EDGE_LOOP('',(#22765,#22766,#22767,#22768)) ;
#4672 = EDGE_LOOP('',(#22769,#22770,#22771,#22772)) ;
#4673 = EDGE_LOOP('',(#22773,#22774,#22775,#22776)) ;
#4674 = EDGE_LOOP('',(#22777,#22778,#22779,#22780)) ;
#4675 = EDGE_LOOP('',(#22781,#22782,#22783,#22784)) ;
#4676 = EDGE_LOOP('',(#22785,#22786,#22787,#22788)) ;
#4677 = EDGE_LOOP('',(#22789,#22790,#22791,#22792)) ;
#4678 = EDGE_LOOP('',(#22793,#22794,#22795,#22796)) ;
#4679 = EDGE_LOOP('',(#22797,#22798,#22799,#22800)) ;
#4680 = EDGE_LOOP('',(#22801,#22802,#22803,#22804)) ;
#4681 = EDGE_LOOP('',(#22805,#22806,#22807,#22808)) ;
#4682 = EDGE_LOOP('',(#22809,#22810,#22811,#22812)) ;
#4683 = EDGE_LOOP('',(#22813,#22814,#22815,#22816,#22817,#22818,#22819,#22820)) ;
#4684 = EDGE_LOOP('',(#22821,#22822,#22823,#22824)) ;
#4685 = EDGE_LOOP('',(#22825,#22826,#22827,#22828,#22829,#22830,#22831,#22832)) ;
#4686 = EDGE_LOOP('',(#22833,#22834,#22835,#22836,#22837,#22838,#22839,#22840,
#22841,#22842)) ;
#4687 = EDGE_LOOP('',(#22843,#22844,#22845,#22846,#22847,#22848)) ;
#4688 = EDGE_LOOP('',(#22849,#22850,#22851,#22852,#22853,#22854,#22855,#22856,
#22857,#22858)) ;
#4689 = EDGE_LOOP('',(#22859)) ;
#4690 = EDGE_LOOP('',(#22860,#22861,#22862,#22863,#22864)) ;
#4691 = EDGE_LOOP('',(#22865,#22866,#22867,#22868,#22869)) ;
#4692 = EDGE_LOOP('',(#22870,#22871,#22872,#22873,#22874,#22875,#22876,#22877,
#22878,#22879,#22880,#22881)) ;
#4693 = EDGE_LOOP('',(#22882,#22883,#22884,#22885,#22886,#22887,#22888,#22889,
#22890,#22891,#22892,#22893,#22894)) ;
#4694 = EDGE_LOOP('',(#22895,#22896,#22897,#22898,#22899,#22900,#22901,#22902,
#22903,#22904,#22905,#22906)) ;
#4695 = EDGE_LOOP('',(#22907,#22908,#22909,#22910,#22911,#22912,#22913,#22914,
#22915,#22916,#22917,#22918,#22919)) ;
#4696 = EDGE_LOOP('',(#22920,#22921,#22922,#22923,#22924,#22925,#22926,#22927,
#22928,#22929,#22930,#22931)) ;
#4697 = EDGE_LOOP('',(#22932,#22933,#22934,#22935,#22936,#22937,#22938,#22939,
#22940,#22941,#22942,#22943,#22944,#22945,#22946)) ;
#4698 = EDGE_LOOP('',(#22947,#22948,#22949,#22950,#22951,#22952,#22953,#22954,
#22955,#22956,#22957,#22958)) ;
#4699 = EDGE_LOOP('',(#22959,#22960,#22961,#22962,#22963,#22964,#22965,#22966,
#22967,#22968,#22969,#22970,#22971)) ;
#4700 = EDGE_LOOP('',(#22972,#22973,#22974,#22975)) ;
#4701 = EDGE_LOOP('',(#22976,#22977,#22978,#22979)) ;
#4702 = EDGE_LOOP('',(#22980,#22981,#22982,#22983)) ;
#4703 = EDGE_LOOP('',(#22984,#22985,#22986,#22987)) ;
#4704 = EDGE_LOOP('',(#22988,#22989,#22990,#22991)) ;
#4705 = EDGE_LOOP('',(#22992,#22993,#22994,#22995)) ;
#4706 = EDGE_LOOP('',(#22996,#22997,#22998,#22999)) ;
#4707 = EDGE_LOOP('',(#23000,#23001,#23002,#23003)) ;
#4708 = EDGE_LOOP('',(#23004,#23005,#23006,#23007)) ;
#4709 = EDGE_LOOP('',(#23008,#23009,#23010,#23011)) ;
#4710 = EDGE_LOOP('',(#23012,#23013,#23014,#23015)) ;
#4711 = EDGE_LOOP('',(#23016,#23017,#23018,#23019)) ;
#4712 = EDGE_LOOP('',(#23020,#23021,#23022,#23023)) ;
#4713 = EDGE_LOOP('',(#23024,#23025,#23026,#23027)) ;
#4714 = EDGE_LOOP('',(#23028,#23029,#23030,#23031)) ;
#4715 = EDGE_LOOP('',(#23032,#23033,#23034,#23035)) ;
#4716 = EDGE_LOOP('',(#23036,#23037,#23038,#23039)) ;
#4717 = EDGE_LOOP('',(#23040,#23041,#23042,#23043,#23044,#23045,#23046)) ;
#4718 = EDGE_LOOP('',(#23047,#23048,#23049,#23050)) ;
#4719 = EDGE_LOOP('',(#23051,#23052,#23053,#23054,#23055,#23056,#23057)) ;
#4720 = EDGE_LOOP('',(#23058,#23059,#23060,#23061,#23062)) ;
#4721 = EDGE_LOOP('',(#23063,#23064,#23065,#23066,#23067)) ;
#4722 = EDGE_LOOP('',(#23068,#23069,#23070,#23071,#23072)) ;
#4723 = EDGE_LOOP('',(#23073,#23074,#23075,#23076,#23077,#23078,#23079,#23080)) ;
#4724 = EDGE_LOOP('',(#23081)) ;
#4725 = EDGE_LOOP('',(#23082)) ;
#4726 = EDGE_LOOP('',(#23083)) ;
#4727 = EDGE_LOOP('',(#23084)) ;
#4728 = EDGE_LOOP('',(#23085,#23086,#23087,#23088)) ;
#4729 = EDGE_LOOP('',(#23089,#23090,#23091,#23092)) ;
#4730 = EDGE_LOOP('',(#23093,#23094,#23095,#23096)) ;
#4731 = EDGE_LOOP('',(#23097,#23098,#23099,#23100,#23101,#23102)) ;
#4732 = EDGE_LOOP('',(#23103)) ;
#4733 = EDGE_LOOP('',(#23104,#23105,#23106,#23107,#23108)) ;
#4734 = EDGE_LOOP('',(#23109,#23110,#23111,#23112)) ;
#4735 = EDGE_LOOP('',(#23113,#23114,#23115,#23116)) ;
#4736 = EDGE_LOOP('',(#23117,#23118,#23119,#23120)) ;
#4737 = EDGE_LOOP('',(#23121,#23122,#23123,#23124,#23125,#23126,#23127,#23128,
#23129,#23130,#23131,#23132)) ;
#4738 = EDGE_LOOP('',(#23133,#23134,#23135,#23136,#23137,#23138,#23139,#23140,
#23141,#23142,#23143,#23144,#23145)) ;
#4739 = EDGE_LOOP('',(#23146,#23147,#23148,#23149,#23150,#23151,#23152,#23153,
#23154,#23155,#23156,#23157)) ;
#4740 = EDGE_LOOP('',(#23158,#23159,#23160,#23161,#23162,#23163,#23164,#23165,
#23166,#23167,#23168,#23169,#23170,#23171,#23172)) ;
#4741 = EDGE_LOOP('',(#23173,#23174,#23175,#23176,#23177,#23178,#23179,#23180,
#23181,#23182,#23183,#23184,#23185,#23186)) ;
#4742 = EDGE_LOOP('',(#23187,#23188,#23189,#23190,#23191,#23192,#23193,#23194,
#23195,#23196,#23197,#23198,#23199,#23200)) ;
#4743 = EDGE_LOOP('',(#23201,#23202,#23203,#23204,#23205,#23206,#23207,#23208,
#23209,#23210,#23211,#23212,#23213,#23214,#23215,#23216,#23217,#23218,#23219,
#23220,#23221,#23222,#23223,#23224,#23225,#23226,#23227,#23228,#23229,#23230,
#23231,#23232)) ;
#4744 = EDGE_LOOP('',(#23233,#23234,#23235,#23236,#23237,#23238)) ;
#4745 = EDGE_LOOP('',(#23239,#23240,#23241,#23242,#23243,#23244)) ;
#4746 = EDGE_LOOP('',(#23245,#23246,#23247,#23248,#23249,#23250)) ;
#4747 = EDGE_LOOP('',(#23251,#23252,#23253,#23254,#23255,#23256)) ;
#4748 = EDGE_LOOP('',(#23257,#23258,#23259,#23260,#23261,#23262)) ;
#4749 = EDGE_LOOP('',(#23263,#23264,#23265,#23266,#23267)) ;
#4750 = EDGE_LOOP('',(#23268,#23269,#23270,#23271,#23272)) ;
#4751 = EDGE_LOOP('',(#23273,#23274,#23275,#23276,#23277)) ;
#4752 = EDGE_LOOP('',(#23278,#23279,#23280,#23281,#23282)) ;
#4753 = EDGE_LOOP('',(#23283,#23284,#23285,#23286,#23287,#23288,#23289,#23290,
#23291,#23292,#23293,#23294)) ;
#4754 = EDGE_LOOP('',(#23295,#23296,#23297,#23298,#23299,#23300,#23301,#23302,
#23303,#23304,#23305,#23306,#23307)) ;
#4755 = EDGE_LOOP('',(#23308,#23309,#23310,#23311)) ;
#4756 = EDGE_LOOP('',(#23312,#23313,#23314,#23315)) ;
#4757 = EDGE_LOOP('',(#23316,#23317,#23318,#23319)) ;
#4758 = EDGE_LOOP('',(#23320,#23321,#23322,#23323)) ;
#4759 = EDGE_LOOP('',(#23324,#23325,#23326,#23327)) ;
#4760 = EDGE_LOOP('',(#23328,#23329,#23330,#23331)) ;
#4761 = EDGE_LOOP('',(#23332,#23333,#23334,#23335)) ;
#4762 = EDGE_LOOP('',(#23336,#23337,#23338,#23339)) ;
#4763 = EDGE_LOOP('',(#23340,#23341,#23342,#23343)) ;
#4764 = EDGE_LOOP('',(#23344,#23345,#23346,#23347)) ;
#4765 = EDGE_LOOP('',(#23348,#23349,#23350,#23351)) ;
#4766 = EDGE_LOOP('',(#23352,#23353,#23354,#23355)) ;
#4767 = EDGE_LOOP('',(#23356,#23357,#23358,#23359,#23360,#23361,#23362,#23363,
#23364,#23365,#23366,#23367,#23368,#23369,#23370,#23371,#23372,#23373,#23374,
#23375,#23376,#23377,#23378,#23379,#23380,#23381,#23382,#23383,#23384,#23385)) ;
#4768 = EDGE_LOOP('',(#23386,#23387,#23388,#23389,#23390,#23391)) ;
#4769 = EDGE_LOOP('',(#23392,#23393,#23394,#23395,#23396,#23397)) ;
#4770 = EDGE_LOOP('',(#23398,#23399,#23400,#23401,#23402,#23403)) ;
#4771 = EDGE_LOOP('',(#23404,#23405,#23406,#23407,#23408,#23409)) ;
#4772 = EDGE_LOOP('',(#23410,#23411,#23412,#23413,#23414,#23415)) ;
#4773 = EDGE_LOOP('',(#23416,#23417,#23418,#23419,#23420,#23421)) ;
#4774 = EDGE_LOOP('',(#23422,#23423,#23424,#23425,#23426,#23427)) ;
#4775 = EDGE_LOOP('',(#23428,#23429,#23430,#23431,#23432,#23433)) ;
#4776 = EDGE_LOOP('',(#23434,#23435,#23436,#23437,#23438,#23439)) ;
#4777 = EDGE_LOOP('',(#23440,#23441,#23442,#23443)) ;
#4778 = EDGE_LOOP('',(#23444,#23445,#23446,#23447)) ;
#4779 = EDGE_LOOP('',(#23448,#23449,#23450,#23451)) ;
#4780 = EDGE_LOOP('',(#23452,#23453,#23454,#23455)) ;
#4781 = EDGE_LOOP('',(#23456,#23457,#23458,#23459)) ;
#4782 = EDGE_LOOP('',(#23460,#23461,#23462,#23463)) ;
#4783 = EDGE_LOOP('',(#23464,#23465,#23466,#23467)) ;
#4784 = EDGE_LOOP('',(#23468,#23469,#23470,#23471)) ;
#4785 = EDGE_LOOP('',(#23472,#23473,#23474,#23475)) ;
#4786 = EDGE_LOOP('',(#23476,#23477,#23478,#23479)) ;
#4787 = EDGE_LOOP('',(#23480,#23481,#23482,#23483)) ;
#4788 = EDGE_LOOP('',(#23484,#23485,#23486,#23487)) ;
#4789 = EDGE_LOOP('',(#23488,#23489,#23490,#23491)) ;
#4790 = EDGE_LOOP('',(#23492,#23493,#23494,#23495)) ;
#4791 = EDGE_LOOP('',(#23496,#23497,#23498,#23499)) ;
#4792 = EDGE_LOOP('',(#23500,#23501,#23502,#23503)) ;
#4793 = EDGE_LOOP('',(#23504,#23505,#23506,#23507)) ;
#4794 = EDGE_LOOP('',(#23508,#23509,#23510,#23511)) ;
#4795 = EDGE_LOOP('',(#23512,#23513,#23514,#23515)) ;
#4796 = EDGE_LOOP('',(#23516,#23517,#23518,#23519)) ;
#4797 = EDGE_LOOP('',(#23520,#23521,#23522,#23523)) ;
#4798 = EDGE_LOOP('',(#23524,#23525,#23526,#23527)) ;
#4799 = EDGE_LOOP('',(#23528,#23529,#23530,#23531)) ;
#4800 = EDGE_LOOP('',(#23532,#23533,#23534,#23535)) ;
#4801 = EDGE_LOOP('',(#23536,#23537,#23538,#23539)) ;
#4802 = EDGE_LOOP('',(#23540,#23541,#23542,#23543)) ;
#4803 = EDGE_LOOP('',(#23544,#23545,#23546,#23547)) ;
#4804 = EDGE_LOOP('',(#23548,#23549,#23550,#23551)) ;
#4805 = EDGE_LOOP('',(#23552,#23553,#23554,#23555)) ;
#4806 = EDGE_LOOP('',(#23556,#23557,#23558,#23559)) ;
#4807 = EDGE_LOOP('',(#23560,#23561,#23562,#23563)) ;
#4808 = EDGE_LOOP('',(#23564,#23565,#23566,#23567)) ;
#4809 = EDGE_LOOP('',(#23568,#23569,#23570,#23571)) ;
#4810 = EDGE_LOOP('',(#23572,#23573,#23574,#23575)) ;
#4811 = EDGE_LOOP('',(#23576,#23577,#23578,#23579)) ;
#4812 = EDGE_LOOP('',(#23580,#23581,#23582,#23583)) ;
#4813 = EDGE_LOOP('',(#23584,#23585,#23586,#23587)) ;
#4814 = EDGE_LOOP('',(#23588,#23589,#23590,#23591)) ;
#4815 = EDGE_LOOP('',(#23592,#23593,#23594,#23595)) ;
#4816 = EDGE_LOOP('',(#23596,#23597,#23598,#23599)) ;
#4817 = EDGE_LOOP('',(#23600,#23601,#23602,#23603)) ;
#4818 = EDGE_LOOP('',(#23604,#23605,#23606,#23607)) ;
#4819 = EDGE_LOOP('',(#23608,#23609,#23610,#23611,#23612,#23613,#23614,#23615,
#23616,#23617,#23618,#23619,#23620,#23621,#23622,#23623,#23624,#23625,#23626,
#23627,#23628,#23629,#23630,#23631,#23632,#23633,#23634,#23635,#23636,#23637,
#23638,#23639,#23640,#23641,#23642,#23643,#23644,#23645,#23646,#23647,#23648,
#23649,#23650,#23651,#23652,#23653,#23654,#23655,#23656,#23657,#23658,#23659,
#23660,#23661,#23662,#23663,#23664,#23665,#23666,#23667,#23668,#23669,#23670,
#23671,#23672,#23673,#23674,#23675,#23676,#23677,#23678,#23679,#23680,#23681,
#23682,#23683)) ;
#4820 = EDGE_LOOP('',(#23684,#23685,#23686,#23687)) ;
#4821 = EDGE_LOOP('',(#23688,#23689,#23690,#23691)) ;
#4822 = EDGE_LOOP('',(#23692,#23693,#23694,#23695)) ;
#4823 = EDGE_LOOP('',(#23696,#23697,#23698,#23699,#23700,#23701,#23702,#23703)) ;
#4824 = EDGE_LOOP('',(#23704)) ;
#4825 = EDGE_LOOP('',(#23705,#23706,#23707,#23708)) ;
#4826 = EDGE_LOOP('',(#23709,#23710,#23711,#23712)) ;
#4827 = EDGE_LOOP('',(#23713,#23714,#23715,#23716)) ;
#4828 = EDGE_LOOP('',(#23717,#23718,#23719,#23720,#23721,#23722,#23723,#23724)) ;
#4829 = EDGE_LOOP('',(#23725)) ;
#4830 = EDGE_LOOP('',(#23726,#23727,#23728,#23729)) ;
#4831 = EDGE_LOOP('',(#23730,#23731,#23732,#23733)) ;
#4832 = EDGE_LOOP('',(#23734,#23735,#23736,#23737)) ;
#4833 = EDGE_LOOP('',(#23738,#23739,#23740,#23741,#23742,#23743,#23744,#23745)) ;
#4834 = EDGE_LOOP('',(#23746)) ;
#4835 = EDGE_LOOP('',(#23747,#23748,#23749,#23750)) ;
#4836 = EDGE_LOOP('',(#23751,#23752,#23753,#23754)) ;
#4837 = EDGE_LOOP('',(#23755,#23756,#23757,#23758)) ;
#4838 = EDGE_LOOP('',(#23759,#23760,#23761,#23762,#23763,#23764,#23765,#23766)) ;
#4839 = EDGE_LOOP('',(#23767)) ;
#4840 = EDGE_LOOP('',(#23768,#23769,#23770,#23771)) ;
#4841 = EDGE_LOOP('',(#23772,#23773,#23774,#23775)) ;
#4842 = EDGE_LOOP('',(#23776,#23777,#23778,#23779)) ;
#4843 = EDGE_LOOP('',(#23780,#23781,#23782,#23783,#23784,#23785,#23786,#23787)) ;
#4844 = EDGE_LOOP('',(#23788)) ;
#4845 = EDGE_LOOP('',(#23789,#23790,#23791,#23792)) ;
#4846 = EDGE_LOOP('',(#23793,#23794,#23795,#23796)) ;
#4847 = EDGE_LOOP('',(#23797,#23798,#23799,#23800)) ;
#4848 = EDGE_LOOP('',(#23801,#23802,#23803,#23804,#23805,#23806,#23807,#23808)) ;
#4849 = EDGE_LOOP('',(#23809)) ;
#4850 = EDGE_LOOP('',(#23810,#23811,#23812,#23813)) ;
#4851 = EDGE_LOOP('',(#23814,#23815,#23816,#23817)) ;
#4852 = EDGE_LOOP('',(#23818,#23819,#23820,#23821)) ;
#4853 = EDGE_LOOP('',(#23822,#23823,#23824,#23825,#23826,#23827,#23828,#23829)) ;
#4854 = EDGE_LOOP('',(#23830)) ;
#4855 = EDGE_LOOP('',(#23831,#23832,#23833,#23834)) ;
#4856 = EDGE_LOOP('',(#23835,#23836,#23837,#23838)) ;
#4857 = EDGE_LOOP('',(#23839,#23840,#23841,#23842)) ;
#4858 = EDGE_LOOP('',(#23843,#23844,#23845,#23846,#23847,#23848,#23849,#23850)) ;
#4859 = EDGE_LOOP('',(#23851)) ;
#4860 = EDGE_LOOP('',(#23852,#23853,#23854,#23855)) ;
#4861 = EDGE_LOOP('',(#23856,#23857,#23858,#23859)) ;
#4862 = EDGE_LOOP('',(#23860,#23861,#23862,#23863,#23864,#23865,#23866,#23867)) ;
#4863 = EDGE_LOOP('',(#23868)) ;
#4864 = EDGE_LOOP('',(#23869,#23870,#23871,#23872)) ;
#4865 = EDGE_LOOP('',(#23873)) ;
#4866 = EDGE_LOOP('',(#23874)) ;
#4867 = EDGE_LOOP('',(#23875)) ;
#4868 = EDGE_LOOP('',(#23876)) ;
#4869 = EDGE_LOOP('',(#23877)) ;
#4870 = EDGE_LOOP('',(#23878)) ;
#4871 = EDGE_LOOP('',(#23879)) ;
#4872 = EDGE_LOOP('',(#23880)) ;
#4873 = EDGE_LOOP('',(#23881)) ;
#4874 = EDGE_LOOP('',(#23882)) ;
#4875 = EDGE_LOOP('',(#23883)) ;
#4876 = EDGE_LOOP('',(#23884)) ;
#4877 = EDGE_LOOP('',(#23885)) ;
#4878 = EDGE_LOOP('',(#23886)) ;
#4879 = EDGE_LOOP('',(#23887)) ;
#4880 = EDGE_LOOP('',(#23888)) ;
#4881 = EDGE_LOOP('',(#23889,#23890,#23891,#23892)) ;
#4882 = EDGE_LOOP('',(#23893,#23894,#23895,#23896)) ;
#4883 = EDGE_LOOP('',(#23897,#23898,#23899,#23900)) ;
#4884 = EDGE_LOOP('',(#23901,#23902,#23903,#23904)) ;
#4885 = EDGE_LOOP('',(#23905,#23906,#23907,#23908)) ;
#4886 = EDGE_LOOP('',(#23909,#23910,#23911,#23912)) ;
#4887 = EDGE_LOOP('',(#23913,#23914,#23915,#23916)) ;
#4888 = EDGE_LOOP('',(#23917,#23918,#23919,#23920)) ;
#4889 = EDGE_LOOP('',(#23921,#23922,#23923,#23924)) ;
#4890 = EDGE_LOOP('',(#23925,#23926,#23927,#23928,#23929,#23930,#23931,#23932,
#23933,#23934)) ;
#4891 = EDGE_LOOP('',(#23935,#23936,#23937,#23938)) ;
#4892 = EDGE_LOOP('',(#23939,#23940,#23941,#23942)) ;
#4893 = EDGE_LOOP('',(#23943,#23944,#23945,#23946)) ;
#4894 = EDGE_LOOP('',(#23947,#23948,#23949,#23950)) ;
#4895 = EDGE_LOOP('',(#23951,#23952,#23953,#23954)) ;
#4896 = EDGE_LOOP('',(#23955,#23956,#23957,#23958)) ;
#4897 = EDGE_LOOP('',(#23959,#23960,#23961,#23962)) ;
#4898 = EDGE_LOOP('',(#23963,#23964,#23965,#23966)) ;
#4899 = EDGE_LOOP('',(#23967,#23968,#23969,#23970)) ;
#4900 = EDGE_LOOP('',(#23971,#23972,#23973,#23974)) ;
#4901 = EDGE_LOOP('',(#23975,#23976,#23977,#23978)) ;
#4902 = EDGE_LOOP('',(#23979,#23980,#23981,#23982,#23983,#23984,#23985,#23986,
#23987,#23988)) ;
#4903 = EDGE_LOOP('',(#23989,#23990,#23991,#23992)) ;
#4904 = EDGE_LOOP('',(#23993,#23994,#23995,#23996)) ;
#4905 = EDGE_LOOP('',(#23997,#23998,#23999,#24000)) ;
#4906 = EDGE_LOOP('',(#24001,#24002,#24003,#24004)) ;
#4907 = EDGE_LOOP('',(#24005,#24006,#24007,#24008)) ;
#4908 = EDGE_LOOP('',(#24009,#24010,#24011,#24012)) ;
#4909 = EDGE_LOOP('',(#24013,#24014,#24015,#24016)) ;
#4910 = EDGE_LOOP('',(#24017,#24018,#24019,#24020)) ;
#4911 = EDGE_LOOP('',(#24021,#24022,#24023,#24024)) ;
#4912 = EDGE_LOOP('',(#24025,#24026,#24027,#24028)) ;
#4913 = EDGE_LOOP('',(#24029,#24030,#24031,#24032)) ;
#4914 = EDGE_LOOP('',(#24033,#24034,#24035,#24036,#24037,#24038,#24039,#24040,
#24041,#24042)) ;
#4915 = EDGE_LOOP('',(#24043,#24044,#24045,#24046)) ;
#4916 = EDGE_LOOP('',(#24047,#24048,#24049,#24050)) ;
#4917 = EDGE_LOOP('',(#24051,#24052,#24053,#24054)) ;
#4918 = EDGE_LOOP('',(#24055,#24056,#24057,#24058)) ;
#4919 = EDGE_LOOP('',(#24059,#24060,#24061,#24062)) ;
#4920 = EDGE_LOOP('',(#24063,#24064,#24065,#24066)) ;
#4921 = EDGE_LOOP('',(#24067,#24068,#24069,#24070)) ;
#4922 = EDGE_LOOP('',(#24071,#24072,#24073,#24074)) ;
#4923 = EDGE_LOOP('',(#24075,#24076,#24077,#24078)) ;
#4924 = EDGE_LOOP('',(#24079,#24080,#24081,#24082)) ;
#4925 = EDGE_LOOP('',(#24083,#24084,#24085,#24086)) ;
#4926 = EDGE_LOOP('',(#24087,#24088,#24089,#24090,#24091,#24092,#24093,#24094,
#24095,#24096)) ;
#4927 = EDGE_LOOP('',(#24097,#24098,#24099,#24100)) ;
#4928 = EDGE_LOOP('',(#24101,#24102,#24103,#24104)) ;
#4929 = EDGE_LOOP('',(#24105,#24106,#24107,#24108)) ;
#4930 = EDGE_LOOP('',(#24109,#24110,#24111,#24112)) ;
#4931 = EDGE_LOOP('',(#24113,#24114,#24115,#24116)) ;
#4932 = EDGE_LOOP('',(#24117,#24118,#24119,#24120)) ;
#4933 = EDGE_LOOP('',(#24121,#24122,#24123,#24124)) ;
#4934 = EDGE_LOOP('',(#24125,#24126,#24127,#24128)) ;
#4935 = EDGE_LOOP('',(#24129,#24130,#24131,#24132)) ;
#4936 = EDGE_LOOP('',(#24133,#24134,#24135,#24136)) ;
#4937 = EDGE_LOOP('',(#24137,#24138,#24139,#24140)) ;
#4938 = EDGE_LOOP('',(#24141,#24142,#24143,#24144,#24145,#24146,#24147,#24148,
#24149,#24150)) ;
#4939 = EDGE_LOOP('',(#24151,#24152,#24153,#24154)) ;
#4940 = EDGE_LOOP('',(#24155,#24156,#24157,#24158)) ;
#4941 = EDGE_LOOP('',(#24159,#24160,#24161,#24162)) ;
#4942 = EDGE_LOOP('',(#24163,#24164,#24165,#24166)) ;
#4943 = EDGE_LOOP('',(#24167,#24168,#24169,#24170)) ;
#4944 = EDGE_LOOP('',(#24171,#24172,#24173,#24174)) ;
#4945 = EDGE_LOOP('',(#24175,#24176,#24177,#24178)) ;
#4946 = EDGE_LOOP('',(#24179,#24180,#24181,#24182)) ;
#4947 = EDGE_LOOP('',(#24183,#24184,#24185,#24186)) ;
#4948 = EDGE_LOOP('',(#24187,#24188,#24189,#24190)) ;
#4949 = EDGE_LOOP('',(#24191,#24192,#24193,#24194)) ;
#4950 = EDGE_LOOP('',(#24195,#24196,#24197,#24198,#24199,#24200,#24201,#24202,
#24203,#24204)) ;
#4951 = EDGE_LOOP('',(#24205,#24206,#24207,#24208)) ;
#4952 = EDGE_LOOP('',(#24209,#24210,#24211,#24212)) ;
#4953 = EDGE_LOOP('',(#24213,#24214,#24215,#24216)) ;
#4954 = EDGE_LOOP('',(#24217,#24218,#24219,#24220)) ;
#4955 = EDGE_LOOP('',(#24221,#24222,#24223,#24224)) ;
#4956 = EDGE_LOOP('',(#24225,#24226,#24227,#24228)) ;
#4957 = EDGE_LOOP('',(#24229,#24230,#24231,#24232)) ;
#4958 = EDGE_LOOP('',(#24233,#24234,#24235,#24236)) ;
#4959 = EDGE_LOOP('',(#24237,#24238,#24239,#24240)) ;
#4960 = EDGE_LOOP('',(#24241,#24242,#24243,#24244)) ;
#4961 = EDGE_LOOP('',(#24245,#24246,#24247,#24248)) ;
#4962 = EDGE_LOOP('',(#24249,#24250,#24251,#24252,#24253,#24254,#24255,#24256,
#24257,#24258)) ;
#4963 = EDGE_LOOP('',(#24259,#24260,#24261,#24262)) ;
#4964 = EDGE_LOOP('',(#24263,#24264,#24265,#24266)) ;
#4965 = EDGE_LOOP('',(#24267,#24268,#24269,#24270)) ;
#4966 = EDGE_LOOP('',(#24271,#24272,#24273,#24274)) ;
#4967 = EDGE_LOOP('',(#24275,#24276,#24277,#24278)) ;
#4968 = EDGE_LOOP('',(#24279,#24280,#24281,#24282)) ;
#4969 = EDGE_LOOP('',(#24283,#24284,#24285,#24286)) ;
#4970 = EDGE_LOOP('',(#24287,#24288,#24289,#24290)) ;
#4971 = EDGE_LOOP('',(#24291,#24292,#24293,#24294)) ;
#4972 = EDGE_LOOP('',(#24295,#24296,#24297,#24298)) ;
#4973 = EDGE_LOOP('',(#24299,#24300,#24301,#24302)) ;
#4974 = EDGE_LOOP('',(#24303,#24304,#24305,#24306,#24307,#24308,#24309,#24310,
#24311,#24312)) ;
#4975 = EDGE_LOOP('',(#24313,#24314,#24315,#24316)) ;
#4976 = EDGE_LOOP('',(#24317,#24318,#24319,#24320)) ;
#4977 = EDGE_LOOP('',(#24321,#24322,#24323,#24324)) ;
#4978 = EDGE_LOOP('',(#24325,#24326,#24327,#24328)) ;
#4979 = EDGE_LOOP('',(#24329,#24330,#24331,#24332)) ;
#4980 = EDGE_LOOP('',(#24333,#24334,#24335,#24336)) ;
#4981 = EDGE_LOOP('',(#24337,#24338,#24339,#24340)) ;
#4982 = EDGE_LOOP('',(#24341,#24342,#24343,#24344)) ;
#4983 = EDGE_LOOP('',(#24345,#24346,#24347,#24348)) ;
#4984 = EDGE_LOOP('',(#24349,#24350,#24351,#24352)) ;
#4985 = EDGE_LOOP('',(#24353,#24354,#24355,#24356)) ;
#4986 = EDGE_LOOP('',(#24357,#24358,#24359,#24360,#24361,#24362,#24363,#24364,
#24365,#24366)) ;
#4987 = EDGE_LOOP('',(#24367,#24368,#24369,#24370)) ;
#4988 = EDGE_LOOP('',(#24371,#24372,#24373,#24374)) ;
#4989 = EDGE_LOOP('',(#24375,#24376,#24377,#24378)) ;
#4990 = EDGE_LOOP('',(#24379,#24380,#24381,#24382)) ;
#4991 = EDGE_LOOP('',(#24383,#24384,#24385,#24386)) ;
#4992 = EDGE_LOOP('',(#24387,#24388,#24389,#24390)) ;
#4993 = EDGE_LOOP('',(#24391,#24392,#24393,#24394)) ;
#4994 = EDGE_LOOP('',(#24395,#24396,#24397,#24398)) ;
#4995 = EDGE_LOOP('',(#24399,#24400,#24401,#24402)) ;
#4996 = EDGE_LOOP('',(#24403,#24404,#24405,#24406)) ;
#4997 = EDGE_LOOP('',(#24407,#24408,#24409,#24410)) ;
#4998 = EDGE_LOOP('',(#24411,#24412,#24413,#24414)) ;
#4999 = EDGE_LOOP('',(#24415,#24416,#24417,#24418)) ;
#5000 = EDGE_LOOP('',(#24419,#24420,#24421,#24422)) ;
#5001 = EDGE_LOOP('',(#24423,#24424,#24425,#24426)) ;
#5002 = EDGE_LOOP('',(#24427,#24428,#24429,#24430)) ;
#5003 = EDGE_LOOP('',(#24431,#24432,#24433,#24434)) ;
#5004 = EDGE_LOOP('',(#24435,#24436,#24437,#24438)) ;
#5005 = EDGE_LOOP('',(#24439,#24440,#24441,#24442)) ;
#5006 = EDGE_LOOP('',(#24443,#24444,#24445,#24446)) ;
#5007 = EDGE_LOOP('',(#24447,#24448,#24449,#24450)) ;
#5008 = EDGE_LOOP('',(#24451,#24452,#24453,#24454)) ;
#5009 = EDGE_LOOP('',(#24455,#24456,#24457,#24458)) ;
#5010 = EDGE_LOOP('',(#24459,#24460,#24461,#24462)) ;
#5011 = EDGE_LOOP('',(#24463,#24464,#24465,#24466)) ;
#5012 = EDGE_LOOP('',(#24467,#24468,#24469,#24470)) ;
#5013 = EDGE_LOOP('',(#24471,#24472,#24473,#24474)) ;
#5014 = EDGE_LOOP('',(#24475,#24476,#24477,#24478)) ;
#5015 = EDGE_LOOP('',(#24479,#24480,#24481,#24482)) ;
#5016 = EDGE_LOOP('',(#24483,#24484,#24485,#24486)) ;
#5017 = EDGE_LOOP('',(#24487,#24488,#24489,#24490)) ;
#5018 = EDGE_LOOP('',(#24491,#24492,#24493,#24494)) ;
#5019 = EDGE_LOOP('',(#24495,#24496,#24497,#24498)) ;
#5020 = EDGE_LOOP('',(#24499,#24500,#24501,#24502)) ;
#5021 = EDGE_LOOP('',(#24503,#24504,#24505,#24506)) ;
#5022 = EDGE_LOOP('',(#24507,#24508,#24509,#24510)) ;
#5023 = EDGE_LOOP('',(#24511,#24512,#24513,#24514)) ;
#5024 = EDGE_LOOP('',(#24515,#24516,#24517,#24518)) ;
#5025 = EDGE_LOOP('',(#24519,#24520,#24521,#24522)) ;
#5026 = EDGE_LOOP('',(#24523,#24524,#24525,#24526)) ;
#5027 = EDGE_LOOP('',(#24527,#24528,#24529,#24530)) ;
#5028 = EDGE_LOOP('',(#24531,#24532,#24533,#24534)) ;
#5029 = EDGE_LOOP('',(#24535,#24536,#24537,#24538)) ;
#5030 = EDGE_LOOP('',(#24539,#24540,#24541,#24542)) ;
#5031 = EDGE_LOOP('',(#24543,#24544,#24545,#24546)) ;
#5032 = EDGE_LOOP('',(#24547,#24548,#24549,#24550)) ;
#5033 = EDGE_LOOP('',(#24551,#24552,#24553,#24554)) ;
#5034 = EDGE_LOOP('',(#24555,#24556,#24557,#24558)) ;
#5035 = EDGE_LOOP('',(#24559,#24560,#24561,#24562)) ;
#5036 = EDGE_LOOP('',(#24563,#24564,#24565,#24566)) ;
#5037 = EDGE_LOOP('',(#24567,#24568,#24569,#24570)) ;
#5038 = EDGE_LOOP('',(#24571,#24572,#24573,#24574)) ;
#5039 = EDGE_LOOP('',(#24575,#24576,#24577,#24578)) ;
#5040 = EDGE_LOOP('',(#24579,#24580,#24581,#24582)) ;
#5041 = EDGE_LOOP('',(#24583,#24584,#24585,#24586)) ;
#5042 = EDGE_LOOP('',(#24587,#24588,#24589,#24590)) ;
#5043 = EDGE_LOOP('',(#24591,#24592,#24593,#24594)) ;
#5044 = EDGE_LOOP('',(#24595,#24596,#24597,#24598)) ;
#5045 = EDGE_LOOP('',(#24599,#24600,#24601,#24602)) ;
#5046 = EDGE_LOOP('',(#24603,#24604,#24605,#24606)) ;
#5047 = EDGE_LOOP('',(#24607,#24608,#24609,#24610)) ;
#5048 = EDGE_LOOP('',(#24611,#24612,#24613,#24614)) ;
#5049 = EDGE_LOOP('',(#24615,#24616,#24617,#24618)) ;
#5050 = EDGE_LOOP('',(#24619,#24620,#24621,#24622)) ;
#5051 = EDGE_LOOP('',(#24623,#24624,#24625,#24626)) ;
#5052 = EDGE_LOOP('',(#24627,#24628,#24629,#24630)) ;
#5053 = EDGE_LOOP('',(#24631,#24632,#24633,#24634)) ;
#5054 = EDGE_LOOP('',(#24635,#24636,#24637,#24638)) ;
#5055 = EDGE_LOOP('',(#24639,#24640,#24641,#24642)) ;
#5056 = EDGE_LOOP('',(#24643,#24644,#24645,#24646)) ;
#5057 = EDGE_LOOP('',(#24647,#24648,#24649,#24650)) ;
#5058 = EDGE_LOOP('',(#24651,#24652,#24653,#24654)) ;
#5059 = EDGE_LOOP('',(#24655,#24656,#24657,#24658)) ;
#5060 = EDGE_LOOP('',(#24659,#24660,#24661,#24662)) ;
#5061 = EDGE_LOOP('',(#24663,#24664,#24665,#24666)) ;
#5062 = EDGE_LOOP('',(#24667,#24668,#24669,#24670)) ;
#5063 = EDGE_LOOP('',(#24671,#24672,#24673,#24674)) ;
#5064 = EDGE_LOOP('',(#24675,#24676,#24677,#24678)) ;
#5065 = EDGE_LOOP('',(#24679,#24680,#24681,#24682)) ;
#5066 = EDGE_LOOP('',(#24683,#24684,#24685,#24686)) ;
#5067 = EDGE_LOOP('',(#24687,#24688,#24689,#24690)) ;
#5068 = EDGE_LOOP('',(#24691,#24692,#24693,#24694)) ;
#5069 = EDGE_LOOP('',(#24695,#24696,#24697,#24698)) ;
#5070 = EDGE_LOOP('',(#24699,#24700,#24701,#24702)) ;
#5071 = EDGE_LOOP('',(#24703,#24704,#24705,#24706)) ;
#5072 = EDGE_LOOP('',(#24707,#24708,#24709,#24710)) ;
#5073 = EDGE_LOOP('',(#24711,#24712,#24713,#24714)) ;
#5074 = EDGE_LOOP('',(#24715,#24716,#24717,#24718)) ;
#5075 = EDGE_LOOP('',(#24719,#24720,#24721,#24722)) ;
#5076 = EDGE_LOOP('',(#24723,#24724,#24725,#24726)) ;
#5077 = EDGE_LOOP('',(#24727,#24728,#24729,#24730)) ;
#5078 = EDGE_LOOP('',(#24731,#24732,#24733,#24734)) ;
#5079 = EDGE_LOOP('',(#24735,#24736,#24737,#24738)) ;
#5080 = EDGE_LOOP('',(#24739,#24740,#24741,#24742)) ;
#5081 = EDGE_LOOP('',(#24743,#24744,#24745,#24746)) ;
#5082 = EDGE_LOOP('',(#24747,#24748,#24749,#24750)) ;
#5083 = EDGE_LOOP('',(#24751,#24752,#24753,#24754)) ;
#5084 = EDGE_LOOP('',(#24755,#24756,#24757,#24758)) ;
#5085 = EDGE_LOOP('',(#24759,#24760,#24761,#24762)) ;
#5086 = EDGE_LOOP('',(#24763,#24764,#24765,#24766)) ;
#5087 = EDGE_LOOP('',(#24767,#24768,#24769,#24770)) ;
#5088 = EDGE_LOOP('',(#24771,#24772,#24773,#24774)) ;
#5089 = EDGE_LOOP('',(#24775,#24776,#24777,#24778)) ;
#5090 = EDGE_LOOP('',(#24779,#24780,#24781,#24782)) ;
#5091 = EDGE_LOOP('',(#24783,#24784,#24785,#24786)) ;
#5092 = EDGE_LOOP('',(#24787,#24788,#24789,#24790)) ;
#5093 = EDGE_LOOP('',(#24791,#24792,#24793,#24794)) ;
#5094 = EDGE_LOOP('',(#24795,#24796,#24797,#24798,#24799,#24800,#24801,#24802,
#24803,#24804)) ;
#5095 = EDGE_LOOP('',(#24805,#24806,#24807,#24808)) ;
#5096 = EDGE_LOOP('',(#24809,#24810,#24811,#24812)) ;
#5097 = EDGE_LOOP('',(#24813,#24814,#24815,#24816)) ;
#5098 = EDGE_LOOP('',(#24817,#24818,#24819,#24820)) ;
#5099 = EDGE_LOOP('',(#24821,#24822,#24823,#24824)) ;
#5100 = EDGE_LOOP('',(#24825,#24826,#24827,#24828)) ;
#5101 = EDGE_LOOP('',(#24829,#24830,#24831,#24832)) ;
#5102 = EDGE_LOOP('',(#24833,#24834,#24835,#24836)) ;
#5103 = EDGE_LOOP('',(#24837,#24838,#24839,#24840)) ;
#5104 = EDGE_LOOP('',(#24841,#24842,#24843,#24844)) ;
#5105 = EDGE_LOOP('',(#24845,#24846,#24847,#24848)) ;
#5106 = EDGE_LOOP('',(#24849,#24850,#24851,#24852,#24853,#24854,#24855,#24856,
#24857,#24858)) ;
#5107 = EDGE_LOOP('',(#24859,#24860,#24861,#24862)) ;
#5108 = EDGE_LOOP('',(#24863,#24864,#24865,#24866)) ;
#5109 = EDGE_LOOP('',(#24867,#24868,#24869,#24870)) ;
#5110 = EDGE_LOOP('',(#24871,#24872,#24873,#24874)) ;
#5111 = EDGE_LOOP('',(#24875,#24876,#24877,#24878)) ;
#5112 = EDGE_LOOP('',(#24879,#24880,#24881,#24882)) ;
#5113 = EDGE_LOOP('',(#24883,#24884,#24885,#24886)) ;
#5114 = EDGE_LOOP('',(#24887,#24888,#24889,#24890)) ;
#5115 = EDGE_LOOP('',(#24891,#24892,#24893,#24894)) ;
#5116 = EDGE_LOOP('',(#24895,#24896,#24897,#24898)) ;
#5117 = EDGE_LOOP('',(#24899,#24900,#24901,#24902)) ;
#5118 = EDGE_LOOP('',(#24903,#24904,#24905,#24906,#24907,#24908,#24909,#24910,
#24911,#24912)) ;
#5119 = EDGE_LOOP('',(#24913,#24914,#24915,#24916)) ;
#5120 = EDGE_LOOP('',(#24917,#24918,#24919,#24920)) ;
#5121 = EDGE_LOOP('',(#24921,#24922,#24923,#24924)) ;
#5122 = EDGE_LOOP('',(#24925,#24926,#24927,#24928)) ;
#5123 = EDGE_LOOP('',(#24929,#24930,#24931,#24932)) ;
#5124 = EDGE_LOOP('',(#24933,#24934,#24935,#24936)) ;
#5125 = EDGE_LOOP('',(#24937,#24938,#24939,#24940)) ;
#5126 = EDGE_LOOP('',(#24941,#24942,#24943,#24944)) ;
#5127 = EDGE_LOOP('',(#24945,#24946,#24947,#24948)) ;
#5128 = EDGE_LOOP('',(#24949,#24950,#24951,#24952)) ;
#5129 = EDGE_LOOP('',(#24953,#24954,#24955,#24956)) ;
#5130 = EDGE_LOOP('',(#24957,#24958,#24959,#24960,#24961,#24962,#24963,#24964,
#24965,#24966)) ;
#5131 = EDGE_LOOP('',(#24967,#24968,#24969,#24970)) ;
#5132 = EDGE_LOOP('',(#24971,#24972,#24973,#24974)) ;
#5133 = EDGE_LOOP('',(#24975,#24976,#24977,#24978)) ;
#5134 = EDGE_LOOP('',(#24979,#24980,#24981,#24982)) ;
#5135 = EDGE_LOOP('',(#24983,#24984,#24985,#24986)) ;
#5136 = EDGE_LOOP('',(#24987,#24988,#24989,#24990)) ;
#5137 = EDGE_LOOP('',(#24991,#24992,#24993,#24994)) ;
#5138 = EDGE_LOOP('',(#24995,#24996,#24997,#24998)) ;
#5139 = EDGE_LOOP('',(#24999,#25000,#25001,#25002)) ;
#5140 = EDGE_LOOP('',(#25003,#25004,#25005,#25006)) ;
#5141 = EDGE_LOOP('',(#25007,#25008,#25009,#25010)) ;
#5142 = EDGE_LOOP('',(#25011,#25012,#25013,#25014,#25015,#25016,#25017,#25018,
#25019,#25020)) ;
#5143 = EDGE_LOOP('',(#25021,#25022,#25023,#25024)) ;
#5144 = EDGE_LOOP('',(#25025,#25026,#25027,#25028)) ;
#5145 = EDGE_LOOP('',(#25029,#25030,#25031,#25032)) ;
#5146 = EDGE_LOOP('',(#25033,#25034,#25035,#25036)) ;
#5147 = EDGE_LOOP('',(#25037,#25038,#25039,#25040)) ;
#5148 = EDGE_LOOP('',(#25041,#25042,#25043,#25044)) ;
#5149 = EDGE_LOOP('',(#25045,#25046,#25047,#25048)) ;
#5150 = EDGE_LOOP('',(#25049,#25050,#25051,#25052)) ;
#5151 = EDGE_LOOP('',(#25053,#25054,#25055,#25056)) ;
#5152 = EDGE_LOOP('',(#25057,#25058,#25059,#25060)) ;
#5153 = EDGE_LOOP('',(#25061,#25062,#25063,#25064)) ;
#5154 = EDGE_LOOP('',(#25065,#25066,#25067,#25068,#25069,#25070,#25071,#25072,
#25073,#25074)) ;
#5155 = EDGE_LOOP('',(#25075,#25076,#25077,#25078)) ;
#5156 = EDGE_LOOP('',(#25079,#25080,#25081,#25082)) ;
#5157 = EDGE_LOOP('',(#25083,#25084,#25085,#25086)) ;
#5158 = EDGE_LOOP('',(#25087,#25088,#25089,#25090)) ;
#5159 = EDGE_LOOP('',(#25091,#25092,#25093,#25094)) ;
#5160 = EDGE_LOOP('',(#25095,#25096,#25097,#25098)) ;
#5161 = EDGE_LOOP('',(#25099,#25100,#25101,#25102)) ;
#5162 = EDGE_LOOP('',(#25103,#25104,#25105,#25106)) ;
#5163 = EDGE_LOOP('',(#25107,#25108,#25109,#25110)) ;
#5164 = EDGE_LOOP('',(#25111,#25112,#25113,#25114)) ;
#5165 = EDGE_LOOP('',(#25115,#25116,#25117,#25118)) ;
#5166 = EDGE_LOOP('',(#25119,#25120,#25121,#25122,#25123,#25124,#25125,#25126,
#25127,#25128)) ;
#5167 = EDGE_LOOP('',(#25129,#25130,#25131,#25132)) ;
#5168 = EDGE_LOOP('',(#25133,#25134,#25135,#25136)) ;
#5169 = EDGE_LOOP('',(#25137,#25138,#25139,#25140)) ;
#5170 = EDGE_LOOP('',(#25141,#25142,#25143,#25144)) ;
#5171 = EDGE_LOOP('',(#25145,#25146,#25147,#25148)) ;
#5172 = EDGE_LOOP('',(#25149,#25150,#25151,#25152)) ;
#5173 = EDGE_LOOP('',(#25153,#25154,#25155,#25156)) ;
#5174 = EDGE_LOOP('',(#25157,#25158,#25159,#25160)) ;
#5175 = EDGE_LOOP('',(#25161,#25162,#25163,#25164)) ;
#5176 = EDGE_LOOP('',(#25165,#25166,#25167,#25168)) ;
#5177 = EDGE_LOOP('',(#25169,#25170,#25171,#25172)) ;
#5178 = EDGE_LOOP('',(#25173,#25174,#25175,#25176,#25177,#25178,#25179,#25180,
#25181,#25182)) ;
#5179 = EDGE_LOOP('',(#25183,#25184,#25185,#25186)) ;
#5180 = EDGE_LOOP('',(#25187,#25188,#25189,#25190)) ;
#5181 = EDGE_LOOP('',(#25191,#25192,#25193,#25194)) ;
#5182 = EDGE_LOOP('',(#25195,#25196,#25197,#25198)) ;
#5183 = EDGE_LOOP('',(#25199,#25200,#25201,#25202)) ;
#5184 = EDGE_LOOP('',(#25203,#25204,#25205,#25206)) ;
#5185 = EDGE_LOOP('',(#25207,#25208,#25209,#25210)) ;
#5186 = EDGE_LOOP('',(#25211,#25212,#25213,#25214)) ;
#5187 = EDGE_LOOP('',(#25215,#25216,#25217,#25218)) ;
#5188 = EDGE_LOOP('',(#25219,#25220,#25221,#25222)) ;
#5189 = EDGE_LOOP('',(#25223,#25224,#25225,#25226)) ;
#5190 = EDGE_LOOP('',(#25227,#25228,#25229,#25230)) ;
#5191 = EDGE_LOOP('',(#25231,#25232,#25233,#25234)) ;
#5192 = EDGE_LOOP('',(#25235,#25236,#25237,#25238)) ;
#5193 = EDGE_LOOP('',(#25239,#25240,#25241,#25242)) ;
#5194 = EDGE_LOOP('',(#25243,#25244,#25245,#25246,#25247,#25248,#25249,#25250)) ;
#5195 = EDGE_LOOP('',(#25251)) ;
#5196 = EDGE_LOOP('',(#25252,#25253,#25254,#25255,#25256,#25257,#25258,#25259)) ;
#5197 = EDGE_LOOP('',(#25260,#25261,#25262,#25263)) ;
#5198 = EDGE_LOOP('',(#25264,#25265,#25266,#25267)) ;
#5199 = EDGE_LOOP('',(#25268,#25269,#25270,#25271)) ;
#5200 = EDGE_LOOP('',(#25272,#25273,#25274,#25275)) ;
#5201 = EDGE_LOOP('',(#25276,#25277,#25278,#25279)) ;
#5202 = EDGE_LOOP('',(#25280,#25281,#25282,#25283)) ;
#5203 = EDGE_LOOP('',(#25284,#25285,#25286,#25287)) ;
#5204 = EDGE_LOOP('',(#25288,#25289,#25290,#25291)) ;
#5205 = EDGE_LOOP('',(#25292,#25293,#25294,#25295)) ;
#5206 = EDGE_LOOP('',(#25296,#25297,#25298,#25299,#25300,#25301,#25302,#25303,
#25304,#25305)) ;
#5207 = EDGE_LOOP('',(#25306,#25307,#25308,#25309)) ;
#5208 = EDGE_LOOP('',(#25310,#25311,#25312,#25313)) ;
#5209 = EDGE_LOOP('',(#25314,#25315,#25316,#25317)) ;
#5210 = EDGE_LOOP('',(#25318,#25319,#25320,#25321)) ;
#5211 = EDGE_LOOP('',(#25322,#25323,#25324,#25325)) ;
#5212 = EDGE_LOOP('',(#25326,#25327,#25328,#25329)) ;
#5213 = EDGE_LOOP('',(#25330,#25331,#25332,#25333)) ;
#5214 = EDGE_LOOP('',(#25334,#25335,#25336,#25337)) ;
#5215 = EDGE_LOOP('',(#25338,#25339,#25340,#25341)) ;
#5216 = EDGE_LOOP('',(#25342)) ;
#5217 = EDGE_LOOP('',(#25343)) ;
#5218 = EDGE_LOOP('',(#25344,#25345,#25346,#25347)) ;
#5219 = EDGE_LOOP('',(#25348,#25349,#25350,#25351)) ;
#5220 = EDGE_LOOP('',(#25352,#25353,#25354,#25355)) ;
#5221 = EDGE_LOOP('',(#25356,#25357,#25358,#25359)) ;
#5222 = EDGE_LOOP('',(#25360,#25361,#25362,#25363)) ;
#5223 = EDGE_LOOP('',(#25364,#25365,#25366,#25367)) ;
#5224 = EDGE_LOOP('',(#25368,#25369,#25370,#25371)) ;
#5225 = EDGE_LOOP('',(#25372,#25373,#25374,#25375)) ;
#5226 = EDGE_LOOP('',(#25376,#25377,#25378,#25379)) ;
#5227 = EDGE_LOOP('',(#25380,#25381,#25382,#25383)) ;
#5228 = EDGE_LOOP('',(#25384,#25385,#25386,#25387)) ;
#5229 = EDGE_LOOP('',(#25388,#25389,#25390,#25391)) ;
#5230 = EDGE_LOOP('',(#25392,#25393,#25394,#25395)) ;
#5231 = EDGE_LOOP('',(#25396,#25397,#25398)) ;
#5232 = EDGE_LOOP('',(#25399,#25400,#25401)) ;
#5233 = EDGE_LOOP('',(#25402,#25403,#25404,#25405)) ;
#5234 = EDGE_LOOP('',(#25406,#25407,#25408)) ;
#5235 = EDGE_LOOP('',(#25409,#25410,#25411)) ;
#5236 = EDGE_LOOP('',(#25412,#25413,#25414,#25415)) ;
#5237 = EDGE_LOOP('',(#25416,#25417,#25418,#25419)) ;
#5238 = EDGE_LOOP('',(#25420,#25421,#25422,#25423)) ;
#5239 = EDGE_LOOP('',(#25424,#25425,#25426,#25427)) ;
#5240 = EDGE_LOOP('',(#25428,#25429,#25430)) ;
#5241 = EDGE_LOOP('',(#25431,#25432,#25433)) ;
#5242 = EDGE_LOOP('',(#25434,#25435,#25436,#25437)) ;
#5243 = EDGE_LOOP('',(#25438,#25439,#25440,#25441)) ;
#5244 = EDGE_LOOP('',(#25442,#25443,#25444,#25445)) ;
#5245 = EDGE_LOOP('',(#25446,#25447,#25448,#25449)) ;
#5246 = EDGE_LOOP('',(#25450,#25451,#25452)) ;
#5247 = EDGE_LOOP('',(#25453,#25454,#25455)) ;
#5248 = EDGE_LOOP('',(#25456,#25457,#25458,#25459)) ;
#5249 = EDGE_LOOP('',(#25460,#25461,#25462,#25463)) ;
#5250 = EDGE_LOOP('',(#25464,#25465,#25466,#25467)) ;
#5251 = EDGE_LOOP('',(#25468,#25469,#25470,#25471)) ;
#5252 = EDGE_LOOP('',(#25472,#25473,#25474,#25475)) ;
#5253 = EDGE_LOOP('',(#25476,#25477,#25478,#25479)) ;
#5254 = EDGE_LOOP('',(#25480,#25481,#25482,#25483)) ;
#5255 = EDGE_LOOP('',(#25484,#25485,#25486,#25487)) ;
#5256 = EDGE_LOOP('',(#25488,#25489,#25490,#25491)) ;
#5257 = EDGE_LOOP('',(#25492,#25493,#25494,#25495)) ;
#5258 = EDGE_LOOP('',(#25496,#25497,#25498,#25499)) ;
#5259 = EDGE_LOOP('',(#25500,#25501,#25502,#25503)) ;
#5260 = EDGE_LOOP('',(#25504,#25505,#25506,#25507)) ;
#5261 = EDGE_LOOP('',(#25508,#25509,#25510)) ;
#5262 = EDGE_LOOP('',(#25511,#25512,#25513)) ;
#5263 = EDGE_LOOP('',(#25514,#25515,#25516,#25517)) ;
#5264 = EDGE_LOOP('',(#25518,#25519,#25520)) ;
#5265 = EDGE_LOOP('',(#25521,#25522,#25523)) ;
#5266 = EDGE_LOOP('',(#25524,#25525,#25526,#25527)) ;
#5267 = EDGE_LOOP('',(#25528,#25529,#25530,#25531)) ;
#5268 = EDGE_LOOP('',(#25532,#25533,#25534,#25535)) ;
#5269 = EDGE_LOOP('',(#25536,#25537,#25538,#25539)) ;
#5270 = EDGE_LOOP('',(#25540,#25541,#25542)) ;
#5271 = EDGE_LOOP('',(#25543,#25544,#25545)) ;
#5272 = EDGE_LOOP('',(#25546,#25547,#25548,#25549)) ;
#5273 = EDGE_LOOP('',(#25550,#25551,#25552,#25553)) ;
#5274 = EDGE_LOOP('',(#25554,#25555,#25556,#25557)) ;
#5275 = EDGE_LOOP('',(#25558,#25559,#25560,#25561)) ;
#5276 = EDGE_LOOP('',(#25562,#25563,#25564)) ;
#5277 = EDGE_LOOP('',(#25565,#25566,#25567)) ;
#5278 = EDGE_LOOP('',(#25568,#25569,#25570,#25571)) ;
#5279 = EDGE_LOOP('',(#25572,#25573,#25574,#25575)) ;
#5280 = EDGE_LOOP('',(#25576,#25577,#25578,#25579)) ;
#5281 = EDGE_LOOP('',(#25580,#25581,#25582,#25583)) ;
#5282 = EDGE_LOOP('',(#25584,#25585,#25586,#25587)) ;
#5283 = EDGE_LOOP('',(#25588,#25589,#25590,#25591)) ;
#5284 = EDGE_LOOP('',(#25592,#25593,#25594,#25595)) ;
#5285 = EDGE_LOOP('',(#25596,#25597,#25598,#25599)) ;
#5286 = EDGE_LOOP('',(#25600,#25601,#25602,#25603)) ;
#5287 = EDGE_LOOP('',(#25604,#25605,#25606,#25607)) ;
#5288 = EDGE_LOOP('',(#25608,#25609,#25610,#25611)) ;
#5289 = EDGE_LOOP('',(#25612,#25613,#25614,#25615)) ;
#5290 = EDGE_LOOP('',(#25616,#25617,#25618,#25619)) ;
#5291 = EDGE_LOOP('',(#25620,#25621,#25622)) ;
#5292 = EDGE_LOOP('',(#25623,#25624,#25625)) ;
#5293 = EDGE_LOOP('',(#25626,#25627,#25628,#25629)) ;
#5294 = EDGE_LOOP('',(#25630,#25631,#25632)) ;
#5295 = EDGE_LOOP('',(#25633,#25634,#25635)) ;
#5296 = EDGE_LOOP('',(#25636,#25637,#25638,#25639)) ;
#5297 = EDGE_LOOP('',(#25640,#25641,#25642,#25643)) ;
#5298 = EDGE_LOOP('',(#25644,#25645,#25646,#25647)) ;
#5299 = EDGE_LOOP('',(#25648,#25649,#25650,#25651)) ;
#5300 = EDGE_LOOP('',(#25652,#25653,#25654)) ;
#5301 = EDGE_LOOP('',(#25655,#25656,#25657)) ;
#5302 = EDGE_LOOP('',(#25658,#25659,#25660,#25661)) ;
#5303 = EDGE_LOOP('',(#25662,#25663,#25664,#25665)) ;
#5304 = EDGE_LOOP('',(#25666,#25667,#25668,#25669)) ;
#5305 = EDGE_LOOP('',(#25670,#25671,#25672,#25673)) ;
#5306 = EDGE_LOOP('',(#25674,#25675,#25676)) ;
#5307 = EDGE_LOOP('',(#25677,#25678,#25679)) ;
#5308 = EDGE_LOOP('',(#25680,#25681,#25682,#25683)) ;
#5309 = EDGE_LOOP('',(#25684,#25685,#25686,#25687)) ;
#5310 = EDGE_LOOP('',(#25688,#25689,#25690,#25691)) ;
#5311 = EDGE_LOOP('',(#25692,#25693,#25694,#25695)) ;
#5312 = EDGE_LOOP('',(#25696,#25697,#25698,#25699)) ;
#5313 = EDGE_LOOP('',(#25700,#25701,#25702,#25703)) ;
#5314 = EDGE_LOOP('',(#25704,#25705,#25706,#25707)) ;
#5315 = EDGE_LOOP('',(#25708,#25709,#25710,#25711)) ;
#5316 = EDGE_LOOP('',(#25712,#25713,#25714,#25715)) ;
#5317 = EDGE_LOOP('',(#25716,#25717,#25718,#25719)) ;
#5318 = EDGE_LOOP('',(#25720,#25721,#25722,#25723)) ;
#5319 = EDGE_LOOP('',(#25724,#25725,#25726,#25727)) ;
#5320 = EDGE_LOOP('',(#25728,#25729,#25730,#25731)) ;
#5321 = EDGE_LOOP('',(#25732,#25733,#25734)) ;
#5322 = EDGE_LOOP('',(#25735,#25736,#25737)) ;
#5323 = EDGE_LOOP('',(#25738,#25739,#25740,#25741)) ;
#5324 = EDGE_LOOP('',(#25742,#25743,#25744)) ;
#5325 = EDGE_LOOP('',(#25745,#25746,#25747)) ;
#5326 = EDGE_LOOP('',(#25748,#25749,#25750,#25751)) ;
#5327 = EDGE_LOOP('',(#25752,#25753,#25754,#25755)) ;
#5328 = EDGE_LOOP('',(#25756,#25757,#25758,#25759)) ;
#5329 = EDGE_LOOP('',(#25760,#25761,#25762,#25763)) ;
#5330 = EDGE_LOOP('',(#25764,#25765,#25766)) ;
#5331 = EDGE_LOOP('',(#25767,#25768,#25769)) ;
#5332 = EDGE_LOOP('',(#25770,#25771,#25772,#25773)) ;
#5333 = EDGE_LOOP('',(#25774,#25775,#25776,#25777)) ;
#5334 = EDGE_LOOP('',(#25778,#25779,#25780,#25781)) ;
#5335 = EDGE_LOOP('',(#25782,#25783,#25784,#25785)) ;
#5336 = EDGE_LOOP('',(#25786,#25787,#25788)) ;
#5337 = EDGE_LOOP('',(#25789,#25790,#25791)) ;
#5338 = EDGE_LOOP('',(#25792,#25793,#25794,#25795)) ;
#5339 = EDGE_LOOP('',(#25796,#25797,#25798,#25799)) ;
#5340 = EDGE_LOOP('',(#25800,#25801,#25802,#25803)) ;
#5341 = EDGE_LOOP('',(#25804,#25805,#25806,#25807)) ;
#5342 = EDGE_LOOP('',(#25808,#25809,#25810,#25811)) ;
#5343 = EDGE_LOOP('',(#25812,#25813,#25814,#25815)) ;
#5344 = EDGE_LOOP('',(#25816,#25817,#25818,#25819)) ;
#5345 = EDGE_LOOP('',(#25820,#25821,#25822,#25823)) ;
#5346 = EDGE_LOOP('',(#25824,#25825,#25826,#25827)) ;
#5347 = EDGE_LOOP('',(#25828,#25829,#25830,#25831)) ;
#5348 = EDGE_LOOP('',(#25832,#25833,#25834,#25835)) ;
#5349 = EDGE_LOOP('',(#25836,#25837,#25838,#25839)) ;
#5350 = EDGE_LOOP('',(#25840,#25841,#25842,#25843)) ;
#5351 = EDGE_LOOP('',(#25844,#25845,#25846)) ;
#5352 = EDGE_LOOP('',(#25847,#25848,#25849)) ;
#5353 = EDGE_LOOP('',(#25850,#25851,#25852,#25853)) ;
#5354 = EDGE_LOOP('',(#25854,#25855,#25856)) ;
#5355 = EDGE_LOOP('',(#25857,#25858,#25859)) ;
#5356 = EDGE_LOOP('',(#25860,#25861,#25862,#25863)) ;
#5357 = EDGE_LOOP('',(#25864,#25865,#25866,#25867)) ;
#5358 = EDGE_LOOP('',(#25868,#25869,#25870,#25871)) ;
#5359 = EDGE_LOOP('',(#25872,#25873,#25874,#25875)) ;
#5360 = EDGE_LOOP('',(#25876,#25877,#25878)) ;
#5361 = EDGE_LOOP('',(#25879,#25880,#25881)) ;
#5362 = EDGE_LOOP('',(#25882,#25883,#25884,#25885)) ;
#5363 = EDGE_LOOP('',(#25886,#25887,#25888,#25889)) ;
#5364 = EDGE_LOOP('',(#25890,#25891,#25892,#25893)) ;
#5365 = EDGE_LOOP('',(#25894,#25895,#25896,#25897)) ;
#5366 = EDGE_LOOP('',(#25898,#25899,#25900)) ;
#5367 = EDGE_LOOP('',(#25901,#25902,#25903)) ;
#5368 = EDGE_LOOP('',(#25904,#25905,#25906,#25907)) ;
#5369 = EDGE_LOOP('',(#25908,#25909,#25910,#25911)) ;
#5370 = EDGE_LOOP('',(#25912,#25913,#25914,#25915)) ;
#5371 = EDGE_LOOP('',(#25916,#25917,#25918,#25919)) ;
#5372 = EDGE_LOOP('',(#25920,#25921,#25922,#25923)) ;
#5373 = EDGE_LOOP('',(#25924,#25925,#25926,#25927)) ;
#5374 = EDGE_LOOP('',(#25928,#25929,#25930,#25931)) ;
#5375 = EDGE_LOOP('',(#25932,#25933,#25934,#25935)) ;
#5376 = EDGE_LOOP('',(#25936,#25937,#25938,#25939)) ;
#5377 = EDGE_LOOP('',(#25940,#25941,#25942,#25943)) ;
#5378 = EDGE_LOOP('',(#25944,#25945,#25946,#25947)) ;
#5379 = EDGE_LOOP('',(#25948,#25949,#25950,#25951)) ;
#5380 = EDGE_LOOP('',(#25952,#25953,#25954,#25955)) ;
#5381 = EDGE_LOOP('',(#25956,#25957,#25958)) ;
#5382 = EDGE_LOOP('',(#25959,#25960,#25961)) ;
#5383 = EDGE_LOOP('',(#25962,#25963,#25964,#25965)) ;
#5384 = EDGE_LOOP('',(#25966,#25967,#25968)) ;
#5385 = EDGE_LOOP('',(#25969,#25970,#25971)) ;
#5386 = EDGE_LOOP('',(#25972,#25973,#25974,#25975)) ;
#5387 = EDGE_LOOP('',(#25976,#25977,#25978,#25979)) ;
#5388 = EDGE_LOOP('',(#25980,#25981,#25982,#25983)) ;
#5389 = EDGE_LOOP('',(#25984,#25985,#25986,#25987)) ;
#5390 = EDGE_LOOP('',(#25988,#25989,#25990)) ;
#5391 = EDGE_LOOP('',(#25991,#25992,#25993)) ;
#5392 = EDGE_LOOP('',(#25994,#25995,#25996,#25997)) ;
#5393 = EDGE_LOOP('',(#25998,#25999,#26000,#26001)) ;
#5394 = EDGE_LOOP('',(#26002,#26003,#26004,#26005)) ;
#5395 = EDGE_LOOP('',(#26006,#26007,#26008,#26009)) ;
#5396 = EDGE_LOOP('',(#26010,#26011,#26012)) ;
#5397 = EDGE_LOOP('',(#26013,#26014,#26015)) ;
#5398 = EDGE_LOOP('',(#26016,#26017,#26018,#26019)) ;
#5399 = EDGE_LOOP('',(#26020,#26021,#26022,#26023)) ;
#5400 = EDGE_LOOP('',(#26024,#26025,#26026,#26027)) ;
#5401 = EDGE_LOOP('',(#26028,#26029,#26030,#26031)) ;
#5402 = EDGE_LOOP('',(#26032,#26033,#26034,#26035)) ;
#5403 = EDGE_LOOP('',(#26036,#26037,#26038,#26039)) ;
#5404 = EDGE_LOOP('',(#26040,#26041,#26042,#26043)) ;
#5405 = EDGE_LOOP('',(#26044,#26045,#26046,#26047)) ;
#5406 = EDGE_LOOP('',(#26048,#26049,#26050,#26051)) ;
#5407 = EDGE_LOOP('',(#26052,#26053,#26054,#26055)) ;
#5408 = EDGE_LOOP('',(#26056,#26057,#26058,#26059)) ;
#5409 = EDGE_LOOP('',(#26060,#26061,#26062,#26063)) ;
#5410 = EDGE_LOOP('',(#26064,#26065,#26066,#26067)) ;
#5411 = EDGE_LOOP('',(#26068,#26069,#26070)) ;
#5412 = EDGE_LOOP('',(#26071,#26072,#26073)) ;
#5413 = EDGE_LOOP('',(#26074,#26075,#26076,#26077)) ;
#5414 = EDGE_LOOP('',(#26078,#26079,#26080)) ;
#5415 = EDGE_LOOP('',(#26081,#26082,#26083)) ;
#5416 = EDGE_LOOP('',(#26084,#26085,#26086,#26087)) ;
#5417 = EDGE_LOOP('',(#26088,#26089,#26090,#26091)) ;
#5418 = EDGE_LOOP('',(#26092,#26093,#26094,#26095)) ;
#5419 = EDGE_LOOP('',(#26096,#26097,#26098,#26099)) ;
#5420 = EDGE_LOOP('',(#26100,#26101,#26102)) ;
#5421 = EDGE_LOOP('',(#26103,#26104,#26105)) ;
#5422 = EDGE_LOOP('',(#26106,#26107,#26108,#26109)) ;
#5423 = EDGE_LOOP('',(#26110,#26111,#26112,#26113)) ;
#5424 = EDGE_LOOP('',(#26114,#26115,#26116,#26117)) ;
#5425 = EDGE_LOOP('',(#26118,#26119,#26120,#26121)) ;
#5426 = EDGE_LOOP('',(#26122,#26123,#26124)) ;
#5427 = EDGE_LOOP('',(#26125,#26126,#26127)) ;
#5428 = EDGE_LOOP('',(#26128,#26129,#26130,#26131)) ;
#5429 = EDGE_LOOP('',(#26132,#26133,#26134,#26135)) ;
#5430 = EDGE_LOOP('',(#26136,#26137,#26138,#26139)) ;
#5431 = EDGE_LOOP('',(#26140,#26141,#26142,#26143)) ;
#5432 = EDGE_LOOP('',(#26144,#26145,#26146,#26147)) ;
#5433 = EDGE_LOOP('',(#26148,#26149,#26150,#26151)) ;
#5434 = EDGE_LOOP('',(#26152,#26153,#26154,#26155)) ;
#5435 = EDGE_LOOP('',(#26156,#26157,#26158,#26159)) ;
#5436 = EDGE_LOOP('',(#26160,#26161,#26162,#26163)) ;
#5437 = EDGE_LOOP('',(#26164,#26165,#26166,#26167)) ;
#5438 = EDGE_LOOP('',(#26168,#26169,#26170,#26171)) ;
#5439 = EDGE_LOOP('',(#26172,#26173,#26174,#26175)) ;
#5440 = EDGE_LOOP('',(#26176,#26177,#26178,#26179)) ;
#5441 = EDGE_LOOP('',(#26180,#26181,#26182)) ;
#5442 = EDGE_LOOP('',(#26183,#26184,#26185)) ;
#5443 = EDGE_LOOP('',(#26186,#26187,#26188,#26189)) ;
#5444 = EDGE_LOOP('',(#26190,#26191,#26192)) ;
#5445 = EDGE_LOOP('',(#26193,#26194,#26195)) ;
#5446 = EDGE_LOOP('',(#26196,#26197,#26198,#26199)) ;
#5447 = EDGE_LOOP('',(#26200,#26201,#26202,#26203)) ;
#5448 = EDGE_LOOP('',(#26204,#26205,#26206,#26207)) ;
#5449 = EDGE_LOOP('',(#26208,#26209,#26210,#26211)) ;
#5450 = EDGE_LOOP('',(#26212,#26213,#26214)) ;
#5451 = EDGE_LOOP('',(#26215,#26216,#26217)) ;
#5452 = EDGE_LOOP('',(#26218,#26219,#26220,#26221)) ;
#5453 = EDGE_LOOP('',(#26222,#26223,#26224,#26225)) ;
#5454 = EDGE_LOOP('',(#26226,#26227,#26228,#26229)) ;
#5455 = EDGE_LOOP('',(#26230,#26231,#26232,#26233)) ;
#5456 = EDGE_LOOP('',(#26234,#26235,#26236)) ;
#5457 = EDGE_LOOP('',(#26237,#26238,#26239)) ;
#5458 = EDGE_LOOP('',(#26240,#26241,#26242,#26243)) ;
#5459 = EDGE_LOOP('',(#26244,#26245,#26246,#26247)) ;
#5460 = EDGE_LOOP('',(#26248,#26249,#26250,#26251)) ;
#5461 = EDGE_LOOP('',(#26252,#26253,#26254,#26255)) ;
#5462 = EDGE_LOOP('',(#26256,#26257,#26258,#26259)) ;
#5463 = EDGE_LOOP('',(#26260,#26261,#26262,#26263)) ;
#5464 = EDGE_LOOP('',(#26264,#26265,#26266,#26267)) ;
#5465 = EDGE_LOOP('',(#26268,#26269,#26270,#26271)) ;
#5466 = EDGE_LOOP('',(#26272,#26273,#26274,#26275)) ;
#5467 = EDGE_LOOP('',(#26276,#26277,#26278,#26279)) ;
#5468 = EDGE_LOOP('',(#26280,#26281,#26282,#26283)) ;
#5469 = EDGE_LOOP('',(#26284,#26285,#26286,#26287)) ;
#5470 = EDGE_LOOP('',(#26288,#26289,#26290,#26291)) ;
#5471 = EDGE_LOOP('',(#26292,#26293,#26294)) ;
#5472 = EDGE_LOOP('',(#26295,#26296,#26297)) ;
#5473 = EDGE_LOOP('',(#26298,#26299,#26300,#26301)) ;
#5474 = EDGE_LOOP('',(#26302,#26303,#26304)) ;
#5475 = EDGE_LOOP('',(#26305,#26306,#26307)) ;
#5476 = EDGE_LOOP('',(#26308,#26309,#26310,#26311)) ;
#5477 = EDGE_LOOP('',(#26312,#26313,#26314,#26315)) ;
#5478 = EDGE_LOOP('',(#26316,#26317,#26318,#26319)) ;
#5479 = EDGE_LOOP('',(#26320,#26321,#26322,#26323)) ;
#5480 = EDGE_LOOP('',(#26324,#26325,#26326)) ;
#5481 = EDGE_LOOP('',(#26327,#26328,#26329)) ;
#5482 = EDGE_LOOP('',(#26330,#26331,#26332,#26333)) ;
#5483 = EDGE_LOOP('',(#26334,#26335,#26336,#26337)) ;
#5484 = EDGE_LOOP('',(#26338,#26339,#26340,#26341)) ;
#5485 = EDGE_LOOP('',(#26342,#26343,#26344,#26345)) ;
#5486 = EDGE_LOOP('',(#26346,#26347,#26348)) ;
#5487 = EDGE_LOOP('',(#26349,#26350,#26351)) ;
#5488 = EDGE_LOOP('',(#26352,#26353,#26354,#26355)) ;
#5489 = EDGE_LOOP('',(#26356,#26357,#26358,#26359)) ;
#5490 = EDGE_LOOP('',(#26360,#26361,#26362,#26363)) ;
#5491 = EDGE_LOOP('',(#26364,#26365,#26366,#26367)) ;
#5492 = EDGE_LOOP('',(#26368,#26369,#26370,#26371)) ;
#5493 = EDGE_LOOP('',(#26372,#26373,#26374,#26375)) ;
#5494 = EDGE_LOOP('',(#26376,#26377,#26378,#26379)) ;
#5495 = EDGE_LOOP('',(#26380,#26381,#26382,#26383)) ;
#5496 = EDGE_LOOP('',(#26384,#26385,#26386,#26387)) ;
#5497 = EDGE_LOOP('',(#26388,#26389,#26390,#26391)) ;
#5498 = EDGE_LOOP('',(#26392,#26393,#26394,#26395)) ;
#5499 = EDGE_LOOP('',(#26396,#26397,#26398,#26399)) ;
#5500 = EDGE_LOOP('',(#26400,#26401,#26402,#26403)) ;
#5501 = EDGE_LOOP('',(#26404,#26405,#26406,#26407)) ;
#5502 = EDGE_LOOP('',(#26408,#26409,#26410,#26411)) ;
#5503 = EDGE_LOOP('',(#26412,#26413,#26414,#26415)) ;
#5504 = EDGE_LOOP('',(#26416,#26417,#26418,#26419)) ;
#5505 = EDGE_LOOP('',(#26420,#26421,#26422,#26423)) ;
#5506 = EDGE_LOOP('',(#26424,#26425,#26426,#26427)) ;
#5507 = EDGE_LOOP('',(#26428,#26429,#26430,#26431)) ;
#5508 = EDGE_LOOP('',(#26432,#26433,#26434,#26435)) ;
#5509 = EDGE_LOOP('',(#26436,#26437,#26438,#26439)) ;
#5510 = EDGE_LOOP('',(#26440,#26441,#26442,#26443)) ;
#5511 = EDGE_LOOP('',(#26444,#26445,#26446,#26447)) ;
#5512 = EDGE_LOOP('',(#26448,#26449,#26450,#26451)) ;
#5513 = EDGE_LOOP('',(#26452,#26453,#26454,#26455)) ;
#5514 = EDGE_LOOP('',(#26456,#26457,#26458,#26459)) ;
#5515 = EDGE_LOOP('',(#26460,#26461,#26462,#26463,#26464,#26465,#26466,#26467,
#26468,#26469,#26470,#26471,#26472,#26473,#26474,#26475,#26476,#26477,#26478,
#26479,#26480,#26481,#26482,#26483,#26484,#26485,#26486,#26487,#26488,#26489,
#26490,#26491,#26492,#26493,#26494,#26495,#26496,#26497,#26498,#26499)) ;
#5516 = EDGE_LOOP('',(#26500,#26501,#26502,#26503)) ;
#5517 = EDGE_LOOP('',(#26504,#26505,#26506,#26507,#26508,#26509)) ;
#5518 = EDGE_LOOP('',(#26510,#26511,#26512,#26513)) ;
#5519 = EDGE_LOOP('',(#26514,#26515,#26516,#26517)) ;
#5520 = EDGE_LOOP('',(#26518,#26519,#26520,#26521)) ;
#5521 = EDGE_LOOP('',(#26522,#26523,#26524,#26525)) ;
#5522 = EDGE_LOOP('',(#26526,#26527,#26528,#26529)) ;
#5523 = EDGE_LOOP('',(#26530,#26531,#26532,#26533)) ;
#5524 = EDGE_LOOP('',(#26534,#26535,#26536,#26537)) ;
#5525 = EDGE_LOOP('',(#26538,#26539,#26540,#26541)) ;
#5526 = EDGE_LOOP('',(#26542,#26543,#26544,#26545,#26546,#26547)) ;
#5527 = EDGE_LOOP('',(#26548,#26549,#26550,#26551)) ;
#5528 = EDGE_LOOP('',(#26552,#26553,#26554,#26555)) ;
#5529 = EDGE_LOOP('',(#26556,#26557,#26558,#26559)) ;
#5530 = EDGE_LOOP('',(#26560,#26561,#26562,#26563)) ;
#5531 = EDGE_LOOP('',(#26564,#26565,#26566,#26567)) ;
#5532 = EDGE_LOOP('',(#26568,#26569,#26570,#26571)) ;
#5533 = EDGE_LOOP('',(#26572,#26573,#26574,#26575)) ;
#5534 = EDGE_LOOP('',(#26576,#26577,#26578,#26579)) ;
#5535 = EDGE_LOOP('',(#26580,#26581,#26582,#26583)) ;
#5536 = EDGE_LOOP('',(#26584,#26585,#26586,#26587)) ;
#5537 = EDGE_LOOP('',(#26588,#26589,#26590,#26591,#26592)) ;
#5538 = EDGE_LOOP('',(#26593,#26594,#26595,#26596,#26597,#26598)) ;
#5539 = EDGE_LOOP('',(#26599,#26600,#26601,#26602,#26603,#26604)) ;
#5540 = EDGE_LOOP('',(#26605,#26606,#26607,#26608,#26609,#26610)) ;
#5541 = EDGE_LOOP('',(#26611,#26612,#26613,#26614,#26615,#26616)) ;
#5542 = EDGE_LOOP('',(#26617,#26618,#26619,#26620,#26621,#26622)) ;
#5543 = EDGE_LOOP('',(#26623,#26624,#26625,#26626,#26627,#26628)) ;
#5544 = EDGE_LOOP('',(#26629,#26630,#26631,#26632,#26633,#26634)) ;
#5545 = EDGE_LOOP('',(#26635,#26636,#26637,#26638,#26639,#26640)) ;
#5546 = EDGE_LOOP('',(#26641,#26642,#26643,#26644,#26645,#26646)) ;
#5547 = EDGE_LOOP('',(#26647,#26648,#26649,#26650,#26651,#26652)) ;
#5548 = EDGE_LOOP('',(#26653,#26654,#26655,#26656,#26657,#26658)) ;
#5549 = EDGE_LOOP('',(#26659,#26660,#26661,#26662,#26663,#26664)) ;
#5550 = EDGE_LOOP('',(#26665,#26666,#26667,#26668,#26669,#26670)) ;
#5551 = EDGE_LOOP('',(#26671,#26672,#26673,#26674,#26675,#26676)) ;
#5552 = EDGE_LOOP('',(#26677,#26678,#26679,#26680,#26681,#26682)) ;
#5553 = EDGE_LOOP('',(#26683,#26684,#26685,#26686,#26687,#26688)) ;
#5554 = EDGE_LOOP('',(#26689,#26690,#26691,#26692)) ;
#5555 = EDGE_LOOP('',(#26693,#26694,#26695,#26696,#26697,#26698,#26699,#26700,
#26701,#26702,#26703,#26704,#26705,#26706,#26707,#26708,#26709,#26710,#26711,
#26712,#26713,#26714,#26715,#26716,#26717,#26718,#26719,#26720,#26721,#26722,
#26723,#26724,#26725,#26726,#26727,#26728,#26729,#26730,#26731,#26732)) ;
#5556 = EDGE_LOOP('',(#26733,#26734,#26735,#26736)) ;
#5557 = EDGE_LOOP('',(#26737,#26738,#26739,#26740)) ;
#5558 = EDGE_LOOP('',(#26741,#26742,#26743,#26744)) ;
#5559 = EDGE_LOOP('',(#26745,#26746,#26747,#26748)) ;
#5560 = EDGE_LOOP('',(#26749,#26750,#26751,#26752)) ;
#5561 = EDGE_LOOP('',(#26753,#26754,#26755,#26756)) ;
#5562 = EDGE_LOOP('',(#26757,#26758,#26759,#26760)) ;
#5563 = EDGE_LOOP('',(#26761,#26762,#26763,#26764)) ;
#5564 = EDGE_LOOP('',(#26765,#26766,#26767,#26768)) ;
#5565 = EDGE_LOOP('',(#26769,#26770,#26771,#26772,#26773,#26774,#26775,#26776)) ;
#5566 = EDGE_LOOP('',(#26777,#26778,#26779,#26780,#26781,#26782,#26783,#26784)) ;
#5567 = EDGE_LOOP('',(#26785)) ;
#5568 = EDGE_LOOP('',(#26786,#26787,#26788,#26789,#26790)) ;
#5569 = EDGE_LOOP('',(#26791,#26792,#26793,#26794,#26795)) ;
#5570 = EDGE_LOOP('',(#26796,#26797,#26798,#26799)) ;
#5571 = EDGE_LOOP('',(#26800,#26801,#26802,#26803)) ;
#5572 = EDGE_LOOP('',(#26804,#26805,#26806,#26807)) ;
#5573 = EDGE_LOOP('',(#26808,#26809,#26810,#26811)) ;
#5574 = EDGE_LOOP('',(#26812,#26813,#26814,#26815,#26816,#26817,#26818,#26819)) ;
#5575 = EDGE_LOOP('',(#26820,#26821,#26822,#26823,#26824,#26825,#26826,#26827)) ;
#5576 = EDGE_LOOP('',(#26828)) ;
#5577 = EDGE_LOOP('',(#26829,#26830,#26831,#26832,#26833)) ;
#5578 = EDGE_LOOP('',(#26834,#26835,#26836,#26837,#26838)) ;
#5579 = EDGE_LOOP('',(#26839,#26840,#26841,#26842)) ;
#5580 = EDGE_LOOP('',(#26843,#26844,#26845,#26846)) ;
#5581 = EDGE_LOOP('',(#26847,#26848,#26849,#26850)) ;
#5582 = EDGE_LOOP('',(#26851,#26852,#26853,#26854)) ;
#5583 = EDGE_LOOP('',(#26855,#26856,#26857,#26858,#26859,#26860,#26861,#26862)) ;
#5584 = EDGE_LOOP('',(#26863,#26864,#26865,#26866,#26867,#26868,#26869,#26870)) ;
#5585 = EDGE_LOOP('',(#26871)) ;
#5586 = EDGE_LOOP('',(#26872,#26873,#26874,#26875,#26876)) ;
#5587 = EDGE_LOOP('',(#26877,#26878,#26879,#26880,#26881)) ;
#5588 = EDGE_LOOP('',(#26882,#26883,#26884,#26885)) ;
#5589 = EDGE_LOOP('',(#26886,#26887,#26888,#26889)) ;
#5590 = EDGE_LOOP('',(#26890,#26891,#26892,#26893)) ;
#5591 = EDGE_LOOP('',(#26894,#26895,#26896,#26897)) ;
#5592 = EDGE_LOOP('',(#26898,#26899,#26900,#26901,#26902,#26903,#26904,#26905)) ;
#5593 = EDGE_LOOP('',(#26906,#26907,#26908,#26909,#26910,#26911,#26912,#26913)) ;
#5594 = EDGE_LOOP('',(#26914)) ;
#5595 = EDGE_LOOP('',(#26915,#26916,#26917,#26918,#26919)) ;
#5596 = EDGE_LOOP('',(#26920,#26921,#26922,#26923,#26924)) ;
#5597 = EDGE_LOOP('',(#26925,#26926,#26927,#26928)) ;
#5598 = EDGE_LOOP('',(#26929,#26930,#26931,#26932)) ;
#5599 = EDGE_LOOP('',(#26933,#26934,#26935,#26936)) ;
#5600 = EDGE_LOOP('',(#26937,#26938,#26939,#26940)) ;
#5601 = EDGE_LOOP('',(#26941,#26942,#26943,#26944,#26945,#26946,#26947,#26948)) ;
#5602 = EDGE_LOOP('',(#26949,#26950,#26951,#26952,#26953,#26954,#26955,#26956)) ;
#5603 = EDGE_LOOP('',(#26957)) ;
#5604 = EDGE_LOOP('',(#26958,#26959,#26960,#26961,#26962)) ;
#5605 = EDGE_LOOP('',(#26963,#26964,#26965,#26966,#26967)) ;
#5606 = EDGE_LOOP('',(#26968,#26969,#26970,#26971)) ;
#5607 = EDGE_LOOP('',(#26972,#26973,#26974,#26975)) ;
#5608 = EDGE_LOOP('',(#26976,#26977,#26978,#26979)) ;
#5609 = EDGE_LOOP('',(#26980,#26981,#26982,#26983)) ;
#5610 = EDGE_LOOP('',(#26984,#26985,#26986,#26987,#26988,#26989,#26990,#26991)) ;
#5611 = EDGE_LOOP('',(#26992,#26993,#26994,#26995,#26996,#26997,#26998,#26999)) ;
#5612 = EDGE_LOOP('',(#27000)) ;
#5613 = EDGE_LOOP('',(#27001,#27002,#27003,#27004,#27005)) ;
#5614 = EDGE_LOOP('',(#27006,#27007,#27008,#27009,#27010)) ;
#5615 = EDGE_LOOP('',(#27011,#27012,#27013,#27014)) ;
#5616 = EDGE_LOOP('',(#27015,#27016,#27017,#27018)) ;
#5617 = EDGE_LOOP('',(#27019,#27020,#27021,#27022)) ;
#5618 = EDGE_LOOP('',(#27023,#27024,#27025,#27026)) ;
#5619 = EDGE_LOOP('',(#27027,#27028,#27029,#27030,#27031,#27032,#27033,#27034)) ;
#5620 = EDGE_LOOP('',(#27035,#27036,#27037,#27038,#27039,#27040,#27041,#27042)) ;
#5621 = EDGE_LOOP('',(#27043)) ;
#5622 = EDGE_LOOP('',(#27044,#27045,#27046,#27047,#27048)) ;
#5623 = EDGE_LOOP('',(#27049,#27050,#27051,#27052,#27053)) ;
#5624 = EDGE_LOOP('',(#27054,#27055,#27056,#27057)) ;
#5625 = EDGE_LOOP('',(#27058,#27059,#27060,#27061)) ;
#5626 = EDGE_LOOP('',(#27062,#27063,#27064,#27065)) ;
#5627 = EDGE_LOOP('',(#27066,#27067,#27068,#27069)) ;
#5628 = EDGE_LOOP('',(#27070,#27071,#27072,#27073,#27074,#27075,#27076,#27077)) ;
#5629 = EDGE_LOOP('',(#27078,#27079,#27080,#27081,#27082,#27083,#27084,#27085)) ;
#5630 = EDGE_LOOP('',(#27086)) ;
#5631 = EDGE_LOOP('',(#27087,#27088,#27089,#27090,#27091)) ;
#5632 = EDGE_LOOP('',(#27092,#27093,#27094,#27095,#27096)) ;
#5633 = EDGE_LOOP('',(#27097,#27098,#27099,#27100)) ;
#5634 = EDGE_LOOP('',(#27101,#27102,#27103,#27104)) ;
#5635 = EDGE_LOOP('',(#27105,#27106,#27107,#27108)) ;
#5636 = EDGE_LOOP('',(#27109,#27110,#27111,#27112,#27113)) ;
#5637 = EDGE_LOOP('',(#27114,#27115,#27116,#27117,#27118)) ;
#5638 = EDGE_LOOP('',(#27119,#27120,#27121,#27122)) ;
#5639 = EDGE_LOOP('',(#27123,#27124,#27125,#27126,#27127)) ;
#5640 = EDGE_LOOP('',(#27128,#27129,#27130,#27131,#27132,#27133,#27134,#27135,
#27136,#27137,#27138,#27139,#27140,#27141,#27142,#27143,#27144,#27145,#27146,
#27147,#27148,#27149,#27150,#27151,#27152,#27153,#27154,#27155,#27156,#27157,
#27158,#27159,#27160,#27161,#27162,#27163,#27164,#27165,#27166,#27167,#27168,
#27169,#27170,#27171,#27172,#27173,#27174,#27175,#27176,#27177,#27178,#27179,
#27180,#27181,#27182,#27183,#27184,#27185,#27186,#27187,#27188,#27189,#27190,
#27191,#27192,#27193,#27194,#27195,#27196,#27197,#27198,#27199,#27200,#27201,
#27202,#27203)) ;
#5641 = EDGE_LOOP('',(#27204,#27205,#27206,#27207)) ;
#5642 = EDGE_LOOP('',(#27208,#27209,#27210,#27211)) ;
#5643 = EDGE_LOOP('',(#27212,#27213,#27214,#27215)) ;
#5644 = EDGE_LOOP('',(#27216,#27217,#27218,#27219)) ;
#5645 = EDGE_LOOP('',(#27220,#27221,#27222,#27223)) ;
#5646 = EDGE_LOOP('',(#27224,#27225,#27226,#27227)) ;
#5647 = EDGE_LOOP('',(#27228,#27229,#27230,#27231)) ;
#5648 = EDGE_LOOP('',(#27232,#27233,#27234,#27235)) ;
#5649 = EDGE_LOOP('',(#27236,#27237,#27238,#27239)) ;
#5650 = EDGE_LOOP('',(#27240,#27241,#27242,#27243)) ;
#5651 = EDGE_LOOP('',(#27244,#27245,#27246,#27247)) ;
#5652 = EDGE_LOOP('',(#27248,#27249,#27250,#27251)) ;
#5653 = EDGE_LOOP('',(#27252,#27253,#27254,#27255)) ;
#5654 = EDGE_LOOP('',(#27256,#27257,#27258,#27259)) ;
#5655 = EDGE_LOOP('',(#27260,#27261,#27262,#27263)) ;
#5656 = EDGE_LOOP('',(#27264,#27265,#27266,#27267)) ;
#5657 = EDGE_LOOP('',(#27268,#27269,#27270,#27271)) ;
#5658 = EDGE_LOOP('',(#27272,#27273,#27274,#27275)) ;
#5659 = EDGE_LOOP('',(#27276,#27277,#27278,#27279)) ;
#5660 = EDGE_LOOP('',(#27280,#27281,#27282,#27283)) ;
#5661 = EDGE_LOOP('',(#27284,#27285,#27286,#27287)) ;
#5662 = EDGE_LOOP('',(#27288,#27289,#27290,#27291)) ;
#5663 = EDGE_LOOP('',(#27292,#27293,#27294,#27295)) ;
#5664 = EDGE_LOOP('',(#27296,#27297,#27298,#27299)) ;
#5665 = EDGE_LOOP('',(#27300,#27301,#27302,#27303)) ;
#5666 = EDGE_LOOP('',(#27304,#27305,#27306,#27307)) ;
#5667 = EDGE_LOOP('',(#27308,#27309,#27310,#27311)) ;
#5668 = EDGE_LOOP('',(#27312,#27313,#27314,#27315)) ;
#5669 = EDGE_LOOP('',(#27316,#27317,#27318,#27319)) ;
#5670 = EDGE_LOOP('',(#27320,#27321,#27322,#27323)) ;
#5671 = EDGE_LOOP('',(#27324,#27325,#27326,#27327)) ;
#5672 = EDGE_LOOP('',(#27328,#27329,#27330,#27331)) ;
#5673 = EDGE_LOOP('',(#27332,#27333,#27334,#27335)) ;
#5674 = EDGE_LOOP('',(#27336,#27337,#27338,#27339)) ;
#5675 = EDGE_LOOP('',(#27340,#27341,#27342,#27343)) ;
#5676 = EDGE_LOOP('',(#27344,#27345,#27346,#27347)) ;
#5677 = EDGE_LOOP('',(#27348,#27349,#27350,#27351)) ;
#5678 = EDGE_LOOP('',(#27352,#27353,#27354,#27355)) ;
#5679 = EDGE_LOOP('',(#27356,#27357,#27358,#27359)) ;
#5680 = EDGE_LOOP('',(#27360,#27361,#27362,#27363)) ;
#5681 = EDGE_LOOP('',(#27364,#27365,#27366,#27367)) ;
#5682 = EDGE_LOOP('',(#27368,#27369,#27370,#27371)) ;
#5683 = EDGE_LOOP('',(#27372,#27373,#27374,#27375)) ;
#5684 = EDGE_LOOP('',(#27376,#27377,#27378,#27379)) ;
#5685 = EDGE_LOOP('',(#27380,#27381,#27382,#27383)) ;
#5686 = EDGE_LOOP('',(#27384,#27385,#27386,#27387)) ;
#5687 = EDGE_LOOP('',(#27388,#27389,#27390,#27391)) ;
#5688 = EDGE_LOOP('',(#27392,#27393,#27394,#27395,#27396)) ;
#5689 = EDGE_LOOP('',(#27397,#27398,#27399,#27400)) ;
#5690 = EDGE_LOOP('',(#27401,#27402,#27403,#27404)) ;
#5691 = EDGE_LOOP('',(#27405,#27406,#27407,#27408)) ;
#5692 = EDGE_LOOP('',(#27409,#27410,#27411,#27412)) ;
#5693 = EDGE_LOOP('',(#27413,#27414,#27415,#27416)) ;
#5694 = EDGE_LOOP('',(#27417,#27418,#27419,#27420)) ;
#5695 = EDGE_LOOP('',(#27421,#27422,#27423,#27424)) ;
#5696 = EDGE_LOOP('',(#27425,#27426,#27427,#27428,#27429)) ;
#5697 = EDGE_LOOP('',(#27430,#27431,#27432)) ;
#5698 = EDGE_LOOP('',(#27433,#27434,#27435)) ;
#5699 = EDGE_LOOP('',(#27436,#27437,#27438,#27439)) ;
#5700 = EDGE_LOOP('',(#27440,#27441,#27442,#27443)) ;
#5701 = EDGE_LOOP('',(#27444,#27445,#27446,#27447)) ;
#5702 = EDGE_LOOP('',(#27448,#27449,#27450)) ;
#5703 = EDGE_LOOP('',(#27451,#27452,#27453,#27454)) ;
#5704 = EDGE_LOOP('',(#27455,#27456,#27457,#27458)) ;
#5705 = EDGE_LOOP('',(#27459,#27460,#27461)) ;
#5706 = EDGE_LOOP('',(#27462,#27463,#27464,#27465,#27466,#27467,#27468,#27469,
#27470,#27471,#27472,#27473,#27474,#27475,#27476,#27477)) ;
#5707 = EDGE_LOOP('',(#27478,#27479,#27480,#27481,#27482,#27483,#27484,#27485)) ;
#5708 = EDGE_LOOP('',(#27486,#27487,#27488)) ;
#5709 = EDGE_LOOP('',(#27489,#27490,#27491,#27492)) ;
#5710 = EDGE_LOOP('',(#27493,#27494,#27495,#27496)) ;
#5711 = EDGE_LOOP('',(#27497,#27498,#27499,#27500)) ;
#5712 = EDGE_LOOP('',(#27501,#27502,#27503)) ;
#5713 = EDGE_LOOP('',(#27504,#27505,#27506,#27507)) ;
#5714 = EDGE_LOOP('',(#27508,#27509,#27510,#27511)) ;
#5715 = EDGE_LOOP('',(#27512,#27513,#27514,#27515,#27516,#27517)) ;
#5716 = EDGE_LOOP('',(#27518,#27519,#27520,#27521,#27522,#27523,#27524,#27525,
#27526)) ;
#5717 = EDGE_LOOP('',(#27527,#27528,#27529)) ;
#5718 = EDGE_LOOP('',(#27530,#27531,#27532,#27533)) ;
#5719 = EDGE_LOOP('',(#27534,#27535,#27536,#27537)) ;
#5720 = EDGE_LOOP('',(#27538,#27539,#27540,#27541)) ;
#5721 = EDGE_LOOP('',(#27542,#27543,#27544)) ;
#5722 = EDGE_LOOP('',(#27545,#27546,#27547,#27548)) ;
#5723 = EDGE_LOOP('',(#27549,#27550,#27551,#27552)) ;
#5724 = EDGE_LOOP('',(#27553,#27554,#27555)) ;
#5725 = EDGE_LOOP('',(#27556,#27557,#27558,#27559,#27560,#27561,#27562,#27563)) ;
#5726 = EDGE_LOOP('',(#27564,#27565,#27566)) ;
#5727 = EDGE_LOOP('',(#27567,#27568,#27569,#27570)) ;
#5728 = EDGE_LOOP('',(#27571,#27572,#27573,#27574)) ;
#5729 = EDGE_LOOP('',(#27575,#27576,#27577,#27578)) ;
#5730 = EDGE_LOOP('',(#27579,#27580,#27581)) ;
#5731 = EDGE_LOOP('',(#27582,#27583,#27584,#27585)) ;
#5732 = EDGE_LOOP('',(#27586,#27587,#27588,#27589)) ;
#5733 = EDGE_LOOP('',(#27590,#27591,#27592,#27593,#27594,#27595)) ;
#5734 = EDGE_LOOP('',(#27596,#27597,#27598,#27599,#27600,#27601,#27602,#27603,
#27604)) ;
#5735 = EDGE_LOOP('',(#27605,#27606,#27607)) ;
#5736 = EDGE_LOOP('',(#27608,#27609,#27610,#27611)) ;
#5737 = EDGE_LOOP('',(#27612,#27613,#27614)) ;
#5738 = EDGE_LOOP('',(#27615,#27616,#27617,#27618)) ;
#5739 = EDGE_LOOP('',(#27619,#27620,#27621,#27622,#27623)) ;
#5740 = EDGE_LOOP('',(#27624,#27625,#27626,#27627)) ;
#5741 = EDGE_LOOP('',(#27628,#27629,#27630)) ;
#5742 = EDGE_LOOP('',(#27631,#27632,#27633,#27634)) ;
#5743 = EDGE_LOOP('',(#27635,#27636,#27637,#27638)) ;
#5744 = EDGE_LOOP('',(#27639,#27640,#27641)) ;
#5745 = EDGE_LOOP('',(#27642,#27643,#27644)) ;
#5746 = EDGE_LOOP('',(#27645,#27646,#27647,#27648)) ;
#5747 = EDGE_LOOP('',(#27649,#27650,#27651,#27652)) ;
#5748 = EDGE_LOOP('',(#27653,#27654,#27655)) ;
#5749 = EDGE_LOOP('',(#27656,#27657,#27658,#27659)) ;
#5750 = EDGE_LOOP('',(#27660,#27661,#27662,#27663,#27664)) ;
#5751 = EDGE_LOOP('',(#27665,#27666,#27667,#27668)) ;
#5752 = EDGE_LOOP('',(#27669,#27670,#27671)) ;
#5753 = EDGE_LOOP('',(#27672,#27673,#27674,#27675)) ;
#5754 = EDGE_LOOP('',(#27676,#27677,#27678)) ;
#5755 = EDGE_LOOP('',(#27679,#27680,#27681,#27682,#27683,#27684)) ;
#5756 = EDGE_LOOP('',(#27685,#27686,#27687,#27688)) ;
#5757 = EDGE_LOOP('',(#27689,#27690,#27691)) ;
#5758 = EDGE_LOOP('',(#27692,#27693,#27694,#27695)) ;
#5759 = EDGE_LOOP('',(#27696,#27697,#27698,#27699)) ;
#5760 = EDGE_LOOP('',(#27700,#27701,#27702)) ;
#5761 = EDGE_LOOP('',(#27703,#27704,#27705,#27706,#27707,#27708)) ;
#5762 = EDGE_LOOP('',(#27709,#27710,#27711,#27712)) ;
#5763 = EDGE_LOOP('',(#27713,#27714,#27715,#27716)) ;
#5764 = EDGE_LOOP('',(#27717,#27718,#27719,#27720)) ;
#5765 = EDGE_LOOP('',(#27721,#27722,#27723)) ;
#5766 = EDGE_LOOP('',(#27724,#27725,#27726,#27727)) ;
#5767 = EDGE_LOOP('',(#27728,#27729,#27730,#27731)) ;
#5768 = EDGE_LOOP('',(#27732,#27733,#27734)) ;
#5769 = EDGE_LOOP('',(#27735,#27736,#27737,#27738)) ;
#5770 = EDGE_LOOP('',(#27739,#27740,#27741,#27742,#27743)) ;
#5771 = EDGE_LOOP('',(#27744,#27745,#27746,#27747)) ;
#5772 = EDGE_LOOP('',(#27748,#27749,#27750)) ;
#5773 = EDGE_LOOP('',(#27751,#27752,#27753,#27754)) ;
#5774 = EDGE_LOOP('',(#27755,#27756,#27757)) ;
#5775 = EDGE_LOOP('',(#27758,#27759,#27760,#27761,#27762,#27763)) ;
#5776 = EDGE_LOOP('',(#27764,#27765,#27766,#27767)) ;
#5777 = EDGE_LOOP('',(#27768,#27769,#27770)) ;
#5778 = EDGE_LOOP('',(#27771,#27772,#27773,#27774)) ;
#5779 = EDGE_LOOP('',(#27775,#27776,#27777)) ;
#5780 = EDGE_LOOP('',(#27778,#27779,#27780,#27781,#27782)) ;
#5781 = EDGE_LOOP('',(#27783,#27784,#27785,#27786)) ;
#5782 = EDGE_LOOP('',(#27787,#27788,#27789,#27790,#27791,#27792,#27793,#27794)) ;
#5783 = EDGE_LOOP('',(#27795,#27796,#27797,#27798,#27799)) ;
#5784 = EDGE_LOOP('',(#27800,#27801,#27802,#27803,#27804,#27805,#27806,#27807,
#27808,#27809)) ;
#5785 = EDGE_LOOP('',(#27810,#27811,#27812,#27813,#27814,#27815,#27816,#27817,
#27818,#27819,#27820,#27821,#27822,#27823,#27824,#27825,#27826,#27827,#27828,
#27829,#27830,#27831,#27832,#27833,#27834)) ;
#5786 = EDGE_LOOP('',(#27835)) ;
#5787 = EDGE_LOOP('',(#27836,#27837,#27838)) ;
#5788 = EDGE_LOOP('',(#27839,#27840,#27841,#27842,#27843,#27844,#27845,#27846,
#27847)) ;
#5789 = EDGE_LOOP('',(#27848,#27849,#27850,#27851)) ;
#5790 = EDGE_LOOP('',(#27852,#27853,#27854,#27855)) ;
#5791 = EDGE_LOOP('',(#27856,#27857,#27858)) ;
#5792 = EDGE_LOOP('',(#27859,#27860,#27861,#27862)) ;
#5793 = EDGE_LOOP('',(#27863,#27864,#27865,#27866,#27867,#27868,#27869,#27870)) ;
#5794 = EDGE_LOOP('',(#27871,#27872,#27873,#27874,#27875,#27876,#27877,#27878)) ;
#5795 = EDGE_LOOP('',(#27879,#27880,#27881)) ;
#5796 = EDGE_LOOP('',(#27882,#27883,#27884,#27885)) ;
#5797 = EDGE_LOOP('',(#27886,#27887,#27888,#27889)) ;
#5798 = EDGE_LOOP('',(#27890,#27891,#27892,#27893,#27894)) ;
#5799 = EDGE_LOOP('',(#27895,#27896,#27897,#27898,#27899,#27900)) ;
#5800 = EDGE_LOOP('',(#27901,#27902,#27903,#27904)) ;
#5801 = EDGE_LOOP('',(#27905,#27906,#27907,#27908)) ;
#5802 = EDGE_LOOP('',(#27909,#27910,#27911,#27912,#27913,#27914,#27915,#27916)) ;
#5803 = EDGE_LOOP('',(#27917,#27918,#27919)) ;
#5804 = EDGE_LOOP('',(#27920,#27921,#27922,#27923)) ;
#5805 = EDGE_LOOP('',(#27924,#27925,#27926,#27927)) ;
#5806 = EDGE_LOOP('',(#27928,#27929,#27930,#27931)) ;
#5807 = EDGE_LOOP('',(#27932,#27933,#27934)) ;
#5808 = EDGE_LOOP('',(#27935,#27936,#27937)) ;
#5809 = EDGE_LOOP('',(#27938,#27939,#27940,#27941)) ;
#5810 = EDGE_LOOP('',(#27942,#27943,#27944,#27945)) ;
#5811 = EDGE_LOOP('',(#27946,#27947,#27948,#27949,#27950,#27951)) ;
#5812 = EDGE_LOOP('',(#27952,#27953,#27954)) ;
#5813 = EDGE_LOOP('',(#27955,#27956,#27957,#27958)) ;
#5814 = EDGE_LOOP('',(#27959,#27960,#27961,#27962)) ;
#5815 = EDGE_LOOP('',(#27963,#27964,#27965)) ;
#5816 = EDGE_LOOP('',(#27966,#27967,#27968,#27969)) ;
#5817 = EDGE_LOOP('',(#27970,#27971,#27972,#27973)) ;
#5818 = EDGE_LOOP('',(#27974,#27975,#27976)) ;
#5819 = EDGE_LOOP('',(#27977,#27978,#27979,#27980)) ;
#5820 = EDGE_LOOP('',(#27981,#27982,#27983)) ;
#5821 = EDGE_LOOP('',(#27984,#27985,#27986)) ;
#5822 = EDGE_LOOP('',(#27987,#27988,#27989,#27990)) ;
#5823 = EDGE_LOOP('',(#27991,#27992,#27993,#27994)) ;
#5824 = EDGE_LOOP('',(#27995,#27996,#27997,#27998,#27999,#28000,#28001,#28002,
#28003)) ;
#5825 = EDGE_LOOP('',(#28004,#28005,#28006,#28007,#28008,#28009)) ;
#5826 = EDGE_LOOP('',(#28010,#28011,#28012,#28013)) ;
#5827 = EDGE_LOOP('',(#28014,#28015,#28016)) ;
#5828 = EDGE_LOOP('',(#28017,#28018,#28019,#28020)) ;
#5829 = EDGE_LOOP('',(#28021,#28022,#28023,#28024)) ;
#5830 = EDGE_LOOP('',(#28025,#28026,#28027)) ;
#5831 = EDGE_LOOP('',(#28028,#28029,#28030,#28031)) ;
#5832 = EDGE_LOOP('',(#28032,#28033,#28034,#28035)) ;
#5833 = EDGE_LOOP('',(#28036,#28037,#28038)) ;
#5834 = EDGE_LOOP('',(#28039,#28040,#28041)) ;
#5835 = EDGE_LOOP('',(#28042,#28043,#28044,#28045,#28046,#28047)) ;
#5836 = EDGE_LOOP('',(#28048,#28049,#28050,#28051,#28052,#28053,#28054,#28055,
#28056)) ;
#5837 = EDGE_LOOP('',(#28057,#28058,#28059,#28060)) ;
#5838 = EDGE_LOOP('',(#28061,#28062,#28063,#28064)) ;
#5839 = EDGE_LOOP('',(#28065,#28066,#28067)) ;
#5840 = EDGE_LOOP('',(#28068,#28069,#28070,#28071)) ;
#5841 = EDGE_LOOP('',(#28072,#28073,#28074,#28075,#28076,#28077,#28078,#28079)) ;
#5842 = EDGE_LOOP('',(#28080,#28081,#28082,#28083,#28084,#28085,#28086,#28087)) ;
#5843 = EDGE_LOOP('',(#28088,#28089,#28090)) ;
#5844 = EDGE_LOOP('',(#28091,#28092,#28093,#28094)) ;
#5845 = EDGE_LOOP('',(#28095,#28096,#28097,#28098)) ;
#5846 = EDGE_LOOP('',(#28099,#28100,#28101,#28102,#28103)) ;
#5847 = EDGE_LOOP('',(#28104,#28105,#28106,#28107,#28108,#28109)) ;
#5848 = EDGE_LOOP('',(#28110,#28111,#28112,#28113)) ;
#5849 = EDGE_LOOP('',(#28114,#28115,#28116,#28117)) ;
#5850 = EDGE_LOOP('',(#28118,#28119,#28120,#28121,#28122,#28123,#28124,#28125)) ;
#5851 = EDGE_LOOP('',(#28126,#28127,#28128,#28129)) ;
#5852 = EDGE_LOOP('',(#28130,#28131,#28132)) ;
#5853 = EDGE_LOOP('',(#28133,#28134,#28135,#28136)) ;
#5854 = EDGE_LOOP('',(#28137,#28138,#28139,#28140)) ;
#5855 = EDGE_LOOP('',(#28141,#28142,#28143)) ;
#5856 = EDGE_LOOP('',(#28144,#28145,#28146)) ;
#5857 = EDGE_LOOP('',(#28147,#28148,#28149,#28150)) ;
#5858 = EDGE_LOOP('',(#28151,#28152,#28153,#28154)) ;
#5859 = EDGE_LOOP('',(#28155,#28156,#28157,#28158)) ;
#5860 = EDGE_LOOP('',(#28159,#28160,#28161,#28162,#28163,#28164)) ;
#5861 = EDGE_LOOP('',(#28165,#28166,#28167)) ;
#5862 = EDGE_LOOP('',(#28168,#28169,#28170,#28171)) ;
#5863 = EDGE_LOOP('',(#28172,#28173,#28174)) ;
#5864 = EDGE_LOOP('',(#28175,#28176,#28177,#28178)) ;
#5865 = EDGE_LOOP('',(#28179,#28180,#28181,#28182,#28183,#28184)) ;
#5866 = EDGE_LOOP('',(#28185,#28186,#28187,#28188)) ;
#5867 = EDGE_LOOP('',(#28189,#28190,#28191,#28192)) ;
#5868 = EDGE_LOOP('',(#28193,#28194,#28195)) ;
#5869 = EDGE_LOOP('',(#28196,#28197,#28198,#28199)) ;
#5870 = EDGE_LOOP('',(#28200,#28201,#28202)) ;
#5871 = EDGE_LOOP('',(#28203,#28204,#28205)) ;
#5872 = EDGE_LOOP('',(#28206,#28207,#28208,#28209)) ;
#5873 = EDGE_LOOP('',(#28210,#28211,#28212,#28213)) ;
#5874 = EDGE_LOOP('',(#28214,#28215,#28216,#28217,#28218,#28219,#28220,#28221,
#28222)) ;
#5875 = EDGE_LOOP('',(#28223,#28224,#28225,#28226)) ;
#5876 = EDGE_LOOP('',(#28227,#28228,#28229)) ;
#5877 = EDGE_LOOP('',(#28230,#28231,#28232,#28233)) ;
#5878 = EDGE_LOOP('',(#28234,#28235,#28236,#28237)) ;
#5879 = EDGE_LOOP('',(#28238,#28239,#28240)) ;
#5880 = EDGE_LOOP('',(#28241,#28242,#28243,#28244)) ;
#5881 = EDGE_LOOP('',(#28245,#28246,#28247,#28248)) ;
#5882 = EDGE_LOOP('',(#28249,#28250,#28251,#28252)) ;
#5883 = EDGE_LOOP('',(#28253,#28254,#28255,#28256)) ;
#5884 = EDGE_LOOP('',(#28257,#28258,#28259,#28260)) ;
#5885 = EDGE_LOOP('',(#28261,#28262,#28263,#28264,#28265,#28266)) ;
#5886 = EDGE_LOOP('',(#28267,#28268,#28269,#28270,#28271,#28272)) ;
#5887 = EDGE_LOOP('',(#28273,#28274,#28275,#28276,#28277,#28278,#28279,#28280,
#28281,#28282,#28283,#28284,#28285,#28286,#28287,#28288,#28289,#28290,#28291,
#28292)) ;
#5888 = EDGE_LOOP('',(#28293,#28294,#28295,#28296)) ;
#5889 = EDGE_LOOP('',(#28297,#28298,#28299,#28300)) ;
#5890 = EDGE_LOOP('',(#28301,#28302,#28303,#28304)) ;
#5891 = EDGE_LOOP('',(#28305,#28306,#28307,#28308,#28309,#28310)) ;
#5892 = EDGE_LOOP('',(#28311,#28312,#28313,#28314,#28315,#28316)) ;
#5893 = EDGE_LOOP('',(#28317,#28318,#28319,#28320)) ;
#5894 = EDGE_LOOP('',(#28321,#28322,#28323,#28324,#28325,#28326,#28327,#28328)) ;
#5895 = EDGE_LOOP('',(#28329,#28330,#28331,#28332)) ;
#5896 = EDGE_LOOP('',(#28333,#28334,#28335,#28336)) ;
#5897 = EDGE_LOOP('',(#28337,#28338,#28339,#28340)) ;
#5898 = EDGE_LOOP('',(#28341,#28342,#28343,#28344)) ;
#5899 = EDGE_LOOP('',(#28345,#28346,#28347,#28348)) ;
#5900 = EDGE_LOOP('',(#28349,#28350,#28351,#28352)) ;
#5901 = EDGE_LOOP('',(#28353,#28354,#28355,#28356)) ;
#5902 = EDGE_LOOP('',(#28357,#28358,#28359,#28360,#28361,#28362)) ;
#5903 = EDGE_LOOP('',(#28363,#28364,#28365,#28366,#28367,#28368,#28369,#28370)) ;
#5904 = EDGE_LOOP('',(#28371,#28372,#28373,#28374)) ;
#5905 = EDGE_LOOP('',(#28375,#28376,#28377,#28378,#28379)) ;
#5906 = EDGE_LOOP('',(#28380,#28381,#28382,#28383,#28384,#28385,#28386,#28387,
#28388)) ;
#5907 = EDGE_LOOP('',(#28389,#28390,#28391,#28392)) ;
#5908 = EDGE_LOOP('',(#28393,#28394,#28395,#28396,#28397,#28398)) ;
#5909 = EDGE_LOOP('',(#28399)) ;
#5910 = EDGE_LOOP('',(#28400,#28401,#28402,#28403,#28404,#28405,#28406,#28407,
#28408,#28409,#28410,#28411,#28412,#28413,#28414,#28415,#28416,#28417,#28418,
#28419,#28420,#28421)) ;
#5911 = EDGE_LOOP('',(#28422,#28423,#28424,#28425)) ;
#5912 = EDGE_LOOP('',(#28426,#28427,#28428,#28429)) ;
#5913 = EDGE_LOOP('',(#28430,#28431,#28432,#28433)) ;
#5914 = EDGE_LOOP('',(#28434,#28435,#28436,#28437)) ;
#5915 = EDGE_LOOP('',(#28438,#28439,#28440,#28441)) ;
#5916 = EDGE_LOOP('',(#28442,#28443,#28444,#28445)) ;
#5917 = EDGE_LOOP('',(#28446,#28447,#28448,#28449)) ;
#5918 = EDGE_LOOP('',(#28450,#28451,#28452,#28453)) ;
#5919 = EDGE_LOOP('',(#28454,#28455,#28456,#28457)) ;
#5920 = EDGE_LOOP('',(#28458,#28459,#28460,#28461)) ;
#5921 = EDGE_LOOP('',(#28462,#28463,#28464,#28465)) ;
#5922 = EDGE_LOOP('',(#28466,#28467,#28468,#28469)) ;
#5923 = EDGE_LOOP('',(#28470,#28471,#28472,#28473)) ;
#5924 = EDGE_LOOP('',(#28474,#28475,#28476,#28477)) ;
#5925 = EDGE_LOOP('',(#28478,#28479,#28480,#28481)) ;
#5926 = EDGE_LOOP('',(#28482,#28483,#28484,#28485)) ;
#5927 = EDGE_LOOP('',(#28486,#28487,#28488,#28489)) ;
#5928 = EDGE_LOOP('',(#28490,#28491,#28492,#28493)) ;
#5929 = EDGE_LOOP('',(#28494,#28495,#28496,#28497)) ;
#5930 = EDGE_LOOP('',(#28498,#28499,#28500,#28501)) ;
#5931 = EDGE_LOOP('',(#28502,#28503,#28504,#28505)) ;
#5932 = EDGE_LOOP('',(#28506,#28507,#28508,#28509)) ;
#5933 = EDGE_LOOP('',(#28510,#28511,#28512,#28513)) ;
#5934 = EDGE_LOOP('',(#28514,#28515,#28516,#28517)) ;
#5935 = EDGE_LOOP('',(#28518,#28519,#28520,#28521)) ;
#5936 = EDGE_LOOP('',(#28522,#28523,#28524,#28525)) ;
#5937 = EDGE_LOOP('',(#28526,#28527,#28528,#28529)) ;
#5938 = EDGE_LOOP('',(#28530,#28531,#28532)) ;
#5939 = EDGE_LOOP('',(#28533,#28534,#28535)) ;
#5940 = EDGE_LOOP('',(#28536,#28537,#28538,#28539)) ;
#5941 = EDGE_LOOP('',(#28540,#28541,#28542)) ;
#5942 = EDGE_LOOP('',(#28543,#28544,#28545)) ;
#5943 = EDGE_LOOP('',(#28546,#28547,#28548,#28549)) ;
#5944 = EDGE_LOOP('',(#28550,#28551,#28552,#28553)) ;
#5945 = EDGE_LOOP('',(#28554,#28555,#28556,#28557,#28558,#28559,#28560,#28561,
#28562,#28563,#28564,#28565)) ;
#5946 = EDGE_LOOP('',(#28566,#28567,#28568,#28569)) ;
#5947 = EDGE_LOOP('',(#28570,#28571,#28572,#28573)) ;
#5948 = EDGE_LOOP('',(#28574,#28575,#28576,#28577)) ;
#5949 = EDGE_LOOP('',(#28578,#28579,#28580,#28581)) ;
#5950 = EDGE_LOOP('',(#28582,#28583,#28584,#28585)) ;
#5951 = EDGE_LOOP('',(#28586,#28587,#28588,#28589)) ;
#5952 = EDGE_LOOP('',(#28590,#28591,#28592,#28593)) ;
#5953 = EDGE_LOOP('',(#28594,#28595,#28596,#28597)) ;
#5954 = EDGE_LOOP('',(#28598,#28599,#28600,#28601,#28602,#28603,#28604,#28605,
#28606,#28607,#28608,#28609,#28610,#28611,#28612,#28613)) ;
#5955 = EDGE_LOOP('',(#28614,#28615,#28616,#28617)) ;
#5956 = EDGE_LOOP('',(#28618,#28619,#28620,#28621,#28622,#28623)) ;
#5957 = EDGE_LOOP('',(#28624,#28625,#28626,#28627)) ;
#5958 = EDGE_LOOP('',(#28628,#28629,#28630,#28631,#28632,#28633,#28634,#28635,
#28636,#28637)) ;
#5959 = EDGE_LOOP('',(#28638,#28639,#28640,#28641)) ;
#5960 = EDGE_LOOP('',(#28642,#28643,#28644,#28645)) ;
#5961 = EDGE_LOOP('',(#28646,#28647,#28648,#28649)) ;
#5962 = EDGE_LOOP('',(#28650,#28651,#28652,#28653)) ;
#5963 = EDGE_LOOP('',(#28654,#28655,#28656,#28657)) ;
#5964 = EDGE_LOOP('',(#28658,#28659,#28660,#28661)) ;
#5965 = EDGE_LOOP('',(#28662,#28663,#28664,#28665)) ;
#5966 = EDGE_LOOP('',(#28666,#28667,#28668,#28669)) ;
#5967 = EDGE_LOOP('',(#28670,#28671,#28672,#28673,#28674,#28675)) ;
#5968 = EDGE_LOOP('',(#28676,#28677,#28678,#28679,#28680,#28681)) ;
#5969 = EDGE_LOOP('',(#28682,#28683,#28684,#28685)) ;
#5970 = EDGE_LOOP('',(#28686,#28687,#28688,#28689)) ;
#5971 = EDGE_LOOP('',(#28690,#28691,#28692,#28693,#28694)) ;
#5972 = EDGE_LOOP('',(#28695,#28696,#28697,#28698,#28699)) ;
#5973 = EDGE_LOOP('',(#28700,#28701,#28702,#28703,#28704)) ;
#5974 = EDGE_LOOP('',(#28705,#28706,#28707)) ;
#5975 = EDGE_LOOP('',(#28708,#28709,#28710,#28711,#28712)) ;
#5976 = EDGE_LOOP('',(#28713,#28714,#28715)) ;
#5977 = EDGE_LOOP('',(#28716,#28717,#28718,#28719)) ;
#5978 = EDGE_LOOP('',(#28720,#28721,#28722,#28723)) ;
#5979 = EDGE_LOOP('',(#28724,#28725,#28726,#28727)) ;
#5980 = EDGE_LOOP('',(#28728,#28729,#28730,#28731)) ;
#5981 = EDGE_LOOP('',(#28732,#28733,#28734,#28735)) ;
#5982 = EDGE_LOOP('',(#28736,#28737,#28738,#28739)) ;
#5983 = EDGE_LOOP('',(#28740,#28741,#28742,#28743)) ;
#5984 = EDGE_LOOP('',(#28744,#28745,#28746,#28747)) ;
#5985 = EDGE_LOOP('',(#28748,#28749,#28750,#28751)) ;
#5986 = EDGE_LOOP('',(#28752,#28753,#28754,#28755)) ;
#5987 = EDGE_LOOP('',(#28756,#28757,#28758,#28759)) ;
#5988 = EDGE_LOOP('',(#28760,#28761,#28762,#28763)) ;
#5989 = EDGE_LOOP('',(#28764,#28765,#28766,#28767)) ;
#5990 = EDGE_LOOP('',(#28768,#28769,#28770,#28771)) ;
#5991 = EDGE_LOOP('',(#28772,#28773,#28774,#28775)) ;
#5992 = EDGE_LOOP('',(#28776,#28777,#28778,#28779)) ;
#5993 = EDGE_LOOP('',(#28780,#28781,#28782,#28783)) ;
#5994 = EDGE_LOOP('',(#28784,#28785,#28786,#28787)) ;
#5995 = EDGE_LOOP('',(#28788,#28789,#28790,#28791)) ;
#5996 = EDGE_LOOP('',(#28792,#28793,#28794,#28795)) ;
#5997 = EDGE_LOOP('',(#28796,#28797,#28798,#28799)) ;
#5998 = EDGE_LOOP('',(#28800,#28801,#28802,#28803)) ;
#5999 = EDGE_LOOP('',(#28804,#28805,#28806,#28807)) ;
#6000 = EDGE_LOOP('',(#28808,#28809,#28810)) ;
#6001 = EDGE_LOOP('',(#28811,#28812,#28813)) ;
#6002 = EDGE_LOOP('',(#28814,#28815,#28816,#28817)) ;
#6003 = EDGE_LOOP('',(#28818,#28819,#28820,#28821)) ;
#6004 = EDGE_LOOP('',(#28822,#28823,#28824,#28825)) ;
#6005 = EDGE_LOOP('',(#28826,#28827,#28828,#28829)) ;
#6006 = EDGE_LOOP('',(#28830,#28831,#28832,#28833)) ;
#6007 = EDGE_LOOP('',(#28834,#28835,#28836)) ;
#6008 = EDGE_LOOP('',(#28837,#28838,#28839)) ;
#6009 = EDGE_LOOP('',(#28840,#28841,#28842)) ;
#6010 = EDGE_LOOP('',(#28843,#28844,#28845)) ;
#6011 = EDGE_LOOP('',(#28846,#28847,#28848,#28849)) ;
#6012 = EDGE_LOOP('',(#28850,#28851,#28852,#28853)) ;
#6013 = EDGE_LOOP('',(#28854,#28855,#28856,#28857)) ;
#6014 = EDGE_LOOP('',(#28858,#28859,#28860,#28861,#28862,#28863,#28864,#28865,
#28866,#28867,#28868,#28869,#28870,#28871,#28872,#28873)) ;
#6015 = EDGE_LOOP('',(#28874)) ;
#6016 = EDGE_LOOP('',(#28875,#28876,#28877,#28878,#28879)) ;
#6017 = EDGE_LOOP('',(#28880,#28881,#28882,#28883,#28884)) ;
#6018 = EDGE_LOOP('',(#28885)) ;
#6019 = EDGE_LOOP('',(#28886,#28887,#28888,#28889)) ;
#6020 = EDGE_LOOP('',(#28890,#28891,#28892,#28893,#28894,#28895,#28896,#28897,
#28898,#28899,#28900,#28901)) ;
#6021 = EDGE_LOOP('',(#28902,#28903,#28904,#28905,#28906,#28907,#28908,#28909,
#28910,#28911,#28912,#28913)) ;
#6022 = EDGE_LOOP('',(#28914,#28915,#28916,#28917)) ;
#6023 = EDGE_LOOP('',(#28918,#28919,#28920,#28921)) ;
#6024 = EDGE_LOOP('',(#28922,#28923,#28924,#28925)) ;
#6025 = EDGE_LOOP('',(#28926,#28927,#28928,#28929)) ;
#6026 = EDGE_LOOP('',(#28930,#28931,#28932,#28933)) ;
#6027 = EDGE_LOOP('',(#28934,#28935,#28936,#28937)) ;
#6028 = EDGE_LOOP('',(#28938,#28939,#28940,#28941,#28942,#28943,#28944,#28945,
#28946,#28947,#28948,#28949,#28950,#28951,#28952,#28953,#28954,#28955,#28956,
#28957,#28958,#28959,#28960,#28961,#28962)) ;
#6029 = EDGE_LOOP('',(#28963)) ;
#6030 = EDGE_LOOP('',(#28964,#28965,#28966,#28967)) ;
#6031 = EDGE_LOOP('',(#28968,#28969,#28970,#28971)) ;
#6032 = EDGE_LOOP('',(#28972,#28973,#28974,#28975)) ;
#6033 = EDGE_LOOP('',(#28976,#28977,#28978,#28979)) ;
#6034 = EDGE_LOOP('',(#28980,#28981,#28982,#28983)) ;
#6035 = EDGE_LOOP('',(#28984,#28985,#28986,#28987)) ;
#6036 = EDGE_LOOP('',(#28988,#28989,#28990,#28991)) ;
#6037 = EDGE_LOOP('',(#28992,#28993,#28994,#28995)) ;
#6038 = EDGE_LOOP('',(#28996,#28997,#28998,#28999)) ;
#6039 = EDGE_LOOP('',(#29000,#29001,#29002,#29003)) ;
#6040 = EDGE_LOOP('',(#29004,#29005,#29006,#29007)) ;
#6041 = EDGE_LOOP('',(#29008,#29009,#29010,#29011)) ;
#6042 = EDGE_LOOP('',(#29012,#29013,#29014,#29015)) ;
#6043 = EDGE_LOOP('',(#29016,#29017,#29018,#29019)) ;
#6044 = EDGE_LOOP('',(#29020,#29021,#29022,#29023)) ;
#6045 = EDGE_LOOP('',(#29024,#29025,#29026,#29027)) ;
#6046 = EDGE_LOOP('',(#29028,#29029,#29030,#29031)) ;
#6047 = EDGE_LOOP('',(#29032,#29033,#29034,#29035)) ;
#6048 = EDGE_LOOP('',(#29036,#29037,#29038,#29039)) ;
#6049 = EDGE_LOOP('',(#29040,#29041,#29042,#29043)) ;
#6050 = EDGE_LOOP('',(#29044,#29045,#29046,#29047)) ;
#6051 = EDGE_LOOP('',(#29048,#29049,#29050,#29051)) ;
#6052 = EDGE_LOOP('',(#29052,#29053,#29054,#29055)) ;
#6053 = EDGE_LOOP('',(#29056,#29057,#29058,#29059)) ;
#6054 = EDGE_LOOP('',(#29060,#29061,#29062,#29063)) ;
#6055 = EDGE_LOOP('',(#29064,#29065,#29066,#29067)) ;
#6056 = EDGE_LOOP('',(#29068,#29069,#29070,#29071)) ;
#6057 = EDGE_LOOP('',(#29072,#29073,#29074,#29075)) ;
#6058 = EDGE_LOOP('',(#29076,#29077,#29078,#29079)) ;
#6059 = EDGE_LOOP('',(#29080,#29081,#29082,#29083)) ;
#6060 = EDGE_LOOP('',(#29084,#29085,#29086,#29087)) ;
#6061 = EDGE_LOOP('',(#29088,#29089,#29090,#29091)) ;
#6062 = EDGE_LOOP('',(#29092,#29093,#29094,#29095)) ;
#6063 = EDGE_LOOP('',(#29096,#29097,#29098,#29099)) ;
#6064 = EDGE_LOOP('',(#29100,#29101,#29102,#29103)) ;
#6065 = EDGE_LOOP('',(#29104,#29105,#29106,#29107)) ;
#6066 = EDGE_LOOP('',(#29108,#29109,#29110,#29111)) ;
#6067 = EDGE_LOOP('',(#29112,#29113,#29114,#29115)) ;
#6068 = EDGE_LOOP('',(#29116,#29117,#29118,#29119)) ;
#6069 = EDGE_LOOP('',(#29120,#29121,#29122,#29123)) ;
#6070 = EDGE_LOOP('',(#29124,#29125,#29126,#29127)) ;
#6071 = EDGE_LOOP('',(#29128,#29129,#29130)) ;
#6072 = EDGE_LOOP('',(#29131,#29132,#29133,#29134)) ;
#6073 = EDGE_LOOP('',(#29135,#29136,#29137)) ;
#6074 = EDGE_LOOP('',(#29138,#29139,#29140,#29141)) ;
#6075 = EDGE_LOOP('',(#29142,#29143,#29144,#29145)) ;
#6076 = EDGE_LOOP('',(#29146,#29147,#29148,#29149)) ;
#6077 = EDGE_LOOP('',(#29150,#29151,#29152,#29153)) ;
#6078 = EDGE_LOOP('',(#29154,#29155,#29156)) ;
#6079 = EDGE_LOOP('',(#29157,#29158,#29159,#29160)) ;
#6080 = EDGE_LOOP('',(#29161,#29162,#29163)) ;
#6081 = EDGE_LOOP('',(#29164,#29165,#29166,#29167)) ;
#6082 = EDGE_LOOP('',(#29168,#29169,#29170,#29171)) ;
#6083 = EDGE_LOOP('',(#29172,#29173,#29174,#29175)) ;
#6084 = EDGE_LOOP('',(#29176,#29177,#29178,#29179)) ;
#6085 = EDGE_LOOP('',(#29180,#29181,#29182)) ;
#6086 = EDGE_LOOP('',(#29183,#29184,#29185,#29186)) ;
#6087 = EDGE_LOOP('',(#29187,#29188,#29189)) ;
#6088 = EDGE_LOOP('',(#29190,#29191,#29192,#29193)) ;
#6089 = EDGE_LOOP('',(#29194,#29195,#29196,#29197)) ;
#6090 = EDGE_LOOP('',(#29198,#29199,#29200,#29201)) ;
#6091 = EDGE_LOOP('',(#29202,#29203,#29204,#29205)) ;
#6092 = EDGE_LOOP('',(#29206,#29207,#29208)) ;
#6093 = EDGE_LOOP('',(#29209,#29210,#29211,#29212)) ;
#6094 = EDGE_LOOP('',(#29213,#29214,#29215)) ;
#6095 = EDGE_LOOP('',(#29216,#29217,#29218,#29219)) ;
#6096 = EDGE_LOOP('',(#29220,#29221,#29222,#29223)) ;
#6097 = EDGE_LOOP('',(#29224,#29225,#29226,#29227)) ;
#6098 = EDGE_LOOP('',(#29228,#29229,#29230,#29231,#29232,#29233,#29234,#29235,
#29236,#29237,#29238,#29239,#29240,#29241,#29242,#29243,#29244,#29245,#29246,
#29247,#29248,#29249)) ;
#6099 = EDGE_LOOP('',(#29250,#29251,#29252,#29253,#29254,#29255,#29256,#29257,
#29258,#29259,#29260,#29261,#29262,#29263,#29264,#29265,#29266,#29267,#29268,
#29269,#29270,#29271)) ;
#6100 = EDGE_LOOP('',(#29272,#29273,#29274,#29275,#29276,#29277,#29278,#29279,
#29280,#29281,#29282,#29283,#29284,#29285,#29286,#29287,#29288,#29289,#29290,
#29291,#29292,#29293)) ;
#6101 = EDGE_LOOP('',(#29294,#29295,#29296,#29297,#29298,#29299,#29300,#29301,
#29302,#29303,#29304,#29305,#29306,#29307,#29308,#29309,#29310,#29311,#29312,
#29313,#29314,#29315)) ;
#6102 = EDGE_LOOP('',(#29316,#29317,#29318,#29319,#29320,#29321,#29322,#29323,
#29324,#29325,#29326,#29327,#29328,#29329,#29330,#29331,#29332,#29333,#29334,
#29335,#29336,#29337,#29338,#29339,#29340)) ;
#6103 = EDGE_LOOP('',(#29341)) ;
#6104 = EDGE_LOOP('',(#29342,#29343,#29344,#29345)) ;
#6105 = EDGE_LOOP('',(#29346,#29347,#29348)) ;
#6106 = EDGE_LOOP('',(#29349,#29350,#29351)) ;
#6107 = EDGE_LOOP('',(#29352,#29353,#29354,#29355)) ;
#6108 = EDGE_LOOP('',(#29356,#29357,#29358)) ;
#6109 = EDGE_LOOP('',(#29359,#29360,#29361)) ;
#6110 = EDGE_LOOP('',(#29362,#29363,#29364,#29365)) ;
#6111 = EDGE_LOOP('',(#29366,#29367,#29368,#29369)) ;
#6112 = EDGE_LOOP('',(#29370,#29371,#29372)) ;
#6113 = EDGE_LOOP('',(#29373,#29374,#29375)) ;
#6114 = EDGE_LOOP('',(#29376,#29377,#29378,#29379)) ;
#6115 = EDGE_LOOP('',(#29380,#29381,#29382)) ;
#6116 = EDGE_LOOP('',(#29383,#29384,#29385)) ;
#6117 = EDGE_LOOP('',(#29386,#29387,#29388,#29389,#29390,#29391,#29392,#29393)) ;
#6118 = EDGE_LOOP('',(#29394,#29395,#29396,#29397,#29398,#29399)) ;
#6119 = EDGE_LOOP('',(#29400,#29401,#29402,#29403,#29404,#29405)) ;
#6120 = EDGE_LOOP('',(#29406,#29407,#29408,#29409,#29410,#29411)) ;
#6121 = EDGE_LOOP('',(#29412,#29413,#29414,#29415,#29416,#29417)) ;
#6122 = EDGE_LOOP('',(#29418,#29419,#29420,#29421,#29422,#29423)) ;
#6123 = EDGE_LOOP('',(#29424,#29425,#29426,#29427,#29428,#29429)) ;
#6124 = EDGE_LOOP('',(#29430,#29431,#29432,#29433)) ;
#6125 = EDGE_LOOP('',(#29434,#29435,#29436,#29437,#29438,#29439)) ;
#6126 = EDGE_LOOP('',(#29440,#29441,#29442,#29443,#29444,#29445)) ;
#6127 = EDGE_LOOP('',(#29446,#29447,#29448,#29449,#29450,#29451)) ;
#6128 = EDGE_LOOP('',(#29452,#29453,#29454,#29455,#29456,#29457)) ;
#6129 = EDGE_LOOP('',(#29458,#29459,#29460,#29461)) ;
#6130 = EDGE_LOOP('',(#29462,#29463,#29464,#29465,#29466,#29467)) ;
#6131 = EDGE_LOOP('',(#29468,#29469,#29470,#29471,#29472,#29473)) ;
#6132 = EDGE_LOOP('',(#29474,#29475,#29476,#29477)) ;
#6133 = EDGE_LOOP('',(#29478,#29479,#29480,#29481)) ;
#6134 = EDGE_LOOP('',(#29482)) ;
#6135 = EDGE_LOOP('',(#29483)) ;
#6136 = EDGE_LOOP('',(#29484)) ;
#6137 = EDGE_LOOP('',(#29485)) ;
#6138 = EDGE_LOOP('',(#29486)) ;
#6139 = EDGE_LOOP('',(#29487,#29488,#29489,#29490)) ;
#6140 = EDGE_LOOP('',(#29491)) ;
#6141 = EDGE_LOOP('',(#29492)) ;
#6142 = EDGE_LOOP('',(#29493)) ;
#6143 = EDGE_LOOP('',(#29494)) ;
#6144 = EDGE_LOOP('',(#29495)) ;
#6145 = EDGE_LOOP('',(#29496,#29497,#29498,#29499,#29500,#29501)) ;
#6146 = EDGE_LOOP('',(#29502,#29503,#29504,#29505)) ;
#6147 = EDGE_LOOP('',(#29506,#29507,#29508,#29509,#29510,#29511)) ;
#6148 = EDGE_LOOP('',(#29512,#29513,#29514,#29515,#29516,#29517)) ;
#6149 = EDGE_LOOP('',(#29518,#29519,#29520,#29521)) ;
#6150 = EDGE_LOOP('',(#29522,#29523,#29524,#29525)) ;
#6151 = EDGE_LOOP('',(#29526,#29527,#29528,#29529)) ;
#6152 = EDGE_LOOP('',(#29530,#29531,#29532,#29533)) ;
#6153 = EDGE_LOOP('',(#29534,#29535,#29536,#29537)) ;
#6154 = EDGE_LOOP('',(#29538,#29539,#29540,#29541)) ;
#6155 = EDGE_LOOP('',(#29542,#29543,#29544,#29545)) ;
#6156 = EDGE_LOOP('',(#29546,#29547,#29548,#29549)) ;
#6157 = EDGE_LOOP('',(#29550,#29551,#29552,#29553)) ;
#6158 = EDGE_LOOP('',(#29554,#29555,#29556,#29557)) ;
#6159 = EDGE_LOOP('',(#29558,#29559,#29560,#29561)) ;
#6160 = EDGE_LOOP('',(#29562,#29563,#29564,#29565)) ;
#6161 = EDGE_LOOP('',(#29566,#29567,#29568,#29569)) ;
#6162 = EDGE_LOOP('',(#29570,#29571,#29572,#29573)) ;
#6163 = EDGE_LOOP('',(#29574,#29575,#29576,#29577)) ;
#6164 = EDGE_LOOP('',(#29578,#29579,#29580,#29581)) ;
#6165 = EDGE_LOOP('',(#29582,#29583,#29584,#29585)) ;
#6166 = EDGE_LOOP('',(#29586,#29587,#29588,#29589)) ;
#6167 = EDGE_LOOP('',(#29590,#29591,#29592,#29593)) ;
#6168 = EDGE_LOOP('',(#29594,#29595,#29596,#29597)) ;
#6169 = EDGE_LOOP('',(#29598,#29599,#29600,#29601,#29602)) ;
#6170 = EDGE_LOOP('',(#29603,#29604,#29605,#29606)) ;
#6171 = EDGE_LOOP('',(#29607,#29608,#29609,#29610)) ;
#6172 = EDGE_LOOP('',(#29611,#29612,#29613,#29614)) ;
#6173 = EDGE_LOOP('',(#29615,#29616,#29617,#29618)) ;
#6174 = EDGE_LOOP('',(#29619,#29620,#29621,#29622)) ;
#6175 = EDGE_LOOP('',(#29623,#29624,#29625,#29626)) ;
#6176 = EDGE_LOOP('',(#29627,#29628,#29629,#29630)) ;
#6177 = EDGE_LOOP('',(#29631,#29632,#29633,#29634)) ;
#6178 = EDGE_LOOP('',(#29635,#29636,#29637,#29638)) ;
#6179 = EDGE_LOOP('',(#29639,#29640,#29641,#29642)) ;
#6180 = EDGE_LOOP('',(#29643,#29644,#29645,#29646)) ;
#6181 = EDGE_LOOP('',(#29647,#29648,#29649,#29650)) ;
#6182 = EDGE_LOOP('',(#29651,#29652,#29653,#29654)) ;
#6183 = EDGE_LOOP('',(#29655,#29656,#29657,#29658)) ;
#6184 = EDGE_LOOP('',(#29659,#29660,#29661,#29662)) ;
#6185 = EDGE_LOOP('',(#29663,#29664,#29665,#29666)) ;
#6186 = EDGE_LOOP('',(#29667,#29668,#29669,#29670,#29671)) ;
#6187 = EDGE_LOOP('',(#29672,#29673,#29674,#29675)) ;
#6188 = EDGE_LOOP('',(#29676,#29677,#29678,#29679)) ;
#6189 = EDGE_LOOP('',(#29680,#29681,#29682,#29683)) ;
#6190 = EDGE_LOOP('',(#29684,#29685,#29686,#29687)) ;
#6191 = EDGE_LOOP('',(#29688,#29689,#29690,#29691,#29692)) ;
#6192 = EDGE_LOOP('',(#29693)) ;
#6193 = EDGE_LOOP('',(#29694,#29695,#29696,#29697,#29698,#29699,#29700,#29701,
#29702,#29703,#29704,#29705,#29706,#29707,#29708,#29709,#29710,#29711,#29712,
#29713)) ;
#6194 = EDGE_LOOP('',(#29714,#29715,#29716,#29717,#29718,#29719)) ;
#6195 = EDGE_LOOP('',(#29720,#29721,#29722,#29723,#29724)) ;
#6196 = EDGE_LOOP('',(#29725)) ;
#6197 = EDGE_LOOP('',(#29726,#29727,#29728,#29729)) ;
#6198 = EDGE_LOOP('',(#29730,#29731,#29732,#29733,#29734,#29735,#29736,#29737,
#29738,#29739,#29740,#29741,#29742,#29743,#29744,#29745,#29746,#29747,#29748,
#29749,#29750,#29751,#29752,#29753,#29754,#29755,#29756,#29757,#29758,#29759,
#29760,#29761,#29762,#29763,#29764,#29765,#29766)) ;
#6199 = EDGE_LOOP('',(#29767,#29768,#29769,#29770,#29771,#29772,#29773,#29774,
#29775,#29776,#29777,#29778,#29779,#29780,#29781,#29782,#29783,#29784,#29785,
#29786,#29787,#29788,#29789,#29790,#29791,#29792,#29793,#29794,#29795,#29796,
#29797,#29798,#29799,#29800,#29801)) ;
#6200 = EDGE_LOOP('',(#29802,#29803,#29804)) ;
#6201 = EDGE_LOOP('',(#29805,#29806,#29807)) ;
#6202 = EDGE_LOOP('',(#29808,#29809,#29810,#29811)) ;
#6203 = EDGE_LOOP('',(#29812,#29813,#29814,#29815)) ;
#6204 = EDGE_LOOP('',(#29816,#29817,#29818,#29819)) ;
#6205 = EDGE_LOOP('',(#29820,#29821,#29822,#29823)) ;
#6206 = EDGE_LOOP('',(#29824,#29825,#29826,#29827)) ;
#6207 = EDGE_LOOP('',(#29828,#29829,#29830,#29831,#29832,#29833,#29834,#29835,
#29836,#29837,#29838,#29839,#29840,#29841,#29842,#29843,#29844,#29845,#29846,
#29847)) ;
#6208 = EDGE_LOOP('',(#29848,#29849,#29850,#29851)) ;
#6209 = EDGE_LOOP('',(#29852,#29853,#29854,#29855)) ;
#6210 = EDGE_LOOP('',(#29856,#29857,#29858,#29859)) ;
#6211 = EDGE_LOOP('',(#29860,#29861,#29862,#29863)) ;
#6212 = EDGE_LOOP('',(#29864,#29865,#29866,#29867)) ;
#6213 = EDGE_LOOP('',(#29868,#29869,#29870,#29871)) ;
#6214 = EDGE_LOOP('',(#29872,#29873,#29874,#29875)) ;
#6215 = EDGE_LOOP('',(#29876,#29877,#29878,#29879)) ;
#6216 = EDGE_LOOP('',(#29880,#29881,#29882,#29883)) ;
#6217 = EDGE_LOOP('',(#29884,#29885,#29886,#29887)) ;
#6218 = EDGE_LOOP('',(#29888,#29889,#29890,#29891)) ;
#6219 = EDGE_LOOP('',(#29892,#29893,#29894,#29895)) ;
#6220 = EDGE_LOOP('',(#29896,#29897,#29898,#29899)) ;
#6221 = EDGE_LOOP('',(#29900,#29901,#29902,#29903)) ;
#6222 = EDGE_LOOP('',(#29904,#29905,#29906,#29907)) ;
#6223 = EDGE_LOOP('',(#29908,#29909,#29910,#29911)) ;
#6224 = EDGE_LOOP('',(#29912,#29913,#29914,#29915)) ;
#6225 = EDGE_LOOP('',(#29916,#29917,#29918,#29919)) ;
#6226 = EDGE_LOOP('',(#29920,#29921,#29922,#29923)) ;
#6227 = EDGE_LOOP('',(#29924,#29925,#29926,#29927,#29928)) ;
#6228 = EDGE_LOOP('',(#29929,#29930,#29931,#29932,#29933,#29934)) ;
#6229 = EDGE_LOOP('',(#29935)) ;
#6230 = EDGE_LOOP('',(#29936)) ;
#6231 = EDGE_LOOP('',(#29937,#29938,#29939,#29940,#29941)) ;
#6232 = EDGE_LOOP('',(#29942)) ;
#6233 = EDGE_LOOP('',(#29943)) ;
#6234 = EDGE_LOOP('',(#29944,#29945,#29946,#29947)) ;
#6235 = LINE('',#46354,#8554) ;
#6236 = LINE('',#46357,#8555) ;
#6237 = LINE('',#46360,#8556) ;
#6238 = LINE('',#46362,#8557) ;
#6239 = LINE('',#46364,#8558) ;
#6240 = LINE('',#46366,#8559) ;
#6241 = LINE('',#46367,#8560) ;
#6242 = LINE('',#46414,#8561) ;
#6243 = LINE('',#46418,#8562) ;
#6244 = LINE('',#46422,#8563) ;
#6245 = LINE('',#46426,#8564) ;
#6246 = LINE('',#46430,#8565) ;
#6247 = LINE('',#46434,#8566) ;
#6248 = LINE('',#46438,#8567) ;
#6249 = LINE('',#46442,#8568) ;
#6250 = LINE('',#46446,#8569) ;
#6251 = LINE('',#46450,#8570) ;
#6252 = LINE('',#46454,#8571) ;
#6253 = LINE('',#46458,#8572) ;
#6254 = LINE('',#46509,#8573) ;
#6255 = LINE('',#46514,#8574) ;
#6256 = LINE('',#46518,#8575) ;
#6257 = LINE('',#46522,#8576) ;
#6258 = LINE('',#46526,#8577) ;
#6259 = LINE('',#46530,#8578) ;
#6260 = LINE('',#46534,#8579) ;
#6261 = LINE('',#46538,#8580) ;
#6262 = LINE('',#46542,#8581) ;
#6263 = LINE('',#46546,#8582) ;
#6264 = LINE('',#46549,#8583) ;
#6265 = LINE('',#46559,#8584) ;
#6266 = LINE('',#46562,#8585) ;
#6267 = LINE('',#46565,#8586) ;
#6268 = LINE('',#46567,#8587) ;
#6269 = LINE('',#46568,#8588) ;
#6270 = LINE('',#46570,#8589) ;
#6271 = LINE('',#46571,#8590) ;
#6272 = LINE('',#46574,#8591) ;
#6273 = LINE('',#46578,#8592) ;
#6274 = LINE('',#46582,#8593) ;
#6275 = LINE('',#46586,#8594) ;
#6276 = LINE('',#46590,#8595) ;
#6277 = LINE('',#46594,#8596) ;
#6278 = LINE('',#46598,#8597) ;
#6279 = LINE('',#46602,#8598) ;
#6280 = LINE('',#46613,#8599) ;
#6281 = LINE('',#46616,#8600) ;
#6282 = LINE('',#46619,#8601) ;
#6283 = LINE('',#46620,#8602) ;
#6284 = LINE('',#46622,#8603) ;
#6285 = LINE('',#46623,#8604) ;
#6286 = LINE('',#46626,#8605) ;
#6287 = LINE('',#46630,#8606) ;
#6288 = LINE('',#46634,#8607) ;
#6289 = LINE('',#46638,#8608) ;
#6290 = LINE('',#46642,#8609) ;
#6291 = LINE('',#46646,#8610) ;
#6292 = LINE('',#46650,#8611) ;
#6293 = LINE('',#46654,#8612) ;
#6294 = LINE('',#46662,#8613) ;
#6295 = LINE('',#46665,#8614) ;
#6296 = LINE('',#46668,#8615) ;
#6297 = LINE('',#46669,#8616) ;
#6298 = LINE('',#46671,#8617) ;
#6299 = LINE('',#46672,#8618) ;
#6300 = LINE('',#46674,#8619) ;
#6301 = LINE('',#46680,#8620) ;
#6302 = LINE('',#46683,#8621) ;
#6303 = LINE('',#46685,#8622) ;
#6304 = LINE('',#46687,#8623) ;
#6305 = LINE('',#46689,#8624) ;
#6306 = LINE('',#46690,#8625) ;
#6307 = LINE('',#46693,#8626) ;
#6308 = LINE('',#46694,#8627) ;
#6309 = LINE('',#46696,#8628) ;
#6310 = LINE('',#46698,#8629) ;
#6311 = LINE('',#46700,#8630) ;
#6312 = LINE('',#46701,#8631) ;
#6313 = LINE('',#46718,#8632) ;
#6314 = LINE('',#46721,#8633) ;
#6315 = LINE('',#46726,#8634) ;
#6316 = LINE('',#46729,#8635) ;
#6317 = LINE('',#46734,#8636) ;
#6318 = LINE('',#46737,#8637) ;
#6319 = LINE('',#46742,#8638) ;
#6320 = LINE('',#46745,#8639) ;
#6321 = LINE('',#46750,#8640) ;
#6322 = LINE('',#46753,#8641) ;
#6323 = LINE('',#46758,#8642) ;
#6324 = LINE('',#46761,#8643) ;
#6325 = LINE('',#46842,#8644) ;
#6326 = LINE('',#46846,#8645) ;
#6327 = LINE('',#46850,#8646) ;
#6328 = LINE('',#46854,#8647) ;
#6329 = LINE('',#46858,#8648) ;
#6330 = LINE('',#46861,#8649) ;
#6331 = LINE('',#46864,#8650) ;
#6332 = LINE('',#46871,#8651) ;
#6333 = LINE('',#46875,#8652) ;
#6334 = LINE('',#46878,#8653) ;
#6335 = LINE('',#46879,#8654) ;
#6336 = LINE('',#46881,#8655) ;
#6337 = LINE('',#46883,#8656) ;
#6338 = LINE('',#46884,#8657) ;
#6339 = LINE('',#46886,#8658) ;
#6340 = LINE('',#46888,#8659) ;
#6341 = LINE('',#46917,#8660) ;
#6342 = LINE('',#46918,#8661) ;
#6343 = LINE('',#46920,#8662) ;
#6344 = LINE('',#46922,#8663) ;
#6345 = LINE('',#46951,#8664) ;
#6346 = LINE('',#46952,#8665) ;
#6347 = LINE('',#46954,#8666) ;
#6348 = LINE('',#46956,#8667) ;
#6349 = LINE('',#46958,#8668) ;
#6350 = LINE('',#46961,#8669) ;
#6351 = LINE('',#46965,#8670) ;
#6352 = LINE('',#46966,#8671) ;
#6353 = LINE('',#46969,#8672) ;
#6354 = LINE('',#46972,#8673) ;
#6355 = LINE('',#46973,#8674) ;
#6356 = LINE('',#46980,#8675) ;
#6357 = LINE('',#46983,#8676) ;
#6358 = LINE('',#46986,#8677) ;
#6359 = LINE('',#46988,#8678) ;
#6360 = LINE('',#46989,#8679) ;
#6361 = LINE('',#46992,#8680) ;
#6362 = LINE('',#46994,#8681) ;
#6363 = LINE('',#46996,#8682) ;
#6364 = LINE('',#47001,#8683) ;
#6365 = LINE('',#47005,#8684) ;
#6366 = LINE('',#47007,#8685) ;
#6367 = LINE('',#47009,#8686) ;
#6368 = LINE('',#47012,#8687) ;
#6369 = LINE('',#47013,#8688) ;
#6370 = LINE('',#47015,#8689) ;
#6371 = LINE('',#47017,#8690) ;
#6372 = LINE('',#47018,#8691) ;
#6373 = LINE('',#47020,#8692) ;
#6374 = LINE('',#47023,#8693) ;
#6375 = LINE('',#47024,#8694) ;
#6376 = LINE('',#47026,#8695) ;
#6377 = LINE('',#47028,#8696) ;
#6378 = LINE('',#47029,#8697) ;
#6379 = LINE('',#47032,#8698) ;
#6380 = LINE('',#47034,#8699) ;
#6381 = LINE('',#47035,#8700) ;
#6382 = LINE('',#47037,#8701) ;
#6383 = LINE('',#47039,#8702) ;
#6384 = LINE('',#47041,#8703) ;
#6385 = LINE('',#47044,#8704) ;
#6386 = LINE('',#47045,#8705) ;
#6387 = LINE('',#47047,#8706) ;
#6388 = LINE('',#47049,#8707) ;
#6389 = LINE('',#47051,#8708) ;
#6390 = LINE('',#47053,#8709) ;
#6391 = LINE('',#47059,#8710) ;
#6392 = LINE('',#47064,#8711) ;
#6393 = LINE('',#47066,#8712) ;
#6394 = LINE('',#47069,#8713) ;
#6395 = LINE('',#47071,#8714) ;
#6396 = LINE('',#47072,#8715) ;
#6397 = LINE('',#47074,#8716) ;
#6398 = LINE('',#47075,#8717) ;
#6399 = LINE('',#47080,#8718) ;
#6400 = LINE('',#47082,#8719) ;
#6401 = LINE('',#47086,#8720) ;
#6402 = LINE('',#47088,#8721) ;
#6403 = LINE('',#47090,#8722) ;
#6404 = LINE('',#47092,#8723) ;
#6405 = LINE('',#47094,#8724) ;
#6406 = LINE('',#47095,#8725) ;
#6407 = LINE('',#47097,#8726) ;
#6408 = LINE('',#47099,#8727) ;
#6409 = LINE('',#47102,#8728) ;
#6410 = LINE('',#47103,#8729) ;
#6411 = LINE('',#47105,#8730) ;
#6412 = LINE('',#47107,#8731) ;
#6413 = LINE('',#47110,#8732) ;
#6414 = LINE('',#47111,#8733) ;
#6415 = LINE('',#47113,#8734) ;
#6416 = LINE('',#47115,#8735) ;
#6417 = LINE('',#47118,#8736) ;
#6418 = LINE('',#47119,#8737) ;
#6419 = LINE('',#47121,#8738) ;
#6420 = LINE('',#47123,#8739) ;
#6421 = LINE('',#47126,#8740) ;
#6422 = LINE('',#47127,#8741) ;
#6423 = LINE('',#47129,#8742) ;
#6424 = LINE('',#47131,#8743) ;
#6425 = LINE('',#47134,#8744) ;
#6426 = LINE('',#47135,#8745) ;
#6427 = LINE('',#47137,#8746) ;
#6428 = LINE('',#47139,#8747) ;
#6429 = LINE('',#47142,#8748) ;
#6430 = LINE('',#47145,#8749) ;
#6431 = LINE('',#47150,#8750) ;
#6432 = LINE('',#47151,#8751) ;
#6433 = LINE('',#47153,#8752) ;
#6434 = LINE('',#47154,#8753) ;
#6435 = LINE('',#47158,#8754) ;
#6436 = LINE('',#47159,#8755) ;
#6437 = LINE('',#47161,#8756) ;
#6438 = LINE('',#47162,#8757) ;
#6439 = LINE('',#47166,#8758) ;
#6440 = LINE('',#47167,#8759) ;
#6441 = LINE('',#47169,#8760) ;
#6442 = LINE('',#47170,#8761) ;
#6443 = LINE('',#47179,#8762) ;
#6444 = LINE('',#47210,#8763) ;
#6445 = LINE('',#47286,#8764) ;
#6446 = LINE('',#47364,#8765) ;
#6447 = LINE('',#47442,#8766) ;
#6448 = LINE('',#47481,#8767) ;
#6449 = LINE('',#47524,#8768) ;
#6450 = LINE('',#47600,#8769) ;
#6451 = LINE('',#47676,#8770) ;
#6452 = LINE('',#47756,#8771) ;
#6453 = LINE('',#47832,#8772) ;
#6454 = LINE('',#47883,#8773) ;
#6455 = LINE('',#47898,#8774) ;
#6456 = LINE('',#48530,#8775) ;
#6457 = LINE('',#48540,#8776) ;
#6458 = LINE('',#48557,#8777) ;
#6459 = LINE('',#48568,#8778) ;
#6460 = LINE('',#48578,#8779) ;
#6461 = LINE('',#48592,#8780) ;
#6462 = LINE('',#48639,#8781) ;
#6463 = LINE('',#48651,#8782) ;
#6464 = LINE('',#48727,#8783) ;
#6465 = LINE('',#48803,#8784) ;
#6466 = LINE('',#48879,#8785) ;
#6467 = LINE('',#48955,#8786) ;
#6468 = LINE('',#49031,#8787) ;
#6469 = LINE('',#49058,#8788) ;
#6470 = LINE('',#49085,#8789) ;
#6471 = LINE('',#49161,#8790) ;
#6472 = LINE('',#49237,#8791) ;
#6473 = LINE('',#49315,#8792) ;
#6474 = LINE('',#49531,#8793) ;
#6475 = LINE('',#49537,#8794) ;
#6476 = LINE('',#49539,#8795) ;
#6477 = LINE('',#49541,#8796) ;
#6478 = LINE('',#49543,#8797) ;
#6479 = LINE('',#49547,#8798) ;
#6480 = LINE('',#49549,#8799) ;
#6481 = LINE('',#49551,#8800) ;
#6482 = LINE('',#49553,#8801) ;
#6483 = LINE('',#49557,#8802) ;
#6484 = LINE('',#49559,#8803) ;
#6485 = LINE('',#49561,#8804) ;
#6486 = LINE('',#49563,#8805) ;
#6487 = LINE('',#49567,#8806) ;
#6488 = LINE('',#49569,#8807) ;
#6489 = LINE('',#49571,#8808) ;
#6490 = LINE('',#49572,#8809) ;
#6491 = LINE('',#49604,#8810) ;
#6492 = LINE('',#49639,#8811) ;
#6493 = LINE('',#49723,#8812) ;
#6494 = LINE('',#49724,#8813) ;
#6495 = LINE('',#49726,#8814) ;
#6496 = LINE('',#49729,#8815) ;
#6497 = LINE('',#49731,#8816) ;
#6498 = LINE('',#49733,#8817) ;
#6499 = LINE('',#49736,#8818) ;
#6500 = LINE('',#49738,#8819) ;
#6501 = LINE('',#49740,#8820) ;
#6502 = LINE('',#49746,#8821) ;
#6503 = LINE('',#49748,#8822) ;
#6504 = LINE('',#49750,#8823) ;
#6505 = LINE('',#50228,#8824) ;
#6506 = LINE('',#50299,#8825) ;
#6507 = LINE('',#50538,#8826) ;
#6508 = LINE('',#50751,#8827) ;
#6509 = LINE('',#50782,#8828) ;
#6510 = LINE('',#51024,#8829) ;
#6511 = LINE('',#51289,#8830) ;
#6512 = LINE('',#51360,#8831) ;
#6513 = LINE('',#51601,#8832) ;
#6514 = LINE('',#51825,#8833) ;
#6515 = LINE('',#51894,#8834) ;
#6516 = LINE('',#52133,#8835) ;
#6517 = LINE('',#52348,#8836) ;
#6518 = LINE('',#52397,#8837) ;
#6519 = LINE('',#52706,#8838) ;
#6520 = LINE('',#53062,#8839) ;
#6521 = LINE('',#53111,#8840) ;
#6522 = LINE('',#53420,#8841) ;
#6523 = LINE('',#53776,#8842) ;
#6524 = LINE('',#53825,#8843) ;
#6525 = LINE('',#54134,#8844) ;
#6526 = LINE('',#54490,#8845) ;
#6527 = LINE('',#54539,#8846) ;
#6528 = LINE('',#54848,#8847) ;
#6529 = LINE('',#55204,#8848) ;
#6530 = LINE('',#55275,#8849) ;
#6531 = LINE('',#55510,#8850) ;
#6532 = LINE('',#55723,#8851) ;
#6533 = LINE('',#55794,#8852) ;
#6534 = LINE('',#56035,#8853) ;
#6535 = LINE('',#56259,#8854) ;
#6536 = LINE('',#56308,#8855) ;
#6537 = LINE('',#56617,#8856) ;
#6538 = LINE('',#56973,#8857) ;
#6539 = LINE('',#57022,#8858) ;
#6540 = LINE('',#57329,#8859) ;
#6541 = LINE('',#57685,#8860) ;
#6542 = LINE('',#57754,#8861) ;
#6543 = LINE('',#57997,#8862) ;
#6544 = LINE('',#58214,#8863) ;
#6545 = LINE('',#58283,#8864) ;
#6546 = LINE('',#58524,#8865) ;
#6547 = LINE('',#58737,#8866) ;
#6548 = LINE('',#58786,#8867) ;
#6549 = LINE('',#59095,#8868) ;
#6550 = LINE('',#59451,#8869) ;
#6551 = LINE('',#59500,#8870) ;
#6552 = LINE('',#59809,#8871) ;
#6553 = LINE('',#63661,#8872) ;
#6554 = LINE('',#63664,#8873) ;
#6555 = LINE('',#63670,#8874) ;
#6556 = LINE('',#63673,#8875) ;
#6557 = LINE('',#63679,#8876) ;
#6558 = LINE('',#63682,#8877) ;
#6559 = LINE('',#63688,#8878) ;
#6560 = LINE('',#63691,#8879) ;
#6561 = LINE('',#63697,#8880) ;
#6562 = LINE('',#63700,#8881) ;
#6563 = LINE('',#63703,#8882) ;
#6564 = LINE('',#63706,#8883) ;
#6565 = LINE('',#63708,#8884) ;
#6566 = LINE('',#63712,#8885) ;
#6567 = LINE('',#63715,#8886) ;
#6568 = LINE('',#63716,#8887) ;
#6569 = LINE('',#63722,#8888) ;
#6570 = LINE('',#63725,#8889) ;
#6571 = LINE('',#63731,#8890) ;
#6572 = LINE('',#63734,#8891) ;
#6573 = LINE('',#63736,#8892) ;
#6574 = LINE('',#63738,#8893) ;
#6575 = LINE('',#63740,#8894) ;
#6576 = LINE('',#63744,#8895) ;
#6577 = LINE('',#63746,#8896) ;
#6578 = LINE('',#63748,#8897) ;
#6579 = LINE('',#63752,#8898) ;
#6580 = LINE('',#63754,#8899) ;
#6581 = LINE('',#63756,#8900) ;
#6582 = LINE('',#63758,#8901) ;
#6583 = LINE('',#63759,#8902) ;
#6584 = LINE('',#63762,#8903) ;
#6585 = LINE('',#63764,#8904) ;
#6586 = LINE('',#63766,#8905) ;
#6587 = LINE('',#63768,#8906) ;
#6588 = LINE('',#63770,#8907) ;
#6589 = LINE('',#63772,#8908) ;
#6590 = LINE('',#63776,#8909) ;
#6591 = LINE('',#63780,#8910) ;
#6592 = LINE('',#63782,#8911) ;
#6593 = LINE('',#63784,#8912) ;
#6594 = LINE('',#63786,#8913) ;
#6595 = LINE('',#63787,#8914) ;
#6596 = LINE('',#64142,#8915) ;
#6597 = LINE('',#64144,#8916) ;
#6598 = LINE('',#64146,#8917) ;
#6599 = LINE('',#64147,#8918) ;
#6600 = LINE('',#64150,#8919) ;
#6601 = LINE('',#64152,#8920) ;
#6602 = LINE('',#64154,#8921) ;
#6603 = LINE('',#64155,#8922) ;
#6604 = LINE('',#64158,#8923) ;
#6605 = LINE('',#64160,#8924) ;
#6606 = LINE('',#64162,#8925) ;
#6607 = LINE('',#64163,#8926) ;
#6608 = LINE('',#64171,#8927) ;
#6609 = LINE('',#64174,#8928) ;
#6610 = LINE('',#64176,#8929) ;
#6611 = LINE('',#64178,#8930) ;
#6612 = LINE('',#64180,#8931) ;
#6613 = LINE('',#64181,#8932) ;
#6614 = LINE('',#64183,#8933) ;
#6615 = LINE('',#64187,#8934) ;
#6616 = LINE('',#64189,#8935) ;
#6617 = LINE('',#64191,#8936) ;
#6618 = LINE('',#64195,#8937) ;
#6619 = LINE('',#64197,#8938) ;
#6620 = LINE('',#64199,#8939) ;
#6621 = LINE('',#64203,#8940) ;
#6622 = LINE('',#64205,#8941) ;
#6623 = LINE('',#64207,#8942) ;
#6624 = LINE('',#64210,#8943) ;
#6625 = LINE('',#64215,#8944) ;
#6626 = LINE('',#64217,#8945) ;
#6627 = LINE('',#64219,#8946) ;
#6628 = LINE('',#64220,#8947) ;
#6629 = LINE('',#64223,#8948) ;
#6630 = LINE('',#64225,#8949) ;
#6631 = LINE('',#64227,#8950) ;
#6632 = LINE('',#64228,#8951) ;
#6633 = LINE('',#64231,#8952) ;
#6634 = LINE('',#64233,#8953) ;
#6635 = LINE('',#64235,#8954) ;
#6636 = LINE('',#64236,#8955) ;
#6637 = LINE('',#64239,#8956) ;
#6638 = LINE('',#64241,#8957) ;
#6639 = LINE('',#64243,#8958) ;
#6640 = LINE('',#64244,#8959) ;
#6641 = LINE('',#64599,#8960) ;
#6642 = LINE('',#64603,#8961) ;
#6643 = LINE('',#64607,#8962) ;
#6644 = LINE('',#64611,#8963) ;
#6645 = LINE('',#64615,#8964) ;
#6646 = LINE('',#64617,#8965) ;
#6647 = LINE('',#64619,#8966) ;
#6648 = LINE('',#64621,#8967) ;
#6649 = LINE('',#64623,#8968) ;
#6650 = LINE('',#64625,#8969) ;
#6651 = LINE('',#64629,#8970) ;
#6652 = LINE('',#64632,#8971) ;
#6653 = LINE('',#64635,#8972) ;
#6654 = LINE('',#64637,#8973) ;
#6655 = LINE('',#64639,#8974) ;
#6656 = LINE('',#64641,#8975) ;
#6657 = LINE('',#64643,#8976) ;
#6658 = LINE('',#64647,#8977) ;
#6659 = LINE('',#64649,#8978) ;
#6660 = LINE('',#64651,#8979) ;
#6661 = LINE('',#64655,#8980) ;
#6662 = LINE('',#64656,#8981) ;
#6663 = LINE('',#64657,#8982) ;
#6664 = LINE('',#64662,#8983) ;
#6665 = LINE('',#64664,#8984) ;
#6666 = LINE('',#64666,#8985) ;
#6667 = LINE('',#64667,#8986) ;
#6668 = LINE('',#64670,#8987) ;
#6669 = LINE('',#64672,#8988) ;
#6670 = LINE('',#64674,#8989) ;
#6671 = LINE('',#64675,#8990) ;
#6672 = LINE('',#64678,#8991) ;
#6673 = LINE('',#64680,#8992) ;
#6674 = LINE('',#64682,#8993) ;
#6675 = LINE('',#64683,#8994) ;
#6676 = LINE('',#64688,#8995) ;
#6677 = LINE('',#64692,#8996) ;
#6678 = LINE('',#64694,#8997) ;
#6679 = LINE('',#64695,#8998) ;
#6680 = LINE('',#65050,#8999) ;
#6681 = LINE('',#65052,#9000) ;
#6682 = LINE('',#65056,#9001) ;
#6683 = LINE('',#65058,#9002) ;
#6684 = LINE('',#65060,#9003) ;
#6685 = LINE('',#65064,#9004) ;
#6686 = LINE('',#65066,#9005) ;
#6687 = LINE('',#65068,#9006) ;
#6688 = LINE('',#65072,#9007) ;
#6689 = LINE('',#65074,#9008) ;
#6690 = LINE('',#65076,#9009) ;
#6691 = LINE('',#65080,#9010) ;
#6692 = LINE('',#65082,#9011) ;
#6693 = LINE('',#65084,#9012) ;
#6694 = LINE('',#65086,#9013) ;
#6695 = LINE('',#65087,#9014) ;
#6696 = LINE('',#65088,#9015) ;
#6697 = LINE('',#65093,#9016) ;
#6698 = LINE('',#65097,#9017) ;
#6699 = LINE('',#65101,#9018) ;
#6700 = LINE('',#65104,#9019) ;
#6701 = LINE('',#65459,#9020) ;
#6702 = LINE('',#65463,#9021) ;
#6703 = LINE('',#65465,#9022) ;
#6704 = LINE('',#65466,#9023) ;
#6705 = LINE('',#65469,#9024) ;
#6706 = LINE('',#65471,#9025) ;
#6707 = LINE('',#65473,#9026) ;
#6708 = LINE('',#65474,#9027) ;
#6709 = LINE('',#65477,#9028) ;
#6710 = LINE('',#65479,#9029) ;
#6711 = LINE('',#65481,#9030) ;
#6712 = LINE('',#65482,#9031) ;
#6713 = LINE('',#65485,#9032) ;
#6714 = LINE('',#65487,#9033) ;
#6715 = LINE('',#65489,#9034) ;
#6716 = LINE('',#65490,#9035) ;
#6717 = LINE('',#65493,#9036) ;
#6718 = LINE('',#65495,#9037) ;
#6719 = LINE('',#65497,#9038) ;
#6720 = LINE('',#65498,#9039) ;
#6721 = LINE('',#65507,#9040) ;
#6722 = LINE('',#65508,#9041) ;
#6723 = LINE('',#65509,#9042) ;
#6724 = LINE('',#65510,#9043) ;
#6725 = LINE('',#65513,#9044) ;
#6726 = LINE('',#65515,#9045) ;
#6727 = LINE('',#65517,#9046) ;
#6728 = LINE('',#65530,#9047) ;
#6729 = LINE('',#65532,#9048) ;
#6730 = LINE('',#65533,#9049) ;
#6731 = LINE('',#65537,#9050) ;
#6732 = LINE('',#65540,#9051) ;
#6733 = LINE('',#65545,#9052) ;
#6734 = LINE('',#65550,#9053) ;
#6735 = LINE('',#65553,#9054) ;
#6736 = LINE('',#65556,#9055) ;
#6737 = LINE('',#65558,#9056) ;
#6738 = LINE('',#65559,#9057) ;
#6739 = LINE('',#65562,#9058) ;
#6740 = LINE('',#65563,#9059) ;
#6741 = LINE('',#65609,#9060) ;
#6742 = LINE('',#65622,#9061) ;
#6743 = LINE('',#65623,#9062) ;
#6744 = LINE('',#65626,#9063) ;
#6745 = LINE('',#65627,#9064) ;
#6746 = LINE('',#65628,#9065) ;
#6747 = LINE('',#65630,#9066) ;
#6748 = LINE('',#65632,#9067) ;
#6749 = LINE('',#65634,#9068) ;
#6750 = LINE('',#65637,#9069) ;
#6751 = LINE('',#65639,#9070) ;
#6752 = LINE('',#65641,#9071) ;
#6753 = LINE('',#65642,#9072) ;
#6754 = LINE('',#65644,#9073) ;
#6755 = LINE('',#65649,#9074) ;
#6756 = LINE('',#65653,#9075) ;
#6757 = LINE('',#65655,#9076) ;
#6758 = LINE('',#65656,#9077) ;
#6759 = LINE('',#65662,#9078) ;
#6760 = LINE('',#65670,#9079) ;
#6761 = LINE('',#65678,#9080) ;
#6762 = LINE('',#65681,#9081) ;
#6763 = LINE('',#65683,#9082) ;
#6764 = LINE('',#65684,#9083) ;
#6765 = LINE('',#65687,#9084) ;
#6766 = LINE('',#65691,#9085) ;
#6767 = LINE('',#65692,#9086) ;
#6768 = LINE('',#65695,#9087) ;
#6769 = LINE('',#65699,#9088) ;
#6770 = LINE('',#65700,#9089) ;
#6771 = LINE('',#65706,#9090) ;
#6772 = LINE('',#65714,#9091) ;
#6773 = LINE('',#65722,#9092) ;
#6774 = LINE('',#65725,#9093) ;
#6775 = LINE('',#65727,#9094) ;
#6776 = LINE('',#65728,#9095) ;
#6777 = LINE('',#65731,#9096) ;
#6778 = LINE('',#65735,#9097) ;
#6779 = LINE('',#65736,#9098) ;
#6780 = LINE('',#65739,#9099) ;
#6781 = LINE('',#65743,#9100) ;
#6782 = LINE('',#65744,#9101) ;
#6783 = LINE('',#65748,#9102) ;
#6784 = LINE('',#65750,#9103) ;
#6785 = LINE('',#65752,#9104) ;
#6786 = LINE('',#65753,#9105) ;
#6787 = LINE('',#65756,#9106) ;
#6788 = LINE('',#65758,#9107) ;
#6789 = LINE('',#65759,#9108) ;
#6790 = LINE('',#65762,#9109) ;
#6791 = LINE('',#65764,#9110) ;
#6792 = LINE('',#65765,#9111) ;
#6793 = LINE('',#65768,#9112) ;
#6794 = LINE('',#65770,#9113) ;
#6795 = LINE('',#65771,#9114) ;
#6796 = LINE('',#65774,#9115) ;
#6797 = LINE('',#65776,#9116) ;
#6798 = LINE('',#65777,#9117) ;
#6799 = LINE('',#65779,#9118) ;
#6800 = LINE('',#65780,#9119) ;
#6801 = LINE('',#65784,#9120) ;
#6802 = LINE('',#65786,#9121) ;
#6803 = LINE('',#65788,#9122) ;
#6804 = LINE('',#65789,#9123) ;
#6805 = LINE('',#65792,#9124) ;
#6806 = LINE('',#65794,#9125) ;
#6807 = LINE('',#65795,#9126) ;
#6808 = LINE('',#65798,#9127) ;
#6809 = LINE('',#65800,#9128) ;
#6810 = LINE('',#65801,#9129) ;
#6811 = LINE('',#65804,#9130) ;
#6812 = LINE('',#65806,#9131) ;
#6813 = LINE('',#65807,#9132) ;
#6814 = LINE('',#65810,#9133) ;
#6815 = LINE('',#65812,#9134) ;
#6816 = LINE('',#65813,#9135) ;
#6817 = LINE('',#65815,#9136) ;
#6818 = LINE('',#65816,#9137) ;
#6819 = LINE('',#65824,#9138) ;
#6820 = LINE('',#65830,#9139) ;
#6821 = LINE('',#65833,#9140) ;
#6822 = LINE('',#65840,#9141) ;
#6823 = LINE('',#65845,#9142) ;
#6824 = LINE('',#65849,#9143) ;
#6825 = LINE('',#65851,#9144) ;
#6826 = LINE('',#65852,#9145) ;
#6827 = LINE('',#65853,#9146) ;
#6828 = LINE('',#65857,#9147) ;
#6829 = LINE('',#65859,#9148) ;
#6830 = LINE('',#65863,#9149) ;
#6831 = LINE('',#65865,#9150) ;
#6832 = LINE('',#65869,#9151) ;
#6833 = LINE('',#65871,#9152) ;
#6834 = LINE('',#65874,#9153) ;
#6835 = LINE('',#65878,#9154) ;
#6836 = LINE('',#65884,#9155) ;
#6837 = LINE('',#65890,#9156) ;
#6838 = LINE('',#65897,#9157) ;
#6839 = LINE('',#65900,#9158) ;
#6840 = LINE('',#65906,#9159) ;
#6841 = LINE('',#65909,#9160) ;
#6842 = LINE('',#65915,#9161) ;
#6843 = LINE('',#65918,#9162) ;
#6844 = LINE('',#65924,#9163) ;
#6845 = LINE('',#65927,#9164) ;
#6846 = LINE('',#65933,#9165) ;
#6847 = LINE('',#65939,#9166) ;
#6848 = LINE('',#65942,#9167) ;
#6849 = LINE('',#65951,#9168) ;
#6850 = LINE('',#65953,#9169) ;
#6851 = LINE('',#65954,#9170) ;
#6852 = LINE('',#65956,#9171) ;
#6853 = LINE('',#65957,#9172) ;
#6854 = LINE('',#65959,#9173) ;
#6855 = LINE('',#65960,#9174) ;
#6856 = LINE('',#65963,#9175) ;
#6857 = LINE('',#65965,#9176) ;
#6858 = LINE('',#65966,#9177) ;
#6859 = LINE('',#65968,#9178) ;
#6860 = LINE('',#65970,#9179) ;
#6861 = LINE('',#65973,#9180) ;
#6862 = LINE('',#65974,#9181) ;
#6863 = LINE('',#65976,#9182) ;
#6864 = LINE('',#65978,#9183) ;
#6865 = LINE('',#65981,#9184) ;
#6866 = LINE('',#65982,#9185) ;
#6867 = LINE('',#65984,#9186) ;
#6868 = LINE('',#65986,#9187) ;
#6869 = LINE('',#65991,#9188) ;
#6870 = LINE('',#65992,#9189) ;
#6871 = LINE('',#65994,#9190) ;
#6872 = LINE('',#65996,#9191) ;
#6873 = LINE('',#65999,#9192) ;
#6874 = LINE('',#66001,#9193) ;
#6875 = LINE('',#66004,#9194) ;
#6876 = LINE('',#66006,#9195) ;
#6877 = LINE('',#66011,#9196) ;
#6878 = LINE('',#66014,#9197) ;
#6879 = LINE('',#66017,#9198) ;
#6880 = LINE('',#66019,#9199) ;
#6881 = LINE('',#66023,#9200) ;
#6882 = LINE('',#66028,#9201) ;
#6883 = LINE('',#66034,#9202) ;
#6884 = LINE('',#66036,#9203) ;
#6885 = LINE('',#66037,#9204) ;
#6886 = LINE('',#66039,#9205) ;
#6887 = LINE('',#66040,#9206) ;
#6888 = LINE('',#66042,#9207) ;
#6889 = LINE('',#66043,#9208) ;
#6890 = LINE('',#66045,#9209) ;
#6891 = LINE('',#66046,#9210) ;
#6892 = LINE('',#66050,#9211) ;
#6893 = LINE('',#66051,#9212) ;
#6894 = LINE('',#66053,#9213) ;
#6895 = LINE('',#66055,#9214) ;
#6896 = LINE('',#66056,#9215) ;
#6897 = LINE('',#66058,#9216) ;
#6898 = LINE('',#66060,#9217) ;
#6899 = LINE('',#66064,#9218) ;
#6900 = LINE('',#66068,#9219) ;
#6901 = LINE('',#66069,#9220) ;
#6902 = LINE('',#66082,#9221) ;
#6903 = LINE('',#66088,#9222) ;
#6904 = LINE('',#66093,#9223) ;
#6905 = LINE('',#66098,#9224) ;
#6906 = LINE('',#66103,#9225) ;
#6907 = LINE('',#66108,#9226) ;
#6908 = LINE('',#66113,#9227) ;
#6909 = LINE('',#66118,#9228) ;
#6910 = LINE('',#66123,#9229) ;
#6911 = LINE('',#66127,#9230) ;
#6912 = LINE('',#66128,#9231) ;
#6913 = LINE('',#66129,#9232) ;
#6914 = LINE('',#66135,#9233) ;
#6915 = LINE('',#66138,#9234) ;
#6916 = LINE('',#66139,#9235) ;
#6917 = LINE('',#66141,#9236) ;
#6918 = LINE('',#66142,#9237) ;
#6919 = LINE('',#66143,#9238) ;
#6920 = LINE('',#66145,#9239) ;
#6921 = LINE('',#66146,#9240) ;
#6922 = LINE('',#66148,#9241) ;
#6923 = LINE('',#66150,#9242) ;
#6924 = LINE('',#66154,#9243) ;
#6925 = LINE('',#66156,#9244) ;
#6926 = LINE('',#66157,#9245) ;
#6927 = LINE('',#66159,#9246) ;
#6928 = LINE('',#66160,#9247) ;
#6929 = LINE('',#66167,#9248) ;
#6930 = LINE('',#66168,#9249) ;
#6931 = LINE('',#66170,#9250) ;
#6932 = LINE('',#66172,#9251) ;
#6933 = LINE('',#66175,#9252) ;
#6934 = LINE('',#66176,#9253) ;
#6935 = LINE('',#66178,#9254) ;
#6936 = LINE('',#66180,#9255) ;
#6937 = LINE('',#66191,#9256) ;
#6938 = LINE('',#66194,#9257) ;
#6939 = LINE('',#66195,#9258) ;
#6940 = LINE('',#66199,#9259) ;
#6941 = LINE('',#66201,#9260) ;
#6942 = LINE('',#66202,#9261) ;
#6943 = LINE('',#66210,#9262) ;
#6944 = LINE('',#66211,#9263) ;
#6945 = LINE('',#66212,#9264) ;
#6946 = LINE('',#66217,#9265) ;
#6947 = LINE('',#66220,#9266) ;
#6948 = LINE('',#66959,#9267) ;
#6949 = LINE('',#66961,#9268) ;
#6950 = LINE('',#66962,#9269) ;
#6951 = LINE('',#66965,#9270) ;
#6952 = LINE('',#66967,#9271) ;
#6953 = LINE('',#66968,#9272) ;
#6954 = LINE('',#66971,#9273) ;
#6955 = LINE('',#66973,#9274) ;
#6956 = LINE('',#66974,#9275) ;
#6957 = LINE('',#66977,#9276) ;
#6958 = LINE('',#66979,#9277) ;
#6959 = LINE('',#66980,#9278) ;
#6960 = LINE('',#67009,#9279) ;
#6961 = LINE('',#67016,#9280) ;
#6962 = LINE('',#67020,#9281) ;
#6963 = LINE('',#67024,#9282) ;
#6964 = LINE('',#67028,#9283) ;
#6965 = LINE('',#67033,#9284) ;
#6966 = LINE('',#67060,#9285) ;
#6967 = LINE('',#67063,#9286) ;
#6968 = LINE('',#68692,#9287) ;
#6969 = LINE('',#68694,#9288) ;
#6970 = LINE('',#68696,#9289) ;
#6971 = LINE('',#68698,#9290) ;
#6972 = LINE('',#68700,#9291) ;
#6973 = LINE('',#68701,#9292) ;
#6974 = LINE('',#68704,#9293) ;
#6975 = LINE('',#68706,#9294) ;
#6976 = LINE('',#68708,#9295) ;
#6977 = LINE('',#68710,#9296) ;
#6978 = LINE('',#68712,#9297) ;
#6979 = LINE('',#68713,#9298) ;
#6980 = LINE('',#68716,#9299) ;
#6981 = LINE('',#68718,#9300) ;
#6982 = LINE('',#68720,#9301) ;
#6983 = LINE('',#68722,#9302) ;
#6984 = LINE('',#68724,#9303) ;
#6985 = LINE('',#68725,#9304) ;
#6986 = LINE('',#69263,#9305) ;
#6987 = LINE('',#69264,#9306) ;
#6988 = LINE('',#69265,#9307) ;
#6989 = LINE('',#69268,#9308) ;
#6990 = LINE('',#69269,#9309) ;
#6991 = LINE('',#69272,#9310) ;
#6992 = LINE('',#69273,#9311) ;
#6993 = LINE('',#69276,#9312) ;
#6994 = LINE('',#69277,#9313) ;
#6995 = LINE('',#69280,#9314) ;
#6996 = LINE('',#69281,#9315) ;
#6997 = LINE('',#69283,#9316) ;
#6998 = LINE('',#69287,#9317) ;
#6999 = LINE('',#69288,#9318) ;
#7000 = LINE('',#69289,#9319) ;
#7001 = LINE('',#69292,#9320) ;
#7002 = LINE('',#69293,#9321) ;
#7003 = LINE('',#69296,#9322) ;
#7004 = LINE('',#69297,#9323) ;
#7005 = LINE('',#69300,#9324) ;
#7006 = LINE('',#69301,#9325) ;
#7007 = LINE('',#69304,#9326) ;
#7008 = LINE('',#69305,#9327) ;
#7009 = LINE('',#69307,#9328) ;
#7010 = LINE('',#69311,#9329) ;
#7011 = LINE('',#69313,#9330) ;
#7012 = LINE('',#69315,#9331) ;
#7013 = LINE('',#69317,#9332) ;
#7014 = LINE('',#69319,#9333) ;
#7015 = LINE('',#69320,#9334) ;
#7016 = LINE('',#69322,#9335) ;
#7017 = LINE('',#69323,#9336) ;
#7018 = LINE('',#69325,#9337) ;
#7019 = LINE('',#69327,#9338) ;
#7020 = LINE('',#69329,#9339) ;
#7021 = LINE('',#69331,#9340) ;
#7022 = LINE('',#69343,#9341) ;
#7023 = LINE('',#69345,#9342) ;
#7024 = LINE('',#69347,#9343) ;
#7025 = LINE('',#69348,#9344) ;
#7026 = LINE('',#69351,#9345) ;
#7027 = LINE('',#69353,#9346) ;
#7028 = LINE('',#69354,#9347) ;
#7029 = LINE('',#69357,#9348) ;
#7030 = LINE('',#69359,#9349) ;
#7031 = LINE('',#69360,#9350) ;
#7032 = LINE('',#69362,#9351) ;
#7033 = LINE('',#69366,#9352) ;
#7034 = LINE('',#69368,#9353) ;
#7035 = LINE('',#69370,#9354) ;
#7036 = LINE('',#69371,#9355) ;
#7037 = LINE('',#69374,#9356) ;
#7038 = LINE('',#69376,#9357) ;
#7039 = LINE('',#69377,#9358) ;
#7040 = LINE('',#69380,#9359) ;
#7041 = LINE('',#69382,#9360) ;
#7042 = LINE('',#69383,#9361) ;
#7043 = LINE('',#69385,#9362) ;
#7044 = LINE('',#69389,#9363) ;
#7045 = LINE('',#69391,#9364) ;
#7046 = LINE('',#69393,#9365) ;
#7047 = LINE('',#69394,#9366) ;
#7048 = LINE('',#69397,#9367) ;
#7049 = LINE('',#69399,#9368) ;
#7050 = LINE('',#69400,#9369) ;
#7051 = LINE('',#69403,#9370) ;
#7052 = LINE('',#69405,#9371) ;
#7053 = LINE('',#69406,#9372) ;
#7054 = LINE('',#69408,#9373) ;
#7055 = LINE('',#69412,#9374) ;
#7056 = LINE('',#69414,#9375) ;
#7057 = LINE('',#69416,#9376) ;
#7058 = LINE('',#69417,#9377) ;
#7059 = LINE('',#69420,#9378) ;
#7060 = LINE('',#69422,#9379) ;
#7061 = LINE('',#69423,#9380) ;
#7062 = LINE('',#69426,#9381) ;
#7063 = LINE('',#69428,#9382) ;
#7064 = LINE('',#69429,#9383) ;
#7065 = LINE('',#69431,#9384) ;
#7066 = LINE('',#69435,#9385) ;
#7067 = LINE('',#69437,#9386) ;
#7068 = LINE('',#69439,#9387) ;
#7069 = LINE('',#69440,#9388) ;
#7070 = LINE('',#69443,#9389) ;
#7071 = LINE('',#69445,#9390) ;
#7072 = LINE('',#69446,#9391) ;
#7073 = LINE('',#69449,#9392) ;
#7074 = LINE('',#69451,#9393) ;
#7075 = LINE('',#69452,#9394) ;
#7076 = LINE('',#69454,#9395) ;
#7077 = LINE('',#69458,#9396) ;
#7078 = LINE('',#69460,#9397) ;
#7079 = LINE('',#69462,#9398) ;
#7080 = LINE('',#69463,#9399) ;
#7081 = LINE('',#69466,#9400) ;
#7082 = LINE('',#69468,#9401) ;
#7083 = LINE('',#69469,#9402) ;
#7084 = LINE('',#69472,#9403) ;
#7085 = LINE('',#69474,#9404) ;
#7086 = LINE('',#69475,#9405) ;
#7087 = LINE('',#69477,#9406) ;
#7088 = LINE('',#69481,#9407) ;
#7089 = LINE('',#69483,#9408) ;
#7090 = LINE('',#69485,#9409) ;
#7091 = LINE('',#69486,#9410) ;
#7092 = LINE('',#69489,#9411) ;
#7093 = LINE('',#69491,#9412) ;
#7094 = LINE('',#69492,#9413) ;
#7095 = LINE('',#69495,#9414) ;
#7096 = LINE('',#69497,#9415) ;
#7097 = LINE('',#69498,#9416) ;
#7098 = LINE('',#69500,#9417) ;
#7099 = LINE('',#69504,#9418) ;
#7100 = LINE('',#69506,#9419) ;
#7101 = LINE('',#69508,#9420) ;
#7102 = LINE('',#69509,#9421) ;
#7103 = LINE('',#69512,#9422) ;
#7104 = LINE('',#69514,#9423) ;
#7105 = LINE('',#69515,#9424) ;
#7106 = LINE('',#69518,#9425) ;
#7107 = LINE('',#69520,#9426) ;
#7108 = LINE('',#69521,#9427) ;
#7109 = LINE('',#69523,#9428) ;
#7110 = LINE('',#69527,#9429) ;
#7111 = LINE('',#69529,#9430) ;
#7112 = LINE('',#69531,#9431) ;
#7113 = LINE('',#69532,#9432) ;
#7114 = LINE('',#69535,#9433) ;
#7115 = LINE('',#69537,#9434) ;
#7116 = LINE('',#69538,#9435) ;
#7117 = LINE('',#69541,#9436) ;
#7118 = LINE('',#69543,#9437) ;
#7119 = LINE('',#69544,#9438) ;
#7120 = LINE('',#69546,#9439) ;
#7121 = LINE('',#69548,#9440) ;
#7122 = LINE('',#69549,#9441) ;
#7123 = LINE('',#69550,#9442) ;
#7124 = LINE('',#69551,#9443) ;
#7125 = LINE('',#69552,#9444) ;
#7126 = LINE('',#69553,#9445) ;
#7127 = LINE('',#69555,#9446) ;
#7128 = LINE('',#69557,#9447) ;
#7129 = LINE('',#69559,#9448) ;
#7130 = LINE('',#69561,#9449) ;
#7131 = LINE('',#69563,#9450) ;
#7132 = LINE('',#69565,#9451) ;
#7133 = LINE('',#69567,#9452) ;
#7134 = LINE('',#69569,#9453) ;
#7135 = LINE('',#69571,#9454) ;
#7136 = LINE('',#69573,#9455) ;
#7137 = LINE('',#69575,#9456) ;
#7138 = LINE('',#69577,#9457) ;
#7139 = LINE('',#69579,#9458) ;
#7140 = LINE('',#69581,#9459) ;
#7141 = LINE('',#69583,#9460) ;
#7142 = LINE('',#69585,#9461) ;
#7143 = LINE('',#69587,#9462) ;
#7144 = LINE('',#69589,#9463) ;
#7145 = LINE('',#69591,#9464) ;
#7146 = LINE('',#69593,#9465) ;
#7147 = LINE('',#69595,#9466) ;
#7148 = LINE('',#69597,#9467) ;
#7149 = LINE('',#69599,#9468) ;
#7150 = LINE('',#69601,#9469) ;
#7151 = LINE('',#69603,#9470) ;
#7152 = LINE('',#69605,#9471) ;
#7153 = LINE('',#69607,#9472) ;
#7154 = LINE('',#69609,#9473) ;
#7155 = LINE('',#69611,#9474) ;
#7156 = LINE('',#69613,#9475) ;
#7157 = LINE('',#69615,#9476) ;
#7158 = LINE('',#69617,#9477) ;
#7159 = LINE('',#69619,#9478) ;
#7160 = LINE('',#69621,#9479) ;
#7161 = LINE('',#69623,#9480) ;
#7162 = LINE('',#69625,#9481) ;
#7163 = LINE('',#69627,#9482) ;
#7164 = LINE('',#69629,#9483) ;
#7165 = LINE('',#69631,#9484) ;
#7166 = LINE('',#69633,#9485) ;
#7167 = LINE('',#69634,#9486) ;
#7168 = LINE('',#69635,#9487) ;
#7169 = LINE('',#69636,#9488) ;
#7170 = LINE('',#69646,#9489) ;
#7171 = LINE('',#69650,#9490) ;
#7172 = LINE('',#69652,#9491) ;
#7173 = LINE('',#69654,#9492) ;
#7174 = LINE('',#69655,#9493) ;
#7175 = LINE('',#69658,#9494) ;
#7176 = LINE('',#69662,#9495) ;
#7177 = LINE('',#69666,#9496) ;
#7178 = LINE('',#69670,#9497) ;
#7179 = LINE('',#69681,#9498) ;
#7180 = LINE('',#69685,#9499) ;
#7181 = LINE('',#69687,#9500) ;
#7182 = LINE('',#69689,#9501) ;
#7183 = LINE('',#69690,#9502) ;
#7184 = LINE('',#69693,#9503) ;
#7185 = LINE('',#69697,#9504) ;
#7186 = LINE('',#69701,#9505) ;
#7187 = LINE('',#69705,#9506) ;
#7188 = LINE('',#69716,#9507) ;
#7189 = LINE('',#69720,#9508) ;
#7190 = LINE('',#69722,#9509) ;
#7191 = LINE('',#69724,#9510) ;
#7192 = LINE('',#69725,#9511) ;
#7193 = LINE('',#69728,#9512) ;
#7194 = LINE('',#69732,#9513) ;
#7195 = LINE('',#69736,#9514) ;
#7196 = LINE('',#69740,#9515) ;
#7197 = LINE('',#69751,#9516) ;
#7198 = LINE('',#69755,#9517) ;
#7199 = LINE('',#69757,#9518) ;
#7200 = LINE('',#69759,#9519) ;
#7201 = LINE('',#69760,#9520) ;
#7202 = LINE('',#69763,#9521) ;
#7203 = LINE('',#69767,#9522) ;
#7204 = LINE('',#69771,#9523) ;
#7205 = LINE('',#69775,#9524) ;
#7206 = LINE('',#69786,#9525) ;
#7207 = LINE('',#69790,#9526) ;
#7208 = LINE('',#69792,#9527) ;
#7209 = LINE('',#69794,#9528) ;
#7210 = LINE('',#69795,#9529) ;
#7211 = LINE('',#69798,#9530) ;
#7212 = LINE('',#69802,#9531) ;
#7213 = LINE('',#69806,#9532) ;
#7214 = LINE('',#69810,#9533) ;
#7215 = LINE('',#69821,#9534) ;
#7216 = LINE('',#69825,#9535) ;
#7217 = LINE('',#69827,#9536) ;
#7218 = LINE('',#69829,#9537) ;
#7219 = LINE('',#69830,#9538) ;
#7220 = LINE('',#69833,#9539) ;
#7221 = LINE('',#69837,#9540) ;
#7222 = LINE('',#69841,#9541) ;
#7223 = LINE('',#69845,#9542) ;
#7224 = LINE('',#69856,#9543) ;
#7225 = LINE('',#69860,#9544) ;
#7226 = LINE('',#69862,#9545) ;
#7227 = LINE('',#69864,#9546) ;
#7228 = LINE('',#69865,#9547) ;
#7229 = LINE('',#69868,#9548) ;
#7230 = LINE('',#69872,#9549) ;
#7231 = LINE('',#69876,#9550) ;
#7232 = LINE('',#69880,#9551) ;
#7233 = LINE('',#69891,#9552) ;
#7234 = LINE('',#69895,#9553) ;
#7235 = LINE('',#69897,#9554) ;
#7236 = LINE('',#69899,#9555) ;
#7237 = LINE('',#69900,#9556) ;
#7238 = LINE('',#69903,#9557) ;
#7239 = LINE('',#69907,#9558) ;
#7240 = LINE('',#69911,#9559) ;
#7241 = LINE('',#69915,#9560) ;
#7242 = LINE('',#69926,#9561) ;
#7243 = LINE('',#69928,#9562) ;
#7244 = LINE('',#69930,#9563) ;
#7245 = LINE('',#69931,#9564) ;
#7246 = LINE('',#69934,#9565) ;
#7247 = LINE('',#69938,#9566) ;
#7248 = LINE('',#69942,#9567) ;
#7249 = LINE('',#69946,#9568) ;
#7250 = LINE('',#69951,#9569) ;
#7251 = LINE('',#69980,#9570) ;
#7252 = LINE('',#69989,#9571) ;
#7253 = LINE('',#69997,#9572) ;
#7254 = LINE('',#70005,#9573) ;
#7255 = LINE('',#70010,#9574) ;
#7256 = LINE('',#70013,#9575) ;
#7257 = LINE('',#70016,#9576) ;
#7258 = LINE('',#70020,#9577) ;
#7259 = LINE('',#70022,#9578) ;
#7260 = LINE('',#70024,#9579) ;
#7261 = LINE('',#70026,#9580) ;
#7262 = LINE('',#70028,#9581) ;
#7263 = LINE('',#70032,#9582) ;
#7264 = LINE('',#70036,#9583) ;
#7265 = LINE('',#70037,#9584) ;
#7266 = LINE('',#70042,#9585) ;
#7267 = LINE('',#70051,#9586) ;
#7268 = LINE('',#70059,#9587) ;
#7269 = LINE('',#70067,#9588) ;
#7270 = LINE('',#70072,#9589) ;
#7271 = LINE('',#70075,#9590) ;
#7272 = LINE('',#70078,#9591) ;
#7273 = LINE('',#70082,#9592) ;
#7274 = LINE('',#70084,#9593) ;
#7275 = LINE('',#70086,#9594) ;
#7276 = LINE('',#70088,#9595) ;
#7277 = LINE('',#70090,#9596) ;
#7278 = LINE('',#70094,#9597) ;
#7279 = LINE('',#70098,#9598) ;
#7280 = LINE('',#70099,#9599) ;
#7281 = LINE('',#70104,#9600) ;
#7282 = LINE('',#70113,#9601) ;
#7283 = LINE('',#70121,#9602) ;
#7284 = LINE('',#70129,#9603) ;
#7285 = LINE('',#70134,#9604) ;
#7286 = LINE('',#70137,#9605) ;
#7287 = LINE('',#70140,#9606) ;
#7288 = LINE('',#70144,#9607) ;
#7289 = LINE('',#70146,#9608) ;
#7290 = LINE('',#70148,#9609) ;
#7291 = LINE('',#70150,#9610) ;
#7292 = LINE('',#70152,#9611) ;
#7293 = LINE('',#70156,#9612) ;
#7294 = LINE('',#70160,#9613) ;
#7295 = LINE('',#70161,#9614) ;
#7296 = LINE('',#70166,#9615) ;
#7297 = LINE('',#70175,#9616) ;
#7298 = LINE('',#70183,#9617) ;
#7299 = LINE('',#70191,#9618) ;
#7300 = LINE('',#70196,#9619) ;
#7301 = LINE('',#70199,#9620) ;
#7302 = LINE('',#70202,#9621) ;
#7303 = LINE('',#70206,#9622) ;
#7304 = LINE('',#70208,#9623) ;
#7305 = LINE('',#70210,#9624) ;
#7306 = LINE('',#70212,#9625) ;
#7307 = LINE('',#70214,#9626) ;
#7308 = LINE('',#70218,#9627) ;
#7309 = LINE('',#70222,#9628) ;
#7310 = LINE('',#70223,#9629) ;
#7311 = LINE('',#70228,#9630) ;
#7312 = LINE('',#70237,#9631) ;
#7313 = LINE('',#70245,#9632) ;
#7314 = LINE('',#70253,#9633) ;
#7315 = LINE('',#70258,#9634) ;
#7316 = LINE('',#70261,#9635) ;
#7317 = LINE('',#70264,#9636) ;
#7318 = LINE('',#70268,#9637) ;
#7319 = LINE('',#70270,#9638) ;
#7320 = LINE('',#70272,#9639) ;
#7321 = LINE('',#70274,#9640) ;
#7322 = LINE('',#70276,#9641) ;
#7323 = LINE('',#70280,#9642) ;
#7324 = LINE('',#70284,#9643) ;
#7325 = LINE('',#70285,#9644) ;
#7326 = LINE('',#70290,#9645) ;
#7327 = LINE('',#70299,#9646) ;
#7328 = LINE('',#70307,#9647) ;
#7329 = LINE('',#70315,#9648) ;
#7330 = LINE('',#70320,#9649) ;
#7331 = LINE('',#70323,#9650) ;
#7332 = LINE('',#70326,#9651) ;
#7333 = LINE('',#70330,#9652) ;
#7334 = LINE('',#70332,#9653) ;
#7335 = LINE('',#70334,#9654) ;
#7336 = LINE('',#70336,#9655) ;
#7337 = LINE('',#70338,#9656) ;
#7338 = LINE('',#70342,#9657) ;
#7339 = LINE('',#70346,#9658) ;
#7340 = LINE('',#70347,#9659) ;
#7341 = LINE('',#70352,#9660) ;
#7342 = LINE('',#70361,#9661) ;
#7343 = LINE('',#70369,#9662) ;
#7344 = LINE('',#70377,#9663) ;
#7345 = LINE('',#70382,#9664) ;
#7346 = LINE('',#70385,#9665) ;
#7347 = LINE('',#70388,#9666) ;
#7348 = LINE('',#70392,#9667) ;
#7349 = LINE('',#70394,#9668) ;
#7350 = LINE('',#70396,#9669) ;
#7351 = LINE('',#70398,#9670) ;
#7352 = LINE('',#70400,#9671) ;
#7353 = LINE('',#70404,#9672) ;
#7354 = LINE('',#70408,#9673) ;
#7355 = LINE('',#70409,#9674) ;
#7356 = LINE('',#70414,#9675) ;
#7357 = LINE('',#70423,#9676) ;
#7358 = LINE('',#70431,#9677) ;
#7359 = LINE('',#70439,#9678) ;
#7360 = LINE('',#70444,#9679) ;
#7361 = LINE('',#70447,#9680) ;
#7362 = LINE('',#70450,#9681) ;
#7363 = LINE('',#70454,#9682) ;
#7364 = LINE('',#70456,#9683) ;
#7365 = LINE('',#70458,#9684) ;
#7366 = LINE('',#70460,#9685) ;
#7367 = LINE('',#70462,#9686) ;
#7368 = LINE('',#70466,#9687) ;
#7369 = LINE('',#70470,#9688) ;
#7370 = LINE('',#70471,#9689) ;
#7371 = LINE('',#70476,#9690) ;
#7372 = LINE('',#70485,#9691) ;
#7373 = LINE('',#70493,#9692) ;
#7374 = LINE('',#70501,#9693) ;
#7375 = LINE('',#70506,#9694) ;
#7376 = LINE('',#70509,#9695) ;
#7377 = LINE('',#70513,#9696) ;
#7378 = LINE('',#70515,#9697) ;
#7379 = LINE('',#70517,#9698) ;
#7380 = LINE('',#70520,#9699) ;
#7381 = LINE('',#70524,#9700) ;
#7382 = LINE('',#70525,#9701) ;
#7383 = LINE('',#70528,#9702) ;
#7384 = LINE('',#70532,#9703) ;
#7385 = LINE('',#70533,#9704) ;
#7386 = LINE('',#70539,#9705) ;
#7387 = LINE('',#70542,#9706) ;
#7388 = LINE('',#70553,#9707) ;
#7389 = LINE('',#70554,#9708) ;
#7390 = LINE('',#70565,#9709) ;
#7391 = LINE('',#70566,#9710) ;
#7392 = LINE('',#70577,#9711) ;
#7393 = LINE('',#70578,#9712) ;
#7394 = LINE('',#70584,#9713) ;
#7395 = LINE('',#70587,#9714) ;
#7396 = LINE('',#70590,#9715) ;
#7397 = LINE('',#70591,#9716) ;
#7398 = LINE('',#70594,#9717) ;
#7399 = LINE('',#70598,#9718) ;
#7400 = LINE('',#70599,#9719) ;
#7401 = LINE('',#70605,#9720) ;
#7402 = LINE('',#70608,#9721) ;
#7403 = LINE('',#70619,#9722) ;
#7404 = LINE('',#70620,#9723) ;
#7405 = LINE('',#70631,#9724) ;
#7406 = LINE('',#70632,#9725) ;
#7407 = LINE('',#70643,#9726) ;
#7408 = LINE('',#70644,#9727) ;
#7409 = LINE('',#70650,#9728) ;
#7410 = LINE('',#70653,#9729) ;
#7411 = LINE('',#70656,#9730) ;
#7412 = LINE('',#70657,#9731) ;
#7413 = LINE('',#70660,#9732) ;
#7414 = LINE('',#70664,#9733) ;
#7415 = LINE('',#70665,#9734) ;
#7416 = LINE('',#70671,#9735) ;
#7417 = LINE('',#70674,#9736) ;
#7418 = LINE('',#70685,#9737) ;
#7419 = LINE('',#70686,#9738) ;
#7420 = LINE('',#70697,#9739) ;
#7421 = LINE('',#70698,#9740) ;
#7422 = LINE('',#70709,#9741) ;
#7423 = LINE('',#70710,#9742) ;
#7424 = LINE('',#70716,#9743) ;
#7425 = LINE('',#70719,#9744) ;
#7426 = LINE('',#70722,#9745) ;
#7427 = LINE('',#70723,#9746) ;
#7428 = LINE('',#70726,#9747) ;
#7429 = LINE('',#70730,#9748) ;
#7430 = LINE('',#70731,#9749) ;
#7431 = LINE('',#70737,#9750) ;
#7432 = LINE('',#70740,#9751) ;
#7433 = LINE('',#70751,#9752) ;
#7434 = LINE('',#70752,#9753) ;
#7435 = LINE('',#70763,#9754) ;
#7436 = LINE('',#70764,#9755) ;
#7437 = LINE('',#70775,#9756) ;
#7438 = LINE('',#70776,#9757) ;
#7439 = LINE('',#70782,#9758) ;
#7440 = LINE('',#70785,#9759) ;
#7441 = LINE('',#70788,#9760) ;
#7442 = LINE('',#70789,#9761) ;
#7443 = LINE('',#70792,#9762) ;
#7444 = LINE('',#70796,#9763) ;
#7445 = LINE('',#70797,#9764) ;
#7446 = LINE('',#70803,#9765) ;
#7447 = LINE('',#70806,#9766) ;
#7448 = LINE('',#70817,#9767) ;
#7449 = LINE('',#70818,#9768) ;
#7450 = LINE('',#70829,#9769) ;
#7451 = LINE('',#70830,#9770) ;
#7452 = LINE('',#70841,#9771) ;
#7453 = LINE('',#70842,#9772) ;
#7454 = LINE('',#70848,#9773) ;
#7455 = LINE('',#70851,#9774) ;
#7456 = LINE('',#70854,#9775) ;
#7457 = LINE('',#70855,#9776) ;
#7458 = LINE('',#70858,#9777) ;
#7459 = LINE('',#70862,#9778) ;
#7460 = LINE('',#70863,#9779) ;
#7461 = LINE('',#70869,#9780) ;
#7462 = LINE('',#70872,#9781) ;
#7463 = LINE('',#70883,#9782) ;
#7464 = LINE('',#70884,#9783) ;
#7465 = LINE('',#70895,#9784) ;
#7466 = LINE('',#70896,#9785) ;
#7467 = LINE('',#70907,#9786) ;
#7468 = LINE('',#70908,#9787) ;
#7469 = LINE('',#70914,#9788) ;
#7470 = LINE('',#70917,#9789) ;
#7471 = LINE('',#70920,#9790) ;
#7472 = LINE('',#70921,#9791) ;
#7473 = LINE('',#70924,#9792) ;
#7474 = LINE('',#70928,#9793) ;
#7475 = LINE('',#70929,#9794) ;
#7476 = LINE('',#70935,#9795) ;
#7477 = LINE('',#70938,#9796) ;
#7478 = LINE('',#70949,#9797) ;
#7479 = LINE('',#70950,#9798) ;
#7480 = LINE('',#70961,#9799) ;
#7481 = LINE('',#70962,#9800) ;
#7482 = LINE('',#70973,#9801) ;
#7483 = LINE('',#70974,#9802) ;
#7484 = LINE('',#70980,#9803) ;
#7485 = LINE('',#70983,#9804) ;
#7486 = LINE('',#70986,#9805) ;
#7487 = LINE('',#70987,#9806) ;
#7488 = LINE('',#70990,#9807) ;
#7489 = LINE('',#70994,#9808) ;
#7490 = LINE('',#70995,#9809) ;
#7491 = LINE('',#71001,#9810) ;
#7492 = LINE('',#71004,#9811) ;
#7493 = LINE('',#71015,#9812) ;
#7494 = LINE('',#71016,#9813) ;
#7495 = LINE('',#71027,#9814) ;
#7496 = LINE('',#71028,#9815) ;
#7497 = LINE('',#71039,#9816) ;
#7498 = LINE('',#71040,#9817) ;
#7499 = LINE('',#71046,#9818) ;
#7500 = LINE('',#71049,#9819) ;
#7501 = LINE('',#71052,#9820) ;
#7502 = LINE('',#71053,#9821) ;
#7503 = LINE('',#71056,#9822) ;
#7504 = LINE('',#71060,#9823) ;
#7505 = LINE('',#71061,#9824) ;
#7506 = LINE('',#71067,#9825) ;
#7507 = LINE('',#71070,#9826) ;
#7508 = LINE('',#71081,#9827) ;
#7509 = LINE('',#71082,#9828) ;
#7510 = LINE('',#71093,#9829) ;
#7511 = LINE('',#71094,#9830) ;
#7512 = LINE('',#71103,#9831) ;
#7513 = LINE('',#71109,#9832) ;
#7514 = LINE('',#71112,#9833) ;
#7515 = LINE('',#71115,#9834) ;
#7516 = LINE('',#71118,#9835) ;
#7517 = LINE('',#71120,#9836) ;
#7518 = LINE('',#71122,#9837) ;
#7519 = LINE('',#71125,#9838) ;
#7520 = LINE('',#71128,#9839) ;
#7521 = LINE('',#71132,#9840) ;
#7522 = LINE('',#71133,#9841) ;
#7523 = LINE('',#71139,#9842) ;
#7524 = LINE('',#71142,#9843) ;
#7525 = LINE('',#71153,#9844) ;
#7526 = LINE('',#71154,#9845) ;
#7527 = LINE('',#71165,#9846) ;
#7528 = LINE('',#71166,#9847) ;
#7529 = LINE('',#71175,#9848) ;
#7530 = LINE('',#71181,#9849) ;
#7531 = LINE('',#71184,#9850) ;
#7532 = LINE('',#71187,#9851) ;
#7533 = LINE('',#71190,#9852) ;
#7534 = LINE('',#71192,#9853) ;
#7535 = LINE('',#71194,#9854) ;
#7536 = LINE('',#71197,#9855) ;
#7537 = LINE('',#71200,#9856) ;
#7538 = LINE('',#71204,#9857) ;
#7539 = LINE('',#71205,#9858) ;
#7540 = LINE('',#71211,#9859) ;
#7541 = LINE('',#71214,#9860) ;
#7542 = LINE('',#71225,#9861) ;
#7543 = LINE('',#71226,#9862) ;
#7544 = LINE('',#71237,#9863) ;
#7545 = LINE('',#71238,#9864) ;
#7546 = LINE('',#71247,#9865) ;
#7547 = LINE('',#71253,#9866) ;
#7548 = LINE('',#71256,#9867) ;
#7549 = LINE('',#71259,#9868) ;
#7550 = LINE('',#71262,#9869) ;
#7551 = LINE('',#71264,#9870) ;
#7552 = LINE('',#71266,#9871) ;
#7553 = LINE('',#71269,#9872) ;
#7554 = LINE('',#71272,#9873) ;
#7555 = LINE('',#71276,#9874) ;
#7556 = LINE('',#71277,#9875) ;
#7557 = LINE('',#71283,#9876) ;
#7558 = LINE('',#71286,#9877) ;
#7559 = LINE('',#71297,#9878) ;
#7560 = LINE('',#71298,#9879) ;
#7561 = LINE('',#71309,#9880) ;
#7562 = LINE('',#71310,#9881) ;
#7563 = LINE('',#71319,#9882) ;
#7564 = LINE('',#71325,#9883) ;
#7565 = LINE('',#71328,#9884) ;
#7566 = LINE('',#71331,#9885) ;
#7567 = LINE('',#71334,#9886) ;
#7568 = LINE('',#71336,#9887) ;
#7569 = LINE('',#71338,#9888) ;
#7570 = LINE('',#71341,#9889) ;
#7571 = LINE('',#71344,#9890) ;
#7572 = LINE('',#71348,#9891) ;
#7573 = LINE('',#71349,#9892) ;
#7574 = LINE('',#71355,#9893) ;
#7575 = LINE('',#71358,#9894) ;
#7576 = LINE('',#71369,#9895) ;
#7577 = LINE('',#71370,#9896) ;
#7578 = LINE('',#71381,#9897) ;
#7579 = LINE('',#71382,#9898) ;
#7580 = LINE('',#71391,#9899) ;
#7581 = LINE('',#71397,#9900) ;
#7582 = LINE('',#71400,#9901) ;
#7583 = LINE('',#71403,#9902) ;
#7584 = LINE('',#71406,#9903) ;
#7585 = LINE('',#71408,#9904) ;
#7586 = LINE('',#71410,#9905) ;
#7587 = LINE('',#71413,#9906) ;
#7588 = LINE('',#71416,#9907) ;
#7589 = LINE('',#71420,#9908) ;
#7590 = LINE('',#71421,#9909) ;
#7591 = LINE('',#71427,#9910) ;
#7592 = LINE('',#71430,#9911) ;
#7593 = LINE('',#71441,#9912) ;
#7594 = LINE('',#71442,#9913) ;
#7595 = LINE('',#71453,#9914) ;
#7596 = LINE('',#71454,#9915) ;
#7597 = LINE('',#71463,#9916) ;
#7598 = LINE('',#71469,#9917) ;
#7599 = LINE('',#71472,#9918) ;
#7600 = LINE('',#71475,#9919) ;
#7601 = LINE('',#71478,#9920) ;
#7602 = LINE('',#71480,#9921) ;
#7603 = LINE('',#71482,#9922) ;
#7604 = LINE('',#71485,#9923) ;
#7605 = LINE('',#71488,#9924) ;
#7606 = LINE('',#71492,#9925) ;
#7607 = LINE('',#71493,#9926) ;
#7608 = LINE('',#71499,#9927) ;
#7609 = LINE('',#71502,#9928) ;
#7610 = LINE('',#71513,#9929) ;
#7611 = LINE('',#71514,#9930) ;
#7612 = LINE('',#71525,#9931) ;
#7613 = LINE('',#71526,#9932) ;
#7614 = LINE('',#71535,#9933) ;
#7615 = LINE('',#71541,#9934) ;
#7616 = LINE('',#71544,#9935) ;
#7617 = LINE('',#71547,#9936) ;
#7618 = LINE('',#71550,#9937) ;
#7619 = LINE('',#71552,#9938) ;
#7620 = LINE('',#71554,#9939) ;
#7621 = LINE('',#71557,#9940) ;
#7622 = LINE('',#71560,#9941) ;
#7623 = LINE('',#71564,#9942) ;
#7624 = LINE('',#71565,#9943) ;
#7625 = LINE('',#71571,#9944) ;
#7626 = LINE('',#71574,#9945) ;
#7627 = LINE('',#71585,#9946) ;
#7628 = LINE('',#71586,#9947) ;
#7629 = LINE('',#71597,#9948) ;
#7630 = LINE('',#71598,#9949) ;
#7631 = LINE('',#71607,#9950) ;
#7632 = LINE('',#71613,#9951) ;
#7633 = LINE('',#71616,#9952) ;
#7634 = LINE('',#71619,#9953) ;
#7635 = LINE('',#71622,#9954) ;
#7636 = LINE('',#71624,#9955) ;
#7637 = LINE('',#71626,#9956) ;
#7638 = LINE('',#71629,#9957) ;
#7639 = LINE('',#71632,#9958) ;
#7640 = LINE('',#71636,#9959) ;
#7641 = LINE('',#71637,#9960) ;
#7642 = LINE('',#71643,#9961) ;
#7643 = LINE('',#71646,#9962) ;
#7644 = LINE('',#71657,#9963) ;
#7645 = LINE('',#71658,#9964) ;
#7646 = LINE('',#71669,#9965) ;
#7647 = LINE('',#71670,#9966) ;
#7648 = LINE('',#71681,#9967) ;
#7649 = LINE('',#71682,#9968) ;
#7650 = LINE('',#71688,#9969) ;
#7651 = LINE('',#71691,#9970) ;
#7652 = LINE('',#71694,#9971) ;
#7653 = LINE('',#71695,#9972) ;
#7654 = LINE('',#71698,#9973) ;
#7655 = LINE('',#71702,#9974) ;
#7656 = LINE('',#71703,#9975) ;
#7657 = LINE('',#71707,#9976) ;
#7658 = LINE('',#71709,#9977) ;
#7659 = LINE('',#71711,#9978) ;
#7660 = LINE('',#71712,#9979) ;
#7661 = LINE('',#71715,#9980) ;
#7662 = LINE('',#71719,#9981) ;
#7663 = LINE('',#71723,#9982) ;
#7664 = LINE('',#71727,#9983) ;
#7665 = LINE('',#71735,#9984) ;
#7666 = LINE('',#71744,#9985) ;
#7667 = LINE('',#71752,#9986) ;
#7668 = LINE('',#71762,#9987) ;
#7669 = LINE('',#71765,#9988) ;
#7670 = LINE('',#71768,#9989) ;
#7671 = LINE('',#71770,#9990) ;
#7672 = LINE('',#71773,#9991) ;
#7673 = LINE('',#71775,#9992) ;
#7674 = LINE('',#71778,#9993) ;
#7675 = LINE('',#71781,#9994) ;
#7676 = LINE('',#71785,#9995) ;
#7677 = LINE('',#71786,#9996) ;
#7678 = LINE('',#71789,#9997) ;
#7679 = LINE('',#71790,#9998) ;
#7680 = LINE('',#71797,#9999) ;
#7681 = LINE('',#71798,#10000) ;
#7682 = LINE('',#71802,#10001) ;
#7683 = LINE('',#71805,#10002) ;
#7684 = LINE('',#71808,#10003) ;
#7685 = LINE('',#71819,#10004) ;
#7686 = LINE('',#71827,#10005) ;
#7687 = LINE('',#71839,#10006) ;
#7688 = LINE('',#71842,#10007) ;
#7689 = LINE('',#71849,#10008) ;
#7690 = LINE('',#71851,#10009) ;
#7691 = LINE('',#71852,#10010) ;
#7692 = LINE('',#71856,#10011) ;
#7693 = LINE('',#71858,#10012) ;
#7694 = LINE('',#71863,#10013) ;
#7695 = LINE('',#71873,#10014) ;
#7696 = LINE('',#71875,#10015) ;
#7697 = LINE('',#71877,#10016) ;
#7698 = LINE('',#71878,#10017) ;
#7699 = LINE('',#71901,#10018) ;
#7700 = LINE('',#71904,#10019) ;
#7701 = LINE('',#71912,#10020) ;
#7702 = LINE('',#71924,#10021) ;
#7703 = LINE('',#71927,#10022) ;
#7704 = LINE('',#71934,#10023) ;
#7705 = LINE('',#71936,#10024) ;
#7706 = LINE('',#71937,#10025) ;
#7707 = LINE('',#71941,#10026) ;
#7708 = LINE('',#71943,#10027) ;
#7709 = LINE('',#71949,#10028) ;
#7710 = LINE('',#71960,#10029) ;
#7711 = LINE('',#71962,#10030) ;
#7712 = LINE('',#71964,#10031) ;
#7713 = LINE('',#71965,#10032) ;
#7714 = LINE('',#71978,#10033) ;
#7715 = LINE('',#71982,#10034) ;
#7716 = LINE('',#71995,#10035) ;
#7717 = LINE('',#71998,#10036) ;
#7718 = LINE('',#72006,#10037) ;
#7719 = LINE('',#72018,#10038) ;
#7720 = LINE('',#72021,#10039) ;
#7721 = LINE('',#72028,#10040) ;
#7722 = LINE('',#72030,#10041) ;
#7723 = LINE('',#72031,#10042) ;
#7724 = LINE('',#72035,#10043) ;
#7725 = LINE('',#72037,#10044) ;
#7726 = LINE('',#72043,#10045) ;
#7727 = LINE('',#72054,#10046) ;
#7728 = LINE('',#72056,#10047) ;
#7729 = LINE('',#72058,#10048) ;
#7730 = LINE('',#72059,#10049) ;
#7731 = LINE('',#72072,#10050) ;
#7732 = LINE('',#72076,#10051) ;
#7733 = LINE('',#72089,#10052) ;
#7734 = LINE('',#72092,#10053) ;
#7735 = LINE('',#72100,#10054) ;
#7736 = LINE('',#72112,#10055) ;
#7737 = LINE('',#72115,#10056) ;
#7738 = LINE('',#72122,#10057) ;
#7739 = LINE('',#72124,#10058) ;
#7740 = LINE('',#72125,#10059) ;
#7741 = LINE('',#72129,#10060) ;
#7742 = LINE('',#72131,#10061) ;
#7743 = LINE('',#72137,#10062) ;
#7744 = LINE('',#72148,#10063) ;
#7745 = LINE('',#72150,#10064) ;
#7746 = LINE('',#72152,#10065) ;
#7747 = LINE('',#72153,#10066) ;
#7748 = LINE('',#72166,#10067) ;
#7749 = LINE('',#72170,#10068) ;
#7750 = LINE('',#72183,#10069) ;
#7751 = LINE('',#72186,#10070) ;
#7752 = LINE('',#72194,#10071) ;
#7753 = LINE('',#72206,#10072) ;
#7754 = LINE('',#72209,#10073) ;
#7755 = LINE('',#72216,#10074) ;
#7756 = LINE('',#72218,#10075) ;
#7757 = LINE('',#72219,#10076) ;
#7758 = LINE('',#72223,#10077) ;
#7759 = LINE('',#72225,#10078) ;
#7760 = LINE('',#72231,#10079) ;
#7761 = LINE('',#72242,#10080) ;
#7762 = LINE('',#72244,#10081) ;
#7763 = LINE('',#72246,#10082) ;
#7764 = LINE('',#72247,#10083) ;
#7765 = LINE('',#72260,#10084) ;
#7766 = LINE('',#72264,#10085) ;
#7767 = LINE('',#72277,#10086) ;
#7768 = LINE('',#72280,#10087) ;
#7769 = LINE('',#72288,#10088) ;
#7770 = LINE('',#72300,#10089) ;
#7771 = LINE('',#72303,#10090) ;
#7772 = LINE('',#72310,#10091) ;
#7773 = LINE('',#72312,#10092) ;
#7774 = LINE('',#72313,#10093) ;
#7775 = LINE('',#72317,#10094) ;
#7776 = LINE('',#72319,#10095) ;
#7777 = LINE('',#72325,#10096) ;
#7778 = LINE('',#72336,#10097) ;
#7779 = LINE('',#72338,#10098) ;
#7780 = LINE('',#72340,#10099) ;
#7781 = LINE('',#72341,#10100) ;
#7782 = LINE('',#72354,#10101) ;
#7783 = LINE('',#72358,#10102) ;
#7784 = LINE('',#72371,#10103) ;
#7785 = LINE('',#72374,#10104) ;
#7786 = LINE('',#72382,#10105) ;
#7787 = LINE('',#72394,#10106) ;
#7788 = LINE('',#72397,#10107) ;
#7789 = LINE('',#72404,#10108) ;
#7790 = LINE('',#72406,#10109) ;
#7791 = LINE('',#72407,#10110) ;
#7792 = LINE('',#72411,#10111) ;
#7793 = LINE('',#72413,#10112) ;
#7794 = LINE('',#72419,#10113) ;
#7795 = LINE('',#72430,#10114) ;
#7796 = LINE('',#72432,#10115) ;
#7797 = LINE('',#72434,#10116) ;
#7798 = LINE('',#72435,#10117) ;
#7799 = LINE('',#72448,#10118) ;
#7800 = LINE('',#72452,#10119) ;
#7801 = LINE('',#72465,#10120) ;
#7802 = LINE('',#72468,#10121) ;
#7803 = LINE('',#72476,#10122) ;
#7804 = LINE('',#72488,#10123) ;
#7805 = LINE('',#72491,#10124) ;
#7806 = LINE('',#72498,#10125) ;
#7807 = LINE('',#72500,#10126) ;
#7808 = LINE('',#72501,#10127) ;
#7809 = LINE('',#72505,#10128) ;
#7810 = LINE('',#72507,#10129) ;
#7811 = LINE('',#72513,#10130) ;
#7812 = LINE('',#72524,#10131) ;
#7813 = LINE('',#72526,#10132) ;
#7814 = LINE('',#72528,#10133) ;
#7815 = LINE('',#72529,#10134) ;
#7816 = LINE('',#72542,#10135) ;
#7817 = LINE('',#72546,#10136) ;
#7818 = LINE('',#72559,#10137) ;
#7819 = LINE('',#72562,#10138) ;
#7820 = LINE('',#72570,#10139) ;
#7821 = LINE('',#72582,#10140) ;
#7822 = LINE('',#72585,#10141) ;
#7823 = LINE('',#72592,#10142) ;
#7824 = LINE('',#72594,#10143) ;
#7825 = LINE('',#72595,#10144) ;
#7826 = LINE('',#72599,#10145) ;
#7827 = LINE('',#72601,#10146) ;
#7828 = LINE('',#72607,#10147) ;
#7829 = LINE('',#72618,#10148) ;
#7830 = LINE('',#72620,#10149) ;
#7831 = LINE('',#72622,#10150) ;
#7832 = LINE('',#72623,#10151) ;
#7833 = LINE('',#72636,#10152) ;
#7834 = LINE('',#72640,#10153) ;
#7835 = LINE('',#72648,#10154) ;
#7836 = LINE('',#72649,#10155) ;
#7837 = LINE('',#72651,#10156) ;
#7838 = LINE('',#72652,#10157) ;
#7839 = LINE('',#72654,#10158) ;
#7840 = LINE('',#72655,#10159) ;
#7841 = LINE('',#72657,#10160) ;
#7842 = LINE('',#72658,#10161) ;
#7843 = LINE('',#72660,#10162) ;
#7844 = LINE('',#72661,#10163) ;
#7845 = LINE('',#72663,#10164) ;
#7846 = LINE('',#72664,#10165) ;
#7847 = LINE('',#72666,#10166) ;
#7848 = LINE('',#72667,#10167) ;
#7849 = LINE('',#72669,#10168) ;
#7850 = LINE('',#72670,#10169) ;
#7851 = LINE('',#72672,#10170) ;
#7852 = LINE('',#72673,#10171) ;
#7853 = LINE('',#72675,#10172) ;
#7854 = LINE('',#72677,#10173) ;
#7855 = LINE('',#72679,#10174) ;
#7856 = LINE('',#72681,#10175) ;
#7857 = LINE('',#72683,#10176) ;
#7858 = LINE('',#72685,#10177) ;
#7859 = LINE('',#72687,#10178) ;
#7860 = LINE('',#72689,#10179) ;
#7861 = LINE('',#72691,#10180) ;
#7862 = LINE('',#72693,#10181) ;
#7863 = LINE('',#72695,#10182) ;
#7864 = LINE('',#72697,#10183) ;
#7865 = LINE('',#72699,#10184) ;
#7866 = LINE('',#72701,#10185) ;
#7867 = LINE('',#72703,#10186) ;
#7868 = LINE('',#72705,#10187) ;
#7869 = LINE('',#72707,#10188) ;
#7870 = LINE('',#72709,#10189) ;
#7871 = LINE('',#72713,#10190) ;
#7872 = LINE('',#72715,#10191) ;
#7873 = LINE('',#72717,#10192) ;
#7874 = LINE('',#72719,#10193) ;
#7875 = LINE('',#72721,#10194) ;
#7876 = LINE('',#72723,#10195) ;
#7877 = LINE('',#72725,#10196) ;
#7878 = LINE('',#72727,#10197) ;
#7879 = LINE('',#72729,#10198) ;
#7880 = LINE('',#72731,#10199) ;
#7881 = LINE('',#72733,#10200) ;
#7882 = LINE('',#72735,#10201) ;
#7883 = LINE('',#72737,#10202) ;
#7884 = LINE('',#72739,#10203) ;
#7885 = LINE('',#72741,#10204) ;
#7886 = LINE('',#72743,#10205) ;
#7887 = LINE('',#72745,#10206) ;
#7888 = LINE('',#72747,#10207) ;
#7889 = LINE('',#72749,#10208) ;
#7890 = LINE('',#72751,#10209) ;
#7891 = LINE('',#72753,#10210) ;
#7892 = LINE('',#72755,#10211) ;
#7893 = LINE('',#72757,#10212) ;
#7894 = LINE('',#72759,#10213) ;
#7895 = LINE('',#72761,#10214) ;
#7896 = LINE('',#72763,#10215) ;
#7897 = LINE('',#72765,#10216) ;
#7898 = LINE('',#72767,#10217) ;
#7899 = LINE('',#72769,#10218) ;
#7900 = LINE('',#72771,#10219) ;
#7901 = LINE('',#72773,#10220) ;
#7902 = LINE('',#72775,#10221) ;
#7903 = LINE('',#72777,#10222) ;
#7904 = LINE('',#72779,#10223) ;
#7905 = LINE('',#72781,#10224) ;
#7906 = LINE('',#72783,#10225) ;
#7907 = LINE('',#72785,#10226) ;
#7908 = LINE('',#72787,#10227) ;
#7909 = LINE('',#72789,#10228) ;
#7910 = LINE('',#72790,#10229) ;
#7911 = LINE('',#72795,#10230) ;
#7912 = LINE('',#72798,#10231) ;
#7913 = LINE('',#72800,#10232) ;
#7914 = LINE('',#72801,#10233) ;
#7915 = LINE('',#72805,#10234) ;
#7916 = LINE('',#72812,#10235) ;
#7917 = LINE('',#72818,#10236) ;
#7918 = LINE('',#72823,#10237) ;
#7919 = LINE('',#72829,#10238) ;
#7920 = LINE('',#72835,#10239) ;
#7921 = LINE('',#72842,#10240) ;
#7922 = LINE('',#72847,#10241) ;
#7923 = LINE('',#72854,#10242) ;
#7924 = LINE('',#72855,#10243) ;
#7925 = LINE('',#72856,#10244) ;
#7926 = LINE('',#72859,#10245) ;
#7927 = LINE('',#72862,#10246) ;
#7928 = LINE('',#72866,#10247) ;
#7929 = LINE('',#72868,#10248) ;
#7930 = LINE('',#72870,#10249) ;
#7931 = LINE('',#72871,#10250) ;
#7932 = LINE('',#72875,#10251) ;
#7933 = LINE('',#72877,#10252) ;
#7934 = LINE('',#72879,#10253) ;
#7935 = LINE('',#72880,#10254) ;
#7936 = LINE('',#72884,#10255) ;
#7937 = LINE('',#72886,#10256) ;
#7938 = LINE('',#72888,#10257) ;
#7939 = LINE('',#72889,#10258) ;
#7940 = LINE('',#72893,#10259) ;
#7941 = LINE('',#72895,#10260) ;
#7942 = LINE('',#72897,#10261) ;
#7943 = LINE('',#72898,#10262) ;
#7944 = LINE('',#72902,#10263) ;
#7945 = LINE('',#72904,#10264) ;
#7946 = LINE('',#72906,#10265) ;
#7947 = LINE('',#72907,#10266) ;
#7948 = LINE('',#72911,#10267) ;
#7949 = LINE('',#72913,#10268) ;
#7950 = LINE('',#72915,#10269) ;
#7951 = LINE('',#72916,#10270) ;
#7952 = LINE('',#72920,#10271) ;
#7953 = LINE('',#72922,#10272) ;
#7954 = LINE('',#72924,#10273) ;
#7955 = LINE('',#72925,#10274) ;
#7956 = LINE('',#72929,#10275) ;
#7957 = LINE('',#72931,#10276) ;
#7958 = LINE('',#72933,#10277) ;
#7959 = LINE('',#72934,#10278) ;
#7960 = LINE('',#72936,#10279) ;
#7961 = LINE('',#72937,#10280) ;
#7962 = LINE('',#72939,#10281) ;
#7963 = LINE('',#72941,#10282) ;
#7964 = LINE('',#72942,#10283) ;
#7965 = LINE('',#72945,#10284) ;
#7966 = LINE('',#72946,#10285) ;
#7967 = LINE('',#72947,#10286) ;
#7968 = LINE('',#72949,#10287) ;
#7969 = LINE('',#72951,#10288) ;
#7970 = LINE('',#72952,#10289) ;
#7971 = LINE('',#72955,#10290) ;
#7972 = LINE('',#72956,#10291) ;
#7973 = LINE('',#72957,#10292) ;
#7974 = LINE('',#72959,#10293) ;
#7975 = LINE('',#72961,#10294) ;
#7976 = LINE('',#72962,#10295) ;
#7977 = LINE('',#72965,#10296) ;
#7978 = LINE('',#72966,#10297) ;
#7979 = LINE('',#72967,#10298) ;
#7980 = LINE('',#72969,#10299) ;
#7981 = LINE('',#72971,#10300) ;
#7982 = LINE('',#72972,#10301) ;
#7983 = LINE('',#72975,#10302) ;
#7984 = LINE('',#72976,#10303) ;
#7985 = LINE('',#72977,#10304) ;
#7986 = LINE('',#72979,#10305) ;
#7987 = LINE('',#72981,#10306) ;
#7988 = LINE('',#72982,#10307) ;
#7989 = LINE('',#72985,#10308) ;
#7990 = LINE('',#72986,#10309) ;
#7991 = LINE('',#72987,#10310) ;
#7992 = LINE('',#72989,#10311) ;
#7993 = LINE('',#72991,#10312) ;
#7994 = LINE('',#72992,#10313) ;
#7995 = LINE('',#72995,#10314) ;
#7996 = LINE('',#72996,#10315) ;
#7997 = LINE('',#72997,#10316) ;
#7998 = LINE('',#72999,#10317) ;
#7999 = LINE('',#73001,#10318) ;
#8000 = LINE('',#73002,#10319) ;
#8001 = LINE('',#73005,#10320) ;
#8002 = LINE('',#73006,#10321) ;
#8003 = LINE('',#73007,#10322) ;
#8004 = LINE('',#73009,#10323) ;
#8005 = LINE('',#73011,#10324) ;
#8006 = LINE('',#73012,#10325) ;
#8007 = LINE('',#73015,#10326) ;
#8008 = LINE('',#73016,#10327) ;
#8009 = LINE('',#73017,#10328) ;
#8010 = LINE('',#73020,#10329) ;
#8011 = LINE('',#73022,#10330) ;
#8012 = LINE('',#73024,#10331) ;
#8013 = LINE('',#73026,#10332) ;
#8014 = LINE('',#73028,#10333) ;
#8015 = LINE('',#73030,#10334) ;
#8016 = LINE('',#73032,#10335) ;
#8017 = LINE('',#73034,#10336) ;
#8018 = LINE('',#73036,#10337) ;
#8019 = LINE('',#73049,#10338) ;
#8020 = LINE('',#73053,#10339) ;
#8021 = LINE('',#73067,#10340) ;
#8022 = LINE('',#73071,#10341) ;
#8023 = LINE('',#73085,#10342) ;
#8024 = LINE('',#73089,#10343) ;
#8025 = LINE('',#73103,#10344) ;
#8026 = LINE('',#73107,#10345) ;
#8027 = LINE('',#73121,#10346) ;
#8028 = LINE('',#73125,#10347) ;
#8029 = LINE('',#73139,#10348) ;
#8030 = LINE('',#73143,#10349) ;
#8031 = LINE('',#73157,#10350) ;
#8032 = LINE('',#73161,#10351) ;
#8033 = LINE('',#73175,#10352) ;
#8034 = LINE('',#73179,#10353) ;
#8035 = LINE('',#73190,#10354) ;
#8036 = LINE('',#73194,#10355) ;
#8037 = LINE('',#73197,#10356) ;
#8038 = LINE('',#73199,#10357) ;
#8039 = LINE('',#73201,#10358) ;
#8040 = LINE('',#73205,#10359) ;
#8041 = LINE('',#73207,#10360) ;
#8042 = LINE('',#73209,#10361) ;
#8043 = LINE('',#73213,#10362) ;
#8044 = LINE('',#73215,#10363) ;
#8045 = LINE('',#73217,#10364) ;
#8046 = LINE('',#73221,#10365) ;
#8047 = LINE('',#73223,#10366) ;
#8048 = LINE('',#73225,#10367) ;
#8049 = LINE('',#73229,#10368) ;
#8050 = LINE('',#73231,#10369) ;
#8051 = LINE('',#73233,#10370) ;
#8052 = LINE('',#73237,#10371) ;
#8053 = LINE('',#73239,#10372) ;
#8054 = LINE('',#73241,#10373) ;
#8055 = LINE('',#73245,#10374) ;
#8056 = LINE('',#73247,#10375) ;
#8057 = LINE('',#73249,#10376) ;
#8058 = LINE('',#73253,#10377) ;
#8059 = LINE('',#73255,#10378) ;
#8060 = LINE('',#73257,#10379) ;
#8061 = LINE('',#73265,#10380) ;
#8062 = LINE('',#73336,#10381) ;
#8063 = LINE('',#73412,#10382) ;
#8064 = LINE('',#73488,#10383) ;
#8065 = LINE('',#73564,#10384) ;
#8066 = LINE('',#73640,#10385) ;
#8067 = LINE('',#73716,#10386) ;
#8068 = LINE('',#73792,#10387) ;
#8069 = LINE('',#73868,#10388) ;
#8070 = LINE('',#73919,#10389) ;
#8071 = LINE('',#73995,#10390) ;
#8072 = LINE('',#74071,#10391) ;
#8073 = LINE('',#74147,#10392) ;
#8074 = LINE('',#74223,#10393) ;
#8075 = LINE('',#74299,#10394) ;
#8076 = LINE('',#74652,#10395) ;
#8077 = LINE('',#74684,#10396) ;
#8078 = LINE('',#74754,#10397) ;
#8079 = LINE('',#75015,#10398) ;
#8080 = LINE('',#75038,#10399) ;
#8081 = LINE('',#75090,#10400) ;
#8082 = LINE('',#75113,#10401) ;
#8083 = LINE('',#75116,#10402) ;
#8084 = LINE('',#75119,#10403) ;
#8085 = LINE('',#75121,#10404) ;
#8086 = LINE('',#75308,#10405) ;
#8087 = LINE('',#75393,#10406) ;
#8088 = LINE('',#75461,#10407) ;
#8089 = LINE('',#75680,#10408) ;
#8090 = LINE('',#75703,#10409) ;
#8091 = LINE('',#75755,#10410) ;
#8092 = LINE('',#75778,#10411) ;
#8093 = LINE('',#75781,#10412) ;
#8094 = LINE('',#75784,#10413) ;
#8095 = LINE('',#75786,#10414) ;
#8096 = LINE('',#75814,#10415) ;
#8097 = LINE('',#75817,#10416) ;
#8098 = LINE('',#75835,#10417) ;
#8099 = LINE('',#75844,#10418) ;
#8100 = LINE('',#76057,#10419) ;
#8101 = LINE('',#76058,#10420) ;
#8102 = LINE('',#76061,#10421) ;
#8103 = LINE('',#76084,#10422) ;
#8104 = LINE('',#76090,#10423) ;
#8105 = LINE('',#76092,#10424) ;
#8106 = LINE('',#76096,#10425) ;
#8107 = LINE('',#76100,#10426) ;
#8108 = LINE('',#76242,#10427) ;
#8109 = LINE('',#76245,#10428) ;
#8110 = LINE('',#76343,#10429) ;
#8111 = LINE('',#76344,#10430) ;
#8112 = LINE('',#76347,#10431) ;
#8113 = LINE('',#76370,#10432) ;
#8114 = LINE('',#76376,#10433) ;
#8115 = LINE('',#76378,#10434) ;
#8116 = LINE('',#76382,#10435) ;
#8117 = LINE('',#76386,#10436) ;
#8118 = LINE('',#76409,#10437) ;
#8119 = LINE('',#76412,#10438) ;
#8120 = LINE('',#76421,#10439) ;
#8121 = LINE('',#76424,#10440) ;
#8122 = LINE('',#77333,#10441) ;
#8123 = LINE('',#77335,#10442) ;
#8124 = LINE('',#77387,#10443) ;
#8125 = LINE('',#77390,#10444) ;
#8126 = LINE('',#77397,#10445) ;
#8127 = LINE('',#77399,#10446) ;
#8128 = LINE('',#77400,#10447) ;
#8129 = LINE('',#77403,#10448) ;
#8130 = LINE('',#77451,#10449) ;
#8131 = LINE('',#77452,#10450) ;
#8132 = LINE('',#77520,#10451) ;
#8133 = LINE('',#77523,#10452) ;
#8134 = LINE('',#77526,#10453) ;
#8135 = LINE('',#77527,#10454) ;
#8136 = LINE('',#77530,#10455) ;
#8137 = LINE('',#77534,#10456) ;
#8138 = LINE('',#77535,#10457) ;
#8139 = LINE('',#77537,#10458) ;
#8140 = LINE('',#77538,#10459) ;
#8141 = LINE('',#77562,#10460) ;
#8142 = LINE('',#77563,#10461) ;
#8143 = LINE('',#77597,#10462) ;
#8144 = LINE('',#77606,#10463) ;
#8145 = LINE('',#77608,#10464) ;
#8146 = LINE('',#77611,#10465) ;
#8147 = LINE('',#77612,#10466) ;
#8148 = LINE('',#77668,#10467) ;
#8149 = LINE('',#77678,#10468) ;
#8150 = LINE('',#77708,#10469) ;
#8151 = LINE('',#77710,#10470) ;
#8152 = LINE('',#77714,#10471) ;
#8153 = LINE('',#77716,#10472) ;
#8154 = LINE('',#77717,#10473) ;
#8155 = LINE('',#77744,#10474) ;
#8156 = LINE('',#77746,#10475) ;
#8157 = LINE('',#77781,#10476) ;
#8158 = LINE('',#77783,#10477) ;
#8159 = LINE('',#77819,#10478) ;
#8160 = LINE('',#77821,#10479) ;
#8161 = LINE('',#77873,#10480) ;
#8162 = LINE('',#77876,#10481) ;
#8163 = LINE('',#77883,#10482) ;
#8164 = LINE('',#77885,#10483) ;
#8165 = LINE('',#77886,#10484) ;
#8166 = LINE('',#77889,#10485) ;
#8167 = LINE('',#77937,#10486) ;
#8168 = LINE('',#77938,#10487) ;
#8169 = LINE('',#78006,#10488) ;
#8170 = LINE('',#78009,#10489) ;
#8171 = LINE('',#78012,#10490) ;
#8172 = LINE('',#78013,#10491) ;
#8173 = LINE('',#78016,#10492) ;
#8174 = LINE('',#78019,#10493) ;
#8175 = LINE('',#78021,#10494) ;
#8176 = LINE('',#78022,#10495) ;
#8177 = LINE('',#78028,#10496) ;
#8178 = LINE('',#78031,#10497) ;
#8179 = LINE('',#78084,#10498) ;
#8180 = LINE('',#78092,#10499) ;
#8181 = LINE('',#78093,#10500) ;
#8182 = LINE('',#78096,#10501) ;
#8183 = LINE('',#78098,#10502) ;
#8184 = LINE('',#78101,#10503) ;
#8185 = LINE('',#78102,#10504) ;
#8186 = LINE('',#78158,#10505) ;
#8187 = LINE('',#78168,#10506) ;
#8188 = LINE('',#78198,#10507) ;
#8189 = LINE('',#78206,#10508) ;
#8190 = LINE('',#78208,#10509) ;
#8191 = LINE('',#78209,#10510) ;
#8192 = LINE('',#78236,#10511) ;
#8193 = LINE('',#78238,#10512) ;
#8194 = LINE('',#78291,#10513) ;
#8195 = LINE('',#78429,#10514) ;
#8196 = LINE('',#78458,#10515) ;
#8197 = LINE('',#78791,#10516) ;
#8198 = LINE('',#78834,#10517) ;
#8199 = LINE('',#78910,#10518) ;
#8200 = LINE('',#78986,#10519) ;
#8201 = LINE('',#79025,#10520) ;
#8202 = LINE('',#79068,#10521) ;
#8203 = LINE('',#79144,#10522) ;
#8204 = LINE('',#79220,#10523) ;
#8205 = LINE('',#79407,#10524) ;
#8206 = LINE('',#79410,#10525) ;
#8207 = LINE('',#79424,#10526) ;
#8208 = LINE('',#79425,#10527) ;
#8209 = LINE('',#79448,#10528) ;
#8210 = LINE('',#79449,#10529) ;
#8211 = LINE('',#79457,#10530) ;
#8212 = LINE('',#79458,#10531) ;
#8213 = LINE('',#79462,#10532) ;
#8214 = LINE('',#79463,#10533) ;
#8215 = LINE('',#79476,#10534) ;
#8216 = LINE('',#79477,#10535) ;
#8217 = LINE('',#79482,#10536) ;
#8218 = LINE('',#79483,#10537) ;
#8219 = LINE('',#79491,#10538) ;
#8220 = LINE('',#79492,#10539) ;
#8221 = LINE('',#79494,#10540) ;
#8222 = LINE('',#79495,#10541) ;
#8223 = LINE('',#79500,#10542) ;
#8224 = LINE('',#79501,#10543) ;
#8225 = LINE('',#79503,#10544) ;
#8226 = LINE('',#79504,#10545) ;
#8227 = LINE('',#79513,#10546) ;
#8228 = LINE('',#79515,#10547) ;
#8229 = LINE('',#79521,#10548) ;
#8230 = LINE('',#79524,#10549) ;
#8231 = LINE('',#79527,#10550) ;
#8232 = LINE('',#79530,#10551) ;
#8233 = LINE('',#79537,#10552) ;
#8234 = LINE('',#79544,#10553) ;
#8235 = LINE('',#79548,#10554) ;
#8236 = LINE('',#79549,#10555) ;
#8237 = LINE('',#79553,#10556) ;
#8238 = LINE('',#79557,#10557) ;
#8239 = LINE('',#79561,#10558) ;
#8240 = LINE('',#79564,#10559) ;
#8241 = LINE('',#79569,#10560) ;
#8242 = LINE('',#79571,#10561) ;
#8243 = LINE('',#79573,#10562) ;
#8244 = LINE('',#79575,#10563) ;
#8245 = LINE('',#79577,#10564) ;
#8246 = LINE('',#79580,#10565) ;
#8247 = LINE('',#79584,#10566) ;
#8248 = LINE('',#79586,#10567) ;
#8249 = LINE('',#79593,#10568) ;
#8250 = LINE('',#79599,#10569) ;
#8251 = LINE('',#79603,#10570) ;
#8252 = LINE('',#79605,#10571) ;
#8253 = LINE('',#79607,#10572) ;
#8254 = LINE('',#79608,#10573) ;
#8255 = LINE('',#79612,#10574) ;
#8256 = LINE('',#79614,#10575) ;
#8257 = LINE('',#79618,#10576) ;
#8258 = LINE('',#79620,#10577) ;
#8259 = LINE('',#79622,#10578) ;
#8260 = LINE('',#79624,#10579) ;
#8261 = LINE('',#79626,#10580) ;
#8262 = LINE('',#79629,#10581) ;
#8263 = LINE('',#79633,#10582) ;
#8264 = LINE('',#79635,#10583) ;
#8265 = LINE('',#79637,#10584) ;
#8266 = LINE('',#79638,#10585) ;
#8267 = LINE('',#79694,#10586) ;
#8268 = LINE('',#79710,#10587) ;
#8269 = LINE('',#79726,#10588) ;
#8270 = LINE('',#79728,#10589) ;
#8271 = LINE('',#79730,#10590) ;
#8272 = LINE('',#79731,#10591) ;
#8273 = LINE('',#79738,#10592) ;
#8274 = LINE('',#79740,#10593) ;
#8275 = LINE('',#79744,#10594) ;
#8276 = LINE('',#79747,#10595) ;
#8277 = LINE('',#79751,#10596) ;
#8278 = LINE('',#79755,#10597) ;
#8279 = LINE('',#79759,#10598) ;
#8280 = LINE('',#79760,#10599) ;
#8281 = LINE('',#79765,#10600) ;
#8282 = LINE('',#79769,#10601) ;
#8283 = LINE('',#79771,#10602) ;
#8284 = LINE('',#79772,#10603) ;
#8285 = LINE('',#79799,#10604) ;
#8286 = LINE('',#79802,#10605) ;
#8287 = LINE('',#79807,#10606) ;
#8288 = LINE('',#79812,#10607) ;
#8289 = LINE('',#79828,#10608) ;
#8290 = LINE('',#79833,#10609) ;
#8291 = LINE('',#79848,#10610) ;
#8292 = LINE('',#79868,#10611) ;
#8293 = LINE('',#79871,#10612) ;
#8294 = LINE('',#79876,#10613) ;
#8295 = LINE('',#79899,#10614) ;
#8296 = LINE('',#81023,#10615) ;
#8297 = LINE('',#81027,#10616) ;
#8298 = LINE('',#81029,#10617) ;
#8299 = LINE('',#81033,#10618) ;
#8300 = LINE('',#81034,#10619) ;
#8301 = LINE('',#81036,#10620) ;
#8302 = LINE('',#81038,#10621) ;
#8303 = LINE('',#81042,#10622) ;
#8304 = LINE('',#81043,#10623) ;
#8305 = LINE('',#81045,#10624) ;
#8306 = LINE('',#81047,#10625) ;
#8307 = LINE('',#81051,#10626) ;
#8308 = LINE('',#81052,#10627) ;
#8309 = LINE('',#81054,#10628) ;
#8310 = LINE('',#81056,#10629) ;
#8311 = LINE('',#81060,#10630) ;
#8312 = LINE('',#81061,#10631) ;
#8313 = LINE('',#81065,#10632) ;
#8314 = LINE('',#81067,#10633) ;
#8315 = LINE('',#81069,#10634) ;
#8316 = LINE('',#81074,#10635) ;
#8317 = LINE('',#81076,#10636) ;
#8318 = LINE('',#81079,#10637) ;
#8319 = LINE('',#81083,#10638) ;
#8320 = LINE('',#81085,#10639) ;
#8321 = LINE('',#81087,#10640) ;
#8322 = LINE('',#81092,#10641) ;
#8323 = LINE('',#81094,#10642) ;
#8324 = LINE('',#81097,#10643) ;
#8325 = LINE('',#81106,#10644) ;
#8326 = LINE('',#81111,#10645) ;
#8327 = LINE('',#81120,#10646) ;
#8328 = LINE('',#81125,#10647) ;
#8329 = LINE('',#81134,#10648) ;
#8330 = LINE('',#81139,#10649) ;
#8331 = LINE('',#81143,#10650) ;
#8332 = LINE('',#81144,#10651) ;
#8333 = LINE('',#81145,#10652) ;
#8334 = LINE('',#81149,#10653) ;
#8335 = LINE('',#81150,#10654) ;
#8336 = LINE('',#81151,#10655) ;
#8337 = LINE('',#81164,#10656) ;
#8338 = LINE('',#81166,#10657) ;
#8339 = LINE('',#81168,#10658) ;
#8340 = LINE('',#81169,#10659) ;
#8341 = LINE('',#81173,#10660) ;
#8342 = LINE('',#81175,#10661) ;
#8343 = LINE('',#81177,#10662) ;
#8344 = LINE('',#81178,#10663) ;
#8345 = LINE('',#81190,#10664) ;
#8346 = LINE('',#81191,#10665) ;
#8347 = LINE('',#81192,#10666) ;
#8348 = LINE('',#81196,#10667) ;
#8349 = LINE('',#81197,#10668) ;
#8350 = LINE('',#81198,#10669) ;
#8351 = LINE('',#81211,#10670) ;
#8352 = LINE('',#81212,#10671) ;
#8353 = LINE('',#81213,#10672) ;
#8354 = LINE('',#81217,#10673) ;
#8355 = LINE('',#81218,#10674) ;
#8356 = LINE('',#81219,#10675) ;
#8357 = LINE('',#81243,#10676) ;
#8358 = LINE('',#81245,#10677) ;
#8359 = LINE('',#81246,#10678) ;
#8360 = LINE('',#81250,#10679) ;
#8361 = LINE('',#81252,#10680) ;
#8362 = LINE('',#81253,#10681) ;
#8363 = LINE('',#81257,#10682) ;
#8364 = LINE('',#81259,#10683) ;
#8365 = LINE('',#81261,#10684) ;
#8366 = LINE('',#81262,#10685) ;
#8367 = LINE('',#81278,#10686) ;
#8368 = LINE('',#81280,#10687) ;
#8369 = LINE('',#81281,#10688) ;
#8370 = LINE('',#81285,#10689) ;
#8371 = LINE('',#81287,#10690) ;
#8372 = LINE('',#81288,#10691) ;
#8373 = LINE('',#81292,#10692) ;
#8374 = LINE('',#81294,#10693) ;
#8375 = LINE('',#81296,#10694) ;
#8376 = LINE('',#81297,#10695) ;
#8377 = LINE('',#81311,#10696) ;
#8378 = LINE('',#81313,#10697) ;
#8379 = LINE('',#81315,#10698) ;
#8380 = LINE('',#81320,#10699) ;
#8381 = LINE('',#81322,#10700) ;
#8382 = LINE('',#81323,#10701) ;
#8383 = LINE('',#81327,#10702) ;
#8384 = LINE('',#81329,#10703) ;
#8385 = LINE('',#81331,#10704) ;
#8386 = LINE('',#81332,#10705) ;
#8387 = LINE('',#81346,#10706) ;
#8388 = LINE('',#81348,#10707) ;
#8389 = LINE('',#81350,#10708) ;
#8390 = LINE('',#81355,#10709) ;
#8391 = LINE('',#81357,#10710) ;
#8392 = LINE('',#81358,#10711) ;
#8393 = LINE('',#81362,#10712) ;
#8394 = LINE('',#81364,#10713) ;
#8395 = LINE('',#81366,#10714) ;
#8396 = LINE('',#81367,#10715) ;
#8397 = LINE('',#81380,#10716) ;
#8398 = LINE('',#81382,#10717) ;
#8399 = LINE('',#81384,#10718) ;
#8400 = LINE('',#81385,#10719) ;
#8401 = LINE('',#81387,#10720) ;
#8402 = LINE('',#81388,#10721) ;
#8403 = LINE('',#81391,#10722) ;
#8404 = LINE('',#81393,#10723) ;
#8405 = LINE('',#81395,#10724) ;
#8406 = LINE('',#81396,#10725) ;
#8407 = LINE('',#81398,#10726) ;
#8408 = LINE('',#81399,#10727) ;
#8409 = LINE('',#81402,#10728) ;
#8410 = LINE('',#81404,#10729) ;
#8411 = LINE('',#81406,#10730) ;
#8412 = LINE('',#81407,#10731) ;
#8413 = LINE('',#81409,#10732) ;
#8414 = LINE('',#81410,#10733) ;
#8415 = LINE('',#81413,#10734) ;
#8416 = LINE('',#81415,#10735) ;
#8417 = LINE('',#81417,#10736) ;
#8418 = LINE('',#81418,#10737) ;
#8419 = LINE('',#81420,#10738) ;
#8420 = LINE('',#81421,#10739) ;
#8421 = LINE('',#81472,#10740) ;
#8422 = LINE('',#81474,#10741) ;
#8423 = LINE('',#81518,#10742) ;
#8424 = LINE('',#81520,#10743) ;
#8425 = LINE('',#81597,#10744) ;
#8426 = LINE('',#81599,#10745) ;
#8427 = LINE('',#81643,#10746) ;
#8428 = LINE('',#81645,#10747) ;
#8429 = LINE('',#81667,#10748) ;
#8430 = LINE('',#81669,#10749) ;
#8431 = LINE('',#81671,#10750) ;
#8432 = LINE('',#81673,#10751) ;
#8433 = LINE('',#81675,#10752) ;
#8434 = LINE('',#81676,#10753) ;
#8435 = LINE('',#81679,#10754) ;
#8436 = LINE('',#81681,#10755) ;
#8437 = LINE('',#81683,#10756) ;
#8438 = LINE('',#81685,#10757) ;
#8439 = LINE('',#81686,#10758) ;
#8440 = LINE('',#81689,#10759) ;
#8441 = LINE('',#81691,#10760) ;
#8442 = LINE('',#81693,#10761) ;
#8443 = LINE('',#81694,#10762) ;
#8444 = LINE('',#81697,#10763) ;
#8445 = LINE('',#81698,#10764) ;
#8446 = LINE('',#81702,#10765) ;
#8447 = LINE('',#81704,#10766) ;
#8448 = LINE('',#81705,#10767) ;
#8449 = LINE('',#81706,#10768) ;
#8450 = LINE('',#81709,#10769) ;
#8451 = LINE('',#81711,#10770) ;
#8452 = LINE('',#81713,#10771) ;
#8453 = LINE('',#81714,#10772) ;
#8454 = LINE('',#81718,#10773) ;
#8455 = LINE('',#81720,#10774) ;
#8456 = LINE('',#81721,#10775) ;
#8457 = LINE('',#81723,#10776) ;
#8458 = LINE('',#81724,#10777) ;
#8459 = LINE('',#81727,#10778) ;
#8460 = LINE('',#81728,#10779) ;
#8461 = LINE('',#81729,#10780) ;
#8462 = LINE('',#81732,#10781) ;
#8463 = LINE('',#81733,#10782) ;
#8464 = LINE('',#81736,#10783) ;
#8465 = LINE('',#81738,#10784) ;
#8466 = LINE('',#81740,#10785) ;
#8467 = LINE('',#81741,#10786) ;
#8468 = LINE('',#81744,#10787) ;
#8469 = LINE('',#81745,#10788) ;
#8470 = LINE('',#81748,#10789) ;
#8471 = LINE('',#81760,#10790) ;
#8472 = LINE('',#81773,#10791) ;
#8473 = LINE('',#81774,#10792) ;
#8474 = LINE('',#81777,#10793) ;
#8475 = LINE('',#81778,#10794) ;
#8476 = LINE('',#81780,#10795) ;
#8477 = LINE('',#81783,#10796) ;
#8478 = LINE('',#81785,#10797) ;
#8479 = LINE('',#81787,#10798) ;
#8480 = LINE('',#81789,#10799) ;
#8481 = LINE('',#81791,#10800) ;
#8482 = LINE('',#81800,#10801) ;
#8483 = LINE('',#81853,#10802) ;
#8484 = LINE('',#81929,#10803) ;
#8485 = LINE('',#82007,#10804) ;
#8486 = LINE('',#82085,#10805) ;
#8487 = LINE('',#82161,#10806) ;
#8488 = LINE('',#82237,#10807) ;
#8489 = LINE('',#82313,#10808) ;
#8490 = LINE('',#82389,#10809) ;
#8491 = LINE('',#82467,#10810) ;
#8492 = LINE('',#82543,#10811) ;
#8493 = LINE('',#82621,#10812) ;
#8494 = LINE('',#82697,#10813) ;
#8495 = LINE('',#82773,#10814) ;
#8496 = LINE('',#82849,#10815) ;
#8497 = LINE('',#82925,#10816) ;
#8498 = LINE('',#83074,#10817) ;
#8499 = LINE('',#83150,#10818) ;
#8500 = LINE('',#83226,#10819) ;
#8501 = LINE('',#83302,#10820) ;
#8502 = LINE('',#83378,#10821) ;
#8503 = LINE('',#83456,#10822) ;
#8504 = LINE('',#83532,#10823) ;
#8505 = LINE('',#83608,#10824) ;
#8506 = LINE('',#83686,#10825) ;
#8507 = LINE('',#83762,#10826) ;
#8508 = LINE('',#83838,#10827) ;
#8509 = LINE('',#83914,#10828) ;
#8510 = LINE('',#83990,#10829) ;
#8511 = LINE('',#84068,#10830) ;
#8512 = LINE('',#84144,#10831) ;
#8513 = LINE('',#84222,#10832) ;
#8514 = LINE('',#84448,#10833) ;
#8515 = LINE('',#84921,#10834) ;
#8516 = LINE('',#85395,#10835) ;
#8517 = LINE('',#85396,#10836) ;
#8518 = LINE('',#85399,#10837) ;
#8519 = LINE('',#85400,#10838) ;
#8520 = LINE('',#85403,#10839) ;
#8521 = LINE('',#85404,#10840) ;
#8522 = LINE('',#85406,#10841) ;
#8523 = LINE('',#85409,#10842) ;
#8524 = LINE('',#85411,#10843) ;
#8525 = LINE('',#85413,#10844) ;
#8526 = LINE('',#85415,#10845) ;
#8527 = LINE('',#85417,#10846) ;
#8528 = LINE('',#85421,#10847) ;
#8529 = LINE('',#85423,#10848) ;
#8530 = LINE('',#85425,#10849) ;
#8531 = LINE('',#85426,#10850) ;
#8532 = LINE('',#85428,#10851) ;
#8533 = LINE('',#85430,#10852) ;
#8534 = LINE('',#85431,#10853) ;
#8535 = LINE('',#85433,#10854) ;
#8536 = LINE('',#85435,#10855) ;
#8537 = LINE('',#85437,#10856) ;
#8538 = LINE('',#85440,#10857) ;
#8539 = LINE('',#85442,#10858) ;
#8540 = LINE('',#85444,#10859) ;
#8541 = LINE('',#85454,#10860) ;
#8542 = LINE('',#85456,#10861) ;
#8543 = LINE('',#85458,#10862) ;
#8544 = LINE('',#85464,#10863) ;
#8545 = LINE('',#85466,#10864) ;
#8546 = LINE('',#85468,#10865) ;
#8547 = LINE('',#85469,#10866) ;
#8548 = LINE('',#85473,#10867) ;
#8549 = LINE('',#85475,#10868) ;
#8550 = LINE('',#85477,#10869) ;
#8551 = LINE('',#85478,#10870) ;
#8552 = LINE('',#86246,#10871) ;
#8553 = LINE('',#86258,#10872) ;
#8554 = VECTOR('',#36533,10.) ;
#8555 = VECTOR('',#36536,10.) ;
#8556 = VECTOR('',#36539,10.) ;
#8557 = VECTOR('',#36540,10.) ;
#8558 = VECTOR('',#36541,10.) ;
#8559 = VECTOR('',#36542,10.) ;
#8560 = VECTOR('',#36543,10.) ;
#8561 = VECTOR('',#36572,10.) ;
#8562 = VECTOR('',#36575,10.) ;
#8563 = VECTOR('',#36578,10.) ;
#8564 = VECTOR('',#36581,10.) ;
#8565 = VECTOR('',#36584,10.) ;
#8566 = VECTOR('',#36587,10.) ;
#8567 = VECTOR('',#36590,10.) ;
#8568 = VECTOR('',#36593,10.) ;
#8569 = VECTOR('',#36596,10.) ;
#8570 = VECTOR('',#36599,10.) ;
#8571 = VECTOR('',#36602,10.) ;
#8572 = VECTOR('',#36605,10.) ;
#8573 = VECTOR('',#36658,10.) ;
#8574 = VECTOR('',#36663,10.) ;
#8575 = VECTOR('',#36668,10.) ;
#8576 = VECTOR('',#36671,10.) ;
#8577 = VECTOR('',#36674,10.) ;
#8578 = VECTOR('',#36677,10.) ;
#8579 = VECTOR('',#36680,10.) ;
#8580 = VECTOR('',#36683,10.) ;
#8581 = VECTOR('',#36686,10.) ;
#8582 = VECTOR('',#36689,10.) ;
#8583 = VECTOR('',#36692,10.) ;
#8584 = VECTOR('',#36701,10.) ;
#8585 = VECTOR('',#36704,10.) ;
#8586 = VECTOR('',#36707,10.) ;
#8587 = VECTOR('',#36708,10.) ;
#8588 = VECTOR('',#36709,10.) ;
#8589 = VECTOR('',#36710,10.) ;
#8590 = VECTOR('',#36711,10.) ;
#8591 = VECTOR('',#36714,10.) ;
#8592 = VECTOR('',#36717,10.) ;
#8593 = VECTOR('',#36720,10.) ;
#8594 = VECTOR('',#36723,10.) ;
#8595 = VECTOR('',#36726,10.) ;
#8596 = VECTOR('',#36729,10.) ;
#8597 = VECTOR('',#36732,10.) ;
#8598 = VECTOR('',#36735,10.) ;
#8599 = VECTOR('',#36746,10.) ;
#8600 = VECTOR('',#36749,10.) ;
#8601 = VECTOR('',#36752,10.) ;
#8602 = VECTOR('',#36753,10.) ;
#8603 = VECTOR('',#36754,1.711483519287) ;
#8604 = VECTOR('',#36755,10.) ;
#8605 = VECTOR('',#36758,10.) ;
#8606 = VECTOR('',#36761,10.) ;
#8607 = VECTOR('',#36764,10.) ;
#8608 = VECTOR('',#36767,10.) ;
#8609 = VECTOR('',#36770,10.) ;
#8610 = VECTOR('',#36773,10.) ;
#8611 = VECTOR('',#36776,10.) ;
#8612 = VECTOR('',#36779,10.) ;
#8613 = VECTOR('',#36788,10.) ;
#8614 = VECTOR('',#36791,10.) ;
#8615 = VECTOR('',#36794,10.) ;
#8616 = VECTOR('',#36795,10.) ;
#8617 = VECTOR('',#36798,10.) ;
#8618 = VECTOR('',#36799,10.) ;
#8619 = VECTOR('',#36802,10.) ;
#8620 = VECTOR('',#36807,10.) ;
#8621 = VECTOR('',#36810,10.) ;
#8622 = VECTOR('',#36813,10.) ;
#8623 = VECTOR('',#36814,10.) ;
#8624 = VECTOR('',#36815,10.) ;
#8625 = VECTOR('',#36816,10.) ;
#8626 = VECTOR('',#36819,10.) ;
#8627 = VECTOR('',#36820,0.1) ;
#8628 = VECTOR('',#36821,0.09999999999997) ;
#8629 = VECTOR('',#36822,108.3) ;
#8630 = VECTOR('',#36823,0.09999999999997) ;
#8631 = VECTOR('',#36824,0.1) ;
#8632 = VECTOR('',#36839,22.) ;
#8633 = VECTOR('',#36842,22.) ;
#8634 = VECTOR('',#36845,22.) ;
#8635 = VECTOR('',#36848,22.) ;
#8636 = VECTOR('',#36851,22.) ;
#8637 = VECTOR('',#36854,22.) ;
#8638 = VECTOR('',#36857,22.) ;
#8639 = VECTOR('',#36860,22.) ;
#8640 = VECTOR('',#36863,22.) ;
#8641 = VECTOR('',#36866,22.) ;
#8642 = VECTOR('',#36869,22.) ;
#8643 = VECTOR('',#36872,22.) ;
#8644 = VECTOR('',#36937,10.) ;
#8645 = VECTOR('',#36940,10.) ;
#8646 = VECTOR('',#36943,10.) ;
#8647 = VECTOR('',#36946,10.) ;
#8648 = VECTOR('',#36949,10.) ;
#8649 = VECTOR('',#36952,10.) ;
#8650 = VECTOR('',#36955,10.) ;
#8651 = VECTOR('',#36962,10.) ;
#8652 = VECTOR('',#36965,10.) ;
#8653 = VECTOR('',#36970,10.) ;
#8654 = VECTOR('',#36971,0.75) ;
#8655 = VECTOR('',#36974,10.) ;
#8656 = VECTOR('',#36977,10.) ;
#8657 = VECTOR('',#36978,10.) ;
#8658 = VECTOR('',#36981,10.) ;
#8659 = VECTOR('',#36984,0.75) ;
#8660 = VECTOR('',#36985,10.) ;
#8661 = VECTOR('',#36986,10.) ;
#8662 = VECTOR('',#36989,10.) ;
#8663 = VECTOR('',#36992,0.75) ;
#8664 = VECTOR('',#36993,10.) ;
#8665 = VECTOR('',#36994,0.7499999999999) ;
#8666 = VECTOR('',#36997,10.) ;
#8667 = VECTOR('',#37000,0.75) ;
#8668 = VECTOR('',#37003,0.7499999999999) ;
#8669 = VECTOR('',#37006,10.) ;
#8670 = VECTOR('',#37011,10.) ;
#8671 = VECTOR('',#37012,10.) ;
#8672 = VECTOR('',#37015,10.) ;
#8673 = VECTOR('',#37020,10.) ;
#8674 = VECTOR('',#37021,10.) ;
#8675 = VECTOR('',#37028,10.) ;
#8676 = VECTOR('',#37031,10.) ;
#8677 = VECTOR('',#37034,10.) ;
#8678 = VECTOR('',#37035,10.) ;
#8679 = VECTOR('',#37036,10.) ;
#8680 = VECTOR('',#37039,10.) ;
#8681 = VECTOR('',#37040,10.) ;
#8682 = VECTOR('',#37041,10.) ;
#8683 = VECTOR('',#37048,10.) ;
#8684 = VECTOR('',#37053,5.5) ;
#8685 = VECTOR('',#37056,10.) ;
#8686 = VECTOR('',#37059,10.) ;
#8687 = VECTOR('',#37064,10.) ;
#8688 = VECTOR('',#37065,10.) ;
#8689 = VECTOR('',#37068,10.) ;
#8690 = VECTOR('',#37071,10.) ;
#8691 = VECTOR('',#37072,10.) ;
#8692 = VECTOR('',#37075,10.) ;
#8693 = VECTOR('',#37080,10.) ;
#8694 = VECTOR('',#37081,10.) ;
#8695 = VECTOR('',#37084,10.) ;
#8696 = VECTOR('',#37087,10.) ;
#8697 = VECTOR('',#37088,10.) ;
#8698 = VECTOR('',#37093,10.) ;
#8699 = VECTOR('',#37096,10.) ;
#8700 = VECTOR('',#37097,10.) ;
#8701 = VECTOR('',#37100,10.) ;
#8702 = VECTOR('',#37103,10.) ;
#8703 = VECTOR('',#37106,10.) ;
#8704 = VECTOR('',#37111,10.) ;
#8705 = VECTOR('',#37112,10.) ;
#8706 = VECTOR('',#37115,10.) ;
#8707 = VECTOR('',#37118,10.) ;
#8708 = VECTOR('',#37121,10.) ;
#8709 = VECTOR('',#37124,10.) ;
#8710 = VECTOR('',#37133,5.5) ;
#8711 = VECTOR('',#37142,1.25) ;
#8712 = VECTOR('',#37145,1.25) ;
#8713 = VECTOR('',#37150,1.25) ;
#8714 = VECTOR('',#37153,0.75) ;
#8715 = VECTOR('',#37154,0.75) ;
#8716 = VECTOR('',#37157,0.75) ;
#8717 = VECTOR('',#37158,0.75) ;
#8718 = VECTOR('',#37167,2.390165042945) ;
#8719 = VECTOR('',#37170,2.390165042945) ;
#8720 = VECTOR('',#37177,2.) ;
#8721 = VECTOR('',#37180,2.) ;
#8722 = VECTOR('',#37183,2.) ;
#8723 = VECTOR('',#37186,2.) ;
#8724 = VECTOR('',#37189,0.75) ;
#8725 = VECTOR('',#37190,0.75) ;
#8726 = VECTOR('',#37193,0.75) ;
#8727 = VECTOR('',#37196,0.75) ;
#8728 = VECTOR('',#37201,0.75) ;
#8729 = VECTOR('',#37202,0.75) ;
#8730 = VECTOR('',#37205,0.75) ;
#8731 = VECTOR('',#37208,0.75) ;
#8732 = VECTOR('',#37213,0.75) ;
#8733 = VECTOR('',#37214,0.75) ;
#8734 = VECTOR('',#37217,0.75) ;
#8735 = VECTOR('',#37220,0.75) ;
#8736 = VECTOR('',#37225,0.75) ;
#8737 = VECTOR('',#37226,0.75) ;
#8738 = VECTOR('',#37229,0.75) ;
#8739 = VECTOR('',#37232,0.75) ;
#8740 = VECTOR('',#37237,0.75) ;
#8741 = VECTOR('',#37238,0.75) ;
#8742 = VECTOR('',#37241,0.75) ;
#8743 = VECTOR('',#37244,0.75) ;
#8744 = VECTOR('',#37249,0.75) ;
#8745 = VECTOR('',#37250,0.75) ;
#8746 = VECTOR('',#37253,0.75) ;
#8747 = VECTOR('',#37256,0.75) ;
#8748 = VECTOR('',#37261,108.3) ;
#8749 = VECTOR('',#37266,1.25) ;
#8750 = VECTOR('',#37275,0.75) ;
#8751 = VECTOR('',#37276,0.75) ;
#8752 = VECTOR('',#37279,0.75) ;
#8753 = VECTOR('',#37280,0.75) ;
#8754 = VECTOR('',#37287,0.75) ;
#8755 = VECTOR('',#37288,0.75) ;
#8756 = VECTOR('',#37291,0.75) ;
#8757 = VECTOR('',#37292,0.75) ;
#8758 = VECTOR('',#37299,0.75) ;
#8759 = VECTOR('',#37300,0.75) ;
#8760 = VECTOR('',#37303,0.75) ;
#8761 = VECTOR('',#37304,0.75) ;
#8762 = VECTOR('',#37317,1.17524047358083) ;
#8763 = VECTOR('',#37322,1.17524047358083) ;
#8764 = VECTOR('',#37325,1.17524047358083) ;
#8765 = VECTOR('',#37328,1.17524047358083) ;
#8766 = VECTOR('',#37331,1.17524047358083) ;
#8767 = VECTOR('',#37336,1.5) ;
#8768 = VECTOR('',#37341,1.5) ;
#8769 = VECTOR('',#37344,1.5) ;
#8770 = VECTOR('',#37347,1.5) ;
#8771 = VECTOR('',#37350,1.5) ;
#8772 = VECTOR('',#37353,1.5) ;
#8773 = VECTOR('',#37358,1.5) ;
#8774 = VECTOR('',#37361,1.5) ;
#8775 = VECTOR('',#37396,1000.) ;
#8776 = VECTOR('',#37397,1000.) ;
#8777 = VECTOR('',#37400,1000.) ;
#8778 = VECTOR('',#37403,1000.) ;
#8779 = VECTOR('',#37406,1000.) ;
#8780 = VECTOR('',#37409,1000.) ;
#8781 = VECTOR('',#37460,1.00995540144767) ;
#8782 = VECTOR('',#37465,1.00995540144767) ;
#8783 = VECTOR('',#37470,1.00995540144767) ;
#8784 = VECTOR('',#37473,1.00995540144767) ;
#8785 = VECTOR('',#37476,1.00995540144767) ;
#8786 = VECTOR('',#37479,1.00995540144767) ;
#8787 = VECTOR('',#37482,1.4224) ;
#8788 = VECTOR('',#37485,1.4224) ;
#8789 = VECTOR('',#37494,1.4224) ;
#8790 = VECTOR('',#37497,1.4224) ;
#8791 = VECTOR('',#37500,1.4224) ;
#8792 = VECTOR('',#37503,1.4224) ;
#8793 = VECTOR('',#37524,1.4224) ;
#8794 = VECTOR('',#37529,1000.) ;
#8795 = VECTOR('',#37530,1000.) ;
#8796 = VECTOR('',#37531,1000.) ;
#8797 = VECTOR('',#37532,1000.) ;
#8798 = VECTOR('',#37535,1000.) ;
#8799 = VECTOR('',#37536,1000.) ;
#8800 = VECTOR('',#37537,1000.) ;
#8801 = VECTOR('',#37538,1000.) ;
#8802 = VECTOR('',#37541,1000.) ;
#8803 = VECTOR('',#37542,1000.) ;
#8804 = VECTOR('',#37543,1000.) ;
#8805 = VECTOR('',#37544,1000.) ;
#8806 = VECTOR('',#37547,1000.) ;
#8807 = VECTOR('',#37548,1000.) ;
#8808 = VECTOR('',#37549,1000.) ;
#8809 = VECTOR('',#37550,1000.) ;
#8810 = VECTOR('',#37553,0.92075) ;
#8811 = VECTOR('',#37558,0.968718914342085) ;
#8812 = VECTOR('',#37589,1000.) ;
#8813 = VECTOR('',#37590,1000.) ;
#8814 = VECTOR('',#37593,1000.) ;
#8815 = VECTOR('',#37598,1000.) ;
#8816 = VECTOR('',#37601,1000.) ;
#8817 = VECTOR('',#37604,1000.) ;
#8818 = VECTOR('',#37609,1000.) ;
#8819 = VECTOR('',#37612,1000.) ;
#8820 = VECTOR('',#37615,1000.) ;
#8821 = VECTOR('',#37626,1000.) ;
#8822 = VECTOR('',#37629,1000.) ;
#8823 = VECTOR('',#37632,1000.) ;
#8824 = VECTOR('',#37655,2.05475) ;
#8825 = VECTOR('',#37660,2.05475) ;
#8826 = VECTOR('',#37663,2.05475) ;
#8827 = VECTOR('',#37668,2.05475000000001) ;
#8828 = VECTOR('',#37673,2.05475000000001) ;
#8829 = VECTOR('',#37676,2.05475000000001) ;
#8830 = VECTOR('',#37681,2.05475000000001) ;
#8831 = VECTOR('',#37686,2.05475000000001) ;
#8832 = VECTOR('',#37689,2.05475000000001) ;
#8833 = VECTOR('',#37694,2.05474999999993) ;
#8834 = VECTOR('',#37699,2.05474999999993) ;
#8835 = VECTOR('',#37702,2.05474999999993) ;
#8836 = VECTOR('',#37707,1.66599999999999) ;
#8837 = VECTOR('',#37712,1.66599999999999) ;
#8838 = VECTOR('',#37717,1.66599999999999) ;
#8839 = VECTOR('',#37722,1.66599999999999) ;
#8840 = VECTOR('',#37727,1.66599999999999) ;
#8841 = VECTOR('',#37732,1.66599999999999) ;
#8842 = VECTOR('',#37737,1.66599999999999) ;
#8843 = VECTOR('',#37742,1.66599999999999) ;
#8844 = VECTOR('',#37747,1.66599999999999) ;
#8845 = VECTOR('',#37752,1.66599999999998) ;
#8846 = VECTOR('',#37757,1.66599999999998) ;
#8847 = VECTOR('',#37762,1.66599999999998) ;
#8848 = VECTOR('',#37767,2.05475) ;
#8849 = VECTOR('',#37772,2.05475) ;
#8850 = VECTOR('',#37775,2.05475) ;
#8851 = VECTOR('',#37780,2.05475) ;
#8852 = VECTOR('',#37785,2.05475) ;
#8853 = VECTOR('',#37788,2.05475) ;
#8854 = VECTOR('',#37793,1.666) ;
#8855 = VECTOR('',#37798,1.666) ;
#8856 = VECTOR('',#37803,1.666) ;
#8857 = VECTOR('',#37808,1.666) ;
#8858 = VECTOR('',#37813,1.666) ;
#8859 = VECTOR('',#37818,1.666) ;
#8860 = VECTOR('',#37823,2.05475) ;
#8861 = VECTOR('',#37828,2.05475) ;
#8862 = VECTOR('',#37831,2.05475) ;
#8863 = VECTOR('',#37836,2.05475) ;
#8864 = VECTOR('',#37841,2.05475) ;
#8865 = VECTOR('',#37844,2.05475) ;
#8866 = VECTOR('',#37849,1.66600000000001) ;
#8867 = VECTOR('',#37854,1.66600000000001) ;
#8868 = VECTOR('',#37859,1.66600000000001) ;
#8869 = VECTOR('',#37864,1.66600000000001) ;
#8870 = VECTOR('',#37869,1.66600000000001) ;
#8871 = VECTOR('',#37874,1.66600000000001) ;
#8872 = VECTOR('',#37913,10.) ;
#8873 = VECTOR('',#37916,10.) ;
#8874 = VECTOR('',#37921,2.5) ;
#8875 = VECTOR('',#37924,10.) ;
#8876 = VECTOR('',#37929,2.5) ;
#8877 = VECTOR('',#37932,2.5) ;
#8878 = VECTOR('',#37937,2.5) ;
#8879 = VECTOR('',#37940,2.5) ;
#8880 = VECTOR('',#37945,10.) ;
#8881 = VECTOR('',#37948,2.5) ;
#8882 = VECTOR('',#37951,10.) ;
#8883 = VECTOR('',#37954,10.) ;
#8884 = VECTOR('',#37955,10.) ;
#8885 = VECTOR('',#37958,10.) ;
#8886 = VECTOR('',#37961,10.) ;
#8887 = VECTOR('',#37962,10.) ;
#8888 = VECTOR('',#37967,115.) ;
#8889 = VECTOR('',#37970,111.) ;
#8890 = VECTOR('',#37975,10.) ;
#8891 = VECTOR('',#37978,10.) ;
#8892 = VECTOR('',#37981,10.) ;
#8893 = VECTOR('',#37982,10.) ;
#8894 = VECTOR('',#37983,10.) ;
#8895 = VECTOR('',#37986,10.) ;
#8896 = VECTOR('',#37987,10.) ;
#8897 = VECTOR('',#37988,10.) ;
#8898 = VECTOR('',#37991,10.) ;
#8899 = VECTOR('',#37992,10.) ;
#8900 = VECTOR('',#37993,10.) ;
#8901 = VECTOR('',#37994,10.) ;
#8902 = VECTOR('',#37995,10.) ;
#8903 = VECTOR('',#37996,10.) ;
#8904 = VECTOR('',#37997,1.65) ;
#8905 = VECTOR('',#37998,83.9) ;
#8906 = VECTOR('',#37999,1.65) ;
#8907 = VECTOR('',#38000,10.) ;
#8908 = VECTOR('',#38001,10.) ;
#8909 = VECTOR('',#38004,10.) ;
#8910 = VECTOR('',#38007,10.) ;
#8911 = VECTOR('',#38008,10.) ;
#8912 = VECTOR('',#38009,10.) ;
#8913 = VECTOR('',#38010,10.) ;
#8914 = VECTOR('',#38011,10.) ;
#8915 = VECTOR('',#38014,10.) ;
#8916 = VECTOR('',#38015,10.) ;
#8917 = VECTOR('',#38016,10.) ;
#8918 = VECTOR('',#38017,10.) ;
#8919 = VECTOR('',#38018,10.) ;
#8920 = VECTOR('',#38019,10.) ;
#8921 = VECTOR('',#38020,10.) ;
#8922 = VECTOR('',#38021,10.) ;
#8923 = VECTOR('',#38022,10.) ;
#8924 = VECTOR('',#38023,10.) ;
#8925 = VECTOR('',#38024,10.) ;
#8926 = VECTOR('',#38025,10.) ;
#8927 = VECTOR('',#38032,10.) ;
#8928 = VECTOR('',#38035,10.) ;
#8929 = VECTOR('',#38038,10.) ;
#8930 = VECTOR('',#38039,10.) ;
#8931 = VECTOR('',#38040,10.) ;
#8932 = VECTOR('',#38041,10.) ;
#8933 = VECTOR('',#38042,10.) ;
#8934 = VECTOR('',#38045,10.) ;
#8935 = VECTOR('',#38046,10.) ;
#8936 = VECTOR('',#38047,10.) ;
#8937 = VECTOR('',#38050,10.) ;
#8938 = VECTOR('',#38051,10.) ;
#8939 = VECTOR('',#38052,10.) ;
#8940 = VECTOR('',#38055,10.) ;
#8941 = VECTOR('',#38056,10.) ;
#8942 = VECTOR('',#38057,10.) ;
#8943 = VECTOR('',#38060,10.) ;
#8944 = VECTOR('',#38063,10.) ;
#8945 = VECTOR('',#38064,10.) ;
#8946 = VECTOR('',#38065,10.) ;
#8947 = VECTOR('',#38066,10.) ;
#8948 = VECTOR('',#38067,10.) ;
#8949 = VECTOR('',#38068,10.) ;
#8950 = VECTOR('',#38069,10.) ;
#8951 = VECTOR('',#38070,10.) ;
#8952 = VECTOR('',#38071,10.) ;
#8953 = VECTOR('',#38072,10.) ;
#8954 = VECTOR('',#38073,10.) ;
#8955 = VECTOR('',#38074,10.) ;
#8956 = VECTOR('',#38075,10.) ;
#8957 = VECTOR('',#38076,10.) ;
#8958 = VECTOR('',#38077,10.) ;
#8959 = VECTOR('',#38078,10.) ;
#8960 = VECTOR('',#38081,10.) ;
#8961 = VECTOR('',#38084,10.) ;
#8962 = VECTOR('',#38087,10.) ;
#8963 = VECTOR('',#38090,10.) ;
#8964 = VECTOR('',#38093,10.) ;
#8965 = VECTOR('',#38094,10.) ;
#8966 = VECTOR('',#38095,27.5) ;
#8967 = VECTOR('',#38096,10.) ;
#8968 = VECTOR('',#38097,10.) ;
#8969 = VECTOR('',#38098,10.) ;
#8970 = VECTOR('',#38101,10.) ;
#8971 = VECTOR('',#38104,10.) ;
#8972 = VECTOR('',#38107,10.) ;
#8973 = VECTOR('',#38108,10.) ;
#8974 = VECTOR('',#38109,10.) ;
#8975 = VECTOR('',#38110,196.3) ;
#8976 = VECTOR('',#38111,19.) ;
#8977 = VECTOR('',#38114,19.) ;
#8978 = VECTOR('',#38115,3.98) ;
#8979 = VECTOR('',#38116,19.) ;
#8980 = VECTOR('',#38119,19.) ;
#8981 = VECTOR('',#38120,196.3) ;
#8982 = VECTOR('',#38121,10.) ;
#8983 = VECTOR('',#38124,2.) ;
#8984 = VECTOR('',#38125,7.) ;
#8985 = VECTOR('',#38126,2.) ;
#8986 = VECTOR('',#38127,7.) ;
#8987 = VECTOR('',#38128,2.) ;
#8988 = VECTOR('',#38129,7.) ;
#8989 = VECTOR('',#38130,2.) ;
#8990 = VECTOR('',#38131,7.) ;
#8991 = VECTOR('',#38132,2.) ;
#8992 = VECTOR('',#38133,7.) ;
#8993 = VECTOR('',#38134,2.) ;
#8994 = VECTOR('',#38135,7.) ;
#8995 = VECTOR('',#38138,79.4000000028) ;
#8996 = VECTOR('',#38141,14.0000000028) ;
#8997 = VECTOR('',#38142,89.9) ;
#8998 = VECTOR('',#38143,14.) ;
#8999 = VECTOR('',#38148,143.) ;
#9000 = VECTOR('',#38149,19.) ;
#9001 = VECTOR('',#38152,19.) ;
#9002 = VECTOR('',#38153,3.98) ;
#9003 = VECTOR('',#38154,19.) ;
#9004 = VECTOR('',#38157,19.) ;
#9005 = VECTOR('',#38158,41.3) ;
#9006 = VECTOR('',#38159,19.) ;
#9007 = VECTOR('',#38162,19.) ;
#9008 = VECTOR('',#38163,4.) ;
#9009 = VECTOR('',#38164,19.) ;
#9010 = VECTOR('',#38167,19.) ;
#9011 = VECTOR('',#38168,143.) ;
#9012 = VECTOR('',#38169,10.) ;
#9013 = VECTOR('',#38170,10.) ;
#9014 = VECTOR('',#38171,10.) ;
#9015 = VECTOR('',#38172,10.) ;
#9016 = VECTOR('',#38175,10.) ;
#9017 = VECTOR('',#38178,10.) ;
#9018 = VECTOR('',#38181,10.) ;
#9019 = VECTOR('',#38184,10.) ;
#9020 = VECTOR('',#38187,23.0000000028) ;
#9021 = VECTOR('',#38190,14.0000000028) ;
#9022 = VECTOR('',#38191,33.5) ;
#9023 = VECTOR('',#38192,14.) ;
#9024 = VECTOR('',#38193,2.) ;
#9025 = VECTOR('',#38194,7.) ;
#9026 = VECTOR('',#38195,2.) ;
#9027 = VECTOR('',#38196,7.) ;
#9028 = VECTOR('',#38197,2.) ;
#9029 = VECTOR('',#38198,7.) ;
#9030 = VECTOR('',#38199,2.) ;
#9031 = VECTOR('',#38200,7.) ;
#9032 = VECTOR('',#38201,2.) ;
#9033 = VECTOR('',#38202,7.) ;
#9034 = VECTOR('',#38203,2.) ;
#9035 = VECTOR('',#38204,7.) ;
#9036 = VECTOR('',#38205,2.) ;
#9037 = VECTOR('',#38206,7.) ;
#9038 = VECTOR('',#38207,2.) ;
#9039 = VECTOR('',#38208,7.) ;
#9040 = VECTOR('',#38217,10.) ;
#9041 = VECTOR('',#38218,10.) ;
#9042 = VECTOR('',#38219,10.) ;
#9043 = VECTOR('',#38220,10.) ;
#9044 = VECTOR('',#38223,10.) ;
#9045 = VECTOR('',#38224,10.) ;
#9046 = VECTOR('',#38225,10.) ;
#9047 = VECTOR('',#38226,10.) ;
#9048 = VECTOR('',#38227,10.) ;
#9049 = VECTOR('',#38228,10.) ;
#9050 = VECTOR('',#38233,141.) ;
#9051 = VECTOR('',#38236,141.) ;
#9052 = VECTOR('',#38243,194.3) ;
#9053 = VECTOR('',#38248,0.5) ;
#9054 = VECTOR('',#38253,10.) ;
#9055 = VECTOR('',#38256,10.) ;
#9056 = VECTOR('',#38257,10.) ;
#9057 = VECTOR('',#38258,10.) ;
#9058 = VECTOR('',#38261,10.) ;
#9059 = VECTOR('',#38262,10.) ;
#9060 = VECTOR('',#38263,10.) ;
#9061 = VECTOR('',#38266,10.) ;
#9062 = VECTOR('',#38267,10.) ;
#9063 = VECTOR('',#38270,10.) ;
#9064 = VECTOR('',#38271,10.) ;
#9065 = VECTOR('',#38272,10.) ;
#9066 = VECTOR('',#38275,10.) ;
#9067 = VECTOR('',#38276,10.) ;
#9068 = VECTOR('',#38279,10.) ;
#9069 = VECTOR('',#38284,10.) ;
#9070 = VECTOR('',#38287,10.) ;
#9071 = VECTOR('',#38288,10.) ;
#9072 = VECTOR('',#38289,10.) ;
#9073 = VECTOR('',#38292,10.) ;
#9074 = VECTOR('',#38297,10.) ;
#9075 = VECTOR('',#38302,1.25) ;
#9076 = VECTOR('',#38303,10.) ;
#9077 = VECTOR('',#38304,0.75) ;
#9078 = VECTOR('',#38311,10.) ;
#9079 = VECTOR('',#38322,10.) ;
#9080 = VECTOR('',#38333,10.) ;
#9081 = VECTOR('',#38336,1.25) ;
#9082 = VECTOR('',#38337,10.) ;
#9083 = VECTOR('',#38338,1.25) ;
#9084 = VECTOR('',#38341,0.5) ;
#9085 = VECTOR('',#38346,10.) ;
#9086 = VECTOR('',#38347,10.) ;
#9087 = VECTOR('',#38350,1.25) ;
#9088 = VECTOR('',#38355,0.75) ;
#9089 = VECTOR('',#38356,10.) ;
#9090 = VECTOR('',#38363,10.) ;
#9091 = VECTOR('',#38374,10.) ;
#9092 = VECTOR('',#38385,10.) ;
#9093 = VECTOR('',#38388,1.25) ;
#9094 = VECTOR('',#38389,10.) ;
#9095 = VECTOR('',#38390,10.) ;
#9096 = VECTOR('',#38393,0.5) ;
#9097 = VECTOR('',#38398,10.) ;
#9098 = VECTOR('',#38399,10.) ;
#9099 = VECTOR('',#38402,1.25) ;
#9100 = VECTOR('',#38407,10.) ;
#9101 = VECTOR('',#38408,10.) ;
#9102 = VECTOR('',#38411,9.99999999999998) ;
#9103 = VECTOR('',#38412,1000.) ;
#9104 = VECTOR('',#38413,9.99999999999998) ;
#9105 = VECTOR('',#38414,1000.) ;
#9106 = VECTOR('',#38417,9.99999999999998) ;
#9107 = VECTOR('',#38418,9.99999999999998) ;
#9108 = VECTOR('',#38419,1000.) ;
#9109 = VECTOR('',#38422,10.) ;
#9110 = VECTOR('',#38423,10.) ;
#9111 = VECTOR('',#38424,1000.) ;
#9112 = VECTOR('',#38427,10.) ;
#9113 = VECTOR('',#38428,10.) ;
#9114 = VECTOR('',#38429,1000.) ;
#9115 = VECTOR('',#38432,10.) ;
#9116 = VECTOR('',#38433,1000.) ;
#9117 = VECTOR('',#38434,10.) ;
#9118 = VECTOR('',#38437,10.) ;
#9119 = VECTOR('',#38438,10.) ;
#9120 = VECTOR('',#38441,9.99999999999998) ;
#9121 = VECTOR('',#38442,1000.) ;
#9122 = VECTOR('',#38443,9.99999999999998) ;
#9123 = VECTOR('',#38444,1000.) ;
#9124 = VECTOR('',#38447,9.99999999999998) ;
#9125 = VECTOR('',#38448,9.99999999999998) ;
#9126 = VECTOR('',#38449,1000.) ;
#9127 = VECTOR('',#38452,10.) ;
#9128 = VECTOR('',#38453,10.) ;
#9129 = VECTOR('',#38454,1000.) ;
#9130 = VECTOR('',#38457,10.) ;
#9131 = VECTOR('',#38458,10.) ;
#9132 = VECTOR('',#38459,1000.) ;
#9133 = VECTOR('',#38462,10.) ;
#9134 = VECTOR('',#38463,1000.) ;
#9135 = VECTOR('',#38464,10.) ;
#9136 = VECTOR('',#38467,10.) ;
#9137 = VECTOR('',#38468,10.) ;
#9138 = VECTOR('',#38479,10.) ;
#9139 = VECTOR('',#38486,10.) ;
#9140 = VECTOR('',#38489,10.) ;
#9141 = VECTOR('',#38498,10.) ;
#9142 = VECTOR('',#38503,10.) ;
#9143 = VECTOR('',#38508,2.5) ;
#9144 = VECTOR('',#38509,2.) ;
#9145 = VECTOR('',#38510,4.) ;
#9146 = VECTOR('',#38511,2.5) ;
#9147 = VECTOR('',#38516,2.20000000000002) ;
#9148 = VECTOR('',#38519,1.65) ;
#9149 = VECTOR('',#38524,2.2) ;
#9150 = VECTOR('',#38527,1.65) ;
#9151 = VECTOR('',#38532,2.2) ;
#9152 = VECTOR('',#38535,1.65) ;
#9153 = VECTOR('',#38538,10.) ;
#9154 = VECTOR('',#38543,10.) ;
#9155 = VECTOR('',#38550,1.75) ;
#9156 = VECTOR('',#38557,2.25) ;
#9157 = VECTOR('',#38564,2.) ;
#9158 = VECTOR('',#38567,2.) ;
#9159 = VECTOR('',#38572,2.) ;
#9160 = VECTOR('',#38575,2.) ;
#9161 = VECTOR('',#38580,2.) ;
#9162 = VECTOR('',#38583,2.) ;
#9163 = VECTOR('',#38588,2.) ;
#9164 = VECTOR('',#38591,2.) ;
#9165 = VECTOR('',#38598,2.) ;
#9166 = VECTOR('',#38603,2.) ;
#9167 = VECTOR('',#38606,2.) ;
#9168 = VECTOR('',#38619,12.35000000085) ;
#9169 = VECTOR('',#38622,2.5) ;
#9170 = VECTOR('',#38623,2.5) ;
#9171 = VECTOR('',#38626,2.5) ;
#9172 = VECTOR('',#38627,2.5) ;
#9173 = VECTOR('',#38630,2.5) ;
#9174 = VECTOR('',#38631,2.5) ;
#9175 = VECTOR('',#38636,2.5) ;
#9176 = VECTOR('',#38639,2.5) ;
#9177 = VECTOR('',#38640,2.5) ;
#9178 = VECTOR('',#38643,2.5) ;
#9179 = VECTOR('',#38646,2.5) ;
#9180 = VECTOR('',#38651,2.5) ;
#9181 = VECTOR('',#38652,2.5) ;
#9182 = VECTOR('',#38655,2.5) ;
#9183 = VECTOR('',#38658,2.5) ;
#9184 = VECTOR('',#38663,2.5) ;
#9185 = VECTOR('',#38664,2.5) ;
#9186 = VECTOR('',#38667,2.5) ;
#9187 = VECTOR('',#38670,2.5) ;
#9188 = VECTOR('',#38679,2.5) ;
#9189 = VECTOR('',#38680,2.5) ;
#9190 = VECTOR('',#38683,2.5) ;
#9191 = VECTOR('',#38686,2.5) ;
#9192 = VECTOR('',#38691,2.5) ;
#9193 = VECTOR('',#38692,4.) ;
#9194 = VECTOR('',#38697,2.33) ;
#9195 = VECTOR('',#38698,3.83) ;
#9196 = VECTOR('',#38705,3.98) ;
#9197 = VECTOR('',#38708,4.) ;
#9198 = VECTOR('',#38713,2.33) ;
#9199 = VECTOR('',#38714,3.83) ;
#9200 = VECTOR('',#38719,41.3) ;
#9201 = VECTOR('',#38726,23.00000000085) ;
#9202 = VECTOR('',#38735,12.35) ;
#9203 = VECTOR('',#38738,2.33) ;
#9204 = VECTOR('',#38739,3.83) ;
#9205 = VECTOR('',#38742,2.33) ;
#9206 = VECTOR('',#38743,3.83) ;
#9207 = VECTOR('',#38746,4.) ;
#9208 = VECTOR('',#38747,2.5) ;
#9209 = VECTOR('',#38750,4.) ;
#9210 = VECTOR('',#38751,2.5) ;
#9211 = VECTOR('',#38754,4.45) ;
#9212 = VECTOR('',#38755,10.) ;
#9213 = VECTOR('',#38756,10.) ;
#9214 = VECTOR('',#38757,87.4) ;
#9215 = VECTOR('',#38758,10.) ;
#9216 = VECTOR('',#38759,10.) ;
#9217 = VECTOR('',#38760,12.35000000085) ;
#9218 = VECTOR('',#38763,79.40000000085) ;
#9219 = VECTOR('',#38766,0.9) ;
#9220 = VECTOR('',#38767,7.) ;
#9221 = VECTOR('',#38780,10.) ;
#9222 = VECTOR('',#38787,1.75) ;
#9223 = VECTOR('',#38794,2.25) ;
#9224 = VECTOR('',#38799,1.75) ;
#9225 = VECTOR('',#38806,2.25) ;
#9226 = VECTOR('',#38811,1.75) ;
#9227 = VECTOR('',#38818,2.25) ;
#9228 = VECTOR('',#38823,1.75) ;
#9229 = VECTOR('',#38830,2.25) ;
#9230 = VECTOR('',#38833,10.) ;
#9231 = VECTOR('',#38834,2.5) ;
#9232 = VECTOR('',#38835,2.5) ;
#9233 = VECTOR('',#38846,2.5) ;
#9234 = VECTOR('',#38849,3.83) ;
#9235 = VECTOR('',#38850,2.33) ;
#9236 = VECTOR('',#38853,2.33) ;
#9237 = VECTOR('',#38854,3.83) ;
#9238 = VECTOR('',#38855,2.5) ;
#9239 = VECTOR('',#38858,2.5) ;
#9240 = VECTOR('',#38859,2.5) ;
#9241 = VECTOR('',#38862,2.5) ;
#9242 = VECTOR('',#38865,2.5) ;
#9243 = VECTOR('',#38870,2.25) ;
#9244 = VECTOR('',#38871,7.) ;
#9245 = VECTOR('',#38872,2.25) ;
#9246 = VECTOR('',#38875,2.5) ;
#9247 = VECTOR('',#38876,2.5) ;
#9248 = VECTOR('',#38889,2.5) ;
#9249 = VECTOR('',#38890,2.5) ;
#9250 = VECTOR('',#38893,2.5) ;
#9251 = VECTOR('',#38896,2.5) ;
#9252 = VECTOR('',#38901,2.5) ;
#9253 = VECTOR('',#38902,2.5) ;
#9254 = VECTOR('',#38905,2.5) ;
#9255 = VECTOR('',#38908,2.5) ;
#9256 = VECTOR('',#38927,194.3) ;
#9257 = VECTOR('',#38932,3.83) ;
#9258 = VECTOR('',#38933,2.33) ;
#9259 = VECTOR('',#38938,3.98) ;
#9260 = VECTOR('',#38941,2.33) ;
#9261 = VECTOR('',#38942,3.83) ;
#9262 = VECTOR('',#38953,31.) ;
#9263 = VECTOR('',#38954,1.65) ;
#9264 = VECTOR('',#38955,1.65) ;
#9265 = VECTOR('',#38960,1.65) ;
#9266 = VECTOR('',#38965,2.2) ;
#9267 = VECTOR('',#38968,10.) ;
#9268 = VECTOR('',#38969,10.) ;
#9269 = VECTOR('',#38970,10.) ;
#9270 = VECTOR('',#38973,10.) ;
#9271 = VECTOR('',#38974,10.) ;
#9272 = VECTOR('',#38975,10.) ;
#9273 = VECTOR('',#38978,10.) ;
#9274 = VECTOR('',#38979,10.) ;
#9275 = VECTOR('',#38980,10.) ;
#9276 = VECTOR('',#38983,10.) ;
#9277 = VECTOR('',#38984,10.) ;
#9278 = VECTOR('',#38985,10.) ;
#9279 = VECTOR('',#39038,10.) ;
#9280 = VECTOR('',#39049,10.) ;
#9281 = VECTOR('',#39056,10.) ;
#9282 = VECTOR('',#39061,10.) ;
#9283 = VECTOR('',#39066,10.) ;
#9284 = VECTOR('',#39071,10.) ;
#9285 = VECTOR('',#39084,10.) ;
#9286 = VECTOR('',#39087,10.) ;
#9287 = VECTOR('',#39100,10.) ;
#9288 = VECTOR('',#39101,10.) ;
#9289 = VECTOR('',#39102,9.99999999999998) ;
#9290 = VECTOR('',#39103,9.99999999999998) ;
#9291 = VECTOR('',#39104,10.) ;
#9292 = VECTOR('',#39105,10.) ;
#9293 = VECTOR('',#39106,10.) ;
#9294 = VECTOR('',#39107,10.) ;
#9295 = VECTOR('',#39108,9.99999999999998) ;
#9296 = VECTOR('',#39109,9.99999999999998) ;
#9297 = VECTOR('',#39110,10.) ;
#9298 = VECTOR('',#39111,10.) ;
#9299 = VECTOR('',#39112,10.) ;
#9300 = VECTOR('',#39113,10.) ;
#9301 = VECTOR('',#39114,9.99999999999998) ;
#9302 = VECTOR('',#39115,9.99999999999998) ;
#9303 = VECTOR('',#39116,10.) ;
#9304 = VECTOR('',#39117,10.) ;
#9305 = VECTOR('',#39120,10.) ;
#9306 = VECTOR('',#39121,1000.) ;
#9307 = VECTOR('',#39122,1000.) ;
#9308 = VECTOR('',#39125,10.) ;
#9309 = VECTOR('',#39126,1000.) ;
#9310 = VECTOR('',#39129,10.) ;
#9311 = VECTOR('',#39130,1000.) ;
#9312 = VECTOR('',#39133,10.) ;
#9313 = VECTOR('',#39134,1000.) ;
#9314 = VECTOR('',#39137,9.99999999999998) ;
#9315 = VECTOR('',#39138,1000.) ;
#9316 = VECTOR('',#39141,9.99999999999998) ;
#9317 = VECTOR('',#39144,10.) ;
#9318 = VECTOR('',#39145,1000.) ;
#9319 = VECTOR('',#39146,1000.) ;
#9320 = VECTOR('',#39149,10.) ;
#9321 = VECTOR('',#39150,1000.) ;
#9322 = VECTOR('',#39153,10.) ;
#9323 = VECTOR('',#39154,1000.) ;
#9324 = VECTOR('',#39157,10.) ;
#9325 = VECTOR('',#39158,1000.) ;
#9326 = VECTOR('',#39161,9.99999999999998) ;
#9327 = VECTOR('',#39162,1000.) ;
#9328 = VECTOR('',#39165,9.99999999999998) ;
#9329 = VECTOR('',#39168,10.) ;
#9330 = VECTOR('',#39169,10.) ;
#9331 = VECTOR('',#39170,10.) ;
#9332 = VECTOR('',#39171,9.99999999999998) ;
#9333 = VECTOR('',#39172,9.99999999999998) ;
#9334 = VECTOR('',#39173,10.) ;
#9335 = VECTOR('',#39176,1000.) ;
#9336 = VECTOR('',#39177,1000.) ;
#9337 = VECTOR('',#39180,1000.) ;
#9338 = VECTOR('',#39183,1000.) ;
#9339 = VECTOR('',#39186,1000.) ;
#9340 = VECTOR('',#39189,1000.) ;
#9341 = VECTOR('',#39208,10.) ;
#9342 = VECTOR('',#39209,10.) ;
#9343 = VECTOR('',#39210,10.) ;
#9344 = VECTOR('',#39211,10.) ;
#9345 = VECTOR('',#39214,10.) ;
#9346 = VECTOR('',#39215,10.) ;
#9347 = VECTOR('',#39216,10.) ;
#9348 = VECTOR('',#39219,10.) ;
#9349 = VECTOR('',#39220,10.) ;
#9350 = VECTOR('',#39221,10.) ;
#9351 = VECTOR('',#39224,10.) ;
#9352 = VECTOR('',#39227,10.) ;
#9353 = VECTOR('',#39228,10.) ;
#9354 = VECTOR('',#39229,10.) ;
#9355 = VECTOR('',#39230,10.) ;
#9356 = VECTOR('',#39233,10.) ;
#9357 = VECTOR('',#39234,10.) ;
#9358 = VECTOR('',#39235,10.) ;
#9359 = VECTOR('',#39238,10.) ;
#9360 = VECTOR('',#39239,10.) ;
#9361 = VECTOR('',#39240,10.) ;
#9362 = VECTOR('',#39243,10.) ;
#9363 = VECTOR('',#39246,10.) ;
#9364 = VECTOR('',#39247,10.) ;
#9365 = VECTOR('',#39248,10.) ;
#9366 = VECTOR('',#39249,10.) ;
#9367 = VECTOR('',#39252,10.) ;
#9368 = VECTOR('',#39253,10.) ;
#9369 = VECTOR('',#39254,10.) ;
#9370 = VECTOR('',#39257,10.) ;
#9371 = VECTOR('',#39258,10.) ;
#9372 = VECTOR('',#39259,10.) ;
#9373 = VECTOR('',#39262,10.) ;
#9374 = VECTOR('',#39265,10.) ;
#9375 = VECTOR('',#39266,10.) ;
#9376 = VECTOR('',#39267,10.) ;
#9377 = VECTOR('',#39268,10.) ;
#9378 = VECTOR('',#39271,10.) ;
#9379 = VECTOR('',#39272,10.) ;
#9380 = VECTOR('',#39273,10.) ;
#9381 = VECTOR('',#39276,10.) ;
#9382 = VECTOR('',#39277,10.) ;
#9383 = VECTOR('',#39278,10.) ;
#9384 = VECTOR('',#39281,10.) ;
#9385 = VECTOR('',#39284,10.) ;
#9386 = VECTOR('',#39285,10.) ;
#9387 = VECTOR('',#39286,10.) ;
#9388 = VECTOR('',#39287,10.) ;
#9389 = VECTOR('',#39290,10.) ;
#9390 = VECTOR('',#39291,10.) ;
#9391 = VECTOR('',#39292,10.) ;
#9392 = VECTOR('',#39295,10.) ;
#9393 = VECTOR('',#39296,10.) ;
#9394 = VECTOR('',#39297,10.) ;
#9395 = VECTOR('',#39300,10.) ;
#9396 = VECTOR('',#39303,10.) ;
#9397 = VECTOR('',#39304,10.) ;
#9398 = VECTOR('',#39305,10.) ;
#9399 = VECTOR('',#39306,10.) ;
#9400 = VECTOR('',#39309,10.) ;
#9401 = VECTOR('',#39310,10.) ;
#9402 = VECTOR('',#39311,10.) ;
#9403 = VECTOR('',#39314,10.) ;
#9404 = VECTOR('',#39315,10.) ;
#9405 = VECTOR('',#39316,10.) ;
#9406 = VECTOR('',#39319,10.) ;
#9407 = VECTOR('',#39322,10.) ;
#9408 = VECTOR('',#39323,10.) ;
#9409 = VECTOR('',#39324,10.) ;
#9410 = VECTOR('',#39325,10.) ;
#9411 = VECTOR('',#39328,10.) ;
#9412 = VECTOR('',#39329,10.) ;
#9413 = VECTOR('',#39330,10.) ;
#9414 = VECTOR('',#39333,10.) ;
#9415 = VECTOR('',#39334,10.) ;
#9416 = VECTOR('',#39335,10.) ;
#9417 = VECTOR('',#39338,10.) ;
#9418 = VECTOR('',#39341,10.) ;
#9419 = VECTOR('',#39342,10.) ;
#9420 = VECTOR('',#39343,10.) ;
#9421 = VECTOR('',#39344,10.) ;
#9422 = VECTOR('',#39347,10.) ;
#9423 = VECTOR('',#39348,10.) ;
#9424 = VECTOR('',#39349,10.) ;
#9425 = VECTOR('',#39352,10.) ;
#9426 = VECTOR('',#39353,10.) ;
#9427 = VECTOR('',#39354,10.) ;
#9428 = VECTOR('',#39357,10.) ;
#9429 = VECTOR('',#39360,10.) ;
#9430 = VECTOR('',#39361,10.) ;
#9431 = VECTOR('',#39362,10.) ;
#9432 = VECTOR('',#39363,10.) ;
#9433 = VECTOR('',#39366,10.) ;
#9434 = VECTOR('',#39367,10.) ;
#9435 = VECTOR('',#39368,10.) ;
#9436 = VECTOR('',#39371,10.) ;
#9437 = VECTOR('',#39372,10.) ;
#9438 = VECTOR('',#39373,10.) ;
#9439 = VECTOR('',#39376,10.) ;
#9440 = VECTOR('',#39379,10.) ;
#9441 = VECTOR('',#39380,10.) ;
#9442 = VECTOR('',#39381,10.) ;
#9443 = VECTOR('',#39382,10.) ;
#9444 = VECTOR('',#39383,10.) ;
#9445 = VECTOR('',#39384,10.) ;
#9446 = VECTOR('',#39385,10.) ;
#9447 = VECTOR('',#39386,13.3) ;
#9448 = VECTOR('',#39387,87.07601714263) ;
#9449 = VECTOR('',#39388,10.) ;
#9450 = VECTOR('',#39389,10.) ;
#9451 = VECTOR('',#39390,10.) ;
#9452 = VECTOR('',#39391,87.07601714263) ;
#9453 = VECTOR('',#39392,10.) ;
#9454 = VECTOR('',#39393,10.) ;
#9455 = VECTOR('',#39394,10.) ;
#9456 = VECTOR('',#39395,87.07601714263) ;
#9457 = VECTOR('',#39396,10.) ;
#9458 = VECTOR('',#39397,10.) ;
#9459 = VECTOR('',#39398,10.) ;
#9460 = VECTOR('',#39399,87.07601714263) ;
#9461 = VECTOR('',#39400,10.) ;
#9462 = VECTOR('',#39401,10.) ;
#9463 = VECTOR('',#39402,10.) ;
#9464 = VECTOR('',#39403,87.07601714263) ;
#9465 = VECTOR('',#39404,10.) ;
#9466 = VECTOR('',#39405,10.) ;
#9467 = VECTOR('',#39406,10.) ;
#9468 = VECTOR('',#39407,87.07601714263) ;
#9469 = VECTOR('',#39408,10.) ;
#9470 = VECTOR('',#39409,10.) ;
#9471 = VECTOR('',#39410,10.) ;
#9472 = VECTOR('',#39411,87.07601714263) ;
#9473 = VECTOR('',#39412,10.) ;
#9474 = VECTOR('',#39413,10.) ;
#9475 = VECTOR('',#39414,10.) ;
#9476 = VECTOR('',#39415,87.07601714263) ;
#9477 = VECTOR('',#39416,10.) ;
#9478 = VECTOR('',#39417,10.) ;
#9479 = VECTOR('',#39418,10.) ;
#9480 = VECTOR('',#39419,87.07601714263) ;
#9481 = VECTOR('',#39420,10.) ;
#9482 = VECTOR('',#39421,10.) ;
#9483 = VECTOR('',#39422,10.) ;
#9484 = VECTOR('',#39423,87.07601714263) ;
#9485 = VECTOR('',#39424,10.) ;
#9486 = VECTOR('',#39425,10.) ;
#9487 = VECTOR('',#39426,10.) ;
#9488 = VECTOR('',#39427,10.) ;
#9489 = VECTOR('',#39440,1.5) ;
#9490 = VECTOR('',#39443,10.) ;
#9491 = VECTOR('',#39444,10.) ;
#9492 = VECTOR('',#39445,10.) ;
#9493 = VECTOR('',#39446,10.) ;
#9494 = VECTOR('',#39447,10.) ;
#9495 = VECTOR('',#39450,10.) ;
#9496 = VECTOR('',#39453,10.) ;
#9497 = VECTOR('',#39456,10.) ;
#9498 = VECTOR('',#39471,1.5) ;
#9499 = VECTOR('',#39474,10.) ;
#9500 = VECTOR('',#39475,10.) ;
#9501 = VECTOR('',#39476,10.) ;
#9502 = VECTOR('',#39477,10.) ;
#9503 = VECTOR('',#39478,10.) ;
#9504 = VECTOR('',#39481,10.) ;
#9505 = VECTOR('',#39484,10.) ;
#9506 = VECTOR('',#39487,10.) ;
#9507 = VECTOR('',#39502,1.5) ;
#9508 = VECTOR('',#39505,10.) ;
#9509 = VECTOR('',#39506,10.) ;
#9510 = VECTOR('',#39507,10.) ;
#9511 = VECTOR('',#39508,10.) ;
#9512 = VECTOR('',#39509,10.) ;
#9513 = VECTOR('',#39512,10.) ;
#9514 = VECTOR('',#39515,10.) ;
#9515 = VECTOR('',#39518,10.) ;
#9516 = VECTOR('',#39533,1.5) ;
#9517 = VECTOR('',#39536,10.) ;
#9518 = VECTOR('',#39537,10.) ;
#9519 = VECTOR('',#39538,10.) ;
#9520 = VECTOR('',#39539,10.) ;
#9521 = VECTOR('',#39540,10.) ;
#9522 = VECTOR('',#39543,10.) ;
#9523 = VECTOR('',#39546,10.) ;
#9524 = VECTOR('',#39549,10.) ;
#9525 = VECTOR('',#39564,1.5) ;
#9526 = VECTOR('',#39567,10.) ;
#9527 = VECTOR('',#39568,10.) ;
#9528 = VECTOR('',#39569,10.) ;
#9529 = VECTOR('',#39570,10.) ;
#9530 = VECTOR('',#39571,10.) ;
#9531 = VECTOR('',#39574,10.) ;
#9532 = VECTOR('',#39577,10.) ;
#9533 = VECTOR('',#39580,10.) ;
#9534 = VECTOR('',#39595,1.5) ;
#9535 = VECTOR('',#39598,10.) ;
#9536 = VECTOR('',#39599,10.) ;
#9537 = VECTOR('',#39600,10.) ;
#9538 = VECTOR('',#39601,10.) ;
#9539 = VECTOR('',#39602,10.) ;
#9540 = VECTOR('',#39605,10.) ;
#9541 = VECTOR('',#39608,10.) ;
#9542 = VECTOR('',#39611,10.) ;
#9543 = VECTOR('',#39626,1.5) ;
#9544 = VECTOR('',#39629,10.) ;
#9545 = VECTOR('',#39630,10.) ;
#9546 = VECTOR('',#39631,10.) ;
#9547 = VECTOR('',#39632,10.) ;
#9548 = VECTOR('',#39633,10.) ;
#9549 = VECTOR('',#39636,10.) ;
#9550 = VECTOR('',#39639,10.) ;
#9551 = VECTOR('',#39642,10.) ;
#9552 = VECTOR('',#39657,1.5) ;
#9553 = VECTOR('',#39660,10.) ;
#9554 = VECTOR('',#39661,10.) ;
#9555 = VECTOR('',#39662,10.) ;
#9556 = VECTOR('',#39663,10.) ;
#9557 = VECTOR('',#39664,10.) ;
#9558 = VECTOR('',#39667,10.) ;
#9559 = VECTOR('',#39670,10.) ;
#9560 = VECTOR('',#39673,10.) ;
#9561 = VECTOR('',#39686,10.) ;
#9562 = VECTOR('',#39687,10.) ;
#9563 = VECTOR('',#39688,10.) ;
#9564 = VECTOR('',#39689,10.) ;
#9565 = VECTOR('',#39690,10.) ;
#9566 = VECTOR('',#39693,10.) ;
#9567 = VECTOR('',#39696,10.) ;
#9568 = VECTOR('',#39699,10.) ;
#9569 = VECTOR('',#39706,1.5) ;
#9570 = VECTOR('',#39743,10.) ;
#9571 = VECTOR('',#39756,10.) ;
#9572 = VECTOR('',#39767,10.) ;
#9573 = VECTOR('',#39778,10.) ;
#9574 = VECTOR('',#39785,10.) ;
#9575 = VECTOR('',#39788,10.) ;
#9576 = VECTOR('',#39791,10.) ;
#9577 = VECTOR('',#39794,10.) ;
#9578 = VECTOR('',#39795,10.) ;
#9579 = VECTOR('',#39796,10.) ;
#9580 = VECTOR('',#39797,10.) ;
#9581 = VECTOR('',#39798,10.) ;
#9582 = VECTOR('',#39803,10.) ;
#9583 = VECTOR('',#39808,10.) ;
#9584 = VECTOR('',#39809,10.) ;
#9585 = VECTOR('',#39814,10.) ;
#9586 = VECTOR('',#39827,10.) ;
#9587 = VECTOR('',#39838,10.) ;
#9588 = VECTOR('',#39849,10.) ;
#9589 = VECTOR('',#39856,10.) ;
#9590 = VECTOR('',#39859,10.) ;
#9591 = VECTOR('',#39862,10.) ;
#9592 = VECTOR('',#39865,10.) ;
#9593 = VECTOR('',#39866,10.) ;
#9594 = VECTOR('',#39867,10.) ;
#9595 = VECTOR('',#39868,10.) ;
#9596 = VECTOR('',#39869,10.) ;
#9597 = VECTOR('',#39874,10.) ;
#9598 = VECTOR('',#39879,10.) ;
#9599 = VECTOR('',#39880,10.) ;
#9600 = VECTOR('',#39885,10.) ;
#9601 = VECTOR('',#39898,10.) ;
#9602 = VECTOR('',#39909,10.) ;
#9603 = VECTOR('',#39920,10.) ;
#9604 = VECTOR('',#39927,10.) ;
#9605 = VECTOR('',#39930,10.) ;
#9606 = VECTOR('',#39933,10.) ;
#9607 = VECTOR('',#39936,10.) ;
#9608 = VECTOR('',#39937,10.) ;
#9609 = VECTOR('',#39938,10.) ;
#9610 = VECTOR('',#39939,10.) ;
#9611 = VECTOR('',#39940,10.) ;
#9612 = VECTOR('',#39945,10.) ;
#9613 = VECTOR('',#39950,10.) ;
#9614 = VECTOR('',#39951,10.) ;
#9615 = VECTOR('',#39956,10.) ;
#9616 = VECTOR('',#39969,10.) ;
#9617 = VECTOR('',#39980,10.) ;
#9618 = VECTOR('',#39991,10.) ;
#9619 = VECTOR('',#39998,10.) ;
#9620 = VECTOR('',#40001,10.) ;
#9621 = VECTOR('',#40004,10.) ;
#9622 = VECTOR('',#40007,10.) ;
#9623 = VECTOR('',#40008,10.) ;
#9624 = VECTOR('',#40009,10.) ;
#9625 = VECTOR('',#40010,10.) ;
#9626 = VECTOR('',#40011,10.) ;
#9627 = VECTOR('',#40016,10.) ;
#9628 = VECTOR('',#40021,10.) ;
#9629 = VECTOR('',#40022,10.) ;
#9630 = VECTOR('',#40027,10.) ;
#9631 = VECTOR('',#40040,10.) ;
#9632 = VECTOR('',#40051,10.) ;
#9633 = VECTOR('',#40062,10.) ;
#9634 = VECTOR('',#40069,10.) ;
#9635 = VECTOR('',#40072,10.) ;
#9636 = VECTOR('',#40075,10.) ;
#9637 = VECTOR('',#40078,10.) ;
#9638 = VECTOR('',#40079,10.) ;
#9639 = VECTOR('',#40080,10.) ;
#9640 = VECTOR('',#40081,10.) ;
#9641 = VECTOR('',#40082,10.) ;
#9642 = VECTOR('',#40087,10.) ;
#9643 = VECTOR('',#40092,10.) ;
#9644 = VECTOR('',#40093,10.) ;
#9645 = VECTOR('',#40098,10.) ;
#9646 = VECTOR('',#40111,10.) ;
#9647 = VECTOR('',#40122,10.) ;
#9648 = VECTOR('',#40133,10.) ;
#9649 = VECTOR('',#40140,10.) ;
#9650 = VECTOR('',#40143,10.) ;
#9651 = VECTOR('',#40146,10.) ;
#9652 = VECTOR('',#40149,10.) ;
#9653 = VECTOR('',#40150,10.) ;
#9654 = VECTOR('',#40151,10.) ;
#9655 = VECTOR('',#40152,10.) ;
#9656 = VECTOR('',#40153,10.) ;
#9657 = VECTOR('',#40158,10.) ;
#9658 = VECTOR('',#40163,10.) ;
#9659 = VECTOR('',#40164,10.) ;
#9660 = VECTOR('',#40169,10.) ;
#9661 = VECTOR('',#40182,10.) ;
#9662 = VECTOR('',#40193,10.) ;
#9663 = VECTOR('',#40204,10.) ;
#9664 = VECTOR('',#40211,10.) ;
#9665 = VECTOR('',#40214,10.) ;
#9666 = VECTOR('',#40217,10.) ;
#9667 = VECTOR('',#40220,10.) ;
#9668 = VECTOR('',#40221,10.) ;
#9669 = VECTOR('',#40222,10.) ;
#9670 = VECTOR('',#40223,10.) ;
#9671 = VECTOR('',#40224,10.) ;
#9672 = VECTOR('',#40229,10.) ;
#9673 = VECTOR('',#40234,10.) ;
#9674 = VECTOR('',#40235,10.) ;
#9675 = VECTOR('',#40240,10.) ;
#9676 = VECTOR('',#40253,10.) ;
#9677 = VECTOR('',#40264,10.) ;
#9678 = VECTOR('',#40275,10.) ;
#9679 = VECTOR('',#40282,10.) ;
#9680 = VECTOR('',#40285,10.) ;
#9681 = VECTOR('',#40288,10.) ;
#9682 = VECTOR('',#40291,10.) ;
#9683 = VECTOR('',#40292,10.) ;
#9684 = VECTOR('',#40293,10.) ;
#9685 = VECTOR('',#40294,10.) ;
#9686 = VECTOR('',#40295,10.) ;
#9687 = VECTOR('',#40300,10.) ;
#9688 = VECTOR('',#40305,10.) ;
#9689 = VECTOR('',#40306,10.) ;
#9690 = VECTOR('',#40311,10.) ;
#9691 = VECTOR('',#40324,10.) ;
#9692 = VECTOR('',#40335,10.) ;
#9693 = VECTOR('',#40346,10.) ;
#9694 = VECTOR('',#40353,10.) ;
#9695 = VECTOR('',#40356,10.) ;
#9696 = VECTOR('',#40359,10.) ;
#9697 = VECTOR('',#40360,10.) ;
#9698 = VECTOR('',#40361,10.) ;
#9699 = VECTOR('',#40364,10.) ;
#9700 = VECTOR('',#40367,10.) ;
#9701 = VECTOR('',#40368,10.) ;
#9702 = VECTOR('',#40371,10.) ;
#9703 = VECTOR('',#40376,10.) ;
#9704 = VECTOR('',#40377,10.) ;
#9705 = VECTOR('',#40382,10.) ;
#9706 = VECTOR('',#40385,10.) ;
#9707 = VECTOR('',#40398,10.) ;
#9708 = VECTOR('',#40399,10.) ;
#9709 = VECTOR('',#40412,10.) ;
#9710 = VECTOR('',#40413,10.) ;
#9711 = VECTOR('',#40426,10.) ;
#9712 = VECTOR('',#40427,10.) ;
#9713 = VECTOR('',#40436,10.) ;
#9714 = VECTOR('',#40439,10.) ;
#9715 = VECTOR('',#40442,10.) ;
#9716 = VECTOR('',#40443,10.) ;
#9717 = VECTOR('',#40446,10.) ;
#9718 = VECTOR('',#40451,10.) ;
#9719 = VECTOR('',#40452,10.) ;
#9720 = VECTOR('',#40457,10.) ;
#9721 = VECTOR('',#40460,10.) ;
#9722 = VECTOR('',#40473,10.) ;
#9723 = VECTOR('',#40474,10.) ;
#9724 = VECTOR('',#40487,10.) ;
#9725 = VECTOR('',#40488,10.) ;
#9726 = VECTOR('',#40501,10.) ;
#9727 = VECTOR('',#40502,10.) ;
#9728 = VECTOR('',#40511,10.) ;
#9729 = VECTOR('',#40514,10.) ;
#9730 = VECTOR('',#40517,10.) ;
#9731 = VECTOR('',#40518,10.) ;
#9732 = VECTOR('',#40521,10.) ;
#9733 = VECTOR('',#40526,10.) ;
#9734 = VECTOR('',#40527,10.) ;
#9735 = VECTOR('',#40532,10.) ;
#9736 = VECTOR('',#40535,10.) ;
#9737 = VECTOR('',#40548,10.) ;
#9738 = VECTOR('',#40549,10.) ;
#9739 = VECTOR('',#40562,10.) ;
#9740 = VECTOR('',#40563,10.) ;
#9741 = VECTOR('',#40576,10.) ;
#9742 = VECTOR('',#40577,10.) ;
#9743 = VECTOR('',#40586,10.) ;
#9744 = VECTOR('',#40589,10.) ;
#9745 = VECTOR('',#40592,10.) ;
#9746 = VECTOR('',#40593,10.) ;
#9747 = VECTOR('',#40596,10.) ;
#9748 = VECTOR('',#40601,10.) ;
#9749 = VECTOR('',#40602,10.) ;
#9750 = VECTOR('',#40607,10.) ;
#9751 = VECTOR('',#40610,10.) ;
#9752 = VECTOR('',#40623,10.) ;
#9753 = VECTOR('',#40624,10.) ;
#9754 = VECTOR('',#40637,10.) ;
#9755 = VECTOR('',#40638,10.) ;
#9756 = VECTOR('',#40651,10.) ;
#9757 = VECTOR('',#40652,10.) ;
#9758 = VECTOR('',#40661,10.) ;
#9759 = VECTOR('',#40664,10.) ;
#9760 = VECTOR('',#40667,10.) ;
#9761 = VECTOR('',#40668,10.) ;
#9762 = VECTOR('',#40671,10.) ;
#9763 = VECTOR('',#40676,10.) ;
#9764 = VECTOR('',#40677,10.) ;
#9765 = VECTOR('',#40682,10.) ;
#9766 = VECTOR('',#40685,10.) ;
#9767 = VECTOR('',#40698,10.) ;
#9768 = VECTOR('',#40699,10.) ;
#9769 = VECTOR('',#40712,10.) ;
#9770 = VECTOR('',#40713,10.) ;
#9771 = VECTOR('',#40726,10.) ;
#9772 = VECTOR('',#40727,10.) ;
#9773 = VECTOR('',#40736,10.) ;
#9774 = VECTOR('',#40739,10.) ;
#9775 = VECTOR('',#40742,10.) ;
#9776 = VECTOR('',#40743,10.) ;
#9777 = VECTOR('',#40746,10.) ;
#9778 = VECTOR('',#40751,10.) ;
#9779 = VECTOR('',#40752,10.) ;
#9780 = VECTOR('',#40757,10.) ;
#9781 = VECTOR('',#40760,10.) ;
#9782 = VECTOR('',#40773,10.) ;
#9783 = VECTOR('',#40774,10.) ;
#9784 = VECTOR('',#40787,10.) ;
#9785 = VECTOR('',#40788,10.) ;
#9786 = VECTOR('',#40801,10.) ;
#9787 = VECTOR('',#40802,10.) ;
#9788 = VECTOR('',#40811,10.) ;
#9789 = VECTOR('',#40814,10.) ;
#9790 = VECTOR('',#40817,10.) ;
#9791 = VECTOR('',#40818,10.) ;
#9792 = VECTOR('',#40821,10.) ;
#9793 = VECTOR('',#40826,10.) ;
#9794 = VECTOR('',#40827,10.) ;
#9795 = VECTOR('',#40832,10.) ;
#9796 = VECTOR('',#40835,10.) ;
#9797 = VECTOR('',#40848,10.) ;
#9798 = VECTOR('',#40849,10.) ;
#9799 = VECTOR('',#40862,10.) ;
#9800 = VECTOR('',#40863,10.) ;
#9801 = VECTOR('',#40876,10.) ;
#9802 = VECTOR('',#40877,10.) ;
#9803 = VECTOR('',#40886,10.) ;
#9804 = VECTOR('',#40889,10.) ;
#9805 = VECTOR('',#40892,10.) ;
#9806 = VECTOR('',#40893,10.) ;
#9807 = VECTOR('',#40896,10.) ;
#9808 = VECTOR('',#40901,10.) ;
#9809 = VECTOR('',#40902,10.) ;
#9810 = VECTOR('',#40907,10.) ;
#9811 = VECTOR('',#40910,10.) ;
#9812 = VECTOR('',#40923,10.) ;
#9813 = VECTOR('',#40924,10.) ;
#9814 = VECTOR('',#40937,10.) ;
#9815 = VECTOR('',#40938,10.) ;
#9816 = VECTOR('',#40951,10.) ;
#9817 = VECTOR('',#40952,10.) ;
#9818 = VECTOR('',#40961,10.) ;
#9819 = VECTOR('',#40964,10.) ;
#9820 = VECTOR('',#40967,10.) ;
#9821 = VECTOR('',#40968,10.) ;
#9822 = VECTOR('',#40971,10.) ;
#9823 = VECTOR('',#40976,10.) ;
#9824 = VECTOR('',#40977,10.) ;
#9825 = VECTOR('',#40982,10.) ;
#9826 = VECTOR('',#40985,10.) ;
#9827 = VECTOR('',#40998,10.) ;
#9828 = VECTOR('',#40999,10.) ;
#9829 = VECTOR('',#41012,10.) ;
#9830 = VECTOR('',#41013,10.) ;
#9831 = VECTOR('',#41026,10.) ;
#9832 = VECTOR('',#41035,10.) ;
#9833 = VECTOR('',#41038,0.125) ;
#9834 = VECTOR('',#41041,10.) ;
#9835 = VECTOR('',#41044,10.) ;
#9836 = VECTOR('',#41045,10.) ;
#9837 = VECTOR('',#41046,10.) ;
#9838 = VECTOR('',#41049,10.) ;
#9839 = VECTOR('',#41052,10.) ;
#9840 = VECTOR('',#41057,10.) ;
#9841 = VECTOR('',#41058,10.) ;
#9842 = VECTOR('',#41063,10.) ;
#9843 = VECTOR('',#41066,10.) ;
#9844 = VECTOR('',#41079,10.) ;
#9845 = VECTOR('',#41080,10.) ;
#9846 = VECTOR('',#41093,10.) ;
#9847 = VECTOR('',#41094,10.) ;
#9848 = VECTOR('',#41107,10.) ;
#9849 = VECTOR('',#41116,10.) ;
#9850 = VECTOR('',#41119,0.125) ;
#9851 = VECTOR('',#41122,10.) ;
#9852 = VECTOR('',#41125,10.) ;
#9853 = VECTOR('',#41126,10.) ;
#9854 = VECTOR('',#41127,10.) ;
#9855 = VECTOR('',#41130,10.) ;
#9856 = VECTOR('',#41133,10.) ;
#9857 = VECTOR('',#41138,10.) ;
#9858 = VECTOR('',#41139,10.) ;
#9859 = VECTOR('',#41144,10.) ;
#9860 = VECTOR('',#41147,10.) ;
#9861 = VECTOR('',#41160,10.) ;
#9862 = VECTOR('',#41161,10.) ;
#9863 = VECTOR('',#41174,10.) ;
#9864 = VECTOR('',#41175,10.) ;
#9865 = VECTOR('',#41188,10.) ;
#9866 = VECTOR('',#41197,10.) ;
#9867 = VECTOR('',#41200,0.125) ;
#9868 = VECTOR('',#41203,10.) ;
#9869 = VECTOR('',#41206,10.) ;
#9870 = VECTOR('',#41207,10.) ;
#9871 = VECTOR('',#41208,10.) ;
#9872 = VECTOR('',#41211,10.) ;
#9873 = VECTOR('',#41214,10.) ;
#9874 = VECTOR('',#41219,10.) ;
#9875 = VECTOR('',#41220,10.) ;
#9876 = VECTOR('',#41225,10.) ;
#9877 = VECTOR('',#41228,10.) ;
#9878 = VECTOR('',#41241,10.) ;
#9879 = VECTOR('',#41242,10.) ;
#9880 = VECTOR('',#41255,10.) ;
#9881 = VECTOR('',#41256,10.) ;
#9882 = VECTOR('',#41269,10.) ;
#9883 = VECTOR('',#41278,10.) ;
#9884 = VECTOR('',#41281,0.125) ;
#9885 = VECTOR('',#41284,10.) ;
#9886 = VECTOR('',#41287,10.) ;
#9887 = VECTOR('',#41288,10.) ;
#9888 = VECTOR('',#41289,10.) ;
#9889 = VECTOR('',#41292,10.) ;
#9890 = VECTOR('',#41295,10.) ;
#9891 = VECTOR('',#41300,10.) ;
#9892 = VECTOR('',#41301,10.) ;
#9893 = VECTOR('',#41306,10.) ;
#9894 = VECTOR('',#41309,10.) ;
#9895 = VECTOR('',#41322,10.) ;
#9896 = VECTOR('',#41323,10.) ;
#9897 = VECTOR('',#41336,10.) ;
#9898 = VECTOR('',#41337,10.) ;
#9899 = VECTOR('',#41350,10.) ;
#9900 = VECTOR('',#41359,10.) ;
#9901 = VECTOR('',#41362,0.125) ;
#9902 = VECTOR('',#41365,10.) ;
#9903 = VECTOR('',#41368,10.) ;
#9904 = VECTOR('',#41369,10.) ;
#9905 = VECTOR('',#41370,10.) ;
#9906 = VECTOR('',#41373,10.) ;
#9907 = VECTOR('',#41376,10.) ;
#9908 = VECTOR('',#41381,10.) ;
#9909 = VECTOR('',#41382,10.) ;
#9910 = VECTOR('',#41387,10.) ;
#9911 = VECTOR('',#41390,10.) ;
#9912 = VECTOR('',#41403,10.) ;
#9913 = VECTOR('',#41404,10.) ;
#9914 = VECTOR('',#41417,10.) ;
#9915 = VECTOR('',#41418,10.) ;
#9916 = VECTOR('',#41431,10.) ;
#9917 = VECTOR('',#41440,10.) ;
#9918 = VECTOR('',#41443,0.125) ;
#9919 = VECTOR('',#41446,10.) ;
#9920 = VECTOR('',#41449,10.) ;
#9921 = VECTOR('',#41450,10.) ;
#9922 = VECTOR('',#41451,10.) ;
#9923 = VECTOR('',#41454,10.) ;
#9924 = VECTOR('',#41457,10.) ;
#9925 = VECTOR('',#41462,10.) ;
#9926 = VECTOR('',#41463,10.) ;
#9927 = VECTOR('',#41468,10.) ;
#9928 = VECTOR('',#41471,10.) ;
#9929 = VECTOR('',#41484,10.) ;
#9930 = VECTOR('',#41485,10.) ;
#9931 = VECTOR('',#41498,10.) ;
#9932 = VECTOR('',#41499,10.) ;
#9933 = VECTOR('',#41512,10.) ;
#9934 = VECTOR('',#41521,10.) ;
#9935 = VECTOR('',#41524,0.125) ;
#9936 = VECTOR('',#41527,10.) ;
#9937 = VECTOR('',#41530,10.) ;
#9938 = VECTOR('',#41531,10.) ;
#9939 = VECTOR('',#41532,10.) ;
#9940 = VECTOR('',#41535,10.) ;
#9941 = VECTOR('',#41538,10.) ;
#9942 = VECTOR('',#41543,10.) ;
#9943 = VECTOR('',#41544,10.) ;
#9944 = VECTOR('',#41549,10.) ;
#9945 = VECTOR('',#41552,10.) ;
#9946 = VECTOR('',#41565,10.) ;
#9947 = VECTOR('',#41566,10.) ;
#9948 = VECTOR('',#41579,10.) ;
#9949 = VECTOR('',#41580,10.) ;
#9950 = VECTOR('',#41593,10.) ;
#9951 = VECTOR('',#41602,10.) ;
#9952 = VECTOR('',#41605,0.125) ;
#9953 = VECTOR('',#41608,10.) ;
#9954 = VECTOR('',#41611,10.) ;
#9955 = VECTOR('',#41612,10.) ;
#9956 = VECTOR('',#41613,10.) ;
#9957 = VECTOR('',#41616,10.) ;
#9958 = VECTOR('',#41619,10.) ;
#9959 = VECTOR('',#41624,10.) ;
#9960 = VECTOR('',#41625,10.) ;
#9961 = VECTOR('',#41630,10.) ;
#9962 = VECTOR('',#41633,10.) ;
#9963 = VECTOR('',#41646,10.) ;
#9964 = VECTOR('',#41647,10.) ;
#9965 = VECTOR('',#41660,10.) ;
#9966 = VECTOR('',#41661,10.) ;
#9967 = VECTOR('',#41674,10.) ;
#9968 = VECTOR('',#41675,10.) ;
#9969 = VECTOR('',#41684,10.) ;
#9970 = VECTOR('',#41687,10.) ;
#9971 = VECTOR('',#41690,10.) ;
#9972 = VECTOR('',#41691,10.) ;
#9973 = VECTOR('',#41694,10.) ;
#9974 = VECTOR('',#41699,10.) ;
#9975 = VECTOR('',#41700,10.) ;
#9976 = VECTOR('',#41703,10.) ;
#9977 = VECTOR('',#41704,10.) ;
#9978 = VECTOR('',#41705,10.) ;
#9979 = VECTOR('',#41706,10.) ;
#9980 = VECTOR('',#41707,10.) ;
#9981 = VECTOR('',#41710,10.) ;
#9982 = VECTOR('',#41713,10.) ;
#9983 = VECTOR('',#41716,10.) ;
#9984 = VECTOR('',#41725,10.) ;
#9985 = VECTOR('',#41738,10.) ;
#9986 = VECTOR('',#41749,10.) ;
#9987 = VECTOR('',#41766,10.) ;
#9988 = VECTOR('',#41769,0.125) ;
#9989 = VECTOR('',#41772,10.) ;
#9990 = VECTOR('',#41773,10.) ;
#9991 = VECTOR('',#41776,10.) ;
#9992 = VECTOR('',#41777,10.) ;
#9993 = VECTOR('',#41780,10.) ;
#9994 = VECTOR('',#41783,0.125) ;
#9995 = VECTOR('',#41788,10.) ;
#9996 = VECTOR('',#41789,10.) ;
#9997 = VECTOR('',#41792,10.) ;
#9998 = VECTOR('',#41793,10.) ;
#9999 = VECTOR('',#41804,10.) ;
#10000 = VECTOR('',#41805,10.) ;
#10001 = VECTOR('',#41810,10.) ;
#10002 = VECTOR('',#41813,10.) ;
#10003 = VECTOR('',#41818,10.) ;
#10004 = VECTOR('',#41833,10.) ;
#10005 = VECTOR('',#41844,10.) ;
#10006 = VECTOR('',#41861,10.) ;
#10007 = VECTOR('',#41866,10.) ;
#10008 = VECTOR('',#41877,10.) ;
#10009 = VECTOR('',#41880,10.) ;
#10010 = VECTOR('',#41881,10.) ;
#10011 = VECTOR('',#41886,10.) ;
#10012 = VECTOR('',#41889,10.) ;
#10013 = VECTOR('',#41898,10.) ;
#10014 = VECTOR('',#41913,10.) ;
#10015 = VECTOR('',#41914,10.) ;
#10016 = VECTOR('',#41915,10.) ;
#10017 = VECTOR('',#41916,10.) ;
#10018 = VECTOR('',#41957,10.) ;
#10019 = VECTOR('',#41960,10.) ;
#10020 = VECTOR('',#41971,10.) ;
#10021 = VECTOR('',#41988,10.) ;
#10022 = VECTOR('',#41993,10.) ;
#10023 = VECTOR('',#42004,10.) ;
#10024 = VECTOR('',#42007,10.) ;
#10025 = VECTOR('',#42008,10.) ;
#10026 = VECTOR('',#42013,10.) ;
#10027 = VECTOR('',#42016,10.) ;
#10028 = VECTOR('',#42027,10.) ;
#10029 = VECTOR('',#42044,10.) ;
#10030 = VECTOR('',#42045,10.) ;
#10031 = VECTOR('',#42046,10.) ;
#10032 = VECTOR('',#42047,10.) ;
#10033 = VECTOR('',#42066,10.) ;
#10034 = VECTOR('',#42073,10.) ;
#10035 = VECTOR('',#42094,10.) ;
#10036 = VECTOR('',#42097,10.) ;
#10037 = VECTOR('',#42108,10.) ;
#10038 = VECTOR('',#42125,10.) ;
#10039 = VECTOR('',#42130,10.) ;
#10040 = VECTOR('',#42141,10.) ;
#10041 = VECTOR('',#42144,10.) ;
#10042 = VECTOR('',#42145,10.) ;
#10043 = VECTOR('',#42150,10.) ;
#10044 = VECTOR('',#42153,10.) ;
#10045 = VECTOR('',#42164,10.) ;
#10046 = VECTOR('',#42181,10.) ;
#10047 = VECTOR('',#42182,10.) ;
#10048 = VECTOR('',#42183,10.) ;
#10049 = VECTOR('',#42184,10.) ;
#10050 = VECTOR('',#42203,10.) ;
#10051 = VECTOR('',#42210,10.) ;
#10052 = VECTOR('',#42231,10.) ;
#10053 = VECTOR('',#42234,10.) ;
#10054 = VECTOR('',#42245,10.) ;
#10055 = VECTOR('',#42262,10.) ;
#10056 = VECTOR('',#42267,10.) ;
#10057 = VECTOR('',#42278,10.) ;
#10058 = VECTOR('',#42281,10.) ;
#10059 = VECTOR('',#42282,10.) ;
#10060 = VECTOR('',#42287,10.) ;
#10061 = VECTOR('',#42290,10.) ;
#10062 = VECTOR('',#42301,10.) ;
#10063 = VECTOR('',#42318,10.) ;
#10064 = VECTOR('',#42319,10.) ;
#10065 = VECTOR('',#42320,10.) ;
#10066 = VECTOR('',#42321,10.) ;
#10067 = VECTOR('',#42340,10.) ;
#10068 = VECTOR('',#42347,10.) ;
#10069 = VECTOR('',#42368,10.) ;
#10070 = VECTOR('',#42371,10.) ;
#10071 = VECTOR('',#42382,10.) ;
#10072 = VECTOR('',#42399,10.) ;
#10073 = VECTOR('',#42404,10.) ;
#10074 = VECTOR('',#42415,10.) ;
#10075 = VECTOR('',#42418,10.) ;
#10076 = VECTOR('',#42419,10.) ;
#10077 = VECTOR('',#42424,10.) ;
#10078 = VECTOR('',#42427,10.) ;
#10079 = VECTOR('',#42438,10.) ;
#10080 = VECTOR('',#42455,10.) ;
#10081 = VECTOR('',#42456,10.) ;
#10082 = VECTOR('',#42457,10.) ;
#10083 = VECTOR('',#42458,10.) ;
#10084 = VECTOR('',#42477,10.) ;
#10085 = VECTOR('',#42484,10.) ;
#10086 = VECTOR('',#42505,10.) ;
#10087 = VECTOR('',#42508,10.) ;
#10088 = VECTOR('',#42519,10.) ;
#10089 = VECTOR('',#42536,10.) ;
#10090 = VECTOR('',#42541,10.) ;
#10091 = VECTOR('',#42552,10.) ;
#10092 = VECTOR('',#42555,10.) ;
#10093 = VECTOR('',#42556,10.) ;
#10094 = VECTOR('',#42561,10.) ;
#10095 = VECTOR('',#42564,10.) ;
#10096 = VECTOR('',#42575,10.) ;
#10097 = VECTOR('',#42592,10.) ;
#10098 = VECTOR('',#42593,10.) ;
#10099 = VECTOR('',#42594,10.) ;
#10100 = VECTOR('',#42595,10.) ;
#10101 = VECTOR('',#42614,10.) ;
#10102 = VECTOR('',#42621,10.) ;
#10103 = VECTOR('',#42642,10.) ;
#10104 = VECTOR('',#42645,10.) ;
#10105 = VECTOR('',#42656,10.) ;
#10106 = VECTOR('',#42673,10.) ;
#10107 = VECTOR('',#42678,10.) ;
#10108 = VECTOR('',#42689,10.) ;
#10109 = VECTOR('',#42692,10.) ;
#10110 = VECTOR('',#42693,10.) ;
#10111 = VECTOR('',#42698,10.) ;
#10112 = VECTOR('',#42701,10.) ;
#10113 = VECTOR('',#42712,10.) ;
#10114 = VECTOR('',#42729,10.) ;
#10115 = VECTOR('',#42730,10.) ;
#10116 = VECTOR('',#42731,10.) ;
#10117 = VECTOR('',#42732,10.) ;
#10118 = VECTOR('',#42751,10.) ;
#10119 = VECTOR('',#42758,10.) ;
#10120 = VECTOR('',#42779,10.) ;
#10121 = VECTOR('',#42782,10.) ;
#10122 = VECTOR('',#42793,10.) ;
#10123 = VECTOR('',#42810,10.) ;
#10124 = VECTOR('',#42815,10.) ;
#10125 = VECTOR('',#42826,10.) ;
#10126 = VECTOR('',#42829,10.) ;
#10127 = VECTOR('',#42830,10.) ;
#10128 = VECTOR('',#42835,10.) ;
#10129 = VECTOR('',#42838,10.) ;
#10130 = VECTOR('',#42849,10.) ;
#10131 = VECTOR('',#42866,10.) ;
#10132 = VECTOR('',#42867,10.) ;
#10133 = VECTOR('',#42868,10.) ;
#10134 = VECTOR('',#42869,10.) ;
#10135 = VECTOR('',#42888,10.) ;
#10136 = VECTOR('',#42895,10.) ;
#10137 = VECTOR('',#42916,10.) ;
#10138 = VECTOR('',#42919,10.) ;
#10139 = VECTOR('',#42930,10.) ;
#10140 = VECTOR('',#42947,10.) ;
#10141 = VECTOR('',#42952,10.) ;
#10142 = VECTOR('',#42963,10.) ;
#10143 = VECTOR('',#42966,10.) ;
#10144 = VECTOR('',#42967,10.) ;
#10145 = VECTOR('',#42972,10.) ;
#10146 = VECTOR('',#42975,10.) ;
#10147 = VECTOR('',#42986,10.) ;
#10148 = VECTOR('',#43003,10.) ;
#10149 = VECTOR('',#43004,10.) ;
#10150 = VECTOR('',#43005,10.) ;
#10151 = VECTOR('',#43006,10.) ;
#10152 = VECTOR('',#43025,10.) ;
#10153 = VECTOR('',#43032,10.) ;
#10154 = VECTOR('',#43047,10.) ;
#10155 = VECTOR('',#43048,10.) ;
#10156 = VECTOR('',#43051,10.) ;
#10157 = VECTOR('',#43052,10.) ;
#10158 = VECTOR('',#43055,10.) ;
#10159 = VECTOR('',#43056,10.) ;
#10160 = VECTOR('',#43059,10.) ;
#10161 = VECTOR('',#43060,10.) ;
#10162 = VECTOR('',#43063,10.) ;
#10163 = VECTOR('',#43064,10.) ;
#10164 = VECTOR('',#43067,10.) ;
#10165 = VECTOR('',#43068,10.) ;
#10166 = VECTOR('',#43071,10.) ;
#10167 = VECTOR('',#43072,10.) ;
#10168 = VECTOR('',#43075,10.) ;
#10169 = VECTOR('',#43076,10.) ;
#10170 = VECTOR('',#43079,10.) ;
#10171 = VECTOR('',#43080,10.) ;
#10172 = VECTOR('',#43083,10.) ;
#10173 = VECTOR('',#43086,10.) ;
#10174 = VECTOR('',#43089,10.) ;
#10175 = VECTOR('',#43092,10.) ;
#10176 = VECTOR('',#43095,10.) ;
#10177 = VECTOR('',#43098,10.) ;
#10178 = VECTOR('',#43101,10.) ;
#10179 = VECTOR('',#43104,10.) ;
#10180 = VECTOR('',#43107,10.) ;
#10181 = VECTOR('',#43110,10.) ;
#10182 = VECTOR('',#43113,10.) ;
#10183 = VECTOR('',#43116,10.) ;
#10184 = VECTOR('',#43119,10.) ;
#10185 = VECTOR('',#43122,10.) ;
#10186 = VECTOR('',#43125,10.) ;
#10187 = VECTOR('',#43128,10.) ;
#10188 = VECTOR('',#43131,10.) ;
#10189 = VECTOR('',#43134,10.) ;
#10190 = VECTOR('',#43137,12.00001256778) ;
#10191 = VECTOR('',#43138,1.052365151151) ;
#10192 = VECTOR('',#43139,10.) ;
#10193 = VECTOR('',#43140,10.) ;
#10194 = VECTOR('',#43141,12.00001256778) ;
#10195 = VECTOR('',#43142,1.052365151151) ;
#10196 = VECTOR('',#43143,10.) ;
#10197 = VECTOR('',#43144,10.) ;
#10198 = VECTOR('',#43145,12.00001256778) ;
#10199 = VECTOR('',#43146,1.052365151151) ;
#10200 = VECTOR('',#43147,10.) ;
#10201 = VECTOR('',#43148,10.) ;
#10202 = VECTOR('',#43149,12.00001256778) ;
#10203 = VECTOR('',#43150,1.052365151151) ;
#10204 = VECTOR('',#43151,10.) ;
#10205 = VECTOR('',#43152,10.) ;
#10206 = VECTOR('',#43153,12.00001256778) ;
#10207 = VECTOR('',#43154,1.052365151151) ;
#10208 = VECTOR('',#43155,12.00001251274) ;
#10209 = VECTOR('',#43156,10.) ;
#10210 = VECTOR('',#43157,12.00001256778) ;
#10211 = VECTOR('',#43158,1.052365151151) ;
#10212 = VECTOR('',#43159,12.00001251274) ;
#10213 = VECTOR('',#43160,10.) ;
#10214 = VECTOR('',#43161,12.00001256778) ;
#10215 = VECTOR('',#43162,1.052365151151) ;
#10216 = VECTOR('',#43163,12.00001251274) ;
#10217 = VECTOR('',#43164,10.) ;
#10218 = VECTOR('',#43165,12.00001256778) ;
#10219 = VECTOR('',#43166,1.052365151151) ;
#10220 = VECTOR('',#43167,12.00001256778) ;
#10221 = VECTOR('',#43168,10.) ;
#10222 = VECTOR('',#43169,12.00001256778) ;
#10223 = VECTOR('',#43170,1.052365151151) ;
#10224 = VECTOR('',#43171,10.) ;
#10225 = VECTOR('',#43172,10.) ;
#10226 = VECTOR('',#43173,10.) ;
#10227 = VECTOR('',#43174,1.052365151151) ;
#10228 = VECTOR('',#43175,10.) ;
#10229 = VECTOR('',#43176,10.) ;
#10230 = VECTOR('',#43181,1.07854801156) ;
#10231 = VECTOR('',#43186,7.7511742566901) ;
#10232 = VECTOR('',#43187,10.) ;
#10233 = VECTOR('',#43188,7.75117425719307) ;
#10234 = VECTOR('',#43191,1.07854801156) ;
#10235 = VECTOR('',#43200,1.07854801156) ;
#10236 = VECTOR('',#43207,1.07854801156) ;
#10237 = VECTOR('',#43212,1.07854801156) ;
#10238 = VECTOR('',#43219,1.07854801156) ;
#10239 = VECTOR('',#43226,1.07854801156) ;
#10240 = VECTOR('',#43235,1.07854801156) ;
#10241 = VECTOR('',#43240,1.07854801156) ;
#10242 = VECTOR('',#43249,7.75117425713307) ;
#10243 = VECTOR('',#43250,10.) ;
#10244 = VECTOR('',#43251,7.7511743083381) ;
#10245 = VECTOR('',#43254,1.07854801156) ;
#10246 = VECTOR('',#43259,10.) ;
#10247 = VECTOR('',#43262,10.) ;
#10248 = VECTOR('',#43263,10.) ;
#10249 = VECTOR('',#43264,10.) ;
#10250 = VECTOR('',#43265,10.) ;
#10251 = VECTOR('',#43268,10.) ;
#10252 = VECTOR('',#43269,10.) ;
#10253 = VECTOR('',#43270,10.) ;
#10254 = VECTOR('',#43271,10.) ;
#10255 = VECTOR('',#43274,10.) ;
#10256 = VECTOR('',#43275,10.) ;
#10257 = VECTOR('',#43276,10.) ;
#10258 = VECTOR('',#43277,10.) ;
#10259 = VECTOR('',#43280,10.) ;
#10260 = VECTOR('',#43281,10.) ;
#10261 = VECTOR('',#43282,10.) ;
#10262 = VECTOR('',#43283,10.) ;
#10263 = VECTOR('',#43286,10.) ;
#10264 = VECTOR('',#43287,10.) ;
#10265 = VECTOR('',#43288,10.) ;
#10266 = VECTOR('',#43289,10.) ;
#10267 = VECTOR('',#43292,10.) ;
#10268 = VECTOR('',#43293,10.) ;
#10269 = VECTOR('',#43294,10.) ;
#10270 = VECTOR('',#43295,10.) ;
#10271 = VECTOR('',#43298,10.) ;
#10272 = VECTOR('',#43299,10.) ;
#10273 = VECTOR('',#43300,10.) ;
#10274 = VECTOR('',#43301,10.) ;
#10275 = VECTOR('',#43304,10.) ;
#10276 = VECTOR('',#43305,10.) ;
#10277 = VECTOR('',#43306,10.) ;
#10278 = VECTOR('',#43307,10.) ;
#10279 = VECTOR('',#43310,14.2521643894801) ;
#10280 = VECTOR('',#43311,10.) ;
#10281 = VECTOR('',#43314,7.75117425713307) ;
#10282 = VECTOR('',#43315,10.) ;
#10283 = VECTOR('',#43316,7.7511742567501) ;
#10284 = VECTOR('',#43319,7.7511742566901) ;
#10285 = VECTOR('',#43320,10.) ;
#10286 = VECTOR('',#43321,7.75117425719307) ;
#10287 = VECTOR('',#43324,7.75117425713307) ;
#10288 = VECTOR('',#43325,10.) ;
#10289 = VECTOR('',#43326,7.7511743083381) ;
#10290 = VECTOR('',#43329,7.7511742566901) ;
#10291 = VECTOR('',#43330,10.) ;
#10292 = VECTOR('',#43331,7.75117425719307) ;
#10293 = VECTOR('',#43334,7.75117425713307) ;
#10294 = VECTOR('',#43335,10.) ;
#10295 = VECTOR('',#43336,7.7511742567501) ;
#10296 = VECTOR('',#43339,7.7511742566901) ;
#10297 = VECTOR('',#43340,10.) ;
#10298 = VECTOR('',#43341,7.75117425719307) ;
#10299 = VECTOR('',#43344,7.75117425713307) ;
#10300 = VECTOR('',#43345,10.) ;
#10301 = VECTOR('',#43346,7.7511742567501) ;
#10302 = VECTOR('',#43349,7.7511742566901) ;
#10303 = VECTOR('',#43350,10.) ;
#10304 = VECTOR('',#43351,7.75117425719307) ;
#10305 = VECTOR('',#43354,7.75117425713307) ;
#10306 = VECTOR('',#43355,10.) ;
#10307 = VECTOR('',#43356,7.7511743083381) ;
#10308 = VECTOR('',#43359,7.7511742566901) ;
#10309 = VECTOR('',#43360,10.) ;
#10310 = VECTOR('',#43361,7.75117425719307) ;
#10311 = VECTOR('',#43364,7.75117425713307) ;
#10312 = VECTOR('',#43365,10.) ;
#10313 = VECTOR('',#43366,7.7511743083381) ;
#10314 = VECTOR('',#43369,7.7511742566901) ;
#10315 = VECTOR('',#43370,10.) ;
#10316 = VECTOR('',#43371,7.75117425719307) ;
#10317 = VECTOR('',#43374,7.75117425713307) ;
#10318 = VECTOR('',#43375,10.) ;
#10319 = VECTOR('',#43376,7.7511743083381) ;
#10320 = VECTOR('',#43379,7.7511742566901) ;
#10321 = VECTOR('',#43380,10.) ;
#10322 = VECTOR('',#43381,7.75117425719307) ;
#10323 = VECTOR('',#43384,7.75117425713307) ;
#10324 = VECTOR('',#43385,10.) ;
#10325 = VECTOR('',#43386,7.7511742567501) ;
#10326 = VECTOR('',#43389,7.7511742566901) ;
#10327 = VECTOR('',#43390,10.) ;
#10328 = VECTOR('',#43391,7.75117425719307) ;
#10329 = VECTOR('',#43396,10.) ;
#10330 = VECTOR('',#43399,10.) ;
#10331 = VECTOR('',#43402,10.) ;
#10332 = VECTOR('',#43405,10.) ;
#10333 = VECTOR('',#43408,10.) ;
#10334 = VECTOR('',#43411,10.) ;
#10335 = VECTOR('',#43414,10.) ;
#10336 = VECTOR('',#43417,10.) ;
#10337 = VECTOR('',#43420,10.) ;
#10338 = VECTOR('',#43437,2.8575) ;
#10339 = VECTOR('',#43444,10.) ;
#10340 = VECTOR('',#43463,2.8575) ;
#10341 = VECTOR('',#43470,10.) ;
#10342 = VECTOR('',#43489,2.8575) ;
#10343 = VECTOR('',#43496,10.) ;
#10344 = VECTOR('',#43515,2.8575) ;
#10345 = VECTOR('',#43522,10.) ;
#10346 = VECTOR('',#43541,2.8575) ;
#10347 = VECTOR('',#43548,10.) ;
#10348 = VECTOR('',#43567,2.8575) ;
#10349 = VECTOR('',#43574,10.) ;
#10350 = VECTOR('',#43593,2.8575) ;
#10351 = VECTOR('',#43600,10.) ;
#10352 = VECTOR('',#43619,2.8575) ;
#10353 = VECTOR('',#43626,10.) ;
#10354 = VECTOR('',#43641,2.8575) ;
#10355 = VECTOR('',#43648,14.2521643894201) ;
#10356 = VECTOR('',#43653,10.) ;
#10357 = VECTOR('',#43656,10.) ;
#10358 = VECTOR('',#43659,10.) ;
#10359 = VECTOR('',#43666,10.) ;
#10360 = VECTOR('',#43669,10.) ;
#10361 = VECTOR('',#43672,10.) ;
#10362 = VECTOR('',#43679,10.) ;
#10363 = VECTOR('',#43682,10.) ;
#10364 = VECTOR('',#43685,10.) ;
#10365 = VECTOR('',#43692,10.) ;
#10366 = VECTOR('',#43695,10.) ;
#10367 = VECTOR('',#43698,10.) ;
#10368 = VECTOR('',#43705,10.) ;
#10369 = VECTOR('',#43708,10.) ;
#10370 = VECTOR('',#43711,10.) ;
#10371 = VECTOR('',#43718,10.) ;
#10372 = VECTOR('',#43721,10.) ;
#10373 = VECTOR('',#43724,10.) ;
#10374 = VECTOR('',#43731,10.) ;
#10375 = VECTOR('',#43734,10.) ;
#10376 = VECTOR('',#43737,10.) ;
#10377 = VECTOR('',#43744,10.) ;
#10378 = VECTOR('',#43747,10.) ;
#10379 = VECTOR('',#43750,10.) ;
#10380 = VECTOR('',#43761,1.2370442518096) ;
#10381 = VECTOR('',#43764,1.2370442518096) ;
#10382 = VECTOR('',#43767,1.2370442518096) ;
#10383 = VECTOR('',#43770,1.2370442518096) ;
#10384 = VECTOR('',#43773,1.2370442518096) ;
#10385 = VECTOR('',#43776,1.2370442518096) ;
#10386 = VECTOR('',#43779,1.2370442518096) ;
#10387 = VECTOR('',#43782,1.2370442518096) ;
#10388 = VECTOR('',#43787,1.7526) ;
#10389 = VECTOR('',#43792,1.7526) ;
#10390 = VECTOR('',#43795,1.7526) ;
#10391 = VECTOR('',#43798,1.7526) ;
#10392 = VECTOR('',#43801,1.7526) ;
#10393 = VECTOR('',#43804,1.7526) ;
#10394 = VECTOR('',#43807,1.7526) ;
#10395 = VECTOR('',#43830,10.) ;
#10396 = VECTOR('',#43833,10.) ;
#10397 = VECTOR('',#43834,10.) ;
#10398 = VECTOR('',#43879,10.) ;
#10399 = VECTOR('',#43882,10.) ;
#10400 = VECTOR('',#43885,10.) ;
#10401 = VECTOR('',#43888,10.) ;
#10402 = VECTOR('',#43891,10.) ;
#10403 = VECTOR('',#43894,10.) ;
#10404 = VECTOR('',#43895,10.) ;
#10405 = VECTOR('',#43912,10.) ;
#10406 = VECTOR('',#43915,10.) ;
#10407 = VECTOR('',#43916,10.) ;
#10408 = VECTOR('',#43937,10.) ;
#10409 = VECTOR('',#43940,10.) ;
#10410 = VECTOR('',#43943,10.) ;
#10411 = VECTOR('',#43946,10.) ;
#10412 = VECTOR('',#43949,10.) ;
#10413 = VECTOR('',#43952,10.) ;
#10414 = VECTOR('',#43953,10.) ;
#10415 = VECTOR('',#43966,10.) ;
#10416 = VECTOR('',#43969,10.) ;
#10417 = VECTOR('',#43984,10.) ;
#10418 = VECTOR('',#43989,10.) ;
#10419 = VECTOR('',#44030,10.) ;
#10420 = VECTOR('',#44031,10.) ;
#10421 = VECTOR('',#44034,10.) ;
#10422 = VECTOR('',#44043,10.) ;
#10423 = VECTOR('',#44052,10.) ;
#10424 = VECTOR('',#44053,10.) ;
#10425 = VECTOR('',#44056,10.) ;
#10426 = VECTOR('',#44061,10.) ;
#10427 = VECTOR('',#44100,10.) ;
#10428 = VECTOR('',#44103,10.) ;
#10429 = VECTOR('',#44126,10.) ;
#10430 = VECTOR('',#44127,10.) ;
#10431 = VECTOR('',#44130,10.) ;
#10432 = VECTOR('',#44139,10.) ;
#10433 = VECTOR('',#44148,10.) ;
#10434 = VECTOR('',#44149,10.) ;
#10435 = VECTOR('',#44152,10.) ;
#10436 = VECTOR('',#44157,10.) ;
#10437 = VECTOR('',#44166,10.) ;
#10438 = VECTOR('',#44169,10.) ;
#10439 = VECTOR('',#44182,10.) ;
#10440 = VECTOR('',#44185,10.) ;
#10441 = VECTOR('',#44208,10.) ;
#10442 = VECTOR('',#44209,10.) ;
#10443 = VECTOR('',#44222,10.) ;
#10444 = VECTOR('',#44225,10.) ;
#10445 = VECTOR('',#44234,10.) ;
#10446 = VECTOR('',#44235,10.) ;
#10447 = VECTOR('',#44236,10.) ;
#10448 = VECTOR('',#44239,10.) ;
#10449 = VECTOR('',#44258,10.) ;
#10450 = VECTOR('',#44259,10.) ;
#10451 = VECTOR('',#44268,10.) ;
#10452 = VECTOR('',#44271,10.) ;
#10453 = VECTOR('',#44274,10.) ;
#10454 = VECTOR('',#44275,10.) ;
#10455 = VECTOR('',#44278,10.) ;
#10456 = VECTOR('',#44283,10.) ;
#10457 = VECTOR('',#44284,10.) ;
#10458 = VECTOR('',#44285,10.) ;
#10459 = VECTOR('',#44286,9.99999999999999) ;
#10460 = VECTOR('',#44295,10.) ;
#10461 = VECTOR('',#44296,10.) ;
#10462 = VECTOR('',#44309,10.) ;
#10463 = VECTOR('',#44322,10.) ;
#10464 = VECTOR('',#44325,10.) ;
#10465 = VECTOR('',#44328,10.) ;
#10466 = VECTOR('',#44329,10.) ;
#10467 = VECTOR('',#44354,10.) ;
#10468 = VECTOR('',#44367,10.) ;
#10469 = VECTOR('',#44388,10.) ;
#10470 = VECTOR('',#44391,10.) ;
#10471 = VECTOR('',#44396,9.99999999999999) ;
#10472 = VECTOR('',#44397,10.) ;
#10473 = VECTOR('',#44398,9.99999999999999) ;
#10474 = VECTOR('',#44417,10.) ;
#10475 = VECTOR('',#44420,9.99999999999999) ;
#10476 = VECTOR('',#44423,10.) ;
#10477 = VECTOR('',#44424,10.) ;
#10478 = VECTOR('',#44435,10.) ;
#10479 = VECTOR('',#44436,10.) ;
#10480 = VECTOR('',#44449,10.) ;
#10481 = VECTOR('',#44452,9.99999999999999) ;
#10482 = VECTOR('',#44461,10.) ;
#10483 = VECTOR('',#44462,10.) ;
#10484 = VECTOR('',#44463,10.) ;
#10485 = VECTOR('',#44466,10.) ;
#10486 = VECTOR('',#44485,10.) ;
#10487 = VECTOR('',#44486,10.) ;
#10488 = VECTOR('',#44495,10.) ;
#10489 = VECTOR('',#44498,10.) ;
#10490 = VECTOR('',#44501,10.) ;
#10491 = VECTOR('',#44502,10.) ;
#10492 = VECTOR('',#44505,10.) ;
#10493 = VECTOR('',#44510,10.) ;
#10494 = VECTOR('',#44511,10.) ;
#10495 = VECTOR('',#44512,10.) ;
#10496 = VECTOR('',#44517,10.) ;
#10497 = VECTOR('',#44520,10.) ;
#10498 = VECTOR('',#44537,10.) ;
#10499 = VECTOR('',#44550,10.) ;
#10500 = VECTOR('',#44551,10.) ;
#10501 = VECTOR('',#44554,10.) ;
#10502 = VECTOR('',#44557,10.) ;
#10503 = VECTOR('',#44560,10.) ;
#10504 = VECTOR('',#44561,10.) ;
#10505 = VECTOR('',#44588,10.) ;
#10506 = VECTOR('',#44601,10.) ;
#10507 = VECTOR('',#44622,10.) ;
#10508 = VECTOR('',#44625,10.) ;
#10509 = VECTOR('',#44626,10.) ;
#10510 = VECTOR('',#44627,10.) ;
#10511 = VECTOR('',#44646,10.) ;
#10512 = VECTOR('',#44649,10.) ;
#10513 = VECTOR('',#44694,10.) ;
#10514 = VECTOR('',#44725,10.) ;
#10515 = VECTOR('',#44738,1.7526) ;
#10516 = VECTOR('',#44771,1.7526) ;
#10517 = VECTOR('',#44776,1.7526) ;
#10518 = VECTOR('',#44779,1.7526) ;
#10519 = VECTOR('',#44782,1.7526) ;
#10520 = VECTOR('',#44787,1.5) ;
#10521 = VECTOR('',#44792,1.5) ;
#10522 = VECTOR('',#44795,1.5) ;
#10523 = VECTOR('',#44798,1.5) ;
#10524 = VECTOR('',#44809,10.) ;
#10525 = VECTOR('',#44812,10.) ;
#10526 = VECTOR('',#44827,10.) ;
#10527 = VECTOR('',#44828,10.) ;
#10528 = VECTOR('',#44853,10.) ;
#10529 = VECTOR('',#44854,10.) ;
#10530 = VECTOR('',#44865,10.) ;
#10531 = VECTOR('',#44866,10.) ;
#10532 = VECTOR('',#44871,10.) ;
#10533 = VECTOR('',#44872,10.) ;
#10534 = VECTOR('',#44887,10.) ;
#10535 = VECTOR('',#44888,10.) ;
#10536 = VECTOR('',#44893,10.) ;
#10537 = VECTOR('',#44894,10.) ;
#10538 = VECTOR('',#44905,10.) ;
#10539 = VECTOR('',#44906,10.) ;
#10540 = VECTOR('',#44909,10.) ;
#10541 = VECTOR('',#44910,10.) ;
#10542 = VECTOR('',#44915,10.) ;
#10543 = VECTOR('',#44916,10.) ;
#10544 = VECTOR('',#44919,10.) ;
#10545 = VECTOR('',#44920,10.) ;
#10546 = VECTOR('',#44933,10.) ;
#10547 = VECTOR('',#44936,10.) ;
#10548 = VECTOR('',#44947,6.35) ;
#10549 = VECTOR('',#44950,10.) ;
#10550 = VECTOR('',#44953,0.125) ;
#10551 = VECTOR('',#44956,10.) ;
#10552 = VECTOR('',#44957,6.35) ;
#10553 = VECTOR('',#44960,10.) ;
#10554 = VECTOR('',#44965,10.) ;
#10555 = VECTOR('',#44966,10.) ;
#10556 = VECTOR('',#44973,6.35) ;
#10557 = VECTOR('',#44978,10.) ;
#10558 = VECTOR('',#44983,10.) ;
#10559 = VECTOR('',#44986,10.) ;
#10560 = VECTOR('',#44991,10.) ;
#10561 = VECTOR('',#44992,10.) ;
#10562 = VECTOR('',#44993,6.35) ;
#10563 = VECTOR('',#44994,10.) ;
#10564 = VECTOR('',#44995,10.) ;
#10565 = VECTOR('',#45000,10.) ;
#10566 = VECTOR('',#45003,10.) ;
#10567 = VECTOR('',#45004,10.) ;
#10568 = VECTOR('',#45005,6.35) ;
#10569 = VECTOR('',#45006,10.) ;
#10570 = VECTOR('',#45009,10.) ;
#10571 = VECTOR('',#45010,10.) ;
#10572 = VECTOR('',#45011,10.) ;
#10573 = VECTOR('',#45012,10.) ;
#10574 = VECTOR('',#45015,10.) ;
#10575 = VECTOR('',#45016,10.) ;
#10576 = VECTOR('',#45019,10.) ;
#10577 = VECTOR('',#45020,10.) ;
#10578 = VECTOR('',#45021,6.35) ;
#10579 = VECTOR('',#45022,10.) ;
#10580 = VECTOR('',#45023,10.) ;
#10581 = VECTOR('',#45026,10.) ;
#10582 = VECTOR('',#45029,10.) ;
#10583 = VECTOR('',#45030,6.35) ;
#10584 = VECTOR('',#45031,10.) ;
#10585 = VECTOR('',#45032,6.35) ;
#10586 = VECTOR('',#45047,10.) ;
#10587 = VECTOR('',#45050,10.) ;
#10588 = VECTOR('',#45053,10.) ;
#10589 = VECTOR('',#45054,10.) ;
#10590 = VECTOR('',#45055,10.) ;
#10591 = VECTOR('',#45056,10.) ;
#10592 = VECTOR('',#45065,10.) ;
#10593 = VECTOR('',#45066,10.) ;
#10594 = VECTOR('',#45069,10.) ;
#10595 = VECTOR('',#45072,10.) ;
#10596 = VECTOR('',#45075,10.) ;
#10597 = VECTOR('',#45078,10.) ;
#10598 = VECTOR('',#45081,10.) ;
#10599 = VECTOR('',#45082,10.) ;
#10600 = VECTOR('',#45087,10.) ;
#10601 = VECTOR('',#45092,10.) ;
#10602 = VECTOR('',#45093,10.) ;
#10603 = VECTOR('',#45094,10.) ;
#10604 = VECTOR('',#45137,10.) ;
#10605 = VECTOR('',#45140,10.) ;
#10606 = VECTOR('',#45147,10.) ;
#10607 = VECTOR('',#45154,10.) ;
#10608 = VECTOR('',#45183,10.) ;
#10609 = VECTOR('',#45190,10.) ;
#10610 = VECTOR('',#45217,10.) ;
#10611 = VECTOR('',#45254,10.) ;
#10612 = VECTOR('',#45259,10.) ;
#10613 = VECTOR('',#45268,10.) ;
#10614 = VECTOR('',#45303,2.8575) ;
#10615 = VECTOR('',#45356,1.651) ;
#10616 = VECTOR('',#45361,6.35) ;
#10617 = VECTOR('',#45362,6.35) ;
#10618 = VECTOR('',#45365,6.35) ;
#10619 = VECTOR('',#45366,6.35) ;
#10620 = VECTOR('',#45367,6.35) ;
#10621 = VECTOR('',#45368,6.35) ;
#10622 = VECTOR('',#45371,6.35) ;
#10623 = VECTOR('',#45372,6.35) ;
#10624 = VECTOR('',#45373,6.35) ;
#10625 = VECTOR('',#45374,6.35) ;
#10626 = VECTOR('',#45377,6.35) ;
#10627 = VECTOR('',#45378,6.35) ;
#10628 = VECTOR('',#45379,6.35) ;
#10629 = VECTOR('',#45380,6.35) ;
#10630 = VECTOR('',#45383,6.35) ;
#10631 = VECTOR('',#45384,6.35) ;
#10632 = VECTOR('',#45387,6.35) ;
#10633 = VECTOR('',#45388,6.35) ;
#10634 = VECTOR('',#45389,6.35) ;
#10635 = VECTOR('',#45394,6.35) ;
#10636 = VECTOR('',#45395,6.35) ;
#10637 = VECTOR('',#45398,6.35) ;
#10638 = VECTOR('',#45401,6.35) ;
#10639 = VECTOR('',#45402,6.35) ;
#10640 = VECTOR('',#45403,6.35) ;
#10641 = VECTOR('',#45408,6.35) ;
#10642 = VECTOR('',#45409,6.35) ;
#10643 = VECTOR('',#45412,6.35) ;
#10644 = VECTOR('',#45423,6.35) ;
#10645 = VECTOR('',#45430,6.35) ;
#10646 = VECTOR('',#45441,6.35) ;
#10647 = VECTOR('',#45448,6.35) ;
#10648 = VECTOR('',#45459,6.35) ;
#10649 = VECTOR('',#45466,6.35) ;
#10650 = VECTOR('',#45469,6.35) ;
#10651 = VECTOR('',#45470,6.35) ;
#10652 = VECTOR('',#45471,6.35) ;
#10653 = VECTOR('',#45474,6.35) ;
#10654 = VECTOR('',#45475,6.35) ;
#10655 = VECTOR('',#45476,6.35) ;
#10656 = VECTOR('',#45497,6.35) ;
#10657 = VECTOR('',#45498,6.35) ;
#10658 = VECTOR('',#45499,6.35) ;
#10659 = VECTOR('',#45500,6.35) ;
#10660 = VECTOR('',#45503,6.35) ;
#10661 = VECTOR('',#45504,6.35) ;
#10662 = VECTOR('',#45505,6.35) ;
#10663 = VECTOR('',#45506,6.35) ;
#10664 = VECTOR('',#45525,6.35) ;
#10665 = VECTOR('',#45526,6.35) ;
#10666 = VECTOR('',#45527,6.35) ;
#10667 = VECTOR('',#45530,6.35) ;
#10668 = VECTOR('',#45531,6.35) ;
#10669 = VECTOR('',#45532,6.35) ;
#10670 = VECTOR('',#45553,6.35) ;
#10671 = VECTOR('',#45554,6.35) ;
#10672 = VECTOR('',#45555,6.35) ;
#10673 = VECTOR('',#45558,6.35) ;
#10674 = VECTOR('',#45559,6.35) ;
#10675 = VECTOR('',#45560,6.35) ;
#10676 = VECTOR('',#45601,6.35) ;
#10677 = VECTOR('',#45602,6.35) ;
#10678 = VECTOR('',#45603,6.35) ;
#10679 = VECTOR('',#45606,6.35) ;
#10680 = VECTOR('',#45607,6.35) ;
#10681 = VECTOR('',#45608,6.35) ;
#10682 = VECTOR('',#45611,6.35) ;
#10683 = VECTOR('',#45612,6.35) ;
#10684 = VECTOR('',#45613,6.35) ;
#10685 = VECTOR('',#45614,6.35) ;
#10686 = VECTOR('',#45639,6.35) ;
#10687 = VECTOR('',#45640,6.35) ;
#10688 = VECTOR('',#45641,6.35) ;
#10689 = VECTOR('',#45644,6.35) ;
#10690 = VECTOR('',#45645,6.35) ;
#10691 = VECTOR('',#45646,6.35) ;
#10692 = VECTOR('',#45649,6.35) ;
#10693 = VECTOR('',#45650,6.35) ;
#10694 = VECTOR('',#45651,6.35) ;
#10695 = VECTOR('',#45652,6.35) ;
#10696 = VECTOR('',#45675,6.35) ;
#10697 = VECTOR('',#45676,6.35) ;
#10698 = VECTOR('',#45677,6.35) ;
#10699 = VECTOR('',#45682,6.35) ;
#10700 = VECTOR('',#45683,6.35) ;
#10701 = VECTOR('',#45684,6.35) ;
#10702 = VECTOR('',#45687,6.35) ;
#10703 = VECTOR('',#45688,6.35) ;
#10704 = VECTOR('',#45689,6.35) ;
#10705 = VECTOR('',#45690,6.35) ;
#10706 = VECTOR('',#45713,6.35) ;
#10707 = VECTOR('',#45714,6.35) ;
#10708 = VECTOR('',#45715,6.35) ;
#10709 = VECTOR('',#45720,6.35) ;
#10710 = VECTOR('',#45721,6.35) ;
#10711 = VECTOR('',#45722,6.35) ;
#10712 = VECTOR('',#45725,6.35) ;
#10713 = VECTOR('',#45726,6.35) ;
#10714 = VECTOR('',#45727,6.35) ;
#10715 = VECTOR('',#45728,6.35) ;
#10716 = VECTOR('',#45751,6.35) ;
#10717 = VECTOR('',#45752,6.35) ;
#10718 = VECTOR('',#45753,6.35) ;
#10719 = VECTOR('',#45754,6.35) ;
#10720 = VECTOR('',#45755,6.35) ;
#10721 = VECTOR('',#45756,6.35) ;
#10722 = VECTOR('',#45759,6.35) ;
#10723 = VECTOR('',#45760,6.35) ;
#10724 = VECTOR('',#45761,6.35) ;
#10725 = VECTOR('',#45762,6.35) ;
#10726 = VECTOR('',#45763,6.35) ;
#10727 = VECTOR('',#45764,6.35) ;
#10728 = VECTOR('',#45767,6.35) ;
#10729 = VECTOR('',#45768,6.35) ;
#10730 = VECTOR('',#45769,6.35) ;
#10731 = VECTOR('',#45770,6.35) ;
#10732 = VECTOR('',#45771,6.35) ;
#10733 = VECTOR('',#45772,6.35) ;
#10734 = VECTOR('',#45775,6.35) ;
#10735 = VECTOR('',#45776,6.35) ;
#10736 = VECTOR('',#45777,6.35) ;
#10737 = VECTOR('',#45778,6.35) ;
#10738 = VECTOR('',#45779,6.35) ;
#10739 = VECTOR('',#45780,6.35) ;
#10740 = VECTOR('',#45797,6.35) ;
#10741 = VECTOR('',#45800,6.35) ;
#10742 = VECTOR('',#45805,6.35) ;
#10743 = VECTOR('',#45808,6.35) ;
#10744 = VECTOR('',#45815,6.35) ;
#10745 = VECTOR('',#45818,6.35) ;
#10746 = VECTOR('',#45823,6.35) ;
#10747 = VECTOR('',#45826,6.35) ;
#10748 = VECTOR('',#45865,10.) ;
#10749 = VECTOR('',#45866,10.) ;
#10750 = VECTOR('',#45867,10.) ;
#10751 = VECTOR('',#45868,9.99999999999998) ;
#10752 = VECTOR('',#45869,10.) ;
#10753 = VECTOR('',#45870,10.) ;
#10754 = VECTOR('',#45873,10.) ;
#10755 = VECTOR('',#45874,10.) ;
#10756 = VECTOR('',#45875,10.) ;
#10757 = VECTOR('',#45876,10.) ;
#10758 = VECTOR('',#45877,10.) ;
#10759 = VECTOR('',#45880,10.) ;
#10760 = VECTOR('',#45881,10.) ;
#10761 = VECTOR('',#45882,10.) ;
#10762 = VECTOR('',#45883,10.) ;
#10763 = VECTOR('',#45886,10.) ;
#10764 = VECTOR('',#45887,10.) ;
#10765 = VECTOR('',#45890,10.) ;
#10766 = VECTOR('',#45891,10.) ;
#10767 = VECTOR('',#45892,10.) ;
#10768 = VECTOR('',#45893,10.) ;
#10769 = VECTOR('',#45896,10.) ;
#10770 = VECTOR('',#45897,10.) ;
#10771 = VECTOR('',#45898,10.) ;
#10772 = VECTOR('',#45899,10.) ;
#10773 = VECTOR('',#45902,10.) ;
#10774 = VECTOR('',#45903,10.) ;
#10775 = VECTOR('',#45904,10.) ;
#10776 = VECTOR('',#45905,10.) ;
#10777 = VECTOR('',#45906,10.) ;
#10778 = VECTOR('',#45909,10.) ;
#10779 = VECTOR('',#45910,10.) ;
#10780 = VECTOR('',#45911,10.) ;
#10781 = VECTOR('',#45914,10.) ;
#10782 = VECTOR('',#45915,10.) ;
#10783 = VECTOR('',#45918,10.) ;
#10784 = VECTOR('',#45919,10.) ;
#10785 = VECTOR('',#45920,10.) ;
#10786 = VECTOR('',#45921,10.) ;
#10787 = VECTOR('',#45924,10.) ;
#10788 = VECTOR('',#45925,10.) ;
#10789 = VECTOR('',#45930,10.) ;
#10790 = VECTOR('',#45943,10.) ;
#10791 = VECTOR('',#45956,10.) ;
#10792 = VECTOR('',#45957,10.) ;
#10793 = VECTOR('',#45960,10.) ;
#10794 = VECTOR('',#45961,10.) ;
#10795 = VECTOR('',#45964,10.) ;
#10796 = VECTOR('',#45969,1.25) ;
#10797 = VECTOR('',#45972,1.25) ;
#10798 = VECTOR('',#45975,1.25) ;
#10799 = VECTOR('',#45978,1.25) ;
#10800 = VECTOR('',#45981,1.25) ;
#10801 = VECTOR('',#45994,1.5) ;
#10802 = VECTOR('',#45999,1.5) ;
#10803 = VECTOR('',#46002,1.5) ;
#10804 = VECTOR('',#46005,1.5) ;
#10805 = VECTOR('',#46008,1.5) ;
#10806 = VECTOR('',#46011,1.5) ;
#10807 = VECTOR('',#46014,1.5) ;
#10808 = VECTOR('',#46017,1.5) ;
#10809 = VECTOR('',#46020,1.5) ;
#10810 = VECTOR('',#46023,1.5) ;
#10811 = VECTOR('',#46026,1.5) ;
#10812 = VECTOR('',#46029,1.5) ;
#10813 = VECTOR('',#46032,1.5) ;
#10814 = VECTOR('',#46035,1.5) ;
#10815 = VECTOR('',#46038,1.5) ;
#10816 = VECTOR('',#46041,1.17524047358084) ;
#10817 = VECTOR('',#46046,1.17524047358084) ;
#10818 = VECTOR('',#46049,1.17524047358084) ;
#10819 = VECTOR('',#46052,1.17524047358084) ;
#10820 = VECTOR('',#46055,1.17524047358084) ;
#10821 = VECTOR('',#46058,1.17524047358084) ;
#10822 = VECTOR('',#46061,1.17524047358084) ;
#10823 = VECTOR('',#46064,1.17524047358084) ;
#10824 = VECTOR('',#46067,1.17524047358084) ;
#10825 = VECTOR('',#46070,1.17524047358084) ;
#10826 = VECTOR('',#46073,1.17524047358084) ;
#10827 = VECTOR('',#46076,1.17524047358084) ;
#10828 = VECTOR('',#46079,1.17524047358084) ;
#10829 = VECTOR('',#46082,1.17524047358084) ;
#10830 = VECTOR('',#46085,1.17524047358084) ;
#10831 = VECTOR('',#46088,1.17524047358084) ;
#10832 = VECTOR('',#46091,4.35024047358084) ;
#10833 = VECTOR('',#46170,2.99999999999999) ;
#10834 = VECTOR('',#46181,1000.) ;
#10835 = VECTOR('',#46190,1000.) ;
#10836 = VECTOR('',#46191,1000.) ;
#10837 = VECTOR('',#46194,1000.) ;
#10838 = VECTOR('',#46195,1000.) ;
#10839 = VECTOR('',#46198,1000.) ;
#10840 = VECTOR('',#46199,1000.) ;
#10841 = VECTOR('',#46202,1000.) ;
#10842 = VECTOR('',#46205,1000.) ;
#10843 = VECTOR('',#46206,1000.) ;
#10844 = VECTOR('',#46207,1000.) ;
#10845 = VECTOR('',#46208,999.999999999999) ;
#10846 = VECTOR('',#46209,1000.) ;
#10847 = VECTOR('',#46212,1000.) ;
#10848 = VECTOR('',#46213,1000.) ;
#10849 = VECTOR('',#46214,1000.) ;
#10850 = VECTOR('',#46215,1000.) ;
#10851 = VECTOR('',#46216,1000.) ;
#10852 = VECTOR('',#46217,1000.) ;
#10853 = VECTOR('',#46218,1000.) ;
#10854 = VECTOR('',#46221,1000.) ;
#10855 = VECTOR('',#46224,1000.) ;
#10856 = VECTOR('',#46227,1000.) ;
#10857 = VECTOR('',#46232,999.999999999999) ;
#10858 = VECTOR('',#46235,1000.) ;
#10859 = VECTOR('',#46238,1000.) ;
#10860 = VECTOR('',#46245,1000.) ;
#10861 = VECTOR('',#46248,1000.) ;
#10862 = VECTOR('',#46251,1000.) ;
#10863 = VECTOR('',#46258,10.) ;
#10864 = VECTOR('',#46259,10.) ;
#10865 = VECTOR('',#46260,10.) ;
#10866 = VECTOR('',#46261,10.) ;
#10867 = VECTOR('',#46264,10.) ;
#10868 = VECTOR('',#46265,10.) ;
#10869 = VECTOR('',#46266,10.) ;
#10870 = VECTOR('',#46267,10.) ;
#10871 = VECTOR('',#46288,3.) ;
#10872 = VECTOR('',#46305,1.6) ;
#10873 = CIRCLE('',#32775,0.25) ;
#10874 = CIRCLE('',#32776,0.25) ;
#10875 = CIRCLE('',#32778,23.5) ;
#10876 = CIRCLE('',#32779,28.5) ;
#10877 = CIRCLE('',#32780,2.4999999999) ;
#10878 = CIRCLE('',#32781,28.5) ;
#10879 = CIRCLE('',#32782,2.4999999999) ;
#10880 = CIRCLE('',#32783,23.5) ;
#10881 = CIRCLE('',#32784,2.4999999999) ;
#10882 = CIRCLE('',#32785,28.5) ;
#10883 = CIRCLE('',#32786,2.4999999999) ;
#10884 = CIRCLE('',#32787,23.5) ;
#10885 = CIRCLE('',#32788,15.5) ;
#10886 = CIRCLE('',#32789,3.) ;
#10887 = CIRCLE('',#32790,21.5) ;
#10888 = CIRCLE('',#32791,3.) ;
#10889 = CIRCLE('',#32792,1.5) ;
#10890 = CIRCLE('',#32793,1.5) ;
#10891 = CIRCLE('',#32794,1.5) ;
#10892 = CIRCLE('',#32795,1.5) ;
#10893 = CIRCLE('',#32796,1.5) ;
#10894 = CIRCLE('',#32797,1.5) ;
#10895 = CIRCLE('',#32798,1.5) ;
#10896 = CIRCLE('',#32799,1.5) ;
#10897 = CIRCLE('',#32800,1.5) ;
#10898 = CIRCLE('',#32801,1.5) ;
#10899 = CIRCLE('',#32802,1.5) ;
#10900 = CIRCLE('',#32803,1.5) ;
#10901 = CIRCLE('',#32804,1.90000000000502) ;
#10902 = CIRCLE('',#32805,1.90000000000502) ;
#10903 = CIRCLE('',#32806,2.) ;
#10904 = CIRCLE('',#32807,2.) ;
#10905 = CIRCLE('',#32808,2.) ;
#10906 = CIRCLE('',#32809,2.) ;
#10907 = CIRCLE('',#32810,3.) ;
#10908 = CIRCLE('',#32811,21.5) ;
#10909 = CIRCLE('',#32812,3.) ;
#10910 = CIRCLE('',#32813,15.5) ;
#10911 = CIRCLE('',#32814,3.) ;
#10912 = CIRCLE('',#32815,21.5) ;
#10913 = CIRCLE('',#32816,3.) ;
#10914 = CIRCLE('',#32817,15.5) ;
#10915 = CIRCLE('',#32818,3.) ;
#10916 = CIRCLE('',#32819,21.5) ;
#10917 = CIRCLE('',#32820,3.) ;
#10918 = CIRCLE('',#32821,15.5) ;
#10919 = CIRCLE('',#32822,23.5) ;
#10920 = CIRCLE('',#32823,2.4999999999) ;
#10921 = CIRCLE('',#32824,28.5) ;
#10922 = CIRCLE('',#32825,2.4999999999) ;
#10923 = CIRCLE('',#32827,0.25) ;
#10924 = CIRCLE('',#32828,0.25) ;
#10925 = CIRCLE('',#32830,0.25) ;
#10926 = CIRCLE('',#32831,0.25) ;
#10927 = CIRCLE('',#32833,0.5) ;
#10928 = CIRCLE('',#32834,1.) ;
#10929 = CIRCLE('',#32835,1.) ;
#10930 = CIRCLE('',#32836,1.) ;
#10931 = CIRCLE('',#32837,1.) ;
#10932 = CIRCLE('',#32838,1.) ;
#10933 = CIRCLE('',#32839,1.) ;
#10934 = CIRCLE('',#32840,1.) ;
#10935 = CIRCLE('',#32841,1.25) ;
#10936 = CIRCLE('',#32842,1.25) ;
#10937 = CIRCLE('',#32844,0.75) ;
#10938 = CIRCLE('',#32845,0.75) ;
#10939 = CIRCLE('',#32848,0.5) ;
#10940 = CIRCLE('',#32849,1.) ;
#10941 = CIRCLE('',#32850,1.) ;
#10942 = CIRCLE('',#32851,1.) ;
#10943 = CIRCLE('',#32852,1.) ;
#10944 = CIRCLE('',#32853,1.) ;
#10945 = CIRCLE('',#32854,1.) ;
#10946 = CIRCLE('',#32855,1.) ;
#10947 = CIRCLE('',#32856,1.25) ;
#10948 = CIRCLE('',#32857,1.25) ;
#10949 = CIRCLE('',#32859,0.75) ;
#10950 = CIRCLE('',#32860,0.75) ;
#10951 = CIRCLE('',#32863,1.) ;
#10952 = CIRCLE('',#32864,1.) ;
#10953 = CIRCLE('',#32865,1.) ;
#10954 = CIRCLE('',#32866,1.) ;
#10955 = CIRCLE('',#32867,1.) ;
#10956 = CIRCLE('',#32868,1.) ;
#10957 = CIRCLE('',#32869,1.) ;
#10958 = CIRCLE('',#32870,0.5) ;
#10959 = CIRCLE('',#32871,1.25) ;
#10960 = CIRCLE('',#32872,1.25) ;
#10961 = CIRCLE('',#32874,1.) ;
#10962 = CIRCLE('',#32879,0.75) ;
#10963 = CIRCLE('',#32880,0.75) ;
#10964 = CIRCLE('',#32883,23.5) ;
#10965 = CIRCLE('',#32884,2.4999999999) ;
#10966 = CIRCLE('',#32885,28.5) ;
#10967 = CIRCLE('',#32886,2.4999999999) ;
#10968 = CIRCLE('',#32887,2.5) ;
#10969 = CIRCLE('',#32888,2.5) ;
#10970 = CIRCLE('',#32889,1.5) ;
#10971 = CIRCLE('',#32890,1.5) ;
#10972 = CIRCLE('',#32891,1.5) ;
#10973 = CIRCLE('',#32892,1.5) ;
#10974 = CIRCLE('',#32893,1.5) ;
#10975 = CIRCLE('',#32894,1.5) ;
#10976 = CIRCLE('',#32895,1.5) ;
#10977 = CIRCLE('',#32896,1.5) ;
#10978 = CIRCLE('',#32897,1.5) ;
#10979 = CIRCLE('',#32898,1.5) ;
#10980 = CIRCLE('',#32899,1.5) ;
#10981 = CIRCLE('',#32900,1.5) ;
#10982 = CIRCLE('',#32901,2.) ;
#10983 = CIRCLE('',#32902,2.) ;
#10984 = CIRCLE('',#32903,2.) ;
#10985 = CIRCLE('',#32904,2.) ;
#10986 = CIRCLE('',#32905,15.5) ;
#10987 = CIRCLE('',#32906,3.) ;
#10988 = CIRCLE('',#32907,21.5) ;
#10989 = CIRCLE('',#32908,3.) ;
#10990 = CIRCLE('',#32909,3.) ;
#10991 = CIRCLE('',#32910,15.5) ;
#10992 = CIRCLE('',#32911,3.) ;
#10993 = CIRCLE('',#32912,21.5) ;
#10994 = CIRCLE('',#32913,3.) ;
#10995 = CIRCLE('',#32914,15.5) ;
#10996 = CIRCLE('',#32915,3.) ;
#10997 = CIRCLE('',#32916,21.5) ;
#10998 = CIRCLE('',#32917,3.) ;
#10999 = CIRCLE('',#32918,15.5) ;
#11000 = CIRCLE('',#32919,3.) ;
#11001 = CIRCLE('',#32920,21.5) ;
#11002 = CIRCLE('',#32921,23.5) ;
#11003 = CIRCLE('',#32922,2.4999999999) ;
#11004 = CIRCLE('',#32923,28.5) ;
#11005 = CIRCLE('',#32924,2.4999999999) ;
#11006 = CIRCLE('',#32925,23.5) ;
#11007 = CIRCLE('',#32926,2.4999999999) ;
#11008 = CIRCLE('',#32927,28.5) ;
#11009 = CIRCLE('',#32928,23.5) ;
#11010 = CIRCLE('',#32929,2.4999999999) ;
#11011 = CIRCLE('',#32930,28.5) ;
#11012 = CIRCLE('',#32932,1.) ;
#11013 = CIRCLE('',#32933,1.) ;
#11014 = CIRCLE('',#32934,1.) ;
#11015 = CIRCLE('',#32935,1.) ;
#11016 = CIRCLE('',#32936,1.) ;
#11017 = CIRCLE('',#32937,1.) ;
#11018 = CIRCLE('',#32938,0.5) ;
#11019 = CIRCLE('',#32939,1.25) ;
#11020 = CIRCLE('',#32940,1.25) ;
#11021 = CIRCLE('',#32942,0.5) ;
#11022 = CIRCLE('',#32943,0.5) ;
#11023 = CIRCLE('',#32955,0.5) ;
#11024 = CIRCLE('',#32958,0.5) ;
#11025 = CIRCLE('',#32962,0.5) ;
#11026 = CIRCLE('',#32963,0.5) ;
#11027 = CIRCLE('',#32966,0.5) ;
#11028 = CIRCLE('',#32968,0.5) ;
#11029 = CIRCLE('',#32970,0.75) ;
#11030 = CIRCLE('',#32971,0.25) ;
#11031 = CIRCLE('',#32996,0.25) ;
#11032 = CIRCLE('',#32998,0.75) ;
#11033 = CIRCLE('',#33064,1.17524047358084) ;
#11034 = CIRCLE('',#33069,1.17524047358083) ;
#11035 = CIRCLE('',#33071,1.5) ;
#11036 = CIRCLE('',#33077,1.5) ;
#11037 = CIRCLE('',#33081,1.5) ;
#11038 = CIRCLE('',#33083,1.5) ;
#11039 = CIRCLE('',#33087,2.75) ;
#11040 = CIRCLE('',#33089,2.75) ;
#11041 = CIRCLE('',#33091,2.75) ;
#11042 = CIRCLE('',#33092,2.75) ;
#11043 = CIRCLE('',#33093,2.75) ;
#11044 = CIRCLE('',#33094,2.75) ;
#11045 = CIRCLE('',#33095,2.75) ;
#11046 = CIRCLE('',#33103,2.75) ;
#11047 = CIRCLE('',#33104,2.75) ;
#11048 = CIRCLE('',#33105,2.75) ;
#11049 = CIRCLE('',#33106,2.75) ;
#11050 = CIRCLE('',#33107,2.75) ;
#11051 = CIRCLE('',#33126,1.00995540144767) ;
#11052 = CIRCLE('',#33128,1.00995540144767) ;
#11053 = CIRCLE('',#33134,1.4224) ;
#11054 = CIRCLE('',#33135,1.42240000000001) ;
#11055 = CIRCLE('',#33136,1.42240000000001) ;
#11056 = CIRCLE('',#33137,1.4224) ;
#11057 = CIRCLE('',#33143,1.4224) ;
#11058 = CIRCLE('',#33145,1.00995540144768) ;
#11059 = CIRCLE('',#33147,2.55525626680218) ;
#11060 = CIRCLE('',#33148,0.0625) ;
#11061 = CIRCLE('',#33149,2.60242561556611) ;
#11062 = CIRCLE('',#33150,2.60242561556611) ;
#11063 = CIRCLE('',#33153,1.7907) ;
#11064 = CIRCLE('',#33154,1.7907) ;
#11065 = CIRCLE('',#33155,1.7907) ;
#11066 = CIRCLE('',#33156,1.7907) ;
#11067 = CIRCLE('',#33158,0.92075) ;
#11068 = CIRCLE('',#33160,1.7907) ;
#11069 = CIRCLE('',#33161,1.7907) ;
#11070 = CIRCLE('',#33162,1.7907) ;
#11071 = CIRCLE('',#33163,1.7907) ;
#11072 = CIRCLE('',#33164,1.7907) ;
#11073 = CIRCLE('',#33202,2.05475000000016) ;
#11074 = CIRCLE('',#33205,2.05475000000007) ;
#11075 = CIRCLE('',#33207,2.05475000000044) ;
#11076 = CIRCLE('',#33210,2.0547500000002) ;
#11077 = CIRCLE('',#33212,2.05475000000044) ;
#11078 = CIRCLE('',#33215,2.0547500000002) ;
#11079 = CIRCLE('',#33217,2.05475000000009) ;
#11080 = CIRCLE('',#33220,2.05475) ;
#11081 = CIRCLE('',#33222,1.66599999999999) ;
#11082 = CIRCLE('',#33224,1.66599999999999) ;
#11083 = CIRCLE('',#33226,1.66599999999999) ;
#11084 = CIRCLE('',#33228,1.66599999999999) ;
#11085 = CIRCLE('',#33230,1.66599999999999) ;
#11086 = CIRCLE('',#33232,1.66599999999999) ;
#11087 = CIRCLE('',#33234,1.66599999999999) ;
#11088 = CIRCLE('',#33236,1.66599999999999) ;
#11089 = CIRCLE('',#33238,1.66599999999999) ;
#11090 = CIRCLE('',#33240,1.66599999999999) ;
#11091 = CIRCLE('',#33242,1.66599999999999) ;
#11092 = CIRCLE('',#33244,1.66599999999999) ;
#11093 = CIRCLE('',#33246,2.05475) ;
#11094 = CIRCLE('',#33249,2.05475) ;
#11095 = CIRCLE('',#33251,2.05475) ;
#11096 = CIRCLE('',#33254,2.05475) ;
#11097 = CIRCLE('',#33256,1.666) ;
#11098 = CIRCLE('',#33258,1.666) ;
#11099 = CIRCLE('',#33260,1.666) ;
#11100 = CIRCLE('',#33262,1.666) ;
#11101 = CIRCLE('',#33264,1.666) ;
#11102 = CIRCLE('',#33266,1.666) ;
#11103 = CIRCLE('',#33268,2.05475) ;
#11104 = CIRCLE('',#33271,2.05475) ;
#11105 = CIRCLE('',#33273,2.05475) ;
#11106 = CIRCLE('',#33276,2.05475) ;
#11107 = CIRCLE('',#33278,1.66600000000001) ;
#11108 = CIRCLE('',#33280,1.66600000000001) ;
#11109 = CIRCLE('',#33282,1.66600000000001) ;
#11110 = CIRCLE('',#33284,1.66600000000001) ;
#11111 = CIRCLE('',#33286,1.66600000000001) ;
#11112 = CIRCLE('',#33288,1.66600000000001) ;
#11113 = CIRCLE('',#33306,0.5) ;
#11114 = CIRCLE('',#33307,0.5) ;
#11115 = CIRCLE('',#33309,2.) ;
#11116 = CIRCLE('',#33310,2.) ;
#11117 = CIRCLE('',#33312,2.) ;
#11118 = CIRCLE('',#33313,2.) ;
#11119 = CIRCLE('',#33315,2.) ;
#11120 = CIRCLE('',#33316,2.) ;
#11121 = CIRCLE('',#33318,2.) ;
#11122 = CIRCLE('',#33319,2.) ;
#11123 = CIRCLE('',#33321,0.5) ;
#11124 = CIRCLE('',#33322,2.) ;
#11125 = CIRCLE('',#33323,2.) ;
#11126 = CIRCLE('',#33325,2.) ;
#11127 = CIRCLE('',#33326,2.) ;
#11128 = CIRCLE('',#33328,1.) ;
#11129 = CIRCLE('',#33329,1.) ;
#11130 = CIRCLE('',#33331,2.) ;
#11131 = CIRCLE('',#33332,2.) ;
#11132 = CIRCLE('',#33333,5.) ;
#11133 = CIRCLE('',#33334,5.) ;
#11134 = CIRCLE('',#33335,1.65) ;
#11135 = CIRCLE('',#33336,1.65) ;
#11136 = CIRCLE('',#33338,0.5) ;
#11137 = CIRCLE('',#33339,0.5) ;
#11138 = CIRCLE('',#33341,2.) ;
#11139 = CIRCLE('',#33342,2.) ;
#11140 = CIRCLE('',#33343,2.) ;
#11141 = CIRCLE('',#33344,2.) ;
#11142 = CIRCLE('',#33345,1.65) ;
#11143 = CIRCLE('',#33346,1.65) ;
#11144 = CIRCLE('',#33347,0.125) ;
#11145 = CIRCLE('',#33348,0.125) ;
#11146 = CIRCLE('',#33349,0.125) ;
#11147 = CIRCLE('',#33350,0.125) ;
#11148 = CIRCLE('',#33351,5.) ;
#11149 = CIRCLE('',#33352,5.) ;
#11150 = CIRCLE('',#33354,2.) ;
#11151 = CIRCLE('',#33355,2.) ;
#11152 = CIRCLE('',#33356,2.75) ;
#11153 = CIRCLE('',#33357,5.25) ;
#11154 = CIRCLE('',#33358,5.25) ;
#11155 = CIRCLE('',#33359,2.75000000000003) ;
#11156 = CIRCLE('',#33361,2.) ;
#11157 = CIRCLE('',#33362,2.) ;
#11158 = CIRCLE('',#33363,2.) ;
#11159 = CIRCLE('',#33364,2.) ;
#11160 = CIRCLE('',#33365,0.250000000000004) ;
#11161 = CIRCLE('',#33366,0.250000000000012) ;
#11162 = CIRCLE('',#33367,0.250000000000003) ;
#11163 = CIRCLE('',#33368,0.249999999999986) ;
#11164 = CIRCLE('',#33369,5.25) ;
#11165 = CIRCLE('',#33370,5.25) ;
#11166 = CIRCLE('',#33371,2.75) ;
#11167 = CIRCLE('',#33372,2.7499999999968) ;
#11168 = CIRCLE('',#33374,2.) ;
#11169 = CIRCLE('',#33377,2.) ;
#11170 = CIRCLE('',#33379,2.) ;
#11171 = CIRCLE('',#33381,2.) ;
#11172 = CIRCLE('',#33383,0.5) ;
#11173 = CIRCLE('',#33384,0.5) ;
#11174 = CIRCLE('',#33391,2.) ;
#11175 = CIRCLE('',#33397,1.) ;
#11176 = CIRCLE('',#33398,1.) ;
#11177 = CIRCLE('',#33401,0.999999999999996) ;
#11178 = CIRCLE('',#33402,1.) ;
#11179 = CIRCLE('',#33404,0.999999404657181) ;
#11180 = CIRCLE('',#33405,4.) ;
#11181 = CIRCLE('',#33407,1.0000005953428) ;
#11182 = CIRCLE('',#33409,1.00000000000001) ;
#11183 = CIRCLE('',#33410,4.) ;
#11184 = CIRCLE('',#33412,1.) ;
#11185 = CIRCLE('',#33415,4.) ;
#11186 = CIRCLE('',#33418,4.) ;
#11187 = CIRCLE('',#33421,1.00000000000001) ;
#11188 = CIRCLE('',#33422,1.) ;
#11189 = CIRCLE('',#33424,0.999999404660006) ;
#11190 = CIRCLE('',#33425,4.) ;
#11191 = CIRCLE('',#33427,1.00000059533998) ;
#11192 = CIRCLE('',#33429,0.999999999999979) ;
#11193 = CIRCLE('',#33430,4.) ;
#11194 = CIRCLE('',#33432,1.) ;
#11195 = CIRCLE('',#33435,4.) ;
#11196 = CIRCLE('',#33438,4.) ;
#11197 = CIRCLE('',#33455,0.5) ;
#11198 = CIRCLE('',#33456,0.5) ;
#11199 = CIRCLE('',#33458,0.5) ;
#11200 = CIRCLE('',#33459,0.5) ;
#11201 = CIRCLE('',#33461,0.5) ;
#11202 = CIRCLE('',#33463,0.5) ;
#11203 = CIRCLE('',#33464,0.5) ;
#11204 = CIRCLE('',#33466,0.5) ;
#11205 = CIRCLE('',#33467,0.5) ;
#11206 = CIRCLE('',#33470,1.65) ;
#11207 = CIRCLE('',#33473,1.65) ;
#11208 = CIRCLE('',#33476,1.65) ;
#11209 = CIRCLE('',#33479,3.25) ;
#11210 = CIRCLE('',#33481,3.25) ;
#11211 = CIRCLE('',#33483,1.75) ;
#11212 = CIRCLE('',#33484,1.75) ;
#11213 = CIRCLE('',#33485,1.75) ;
#11214 = CIRCLE('',#33487,2.75) ;
#11215 = CIRCLE('',#33489,2.) ;
#11216 = CIRCLE('',#33490,2.) ;
#11217 = CIRCLE('',#33492,2.) ;
#11218 = CIRCLE('',#33493,2.) ;
#11219 = CIRCLE('',#33495,2.) ;
#11220 = CIRCLE('',#33496,2.) ;
#11221 = CIRCLE('',#33498,2.) ;
#11222 = CIRCLE('',#33499,2.) ;
#11223 = CIRCLE('',#33501,2.) ;
#11224 = CIRCLE('',#33502,2.) ;
#11225 = CIRCLE('',#33504,2.) ;
#11226 = CIRCLE('',#33505,2.) ;
#11227 = CIRCLE('',#33507,3.25) ;
#11228 = CIRCLE('',#33508,3.25) ;
#11229 = CIRCLE('',#33509,2.) ;
#11230 = CIRCLE('',#33511,3.25) ;
#11231 = CIRCLE('',#33530,3.25) ;
#11232 = CIRCLE('',#33536,2.) ;
#11233 = CIRCLE('',#33538,2.) ;
#11234 = CIRCLE('',#33540,2.) ;
#11235 = CIRCLE('',#33542,2.) ;
#11236 = CIRCLE('',#33544,2.) ;
#11237 = CIRCLE('',#33546,2.) ;
#11238 = CIRCLE('',#33548,3.25) ;
#11239 = CIRCLE('',#33550,3.25) ;
#11240 = CIRCLE('',#33551,2.) ;
#11241 = CIRCLE('',#33558,2.) ;
#11242 = CIRCLE('',#33559,2.) ;
#11243 = CIRCLE('',#33560,2.75) ;
#11244 = CIRCLE('',#33561,2.75) ;
#11245 = CIRCLE('',#33562,2.75) ;
#11246 = CIRCLE('',#33563,2.75) ;
#11247 = CIRCLE('',#33565,2.) ;
#11248 = CIRCLE('',#33566,2.) ;
#11249 = CIRCLE('',#33568,1.75) ;
#11250 = CIRCLE('',#33569,1.75) ;
#11251 = CIRCLE('',#33570,1.75) ;
#11252 = CIRCLE('',#33573,1.75) ;
#11253 = CIRCLE('',#33574,1.75) ;
#11254 = CIRCLE('',#33575,1.75) ;
#11255 = CIRCLE('',#33578,1.75) ;
#11256 = CIRCLE('',#33579,1.75) ;
#11257 = CIRCLE('',#33580,1.75) ;
#11258 = CIRCLE('',#33583,1.75) ;
#11259 = CIRCLE('',#33584,1.75) ;
#11260 = CIRCLE('',#33585,1.75) ;
#11261 = CIRCLE('',#33589,3.25) ;
#11262 = CIRCLE('',#33591,3.25) ;
#11263 = CIRCLE('',#33593,2.) ;
#11264 = CIRCLE('',#33604,3.25) ;
#11265 = CIRCLE('',#33605,3.25) ;
#11266 = CIRCLE('',#33615,3.25) ;
#11267 = CIRCLE('',#33616,3.25) ;
#11268 = CIRCLE('',#33618,3.25) ;
#11269 = CIRCLE('',#33620,3.25) ;
#11270 = CIRCLE('',#33622,2.) ;
#11271 = CIRCLE('',#33625,2.) ;
#11272 = CIRCLE('',#33628,3.25) ;
#11273 = CIRCLE('',#33629,3.25) ;
#11274 = CIRCLE('',#33633,1.65000070880266) ;
#11275 = CIRCLE('',#33634,1.65000070880266) ;
#11276 = CIRCLE('',#33641,0.125000000000002) ;
#11277 = CIRCLE('',#33643,0.124999999999993) ;
#11278 = CIRCLE('',#33645,0.125000000000002) ;
#11279 = CIRCLE('',#33646,0.125000000000028) ;
#11280 = CIRCLE('',#33648,0.125000000000011) ;
#11281 = CIRCLE('',#33650,0.125000000000002) ;
#11282 = CIRCLE('',#33651,0.124999999999957) ;
#11283 = CIRCLE('',#33653,0.125000000000002) ;
#11284 = CIRCLE('',#33655,0.124999999999975) ;
#11285 = CIRCLE('',#33656,0.125000000000028) ;
#11286 = CIRCLE('',#33659,0.125000000000011) ;
#11287 = CIRCLE('',#33660,0.125000000000028) ;
#11288 = CIRCLE('',#33665,2.) ;
#11289 = CIRCLE('',#33666,2.) ;
#11290 = CIRCLE('',#33668,2.) ;
#11291 = CIRCLE('',#33670,2.00000000000003) ;
#11292 = CIRCLE('',#33672,2.) ;
#11293 = CIRCLE('',#33675,1.99999999999999) ;
#11294 = CIRCLE('',#33677,1.99999999999998) ;
#11295 = CIRCLE('',#33679,2.) ;
#11296 = CIRCLE('',#33680,2.) ;
#11297 = CIRCLE('',#33681,2.) ;
#11298 = CIRCLE('',#33683,1.99999999999996) ;
#11299 = CIRCLE('',#33685,2.) ;
#11300 = CIRCLE('',#33686,2.) ;
#11301 = CIRCLE('',#33688,2.00000000000003) ;
#11302 = CIRCLE('',#33689,1.99999999999999) ;
#11303 = CIRCLE('',#33691,2.00000000000003) ;
#11304 = CIRCLE('',#33757,1.5) ;
#11305 = CIRCLE('',#33758,0.125) ;
#11306 = CIRCLE('',#33759,1.625) ;
#11307 = CIRCLE('',#33761,1.5) ;
#11308 = CIRCLE('',#33763,0.375) ;
#11309 = CIRCLE('',#33764,0.375) ;
#11310 = CIRCLE('',#33765,0.375) ;
#11311 = CIRCLE('',#33766,0.375) ;
#11312 = CIRCLE('',#33768,1.5) ;
#11313 = CIRCLE('',#33769,0.125) ;
#11314 = CIRCLE('',#33770,1.625) ;
#11315 = CIRCLE('',#33772,1.5) ;
#11316 = CIRCLE('',#33774,0.375) ;
#11317 = CIRCLE('',#33775,0.375) ;
#11318 = CIRCLE('',#33776,0.375) ;
#11319 = CIRCLE('',#33777,0.375) ;
#11320 = CIRCLE('',#33779,1.5) ;
#11321 = CIRCLE('',#33780,0.125) ;
#11322 = CIRCLE('',#33781,1.625) ;
#11323 = CIRCLE('',#33783,1.5) ;
#11324 = CIRCLE('',#33785,0.375) ;
#11325 = CIRCLE('',#33786,0.375) ;
#11326 = CIRCLE('',#33787,0.375) ;
#11327 = CIRCLE('',#33788,0.375) ;
#11328 = CIRCLE('',#33790,1.5) ;
#11329 = CIRCLE('',#33791,0.125) ;
#11330 = CIRCLE('',#33792,1.625) ;
#11331 = CIRCLE('',#33794,1.5) ;
#11332 = CIRCLE('',#33796,0.375) ;
#11333 = CIRCLE('',#33797,0.375) ;
#11334 = CIRCLE('',#33798,0.375) ;
#11335 = CIRCLE('',#33799,0.375) ;
#11336 = CIRCLE('',#33801,1.5) ;
#11337 = CIRCLE('',#33802,0.125) ;
#11338 = CIRCLE('',#33803,1.625) ;
#11339 = CIRCLE('',#33805,1.5) ;
#11340 = CIRCLE('',#33807,0.375) ;
#11341 = CIRCLE('',#33808,0.375) ;
#11342 = CIRCLE('',#33809,0.375) ;
#11343 = CIRCLE('',#33810,0.375) ;
#11344 = CIRCLE('',#33812,1.5) ;
#11345 = CIRCLE('',#33813,0.125) ;
#11346 = CIRCLE('',#33814,1.625) ;
#11347 = CIRCLE('',#33816,1.5) ;
#11348 = CIRCLE('',#33818,0.375) ;
#11349 = CIRCLE('',#33819,0.375) ;
#11350 = CIRCLE('',#33820,0.375) ;
#11351 = CIRCLE('',#33821,0.375) ;
#11352 = CIRCLE('',#33823,1.5) ;
#11353 = CIRCLE('',#33824,0.125) ;
#11354 = CIRCLE('',#33825,1.625) ;
#11355 = CIRCLE('',#33827,1.5) ;
#11356 = CIRCLE('',#33829,0.375) ;
#11357 = CIRCLE('',#33830,0.375) ;
#11358 = CIRCLE('',#33831,0.375) ;
#11359 = CIRCLE('',#33832,0.375) ;
#11360 = CIRCLE('',#33834,1.5) ;
#11361 = CIRCLE('',#33835,0.125) ;
#11362 = CIRCLE('',#33836,1.625) ;
#11363 = CIRCLE('',#33838,1.5) ;
#11364 = CIRCLE('',#33840,0.375) ;
#11365 = CIRCLE('',#33841,0.375) ;
#11366 = CIRCLE('',#33842,0.375) ;
#11367 = CIRCLE('',#33843,0.375) ;
#11368 = CIRCLE('',#33845,1.5) ;
#11369 = CIRCLE('',#33846,0.125) ;
#11370 = CIRCLE('',#33847,1.625) ;
#11371 = CIRCLE('',#33849,0.375) ;
#11372 = CIRCLE('',#33850,0.375) ;
#11373 = CIRCLE('',#33851,0.375) ;
#11374 = CIRCLE('',#33852,0.375) ;
#11375 = CIRCLE('',#33854,1.5) ;
#11376 = CIRCLE('',#33856,2.7325) ;
#11377 = CIRCLE('',#33858,2.7325) ;
#11378 = CIRCLE('',#33860,2.7325) ;
#11379 = CIRCLE('',#33862,2.7325) ;
#11380 = CIRCLE('',#33864,2.7325) ;
#11381 = CIRCLE('',#33866,2.7325) ;
#11382 = CIRCLE('',#33868,2.7325) ;
#11383 = CIRCLE('',#33870,2.7325) ;
#11384 = CIRCLE('',#33872,0.250000000000004) ;
#11385 = CIRCLE('',#33873,0.249999999999986) ;
#11386 = CIRCLE('',#33875,0.250000000000021) ;
#11387 = CIRCLE('',#33876,0.125) ;
#11388 = CIRCLE('',#33878,0.249999999999986) ;
#11389 = CIRCLE('',#33880,0.250000000000057) ;
#11390 = CIRCLE('',#33881,0.125) ;
#11391 = CIRCLE('',#33883,0.249999999999986) ;
#11392 = CIRCLE('',#33885,0.249999999999986) ;
#11393 = CIRCLE('',#33886,0.125) ;
#11394 = CIRCLE('',#33888,0.249999999999986) ;
#11395 = CIRCLE('',#33890,0.125) ;
#11396 = CIRCLE('',#33892,0.124999999999993) ;
#11397 = CIRCLE('',#33894,0.188499999999969) ;
#11398 = CIRCLE('',#33895,0.188499999999987) ;
#11399 = CIRCLE('',#33897,0.124999999999957) ;
#11400 = CIRCLE('',#33900,0.250000000000004) ;
#11401 = CIRCLE('',#33901,0.249999999999986) ;
#11402 = CIRCLE('',#33903,0.250000000000021) ;
#11403 = CIRCLE('',#33904,0.125) ;
#11404 = CIRCLE('',#33906,0.249999999999986) ;
#11405 = CIRCLE('',#33908,0.250000000000057) ;
#11406 = CIRCLE('',#33909,0.125) ;
#11407 = CIRCLE('',#33911,0.249999999999986) ;
#11408 = CIRCLE('',#33913,0.249999999999986) ;
#11409 = CIRCLE('',#33914,0.125) ;
#11410 = CIRCLE('',#33916,0.249999999999986) ;
#11411 = CIRCLE('',#33918,0.125) ;
#11412 = CIRCLE('',#33920,0.124999999999993) ;
#11413 = CIRCLE('',#33922,0.188499999999969) ;
#11414 = CIRCLE('',#33923,0.188499999999987) ;
#11415 = CIRCLE('',#33925,0.124999999999957) ;
#11416 = CIRCLE('',#33928,0.250000000000004) ;
#11417 = CIRCLE('',#33929,0.249999999999986) ;
#11418 = CIRCLE('',#33931,0.250000000000021) ;
#11419 = CIRCLE('',#33932,0.125) ;
#11420 = CIRCLE('',#33934,0.249999999999986) ;
#11421 = CIRCLE('',#33936,0.250000000000057) ;
#11422 = CIRCLE('',#33937,0.125) ;
#11423 = CIRCLE('',#33939,0.249999999999986) ;
#11424 = CIRCLE('',#33941,0.249999999999986) ;
#11425 = CIRCLE('',#33942,0.125) ;
#11426 = CIRCLE('',#33944,0.249999999999986) ;
#11427 = CIRCLE('',#33946,0.125) ;
#11428 = CIRCLE('',#33948,0.124999999999993) ;
#11429 = CIRCLE('',#33950,0.188499999999969) ;
#11430 = CIRCLE('',#33951,0.188499999999987) ;
#11431 = CIRCLE('',#33953,0.124999999999957) ;
#11432 = CIRCLE('',#33956,0.250000000000004) ;
#11433 = CIRCLE('',#33957,0.249999999999986) ;
#11434 = CIRCLE('',#33959,0.250000000000021) ;
#11435 = CIRCLE('',#33960,0.125) ;
#11436 = CIRCLE('',#33962,0.249999999999986) ;
#11437 = CIRCLE('',#33964,0.250000000000057) ;
#11438 = CIRCLE('',#33965,0.125) ;
#11439 = CIRCLE('',#33967,0.249999999999986) ;
#11440 = CIRCLE('',#33969,0.249999999999986) ;
#11441 = CIRCLE('',#33970,0.125) ;
#11442 = CIRCLE('',#33972,0.249999999999986) ;
#11443 = CIRCLE('',#33974,0.125) ;
#11444 = CIRCLE('',#33976,0.124999999999993) ;
#11445 = CIRCLE('',#33978,0.188499999999969) ;
#11446 = CIRCLE('',#33979,0.188499999999987) ;
#11447 = CIRCLE('',#33981,0.124999999999957) ;
#11448 = CIRCLE('',#33984,0.250000000000004) ;
#11449 = CIRCLE('',#33985,0.249999999999986) ;
#11450 = CIRCLE('',#33987,0.250000000000021) ;
#11451 = CIRCLE('',#33988,0.125) ;
#11452 = CIRCLE('',#33990,0.249999999999986) ;
#11453 = CIRCLE('',#33992,0.250000000000057) ;
#11454 = CIRCLE('',#33993,0.125) ;
#11455 = CIRCLE('',#33995,0.249999999999986) ;
#11456 = CIRCLE('',#33997,0.249999999999986) ;
#11457 = CIRCLE('',#33998,0.125) ;
#11458 = CIRCLE('',#34000,0.249999999999986) ;
#11459 = CIRCLE('',#34002,0.125) ;
#11460 = CIRCLE('',#34004,0.124999999999993) ;
#11461 = CIRCLE('',#34006,0.188499999999969) ;
#11462 = CIRCLE('',#34007,0.188499999999987) ;
#11463 = CIRCLE('',#34009,0.124999999999957) ;
#11464 = CIRCLE('',#34012,0.250000000000004) ;
#11465 = CIRCLE('',#34013,0.249999999999986) ;
#11466 = CIRCLE('',#34015,0.250000000000021) ;
#11467 = CIRCLE('',#34016,0.125) ;
#11468 = CIRCLE('',#34018,0.249999999999986) ;
#11469 = CIRCLE('',#34020,0.250000000000057) ;
#11470 = CIRCLE('',#34021,0.125) ;
#11471 = CIRCLE('',#34023,0.249999999999986) ;
#11472 = CIRCLE('',#34025,0.249999999999986) ;
#11473 = CIRCLE('',#34026,0.125) ;
#11474 = CIRCLE('',#34028,0.249999999999986) ;
#11475 = CIRCLE('',#34030,0.125) ;
#11476 = CIRCLE('',#34032,0.124999999999993) ;
#11477 = CIRCLE('',#34034,0.188499999999969) ;
#11478 = CIRCLE('',#34035,0.188499999999987) ;
#11479 = CIRCLE('',#34037,0.124999999999957) ;
#11480 = CIRCLE('',#34040,0.250000000000004) ;
#11481 = CIRCLE('',#34041,0.249999999999986) ;
#11482 = CIRCLE('',#34043,0.250000000000021) ;
#11483 = CIRCLE('',#34044,0.125) ;
#11484 = CIRCLE('',#34046,0.249999999999986) ;
#11485 = CIRCLE('',#34048,0.250000000000057) ;
#11486 = CIRCLE('',#34049,0.125) ;
#11487 = CIRCLE('',#34051,0.249999999999986) ;
#11488 = CIRCLE('',#34053,0.249999999999986) ;
#11489 = CIRCLE('',#34054,0.125) ;
#11490 = CIRCLE('',#34056,0.249999999999986) ;
#11491 = CIRCLE('',#34058,0.125) ;
#11492 = CIRCLE('',#34060,0.124999999999993) ;
#11493 = CIRCLE('',#34062,0.188499999999969) ;
#11494 = CIRCLE('',#34063,0.188499999999987) ;
#11495 = CIRCLE('',#34065,0.124999999999957) ;
#11496 = CIRCLE('',#34068,0.250000000000004) ;
#11497 = CIRCLE('',#34069,0.249999999999986) ;
#11498 = CIRCLE('',#34071,0.250000000000021) ;
#11499 = CIRCLE('',#34072,0.125) ;
#11500 = CIRCLE('',#34074,0.249999999999986) ;
#11501 = CIRCLE('',#34076,0.250000000000057) ;
#11502 = CIRCLE('',#34077,0.125) ;
#11503 = CIRCLE('',#34079,0.249999999999986) ;
#11504 = CIRCLE('',#34081,0.249999999999986) ;
#11505 = CIRCLE('',#34082,0.125) ;
#11506 = CIRCLE('',#34084,0.249999999999986) ;
#11507 = CIRCLE('',#34086,0.125) ;
#11508 = CIRCLE('',#34088,0.124999999999993) ;
#11509 = CIRCLE('',#34090,0.188499999999969) ;
#11510 = CIRCLE('',#34091,0.188499999999987) ;
#11511 = CIRCLE('',#34093,0.124999999999957) ;
#11512 = CIRCLE('',#34096,0.250000000000004) ;
#11513 = CIRCLE('',#34097,0.249999999999986) ;
#11514 = CIRCLE('',#34099,0.250000000000021) ;
#11515 = CIRCLE('',#34100,0.125) ;
#11516 = CIRCLE('',#34102,0.249999999999986) ;
#11517 = CIRCLE('',#34104,0.250000000000057) ;
#11518 = CIRCLE('',#34105,0.125) ;
#11519 = CIRCLE('',#34107,0.249999999999986) ;
#11520 = CIRCLE('',#34109,0.249999999999986) ;
#11521 = CIRCLE('',#34110,0.125) ;
#11522 = CIRCLE('',#34112,0.249999999999986) ;
#11523 = CIRCLE('',#34114,0.125) ;
#11524 = CIRCLE('',#34116,0.124999999999993) ;
#11525 = CIRCLE('',#34118,0.188499999999987) ;
#11526 = CIRCLE('',#34119,0.188499999999969) ;
#11527 = CIRCLE('',#34121,0.124999999999957) ;
#11528 = CIRCLE('',#34124,0.249999999999999) ;
#11529 = CIRCLE('',#34125,0.249999999999986) ;
#11530 = CIRCLE('',#34127,0.249999999999986) ;
#11531 = CIRCLE('',#34128,0.375) ;
#11532 = CIRCLE('',#34129,0.125) ;
#11533 = CIRCLE('',#34131,0.24999999999995) ;
#11534 = CIRCLE('',#34133,0.249999999999986) ;
#11535 = CIRCLE('',#34134,0.375) ;
#11536 = CIRCLE('',#34135,0.125) ;
#11537 = CIRCLE('',#34137,0.249999999999986) ;
#11538 = CIRCLE('',#34139,0.249999999999986) ;
#11539 = CIRCLE('',#34140,0.375) ;
#11540 = CIRCLE('',#34141,0.125) ;
#11541 = CIRCLE('',#34143,0.249999999999986) ;
#11542 = CIRCLE('',#34145,0.375) ;
#11543 = CIRCLE('',#34146,0.125) ;
#11544 = CIRCLE('',#34148,0.124999999999993) ;
#11545 = CIRCLE('',#34151,0.124999999999993) ;
#11546 = CIRCLE('',#34154,0.249999999999999) ;
#11547 = CIRCLE('',#34155,0.249999999999986) ;
#11548 = CIRCLE('',#34157,0.249999999999986) ;
#11549 = CIRCLE('',#34158,0.375) ;
#11550 = CIRCLE('',#34159,0.125) ;
#11551 = CIRCLE('',#34161,0.24999999999995) ;
#11552 = CIRCLE('',#34163,0.249999999999986) ;
#11553 = CIRCLE('',#34164,0.375) ;
#11554 = CIRCLE('',#34165,0.125) ;
#11555 = CIRCLE('',#34167,0.249999999999986) ;
#11556 = CIRCLE('',#34169,0.249999999999986) ;
#11557 = CIRCLE('',#34170,0.375) ;
#11558 = CIRCLE('',#34171,0.125) ;
#11559 = CIRCLE('',#34173,0.249999999999986) ;
#11560 = CIRCLE('',#34175,0.375) ;
#11561 = CIRCLE('',#34176,0.125) ;
#11562 = CIRCLE('',#34178,0.124999999999993) ;
#11563 = CIRCLE('',#34181,0.124999999999993) ;
#11564 = CIRCLE('',#34184,0.249999999999999) ;
#11565 = CIRCLE('',#34185,0.249999999999986) ;
#11566 = CIRCLE('',#34187,0.249999999999986) ;
#11567 = CIRCLE('',#34188,0.375) ;
#11568 = CIRCLE('',#34189,0.125) ;
#11569 = CIRCLE('',#34191,0.24999999999995) ;
#11570 = CIRCLE('',#34193,0.249999999999986) ;
#11571 = CIRCLE('',#34194,0.375) ;
#11572 = CIRCLE('',#34195,0.125) ;
#11573 = CIRCLE('',#34197,0.249999999999986) ;
#11574 = CIRCLE('',#34199,0.249999999999986) ;
#11575 = CIRCLE('',#34200,0.375) ;
#11576 = CIRCLE('',#34201,0.125) ;
#11577 = CIRCLE('',#34203,0.249999999999986) ;
#11578 = CIRCLE('',#34205,0.375) ;
#11579 = CIRCLE('',#34206,0.125) ;
#11580 = CIRCLE('',#34208,0.124999999999993) ;
#11581 = CIRCLE('',#34211,0.124999999999993) ;
#11582 = CIRCLE('',#34214,0.249999999999999) ;
#11583 = CIRCLE('',#34215,0.249999999999986) ;
#11584 = CIRCLE('',#34217,0.249999999999986) ;
#11585 = CIRCLE('',#34218,0.375) ;
#11586 = CIRCLE('',#34219,0.125) ;
#11587 = CIRCLE('',#34221,0.24999999999995) ;
#11588 = CIRCLE('',#34223,0.249999999999986) ;
#11589 = CIRCLE('',#34224,0.375) ;
#11590 = CIRCLE('',#34225,0.125) ;
#11591 = CIRCLE('',#34227,0.249999999999986) ;
#11592 = CIRCLE('',#34229,0.249999999999986) ;
#11593 = CIRCLE('',#34230,0.375) ;
#11594 = CIRCLE('',#34231,0.125) ;
#11595 = CIRCLE('',#34233,0.249999999999986) ;
#11596 = CIRCLE('',#34235,0.375) ;
#11597 = CIRCLE('',#34236,0.125) ;
#11598 = CIRCLE('',#34238,0.124999999999993) ;
#11599 = CIRCLE('',#34241,0.124999999999993) ;
#11600 = CIRCLE('',#34244,0.249999999999999) ;
#11601 = CIRCLE('',#34245,0.249999999999986) ;
#11602 = CIRCLE('',#34247,0.249999999999986) ;
#11603 = CIRCLE('',#34248,0.375) ;
#11604 = CIRCLE('',#34249,0.125) ;
#11605 = CIRCLE('',#34251,0.24999999999995) ;
#11606 = CIRCLE('',#34253,0.249999999999986) ;
#11607 = CIRCLE('',#34254,0.375) ;
#11608 = CIRCLE('',#34255,0.125) ;
#11609 = CIRCLE('',#34257,0.249999999999986) ;
#11610 = CIRCLE('',#34259,0.249999999999986) ;
#11611 = CIRCLE('',#34260,0.375) ;
#11612 = CIRCLE('',#34261,0.125) ;
#11613 = CIRCLE('',#34263,0.249999999999986) ;
#11614 = CIRCLE('',#34265,0.375) ;
#11615 = CIRCLE('',#34266,0.125) ;
#11616 = CIRCLE('',#34268,0.124999999999993) ;
#11617 = CIRCLE('',#34271,0.124999999999993) ;
#11618 = CIRCLE('',#34274,0.249999999999999) ;
#11619 = CIRCLE('',#34275,0.249999999999986) ;
#11620 = CIRCLE('',#34277,0.249999999999986) ;
#11621 = CIRCLE('',#34278,0.375) ;
#11622 = CIRCLE('',#34279,0.125) ;
#11623 = CIRCLE('',#34281,0.24999999999995) ;
#11624 = CIRCLE('',#34283,0.249999999999986) ;
#11625 = CIRCLE('',#34284,0.375) ;
#11626 = CIRCLE('',#34285,0.125) ;
#11627 = CIRCLE('',#34287,0.249999999999986) ;
#11628 = CIRCLE('',#34289,0.249999999999986) ;
#11629 = CIRCLE('',#34290,0.375) ;
#11630 = CIRCLE('',#34291,0.125) ;
#11631 = CIRCLE('',#34293,0.249999999999986) ;
#11632 = CIRCLE('',#34295,0.375) ;
#11633 = CIRCLE('',#34296,0.125) ;
#11634 = CIRCLE('',#34298,0.124999999999993) ;
#11635 = CIRCLE('',#34301,0.124999999999993) ;
#11636 = CIRCLE('',#34304,0.249999999999999) ;
#11637 = CIRCLE('',#34305,0.249999999999986) ;
#11638 = CIRCLE('',#34307,0.249999999999986) ;
#11639 = CIRCLE('',#34308,0.375) ;
#11640 = CIRCLE('',#34309,0.125) ;
#11641 = CIRCLE('',#34311,0.24999999999995) ;
#11642 = CIRCLE('',#34313,0.249999999999986) ;
#11643 = CIRCLE('',#34314,0.375) ;
#11644 = CIRCLE('',#34315,0.125) ;
#11645 = CIRCLE('',#34317,0.249999999999986) ;
#11646 = CIRCLE('',#34319,0.249999999999986) ;
#11647 = CIRCLE('',#34320,0.375) ;
#11648 = CIRCLE('',#34321,0.125) ;
#11649 = CIRCLE('',#34323,0.249999999999986) ;
#11650 = CIRCLE('',#34325,0.375) ;
#11651 = CIRCLE('',#34326,0.125) ;
#11652 = CIRCLE('',#34328,0.124999999999993) ;
#11653 = CIRCLE('',#34331,0.124999999999993) ;
#11654 = CIRCLE('',#34334,0.249999999999999) ;
#11655 = CIRCLE('',#34335,0.249999999999986) ;
#11656 = CIRCLE('',#34337,0.249999999999986) ;
#11657 = CIRCLE('',#34338,0.375) ;
#11658 = CIRCLE('',#34339,0.125) ;
#11659 = CIRCLE('',#34341,0.24999999999995) ;
#11660 = CIRCLE('',#34343,0.249999999999986) ;
#11661 = CIRCLE('',#34344,0.375) ;
#11662 = CIRCLE('',#34345,0.125) ;
#11663 = CIRCLE('',#34347,0.249999999999986) ;
#11664 = CIRCLE('',#34349,0.249999999999986) ;
#11665 = CIRCLE('',#34350,0.375) ;
#11666 = CIRCLE('',#34351,0.125) ;
#11667 = CIRCLE('',#34353,0.249999999999986) ;
#11668 = CIRCLE('',#34355,0.375) ;
#11669 = CIRCLE('',#34356,0.125) ;
#11670 = CIRCLE('',#34358,0.124999999999993) ;
#11671 = CIRCLE('',#34361,0.124999999999993) ;
#11672 = CIRCLE('',#34364,0.249999999999999) ;
#11673 = CIRCLE('',#34365,0.249999999999915) ;
#11674 = CIRCLE('',#34367,0.249999999999986) ;
#11675 = CIRCLE('',#34368,0.375) ;
#11676 = CIRCLE('',#34369,0.125) ;
#11677 = CIRCLE('',#34371,0.24999999999995) ;
#11678 = CIRCLE('',#34373,0.249999999999986) ;
#11679 = CIRCLE('',#34374,0.375) ;
#11680 = CIRCLE('',#34375,0.125) ;
#11681 = CIRCLE('',#34377,0.249999999999986) ;
#11682 = CIRCLE('',#34379,0.249999999999986) ;
#11683 = CIRCLE('',#34380,0.375) ;
#11684 = CIRCLE('',#34381,0.125) ;
#11685 = CIRCLE('',#34383,0.249999999999986) ;
#11686 = CIRCLE('',#34385,0.375) ;
#11687 = CIRCLE('',#34386,0.125) ;
#11688 = CIRCLE('',#34388,0.124999999999993) ;
#11689 = CIRCLE('',#34390,0.188499999999987) ;
#11690 = CIRCLE('',#34391,0.188499999999987) ;
#11691 = CIRCLE('',#34393,0.124999999999993) ;
#11692 = CIRCLE('',#34396,0.249999999999999) ;
#11693 = CIRCLE('',#34397,0.249999999999915) ;
#11694 = CIRCLE('',#34399,0.249999999999986) ;
#11695 = CIRCLE('',#34400,0.375) ;
#11696 = CIRCLE('',#34401,0.125) ;
#11697 = CIRCLE('',#34403,0.24999999999995) ;
#11698 = CIRCLE('',#34405,0.249999999999986) ;
#11699 = CIRCLE('',#34406,0.375) ;
#11700 = CIRCLE('',#34407,0.125) ;
#11701 = CIRCLE('',#34409,0.249999999999986) ;
#11702 = CIRCLE('',#34411,0.249999999999986) ;
#11703 = CIRCLE('',#34412,0.375) ;
#11704 = CIRCLE('',#34413,0.125) ;
#11705 = CIRCLE('',#34415,0.249999999999986) ;
#11706 = CIRCLE('',#34417,0.375) ;
#11707 = CIRCLE('',#34418,0.125) ;
#11708 = CIRCLE('',#34420,0.124999999999993) ;
#11709 = CIRCLE('',#34422,0.188499999999987) ;
#11710 = CIRCLE('',#34423,0.188499999999987) ;
#11711 = CIRCLE('',#34425,0.124999999999993) ;
#11712 = CIRCLE('',#34428,0.249999999999999) ;
#11713 = CIRCLE('',#34429,0.249999999999915) ;
#11714 = CIRCLE('',#34431,0.249999999999986) ;
#11715 = CIRCLE('',#34432,0.375) ;
#11716 = CIRCLE('',#34433,0.125) ;
#11717 = CIRCLE('',#34435,0.24999999999995) ;
#11718 = CIRCLE('',#34437,0.249999999999986) ;
#11719 = CIRCLE('',#34438,0.375) ;
#11720 = CIRCLE('',#34439,0.125) ;
#11721 = CIRCLE('',#34441,0.249999999999986) ;
#11722 = CIRCLE('',#34443,0.249999999999986) ;
#11723 = CIRCLE('',#34444,0.375) ;
#11724 = CIRCLE('',#34445,0.125) ;
#11725 = CIRCLE('',#34447,0.249999999999986) ;
#11726 = CIRCLE('',#34449,0.375) ;
#11727 = CIRCLE('',#34450,0.125) ;
#11728 = CIRCLE('',#34452,0.124999999999993) ;
#11729 = CIRCLE('',#34454,0.188499999999987) ;
#11730 = CIRCLE('',#34455,0.188499999999987) ;
#11731 = CIRCLE('',#34457,0.124999999999993) ;
#11732 = CIRCLE('',#34460,0.249999999999999) ;
#11733 = CIRCLE('',#34461,0.249999999999915) ;
#11734 = CIRCLE('',#34463,0.249999999999986) ;
#11735 = CIRCLE('',#34464,0.375) ;
#11736 = CIRCLE('',#34465,0.125) ;
#11737 = CIRCLE('',#34467,0.24999999999995) ;
#11738 = CIRCLE('',#34469,0.249999999999986) ;
#11739 = CIRCLE('',#34470,0.375) ;
#11740 = CIRCLE('',#34471,0.125) ;
#11741 = CIRCLE('',#34473,0.249999999999986) ;
#11742 = CIRCLE('',#34475,0.249999999999986) ;
#11743 = CIRCLE('',#34476,0.375) ;
#11744 = CIRCLE('',#34477,0.125) ;
#11745 = CIRCLE('',#34479,0.249999999999986) ;
#11746 = CIRCLE('',#34481,0.375) ;
#11747 = CIRCLE('',#34482,0.125) ;
#11748 = CIRCLE('',#34484,0.124999999999993) ;
#11749 = CIRCLE('',#34486,0.188499999999987) ;
#11750 = CIRCLE('',#34487,0.188499999999987) ;
#11751 = CIRCLE('',#34489,0.124999999999993) ;
#11752 = CIRCLE('',#34492,0.249999999999999) ;
#11753 = CIRCLE('',#34493,0.249999999999915) ;
#11754 = CIRCLE('',#34495,0.249999999999986) ;
#11755 = CIRCLE('',#34496,0.375) ;
#11756 = CIRCLE('',#34497,0.125) ;
#11757 = CIRCLE('',#34499,0.24999999999995) ;
#11758 = CIRCLE('',#34501,0.249999999999986) ;
#11759 = CIRCLE('',#34502,0.375) ;
#11760 = CIRCLE('',#34503,0.125) ;
#11761 = CIRCLE('',#34505,0.249999999999986) ;
#11762 = CIRCLE('',#34507,0.249999999999986) ;
#11763 = CIRCLE('',#34508,0.375) ;
#11764 = CIRCLE('',#34509,0.125) ;
#11765 = CIRCLE('',#34511,0.249999999999986) ;
#11766 = CIRCLE('',#34513,0.375) ;
#11767 = CIRCLE('',#34514,0.125) ;
#11768 = CIRCLE('',#34516,0.124999999999993) ;
#11769 = CIRCLE('',#34518,0.188499999999987) ;
#11770 = CIRCLE('',#34519,0.188499999999987) ;
#11771 = CIRCLE('',#34521,0.124999999999993) ;
#11772 = CIRCLE('',#34524,0.249999999999999) ;
#11773 = CIRCLE('',#34525,0.249999999999915) ;
#11774 = CIRCLE('',#34527,0.249999999999986) ;
#11775 = CIRCLE('',#34528,0.375) ;
#11776 = CIRCLE('',#34529,0.125) ;
#11777 = CIRCLE('',#34531,0.24999999999995) ;
#11778 = CIRCLE('',#34533,0.249999999999986) ;
#11779 = CIRCLE('',#34534,0.375) ;
#11780 = CIRCLE('',#34535,0.125) ;
#11781 = CIRCLE('',#34537,0.249999999999986) ;
#11782 = CIRCLE('',#34539,0.249999999999986) ;
#11783 = CIRCLE('',#34540,0.375) ;
#11784 = CIRCLE('',#34541,0.125) ;
#11785 = CIRCLE('',#34543,0.249999999999986) ;
#11786 = CIRCLE('',#34545,0.375) ;
#11787 = CIRCLE('',#34546,0.125) ;
#11788 = CIRCLE('',#34548,0.124999999999993) ;
#11789 = CIRCLE('',#34550,0.188499999999987) ;
#11790 = CIRCLE('',#34551,0.188499999999987) ;
#11791 = CIRCLE('',#34553,0.124999999999993) ;
#11792 = CIRCLE('',#34556,0.249999999999999) ;
#11793 = CIRCLE('',#34557,0.249999999999915) ;
#11794 = CIRCLE('',#34559,0.249999999999986) ;
#11795 = CIRCLE('',#34560,0.375) ;
#11796 = CIRCLE('',#34561,0.125) ;
#11797 = CIRCLE('',#34563,0.24999999999995) ;
#11798 = CIRCLE('',#34565,0.249999999999986) ;
#11799 = CIRCLE('',#34566,0.375) ;
#11800 = CIRCLE('',#34567,0.125) ;
#11801 = CIRCLE('',#34569,0.249999999999986) ;
#11802 = CIRCLE('',#34571,0.249999999999986) ;
#11803 = CIRCLE('',#34572,0.375) ;
#11804 = CIRCLE('',#34573,0.125) ;
#11805 = CIRCLE('',#34575,0.249999999999986) ;
#11806 = CIRCLE('',#34577,0.375) ;
#11807 = CIRCLE('',#34578,0.125) ;
#11808 = CIRCLE('',#34580,0.124999999999993) ;
#11809 = CIRCLE('',#34582,0.188499999999987) ;
#11810 = CIRCLE('',#34583,0.188499999999987) ;
#11811 = CIRCLE('',#34585,0.124999999999993) ;
#11812 = CIRCLE('',#34588,0.249999999999999) ;
#11813 = CIRCLE('',#34589,0.249999999999915) ;
#11814 = CIRCLE('',#34591,0.249999999999986) ;
#11815 = CIRCLE('',#34592,0.375) ;
#11816 = CIRCLE('',#34593,0.125) ;
#11817 = CIRCLE('',#34595,0.24999999999995) ;
#11818 = CIRCLE('',#34597,0.249999999999986) ;
#11819 = CIRCLE('',#34598,0.375) ;
#11820 = CIRCLE('',#34599,0.125) ;
#11821 = CIRCLE('',#34601,0.249999999999986) ;
#11822 = CIRCLE('',#34603,0.249999999999986) ;
#11823 = CIRCLE('',#34604,0.375) ;
#11824 = CIRCLE('',#34605,0.125) ;
#11825 = CIRCLE('',#34607,0.249999999999986) ;
#11826 = CIRCLE('',#34609,0.375) ;
#11827 = CIRCLE('',#34610,0.125) ;
#11828 = CIRCLE('',#34612,0.124999999999993) ;
#11829 = CIRCLE('',#34614,0.188499999999987) ;
#11830 = CIRCLE('',#34615,0.188499999999987) ;
#11831 = CIRCLE('',#34617,0.124999999999993) ;
#11832 = CIRCLE('',#34620,0.249999999999999) ;
#11833 = CIRCLE('',#34621,0.249999999999986) ;
#11834 = CIRCLE('',#34623,0.249999999999986) ;
#11835 = CIRCLE('',#34624,0.375) ;
#11836 = CIRCLE('',#34625,0.125) ;
#11837 = CIRCLE('',#34627,0.24999999999995) ;
#11838 = CIRCLE('',#34629,0.249999999999986) ;
#11839 = CIRCLE('',#34630,0.375) ;
#11840 = CIRCLE('',#34631,0.125) ;
#11841 = CIRCLE('',#34633,0.249999999999986) ;
#11842 = CIRCLE('',#34635,0.249999999999986) ;
#11843 = CIRCLE('',#34636,0.375) ;
#11844 = CIRCLE('',#34637,0.125) ;
#11845 = CIRCLE('',#34639,0.249999999999986) ;
#11846 = CIRCLE('',#34641,0.375) ;
#11847 = CIRCLE('',#34642,0.125) ;
#11848 = CIRCLE('',#34644,0.124999999999993) ;
#11849 = CIRCLE('',#34647,0.124999999999993) ;
#11850 = CIRCLE('',#34650,0.375) ;
#11851 = CIRCLE('',#34651,0.375) ;
#11852 = CIRCLE('',#34652,0.375) ;
#11853 = CIRCLE('',#34653,0.375) ;
#11854 = CIRCLE('',#34654,2.88334137894263) ;
#11855 = CIRCLE('',#34656,0.249999999999999) ;
#11856 = CIRCLE('',#34657,0.249999999999915) ;
#11857 = CIRCLE('',#34659,0.249999999999986) ;
#11858 = CIRCLE('',#34660,0.125) ;
#11859 = CIRCLE('',#34662,0.24999999999995) ;
#11860 = CIRCLE('',#34664,0.249999999999986) ;
#11861 = CIRCLE('',#34665,0.125) ;
#11862 = CIRCLE('',#34667,0.249999999999986) ;
#11863 = CIRCLE('',#34669,0.249999999999986) ;
#11864 = CIRCLE('',#34670,0.125) ;
#11865 = CIRCLE('',#34672,0.249999999999986) ;
#11866 = CIRCLE('',#34674,0.125) ;
#11867 = CIRCLE('',#34676,0.124999999999993) ;
#11868 = CIRCLE('',#34678,0.188499999999987) ;
#11869 = CIRCLE('',#34679,0.188499999999987) ;
#11870 = CIRCLE('',#34681,0.124999999999993) ;
#11871 = CIRCLE('',#34685,0.124999999999993) ;
#11872 = CIRCLE('',#34687,0.124999999999993) ;
#11873 = CIRCLE('',#34690,0.125000000000006) ;
#11874 = CIRCLE('',#34692,0.124999999999993) ;
#11875 = CIRCLE('',#34695,2.7325) ;
#11876 = CIRCLE('',#34697,0.124999999999993) ;
#11877 = CIRCLE('',#34699,0.124999999999993) ;
#11878 = CIRCLE('',#34700,0.124999999999993) ;
#11879 = CIRCLE('',#34702,0.0634999999999941) ;
#11880 = CIRCLE('',#34703,0.124999999999993) ;
#11881 = CIRCLE('',#34705,0.124999999999993) ;
#11882 = CIRCLE('',#34707,0.0634999999999764) ;
#11883 = CIRCLE('',#34708,0.124999999999993) ;
#11884 = CIRCLE('',#34710,0.0634999999999941) ;
#11885 = CIRCLE('',#34711,0.124999999999993) ;
#11886 = CIRCLE('',#34712,0.124999999999993) ;
#11887 = CIRCLE('',#34715,0.125000000000028) ;
#11888 = CIRCLE('',#34717,0.0634999999999941) ;
#11889 = CIRCLE('',#34718,0.124999999999993) ;
#11890 = CIRCLE('',#34720,0.124999999999993) ;
#11891 = CIRCLE('',#34723,0.124999999999993) ;
#11892 = CIRCLE('',#34728,0.124999999999993) ;
#11893 = CIRCLE('',#34729,0.124999999999993) ;
#11894 = CIRCLE('',#34737,0.124999999999993) ;
#11895 = CIRCLE('',#34738,0.125000000000011) ;
#11896 = CIRCLE('',#34740,0.124999999999993) ;
#11897 = CIRCLE('',#34741,0.125000000000002) ;
#11898 = CIRCLE('',#34744,0.124999999999993) ;
#11899 = CIRCLE('',#34746,0.125000000000011) ;
#11900 = CIRCLE('',#34748,0.124999999999993) ;
#11901 = CIRCLE('',#34749,0.125000000000011) ;
#11902 = CIRCLE('',#34753,0.124999999999993) ;
#11903 = CIRCLE('',#34755,0.124999999999993) ;
#11904 = CIRCLE('',#34756,0.124999999999993) ;
#11905 = CIRCLE('',#34758,0.0634999999999941) ;
#11906 = CIRCLE('',#34759,0.124999999999993) ;
#11907 = CIRCLE('',#34761,0.124999999999993) ;
#11908 = CIRCLE('',#34763,0.0634999999999764) ;
#11909 = CIRCLE('',#34764,0.124999999999993) ;
#11910 = CIRCLE('',#34766,0.0634999999999941) ;
#11911 = CIRCLE('',#34767,0.124999999999993) ;
#11912 = CIRCLE('',#34768,0.124999999999993) ;
#11913 = CIRCLE('',#34771,0.125000000000028) ;
#11914 = CIRCLE('',#34773,0.0634999999999941) ;
#11915 = CIRCLE('',#34774,0.124999999999993) ;
#11916 = CIRCLE('',#34776,0.124999999999993) ;
#11917 = CIRCLE('',#34779,0.124999999999993) ;
#11918 = CIRCLE('',#34782,0.124999999999993) ;
#11919 = CIRCLE('',#34785,0.124999999999993) ;
#11920 = CIRCLE('',#34786,0.124999999999993) ;
#11921 = CIRCLE('',#34788,0.124999999999993) ;
#11922 = CIRCLE('',#34795,0.124999999999993) ;
#11923 = CIRCLE('',#34796,0.125000000000011) ;
#11924 = CIRCLE('',#34797,0.125000000000006) ;
#11925 = CIRCLE('',#34799,0.124999999999993) ;
#11926 = CIRCLE('',#34800,0.125000000000002) ;
#11927 = CIRCLE('',#34801,0.124999999999993) ;
#11928 = CIRCLE('',#34804,0.124999999999993) ;
#11929 = CIRCLE('',#34806,0.125000000000011) ;
#11930 = CIRCLE('',#34808,0.124999999999993) ;
#11931 = CIRCLE('',#34809,0.125000000000011) ;
#11932 = CIRCLE('',#34813,0.124999999999993) ;
#11933 = CIRCLE('',#34815,0.124999999999993) ;
#11934 = CIRCLE('',#34816,0.124999999999993) ;
#11935 = CIRCLE('',#34818,0.0634999999999941) ;
#11936 = CIRCLE('',#34819,0.124999999999993) ;
#11937 = CIRCLE('',#34821,0.124999999999993) ;
#11938 = CIRCLE('',#34823,0.0634999999999764) ;
#11939 = CIRCLE('',#34824,0.124999999999993) ;
#11940 = CIRCLE('',#34826,0.0634999999999941) ;
#11941 = CIRCLE('',#34827,0.124999999999993) ;
#11942 = CIRCLE('',#34828,0.124999999999993) ;
#11943 = CIRCLE('',#34831,0.125000000000028) ;
#11944 = CIRCLE('',#34833,0.0634999999999941) ;
#11945 = CIRCLE('',#34834,0.124999999999993) ;
#11946 = CIRCLE('',#34836,0.124999999999993) ;
#11947 = CIRCLE('',#34839,0.124999999999993) ;
#11948 = CIRCLE('',#34842,0.124999999999993) ;
#11949 = CIRCLE('',#34845,0.124999999999993) ;
#11950 = CIRCLE('',#34846,0.124999999999993) ;
#11951 = CIRCLE('',#34848,0.124999999999993) ;
#11952 = CIRCLE('',#34855,0.124999999999993) ;
#11953 = CIRCLE('',#34856,0.125000000000011) ;
#11954 = CIRCLE('',#34857,0.125000000000006) ;
#11955 = CIRCLE('',#34859,0.124999999999993) ;
#11956 = CIRCLE('',#34860,0.125000000000002) ;
#11957 = CIRCLE('',#34861,0.124999999999993) ;
#11958 = CIRCLE('',#34864,0.124999999999993) ;
#11959 = CIRCLE('',#34866,0.125000000000011) ;
#11960 = CIRCLE('',#34868,0.124999999999993) ;
#11961 = CIRCLE('',#34869,0.125000000000011) ;
#11962 = CIRCLE('',#34873,0.124999999999993) ;
#11963 = CIRCLE('',#34875,0.124999999999993) ;
#11964 = CIRCLE('',#34876,0.124999999999993) ;
#11965 = CIRCLE('',#34878,0.0634999999999941) ;
#11966 = CIRCLE('',#34879,0.124999999999993) ;
#11967 = CIRCLE('',#34881,0.124999999999993) ;
#11968 = CIRCLE('',#34883,0.0634999999999764) ;
#11969 = CIRCLE('',#34884,0.124999999999993) ;
#11970 = CIRCLE('',#34886,0.0634999999999941) ;
#11971 = CIRCLE('',#34887,0.124999999999993) ;
#11972 = CIRCLE('',#34888,0.124999999999993) ;
#11973 = CIRCLE('',#34891,0.125000000000028) ;
#11974 = CIRCLE('',#34893,0.0634999999999941) ;
#11975 = CIRCLE('',#34894,0.124999999999993) ;
#11976 = CIRCLE('',#34896,0.124999999999993) ;
#11977 = CIRCLE('',#34899,0.124999999999993) ;
#11978 = CIRCLE('',#34902,0.124999999999993) ;
#11979 = CIRCLE('',#34905,0.124999999999993) ;
#11980 = CIRCLE('',#34906,0.124999999999993) ;
#11981 = CIRCLE('',#34908,0.124999999999993) ;
#11982 = CIRCLE('',#34915,0.124999999999993) ;
#11983 = CIRCLE('',#34916,0.125000000000011) ;
#11984 = CIRCLE('',#34917,0.125000000000006) ;
#11985 = CIRCLE('',#34919,0.124999999999993) ;
#11986 = CIRCLE('',#34920,0.125000000000002) ;
#11987 = CIRCLE('',#34921,0.124999999999993) ;
#11988 = CIRCLE('',#34924,0.124999999999993) ;
#11989 = CIRCLE('',#34926,0.125000000000011) ;
#11990 = CIRCLE('',#34928,0.124999999999993) ;
#11991 = CIRCLE('',#34929,0.125000000000011) ;
#11992 = CIRCLE('',#34933,0.124999999999993) ;
#11993 = CIRCLE('',#34935,0.124999999999993) ;
#11994 = CIRCLE('',#34936,0.124999999999993) ;
#11995 = CIRCLE('',#34938,0.0634999999999941) ;
#11996 = CIRCLE('',#34939,0.124999999999993) ;
#11997 = CIRCLE('',#34941,0.124999999999993) ;
#11998 = CIRCLE('',#34943,0.0634999999999764) ;
#11999 = CIRCLE('',#34944,0.124999999999993) ;
#12000 = CIRCLE('',#34946,0.0634999999999941) ;
#12001 = CIRCLE('',#34947,0.124999999999993) ;
#12002 = CIRCLE('',#34948,0.124999999999993) ;
#12003 = CIRCLE('',#34951,0.125000000000028) ;
#12004 = CIRCLE('',#34953,0.0634999999999941) ;
#12005 = CIRCLE('',#34954,0.124999999999993) ;
#12006 = CIRCLE('',#34956,0.124999999999993) ;
#12007 = CIRCLE('',#34959,0.124999999999993) ;
#12008 = CIRCLE('',#34962,0.124999999999993) ;
#12009 = CIRCLE('',#34965,0.124999999999993) ;
#12010 = CIRCLE('',#34966,0.124999999999993) ;
#12011 = CIRCLE('',#34968,0.124999999999993) ;
#12012 = CIRCLE('',#34975,0.124999999999993) ;
#12013 = CIRCLE('',#34976,0.125000000000011) ;
#12014 = CIRCLE('',#34977,0.125000000000006) ;
#12015 = CIRCLE('',#34979,0.124999999999993) ;
#12016 = CIRCLE('',#34980,0.125000000000002) ;
#12017 = CIRCLE('',#34981,0.124999999999993) ;
#12018 = CIRCLE('',#34984,0.124999999999993) ;
#12019 = CIRCLE('',#34986,0.125000000000011) ;
#12020 = CIRCLE('',#34988,0.124999999999993) ;
#12021 = CIRCLE('',#34989,0.125000000000011) ;
#12022 = CIRCLE('',#34993,0.124999999999993) ;
#12023 = CIRCLE('',#34995,0.124999999999993) ;
#12024 = CIRCLE('',#34996,0.124999999999993) ;
#12025 = CIRCLE('',#34998,0.0634999999999941) ;
#12026 = CIRCLE('',#34999,0.124999999999993) ;
#12027 = CIRCLE('',#35001,0.124999999999993) ;
#12028 = CIRCLE('',#35003,0.0634999999999764) ;
#12029 = CIRCLE('',#35004,0.124999999999993) ;
#12030 = CIRCLE('',#35006,0.0634999999999941) ;
#12031 = CIRCLE('',#35007,0.124999999999993) ;
#12032 = CIRCLE('',#35008,0.124999999999993) ;
#12033 = CIRCLE('',#35011,0.125000000000028) ;
#12034 = CIRCLE('',#35013,0.0634999999999941) ;
#12035 = CIRCLE('',#35014,0.124999999999993) ;
#12036 = CIRCLE('',#35016,0.124999999999993) ;
#12037 = CIRCLE('',#35019,0.124999999999993) ;
#12038 = CIRCLE('',#35022,0.124999999999993) ;
#12039 = CIRCLE('',#35025,0.124999999999993) ;
#12040 = CIRCLE('',#35026,0.124999999999993) ;
#12041 = CIRCLE('',#35028,0.124999999999993) ;
#12042 = CIRCLE('',#35035,0.124999999999993) ;
#12043 = CIRCLE('',#35036,0.125000000000011) ;
#12044 = CIRCLE('',#35037,0.125000000000006) ;
#12045 = CIRCLE('',#35039,0.124999999999993) ;
#12046 = CIRCLE('',#35040,0.125000000000002) ;
#12047 = CIRCLE('',#35041,0.124999999999993) ;
#12048 = CIRCLE('',#35044,0.124999999999993) ;
#12049 = CIRCLE('',#35046,0.125000000000011) ;
#12050 = CIRCLE('',#35048,0.124999999999993) ;
#12051 = CIRCLE('',#35049,0.125000000000011) ;
#12052 = CIRCLE('',#35053,0.124999999999993) ;
#12053 = CIRCLE('',#35055,0.124999999999993) ;
#12054 = CIRCLE('',#35056,0.124999999999993) ;
#12055 = CIRCLE('',#35058,0.0634999999999941) ;
#12056 = CIRCLE('',#35059,0.124999999999993) ;
#12057 = CIRCLE('',#35061,0.124999999999993) ;
#12058 = CIRCLE('',#35063,0.0634999999999764) ;
#12059 = CIRCLE('',#35064,0.124999999999993) ;
#12060 = CIRCLE('',#35066,0.0634999999999941) ;
#12061 = CIRCLE('',#35067,0.124999999999993) ;
#12062 = CIRCLE('',#35068,0.124999999999993) ;
#12063 = CIRCLE('',#35071,0.125000000000028) ;
#12064 = CIRCLE('',#35073,0.0634999999999941) ;
#12065 = CIRCLE('',#35074,0.124999999999993) ;
#12066 = CIRCLE('',#35076,0.124999999999993) ;
#12067 = CIRCLE('',#35079,0.124999999999993) ;
#12068 = CIRCLE('',#35082,0.124999999999993) ;
#12069 = CIRCLE('',#35085,0.124999999999993) ;
#12070 = CIRCLE('',#35086,0.124999999999993) ;
#12071 = CIRCLE('',#35088,0.124999999999993) ;
#12072 = CIRCLE('',#35095,0.124999999999993) ;
#12073 = CIRCLE('',#35096,0.125000000000011) ;
#12074 = CIRCLE('',#35097,0.125000000000006) ;
#12075 = CIRCLE('',#35099,0.124999999999993) ;
#12076 = CIRCLE('',#35100,0.125000000000002) ;
#12077 = CIRCLE('',#35101,0.124999999999993) ;
#12078 = CIRCLE('',#35104,0.124999999999993) ;
#12079 = CIRCLE('',#35106,0.125000000000011) ;
#12080 = CIRCLE('',#35108,0.124999999999993) ;
#12081 = CIRCLE('',#35109,0.125000000000011) ;
#12082 = CIRCLE('',#35113,0.124999999999993) ;
#12083 = CIRCLE('',#35115,0.124999999999993) ;
#12084 = CIRCLE('',#35116,0.124999999999993) ;
#12085 = CIRCLE('',#35118,0.0634999999999941) ;
#12086 = CIRCLE('',#35119,0.124999999999993) ;
#12087 = CIRCLE('',#35121,0.124999999999993) ;
#12088 = CIRCLE('',#35123,0.0634999999999764) ;
#12089 = CIRCLE('',#35124,0.124999999999993) ;
#12090 = CIRCLE('',#35126,0.0634999999999941) ;
#12091 = CIRCLE('',#35127,0.124999999999993) ;
#12092 = CIRCLE('',#35128,0.124999999999993) ;
#12093 = CIRCLE('',#35131,0.125000000000028) ;
#12094 = CIRCLE('',#35133,0.0634999999999941) ;
#12095 = CIRCLE('',#35134,0.124999999999993) ;
#12096 = CIRCLE('',#35136,0.124999999999993) ;
#12097 = CIRCLE('',#35139,0.124999999999993) ;
#12098 = CIRCLE('',#35142,0.124999999999993) ;
#12099 = CIRCLE('',#35145,0.124999999999993) ;
#12100 = CIRCLE('',#35146,0.124999999999993) ;
#12101 = CIRCLE('',#35148,0.124999999999993) ;
#12102 = CIRCLE('',#35155,0.124999999999993) ;
#12103 = CIRCLE('',#35156,0.125000000000011) ;
#12104 = CIRCLE('',#35157,0.125000000000006) ;
#12105 = CIRCLE('',#35159,0.124999999999993) ;
#12106 = CIRCLE('',#35160,0.125000000000002) ;
#12107 = CIRCLE('',#35161,0.124999999999993) ;
#12108 = CIRCLE('',#35164,0.124999999999993) ;
#12109 = CIRCLE('',#35166,0.125000000000011) ;
#12110 = CIRCLE('',#35168,0.124999999999993) ;
#12111 = CIRCLE('',#35169,0.125000000000011) ;
#12112 = CIRCLE('',#35173,0.124999999999993) ;
#12113 = CIRCLE('',#35175,0.124999999999993) ;
#12114 = CIRCLE('',#35176,0.124999999999993) ;
#12115 = CIRCLE('',#35178,0.0634999999999941) ;
#12116 = CIRCLE('',#35179,0.124999999999993) ;
#12117 = CIRCLE('',#35181,0.124999999999993) ;
#12118 = CIRCLE('',#35183,0.0634999999999764) ;
#12119 = CIRCLE('',#35184,0.124999999999993) ;
#12120 = CIRCLE('',#35186,0.0634999999999941) ;
#12121 = CIRCLE('',#35187,0.124999999999993) ;
#12122 = CIRCLE('',#35188,0.124999999999993) ;
#12123 = CIRCLE('',#35191,0.125000000000028) ;
#12124 = CIRCLE('',#35193,0.0634999999999941) ;
#12125 = CIRCLE('',#35194,0.124999999999993) ;
#12126 = CIRCLE('',#35196,0.124999999999993) ;
#12127 = CIRCLE('',#35199,0.124999999999993) ;
#12128 = CIRCLE('',#35202,0.124999999999993) ;
#12129 = CIRCLE('',#35205,0.124999999999993) ;
#12130 = CIRCLE('',#35206,0.124999999999993) ;
#12131 = CIRCLE('',#35208,0.124999999999993) ;
#12132 = CIRCLE('',#35215,0.124999999999993) ;
#12133 = CIRCLE('',#35216,0.125000000000011) ;
#12134 = CIRCLE('',#35217,0.125000000000006) ;
#12135 = CIRCLE('',#35219,0.124999999999993) ;
#12136 = CIRCLE('',#35220,0.125000000000002) ;
#12137 = CIRCLE('',#35221,0.124999999999993) ;
#12138 = CIRCLE('',#35224,0.124999999999993) ;
#12139 = CIRCLE('',#35226,0.125000000000011) ;
#12140 = CIRCLE('',#35228,0.124999999999993) ;
#12141 = CIRCLE('',#35229,0.125000000000011) ;
#12142 = CIRCLE('',#35329,2.88334137894263) ;
#12143 = CIRCLE('',#35331,2.8575) ;
#12144 = CIRCLE('',#35332,2.8575) ;
#12145 = CIRCLE('',#35333,0.125) ;
#12146 = CIRCLE('',#35335,2.8575) ;
#12147 = CIRCLE('',#35337,0.125) ;
#12148 = CIRCLE('',#35341,2.88334137894263) ;
#12149 = CIRCLE('',#35343,2.8575) ;
#12150 = CIRCLE('',#35344,2.8575) ;
#12151 = CIRCLE('',#35345,0.125) ;
#12152 = CIRCLE('',#35347,2.8575) ;
#12153 = CIRCLE('',#35349,0.125) ;
#12154 = CIRCLE('',#35353,2.88334137894263) ;
#12155 = CIRCLE('',#35355,2.8575) ;
#12156 = CIRCLE('',#35356,2.8575) ;
#12157 = CIRCLE('',#35357,0.125) ;
#12158 = CIRCLE('',#35359,2.8575) ;
#12159 = CIRCLE('',#35361,0.125) ;
#12160 = CIRCLE('',#35365,2.88334137894263) ;
#12161 = CIRCLE('',#35367,2.8575) ;
#12162 = CIRCLE('',#35368,2.8575) ;
#12163 = CIRCLE('',#35369,0.125) ;
#12164 = CIRCLE('',#35371,2.8575) ;
#12165 = CIRCLE('',#35373,0.125) ;
#12166 = CIRCLE('',#35377,2.88334137894263) ;
#12167 = CIRCLE('',#35379,2.8575) ;
#12168 = CIRCLE('',#35380,2.8575) ;
#12169 = CIRCLE('',#35381,0.125) ;
#12170 = CIRCLE('',#35383,2.8575) ;
#12171 = CIRCLE('',#35385,0.125) ;
#12172 = CIRCLE('',#35389,2.88334137894263) ;
#12173 = CIRCLE('',#35391,2.8575) ;
#12174 = CIRCLE('',#35392,2.8575) ;
#12175 = CIRCLE('',#35393,0.125) ;
#12176 = CIRCLE('',#35395,2.8575) ;
#12177 = CIRCLE('',#35397,0.125) ;
#12178 = CIRCLE('',#35401,2.88334137894263) ;
#12179 = CIRCLE('',#35403,2.8575) ;
#12180 = CIRCLE('',#35404,2.8575) ;
#12181 = CIRCLE('',#35405,0.125) ;
#12182 = CIRCLE('',#35407,2.8575) ;
#12183 = CIRCLE('',#35409,0.125) ;
#12184 = CIRCLE('',#35413,2.88334137894263) ;
#12185 = CIRCLE('',#35415,2.8575) ;
#12186 = CIRCLE('',#35416,2.8575) ;
#12187 = CIRCLE('',#35417,0.125) ;
#12188 = CIRCLE('',#35419,2.8575) ;
#12189 = CIRCLE('',#35421,0.125) ;
#12190 = CIRCLE('',#35425,2.8575) ;
#12191 = CIRCLE('',#35426,2.8575) ;
#12192 = CIRCLE('',#35427,0.125) ;
#12193 = CIRCLE('',#35429,2.8575) ;
#12194 = CIRCLE('',#35431,0.125) ;
#12195 = CIRCLE('',#35484,1.23704425180986) ;
#12196 = CIRCLE('',#35486,1.7526) ;
#12197 = CIRCLE('',#35494,1.7526) ;
#12198 = CIRCLE('',#35496,1.23704425180986) ;
#12199 = CIRCLE('',#35497,0.1) ;
#12200 = CIRCLE('',#35498,0.0999999999999999) ;
#12201 = CIRCLE('',#35499,0.1) ;
#12202 = CIRCLE('',#35500,0.1) ;
#12203 = CIRCLE('',#35503,0.0999999999999989) ;
#12204 = CIRCLE('',#35504,0.0999999999999997) ;
#12205 = CIRCLE('',#35505,0.0999999999999999) ;
#12206 = CIRCLE('',#35508,3.429) ;
#12207 = CIRCLE('',#35510,3.35640733905173) ;
#12208 = CIRCLE('',#35512,3.429) ;
#12209 = CIRCLE('',#35513,3.35640733905173) ;
#12210 = CIRCLE('',#35515,3.429) ;
#12211 = CIRCLE('',#35516,0.443484) ;
#12212 = CIRCLE('',#35517,2.985516) ;
#12213 = CIRCLE('',#35519,3.2727760605723) ;
#12214 = CIRCLE('',#35521,0.1) ;
#12215 = CIRCLE('',#35522,0.0999999999999997) ;
#12216 = CIRCLE('',#35523,0.0999999999999997) ;
#12217 = CIRCLE('',#35524,0.1) ;
#12218 = CIRCLE('',#35525,0.1) ;
#12219 = CIRCLE('',#35527,0.100000000000001) ;
#12220 = CIRCLE('',#35528,0.0999999999999995) ;
#12221 = CIRCLE('',#35530,0.1) ;
#12222 = CIRCLE('',#35532,5.21754264299203) ;
#12223 = CIRCLE('',#35533,0.0999999999999999) ;
#12224 = CIRCLE('',#35534,0.1) ;
#12225 = CIRCLE('',#35535,0.1) ;
#12226 = CIRCLE('',#35536,0.1) ;
#12227 = CIRCLE('',#35539,0.100000000000001) ;
#12228 = CIRCLE('',#35540,0.1) ;
#12229 = CIRCLE('',#35541,0.0999999999999999) ;
#12230 = CIRCLE('',#35543,3.2727760605723) ;
#12231 = CIRCLE('',#35545,0.100000000000001) ;
#12232 = CIRCLE('',#35546,0.1) ;
#12233 = CIRCLE('',#35547,0.1) ;
#12234 = CIRCLE('',#35548,0.1) ;
#12235 = CIRCLE('',#35549,0.1) ;
#12236 = CIRCLE('',#35551,0.100000000000001) ;
#12237 = CIRCLE('',#35552,0.0999999999999988) ;
#12238 = CIRCLE('',#35554,0.1) ;
#12239 = CIRCLE('',#35556,5.21754264299203) ;
#12240 = CIRCLE('',#35558,0.1) ;
#12241 = CIRCLE('',#35562,0.1) ;
#12242 = CIRCLE('',#35564,0.1) ;
#12243 = CIRCLE('',#35565,0.1) ;
#12244 = CIRCLE('',#35567,5.28650897109211) ;
#12245 = CIRCLE('',#35568,5.38647567822556) ;
#12246 = CIRCLE('',#35572,0.1) ;
#12247 = CIRCLE('',#35573,0.1) ;
#12248 = CIRCLE('',#35574,0.1) ;
#12249 = CIRCLE('',#35576,0.1) ;
#12250 = CIRCLE('',#35578,0.1) ;
#12251 = CIRCLE('',#35580,0.0999999999999999) ;
#12252 = CIRCLE('',#35581,0.1) ;
#12253 = CIRCLE('',#35582,0.1) ;
#12254 = CIRCLE('',#35583,0.1) ;
#12255 = CIRCLE('',#35584,0.0999999999999999) ;
#12256 = CIRCLE('',#35588,5.28650897109211) ;
#12257 = CIRCLE('',#35589,0.1) ;
#12258 = CIRCLE('',#35590,5.38647567822556) ;
#12259 = CIRCLE('',#35594,0.0999999999999998) ;
#12260 = CIRCLE('',#35597,0.0999999999999998) ;
#12261 = CIRCLE('',#35599,0.1) ;
#12262 = CIRCLE('',#35602,5.25939963812285) ;
#12263 = CIRCLE('',#35606,0.0999999999999999) ;
#12264 = CIRCLE('',#35607,0.1) ;
#12265 = CIRCLE('',#35608,0.1) ;
#12266 = CIRCLE('',#35609,0.1) ;
#12267 = CIRCLE('',#35611,0.0999999999999999) ;
#12268 = CIRCLE('',#35614,2.21840405576151) ;
#12269 = CIRCLE('',#35616,2.35877270918314) ;
#12270 = CIRCLE('',#35618,1.83996264656598) ;
#12271 = CIRCLE('',#35620,1.74337006393707) ;
#12272 = CIRCLE('',#35621,0.1) ;
#12273 = CIRCLE('',#35625,0.1) ;
#12274 = CIRCLE('',#35626,0.1) ;
#12275 = CIRCLE('',#35627,0.1) ;
#12276 = CIRCLE('',#35628,0.1) ;
#12277 = CIRCLE('',#35631,5.28650897109211) ;
#12278 = CIRCLE('',#35632,0.1) ;
#12279 = CIRCLE('',#35633,5.38647567822556) ;
#12280 = CIRCLE('',#35637,0.0999999999999997) ;
#12281 = CIRCLE('',#35640,0.1) ;
#12282 = CIRCLE('',#35642,0.1) ;
#12283 = CIRCLE('',#35645,5.25939963812284) ;
#12284 = CIRCLE('',#35648,0.0999999999999998) ;
#12285 = CIRCLE('',#35651,0.1) ;
#12286 = CIRCLE('',#35653,0.1) ;
#12287 = CIRCLE('',#35654,0.1) ;
#12288 = CIRCLE('',#35656,5.28650897109211) ;
#12289 = CIRCLE('',#35660,1.81678704225081) ;
#12290 = CIRCLE('',#35662,1.8526) ;
#12291 = CIRCLE('',#35664,1.82930603365754) ;
#12292 = CIRCLE('',#35666,0.1) ;
#12293 = CIRCLE('',#35673,0.1) ;
#12294 = CIRCLE('',#35676,0.1) ;
#12295 = CIRCLE('',#35678,0.1) ;
#12296 = CIRCLE('',#35679,0.1) ;
#12297 = CIRCLE('',#35682,0.1) ;
#12298 = CIRCLE('',#35684,1.89730211487829) ;
#12299 = CIRCLE('',#35685,1.99389469750719) ;
#12300 = CIRCLE('',#35687,0.1) ;
#12301 = CIRCLE('',#35688,0.1) ;
#12302 = CIRCLE('',#35689,0.1) ;
#12303 = CIRCLE('',#35690,0.0999999999999999) ;
#12304 = CIRCLE('',#35692,0.1) ;
#12305 = CIRCLE('',#35695,0.1) ;
#12306 = CIRCLE('',#35700,0.0999999999999998) ;
#12307 = CIRCLE('',#35703,0.1) ;
#12308 = CIRCLE('',#35704,0.0999999999382708) ;
#12309 = CIRCLE('',#35706,0.1) ;
#12310 = CIRCLE('',#35709,0.100000000000001) ;
#12311 = CIRCLE('',#35711,0.1) ;
#12312 = CIRCLE('',#35712,0.1) ;
#12313 = CIRCLE('',#35714,0.1) ;
#12314 = CIRCLE('',#35720,0.0999999999999999) ;
#12315 = CIRCLE('',#35721,0.1) ;
#12316 = CIRCLE('',#35724,0.1) ;
#12317 = CIRCLE('',#35725,0.1) ;
#12318 = CIRCLE('',#35726,0.1) ;
#12319 = CIRCLE('',#35729,0.100000000000001) ;
#12320 = CIRCLE('',#35731,0.1) ;
#12321 = CIRCLE('',#35732,0.1) ;
#12322 = CIRCLE('',#35734,0.1) ;
#12323 = CIRCLE('',#35735,0.1) ;
#12324 = CIRCLE('',#35738,0.1) ;
#12325 = CIRCLE('',#35740,5.35885371380814) ;
#12326 = CIRCLE('',#35742,5.21754264299203) ;
#12327 = CIRCLE('',#35743,0.0999999999999998) ;
#12328 = CIRCLE('',#35744,5.31620521222257) ;
#12329 = CIRCLE('',#35750,0.0999999999999999) ;
#12330 = CIRCLE('',#35751,0.1) ;
#12331 = CIRCLE('',#35754,0.1) ;
#12332 = CIRCLE('',#35761,0.1) ;
#12333 = CIRCLE('',#35768,0.1) ;
#12334 = CIRCLE('',#35771,0.1) ;
#12335 = CIRCLE('',#35773,0.1) ;
#12336 = CIRCLE('',#35774,0.1) ;
#12337 = CIRCLE('',#35777,0.1) ;
#12338 = CIRCLE('',#35779,1.89730211487828) ;
#12339 = CIRCLE('',#35780,1.99389469750719) ;
#12340 = CIRCLE('',#35782,0.1) ;
#12341 = CIRCLE('',#35783,0.1) ;
#12342 = CIRCLE('',#35784,0.1) ;
#12343 = CIRCLE('',#35785,0.0999999999999999) ;
#12344 = CIRCLE('',#35787,0.1) ;
#12345 = CIRCLE('',#35790,0.0999999999999999) ;
#12346 = CIRCLE('',#35796,0.1) ;
#12347 = CIRCLE('',#35797,0.0999999999999999) ;
#12348 = CIRCLE('',#35800,0.0999999999386781) ;
#12349 = CIRCLE('',#35802,0.1) ;
#12350 = CIRCLE('',#35805,0.1) ;
#12351 = CIRCLE('',#35807,0.1) ;
#12352 = CIRCLE('',#35808,0.1) ;
#12353 = CIRCLE('',#35810,0.1) ;
#12354 = CIRCLE('',#35817,0.0999999999999999) ;
#12355 = CIRCLE('',#35818,0.1) ;
#12356 = CIRCLE('',#35820,0.0999999999999999) ;
#12357 = CIRCLE('',#35823,5.25939963812284) ;
#12358 = CIRCLE('',#35824,0.1) ;
#12359 = CIRCLE('',#35825,0.1) ;
#12360 = CIRCLE('',#35827,0.1) ;
#12361 = CIRCLE('',#35829,0.1) ;
#12362 = CIRCLE('',#35830,0.1) ;
#12363 = CIRCLE('',#35832,0.1) ;
#12364 = CIRCLE('',#35833,0.1) ;
#12365 = CIRCLE('',#35836,0.1) ;
#12366 = CIRCLE('',#35838,5.35885371380814) ;
#12367 = CIRCLE('',#35840,5.21754264299203) ;
#12368 = CIRCLE('',#35841,0.1) ;
#12369 = CIRCLE('',#35842,5.31620521222257) ;
#12370 = CIRCLE('',#35846,0.1) ;
#12371 = CIRCLE('',#35847,0.1) ;
#12372 = CIRCLE('',#35850,0.1) ;
#12373 = CIRCLE('',#35856,1.74337006393707) ;
#12374 = CIRCLE('',#35857,1.83996264656598) ;
#12375 = CIRCLE('',#35859,1.74337006393707) ;
#12376 = CIRCLE('',#35860,1.83996264656598) ;
#12377 = CIRCLE('',#35862,1.74337006393707) ;
#12378 = CIRCLE('',#35863,1.83996264656598) ;
#12379 = CIRCLE('',#35865,5.25939963812284) ;
#12380 = CIRCLE('',#35869,5.31620521222257) ;
#12381 = CIRCLE('',#35870,0.100000000000004) ;
#12382 = CIRCLE('',#35872,5.35885371380814) ;
#12383 = CIRCLE('',#35874,2.21840405576151) ;
#12384 = CIRCLE('',#35875,2.35877270918314) ;
#12385 = CIRCLE('',#35877,0.1) ;
#12386 = CIRCLE('',#35879,3.25327858632053) ;
#12387 = CIRCLE('',#35881,3.429) ;
#12388 = CIRCLE('',#35883,0.1) ;
#12389 = CIRCLE('',#35885,5.31620521222257) ;
#12390 = CIRCLE('',#35887,5.35885371380814) ;
#12391 = CIRCLE('',#35889,5.38647567822556) ;
#12392 = CIRCLE('',#35890,0.1) ;
#12393 = CIRCLE('',#35893,3.25327858632053) ;
#12394 = CIRCLE('',#35895,3.429) ;
#12395 = CIRCLE('',#35898,1.1572875) ;
#12396 = CIRCLE('',#35914,1.7526) ;
#12397 = CIRCLE('',#35918,1.7526) ;
#12398 = CIRCLE('',#35920,1.5) ;
#12399 = CIRCLE('',#35924,1.5) ;
#12400 = CIRCLE('',#35928,0.124999999999993) ;
#12401 = CIRCLE('',#35929,0.124999999999993) ;
#12402 = CIRCLE('',#35931,0.0634999999999941) ;
#12403 = CIRCLE('',#35932,0.124999999999993) ;
#12404 = CIRCLE('',#35933,0.188499999999987) ;
#12405 = CIRCLE('',#35934,0.124999999999993) ;
#12406 = CIRCLE('',#35936,0.124999999999993) ;
#12407 = CIRCLE('',#35938,0.0634999999999764) ;
#12408 = CIRCLE('',#35939,0.124999999999957) ;
#12409 = CIRCLE('',#35940,0.188499999999969) ;
#12410 = CIRCLE('',#35941,0.124999999999993) ;
#12411 = CIRCLE('',#35943,0.0634999999999941) ;
#12412 = CIRCLE('',#35944,0.124999999999993) ;
#12413 = CIRCLE('',#35945,0.188499999999987) ;
#12414 = CIRCLE('',#35946,0.124999999999993) ;
#12415 = CIRCLE('',#35948,0.124999999999975) ;
#12416 = CIRCLE('',#35950,0.124999999999851) ;
#12417 = CIRCLE('',#35951,0.509999999999996) ;
#12418 = CIRCLE('',#35952,0.634999999999996) ;
#12419 = CIRCLE('',#35955,0.125000000000028) ;
#12420 = CIRCLE('',#35957,0.0634999999999941) ;
#12421 = CIRCLE('',#35958,0.124999999999993) ;
#12422 = CIRCLE('',#35959,0.188499999999987) ;
#12423 = CIRCLE('',#35960,0.124999999999993) ;
#12424 = CIRCLE('',#35962,0.124999999999993) ;
#12425 = CIRCLE('',#35964,0.125000000000064) ;
#12426 = CIRCLE('',#35966,0.125000000000099) ;
#12427 = CIRCLE('',#35967,0.509999999999996) ;
#12428 = CIRCLE('',#35968,0.634999999999996) ;
#12429 = CIRCLE('',#35972,0.124999999999993) ;
#12430 = CIRCLE('',#35975,0.124999999999993) ;
#12431 = CIRCLE('',#35977,0.124999999999993) ;
#12432 = CIRCLE('',#35979,0.124999999999993) ;
#12433 = CIRCLE('',#35980,0.124999999999993) ;
#12434 = CIRCLE('',#35982,0.124999999999993) ;
#12435 = CIRCLE('',#35984,0.124999999999993) ;
#12436 = CIRCLE('',#35987,0.125) ;
#12437 = CIRCLE('',#35990,0.125) ;
#12438 = CIRCLE('',#35997,0.124999999999993) ;
#12439 = CIRCLE('',#35999,0.124999999999993) ;
#12440 = CIRCLE('',#36001,0.250000000000012) ;
#12441 = CIRCLE('',#36002,0.249999999999986) ;
#12442 = CIRCLE('',#36007,0.249999999999995) ;
#12443 = CIRCLE('',#36008,0.249999999999986) ;
#12444 = CIRCLE('',#36011,0.698499999999999) ;
#12445 = CIRCLE('',#36012,0.698499999999999) ;
#12446 = CIRCLE('',#36014,0.698500000000001) ;
#12447 = CIRCLE('',#36015,0.6985) ;
#12448 = CIRCLE('',#36020,0.124999999999993) ;
#12449 = CIRCLE('',#36021,0.125) ;
#12450 = CIRCLE('',#36023,0.573500000000001) ;
#12451 = CIRCLE('',#36024,0.573499999999999) ;
#12452 = CIRCLE('',#36026,0.573499999999999) ;
#12453 = CIRCLE('',#36027,0.573500000000001) ;
#12454 = CIRCLE('',#36029,0.125000000000006) ;
#12455 = CIRCLE('',#36030,0.125) ;
#12456 = CIRCLE('',#36033,0.125000000000002) ;
#12457 = CIRCLE('',#36034,0.25) ;
#12458 = CIRCLE('',#36036,0.25) ;
#12459 = CIRCLE('',#36037,0.124999999999993) ;
#12460 = CIRCLE('',#36039,0.25) ;
#12461 = CIRCLE('',#36040,0.125000000000011) ;
#12462 = CIRCLE('',#36042,0.124999999999993) ;
#12463 = CIRCLE('',#36043,0.125000000000011) ;
#12464 = CIRCLE('',#36045,0.125000000000002) ;
#12465 = CIRCLE('',#36046,0.25) ;
#12466 = CIRCLE('',#36048,0.124999999999993) ;
#12467 = CIRCLE('',#36049,0.125000000000002) ;
#12468 = CIRCLE('',#36052,0.124999999999993) ;
#12469 = CIRCLE('',#36054,0.125000000000002) ;
#12470 = CIRCLE('',#36056,0.124999999999993) ;
#12471 = CIRCLE('',#36057,0.125000000000011) ;
#12472 = CIRCLE('',#36059,0.124999999999993) ;
#12473 = CIRCLE('',#36060,0.125000000000011) ;
#12474 = CIRCLE('',#36062,0.124999999999993) ;
#12475 = CIRCLE('',#36063,0.124999999999993) ;
#12476 = CIRCLE('',#36065,0.125000000000002) ;
#12477 = CIRCLE('',#36067,0.125000000000002) ;
#12478 = CIRCLE('',#36069,0.124999999999957) ;
#12479 = CIRCLE('',#36071,0.124999999999975) ;
#12480 = CIRCLE('',#36073,0.124999999999993) ;
#12481 = CIRCLE('',#36074,0.124999999999993) ;
#12482 = CIRCLE('',#36076,0.124999999999993) ;
#12483 = CIRCLE('',#36077,0.125000000000002) ;
#12484 = CIRCLE('',#36079,0.124999999999993) ;
#12485 = CIRCLE('',#36080,0.124999999999993) ;
#12486 = CIRCLE('',#36082,0.124999999999993) ;
#12487 = CIRCLE('',#36084,0.125000000000011) ;
#12488 = CIRCLE('',#36086,0.124999999999957) ;
#12489 = CIRCLE('',#36088,0.125000000000011) ;
#12490 = CIRCLE('',#36090,0.125000000000002) ;
#12491 = CIRCLE('',#36092,0.124999999999993) ;
#12492 = CIRCLE('',#36093,0.124999999999993) ;
#12493 = CIRCLE('',#36095,0.124999999999993) ;
#12494 = CIRCLE('',#36097,0.125000000000011) ;
#12495 = CIRCLE('',#36099,0.124999999999993) ;
#12496 = CIRCLE('',#36100,0.124999999999993) ;
#12497 = CIRCLE('',#36102,0.125000000000011) ;
#12498 = CIRCLE('',#36103,0.124999999999993) ;
#12499 = CIRCLE('',#36107,0.124999999999993) ;
#12500 = CIRCLE('',#36109,0.124999999999993) ;
#12501 = CIRCLE('',#36110,0.124999999999993) ;
#12502 = CIRCLE('',#36113,0.124999999999993) ;
#12503 = CIRCLE('',#36114,0.124999999999993) ;
#12504 = CIRCLE('',#36123,2.7325) ;
#12505 = CIRCLE('',#36124,0.125) ;
#12506 = CIRCLE('',#36125,2.8575) ;
#12507 = CIRCLE('',#36127,2.9825) ;
#12508 = CIRCLE('',#36129,2.8575) ;
#12509 = CIRCLE('',#36130,2.8575) ;
#12510 = CIRCLE('',#36132,0.125) ;
#12511 = CIRCLE('',#36145,4.75315367264104) ;
#12512 = CIRCLE('',#36146,5.22940380210988) ;
#12513 = CIRCLE('',#36147,4.75315367264148) ;
#12514 = CIRCLE('',#36148,5.22940367264214) ;
#12515 = CIRCLE('',#36149,4.75315367264191) ;
#12516 = CIRCLE('',#36150,5.22940354317232) ;
#12517 = CIRCLE('',#36151,4.75315367264155) ;
#12518 = CIRCLE('',#36152,5.22940367264084) ;
#12519 = CIRCLE('',#36153,4.75315367264153) ;
#12520 = CIRCLE('',#36154,5.22940367264213) ;
#12521 = CIRCLE('',#36156,1.651) ;
#12522 = CIRCLE('',#36157,1.651) ;
#12523 = CIRCLE('',#36159,0.730250002314184) ;
#12524 = CIRCLE('',#36160,0.730250002314185) ;
#12525 = CIRCLE('',#36161,0.730250002314184) ;
#12526 = CIRCLE('',#36162,0.730250002314185) ;
#12527 = CIRCLE('',#36164,0.571500002304898) ;
#12528 = CIRCLE('',#36166,0.571500002304899) ;
#12529 = CIRCLE('',#36168,0.571500002304899) ;
#12530 = CIRCLE('',#36170,0.571500002304898) ;
#12531 = CIRCLE('',#36172,0.0952500014492024) ;
#12532 = CIRCLE('',#36173,0.0952500013168486) ;
#12533 = CIRCLE('',#36174,0.635) ;
#12534 = CIRCLE('',#36176,0.095249999999996) ;
#12535 = CIRCLE('',#36178,0.095249999999998) ;
#12536 = CIRCLE('',#36180,0.095250001316849) ;
#12537 = CIRCLE('',#36181,0.0952500013168486) ;
#12538 = CIRCLE('',#36182,0.635) ;
#12539 = CIRCLE('',#36184,0.0952499999999976) ;
#12540 = CIRCLE('',#36186,0.0952499999999994) ;
#12541 = CIRCLE('',#36188,0.0952500014492024) ;
#12542 = CIRCLE('',#36189,0.0952500013168531) ;
#12543 = CIRCLE('',#36190,0.635) ;
#12544 = CIRCLE('',#36192,0.0952499999999996) ;
#12545 = CIRCLE('',#36194,0.0952500000000022) ;
#12546 = CIRCLE('',#36198,0.635) ;
#12547 = CIRCLE('',#36200,0.0634999990163235) ;
#12548 = CIRCLE('',#36201,0.0635000000000008) ;
#12549 = CIRCLE('',#36203,0.0634999999999982) ;
#12550 = CIRCLE('',#36204,0.0634999989174561) ;
#12551 = CIRCLE('',#36209,0.0634999990163231) ;
#12552 = CIRCLE('',#36210,0.0634999990163244) ;
#12553 = CIRCLE('',#36211,0.635) ;
#12554 = CIRCLE('',#36213,0.0635000000000008) ;
#12555 = CIRCLE('',#36215,0.0634999999999995) ;
#12556 = CIRCLE('',#36219,0.635) ;
#12557 = CIRCLE('',#36221,0.0634999990163231) ;
#12558 = CIRCLE('',#36222,0.0634999990163244) ;
#12559 = CIRCLE('',#36224,0.0635000000000008) ;
#12560 = CIRCLE('',#36226,0.0635000000000001) ;
#12561 = CIRCLE('',#36230,0.635) ;
#12562 = CIRCLE('',#36232,0.0634999990163235) ;
#12563 = CIRCLE('',#36233,0.0635000000000008) ;
#12564 = CIRCLE('',#36235,0.0634999999999985) ;
#12565 = CIRCLE('',#36236,0.0634999989174561) ;
#12566 = CIRCLE('',#36239,0.635) ;
#12567 = CIRCLE('',#36241,0.0952500013168532) ;
#12568 = CIRCLE('',#36242,0.0952500013168486) ;
#12569 = CIRCLE('',#36244,0.0952500000000016) ;
#12570 = CIRCLE('',#36246,0.095249999999998) ;
#12571 = CIRCLE('',#36248,0.445135) ;
#12572 = CIRCLE('',#36252,0.635000000000001) ;
#12573 = CIRCLE('',#36253,0.635) ;
#12574 = CIRCLE('',#36255,0.189864999999999) ;
#12575 = CIRCLE('',#36256,0.189865) ;
#12576 = CIRCLE('',#36258,0.189864999999999) ;
#12577 = CIRCLE('',#36259,0.189864999999999) ;
#12578 = CIRCLE('',#36262,0.445135) ;
#12579 = CIRCLE('',#36266,0.635000000000001) ;
#12580 = CIRCLE('',#36267,0.635) ;
#12581 = CIRCLE('',#36269,0.189864999999999) ;
#12582 = CIRCLE('',#36270,0.189865) ;
#12583 = CIRCLE('',#36272,0.189864999999999) ;
#12584 = CIRCLE('',#36273,0.189864999999999) ;
#12585 = CIRCLE('',#36276,0.445135) ;
#12586 = CIRCLE('',#36280,0.635) ;
#12587 = CIRCLE('',#36281,0.635) ;
#12588 = CIRCLE('',#36283,0.189865) ;
#12589 = CIRCLE('',#36284,0.189864999999999) ;
#12590 = CIRCLE('',#36286,0.189864999999998) ;
#12591 = CIRCLE('',#36287,0.189864999999999) ;
#12592 = CIRCLE('',#36290,0.445135) ;
#12593 = CIRCLE('',#36294,0.635) ;
#12594 = CIRCLE('',#36295,0.635) ;
#12595 = CIRCLE('',#36297,0.189864999999999) ;
#12596 = CIRCLE('',#36298,0.189864999999999) ;
#12597 = CIRCLE('',#36300,0.189864999999998) ;
#12598 = CIRCLE('',#36301,0.189864999999999) ;
#12599 = CIRCLE('',#36308,4.75315367264138) ;
#12600 = CIRCLE('',#36309,4.75315367264185) ;
#12601 = CIRCLE('',#36310,4.75315367264196) ;
#12602 = CIRCLE('',#36311,4.75315367264146) ;
#12603 = CIRCLE('',#36312,4.75315367264139) ;
#12604 = CIRCLE('',#36313,5.22940367264163) ;
#12605 = CIRCLE('',#36316,5.22940367264085) ;
#12606 = CIRCLE('',#36319,5.22940354316612) ;
#12607 = CIRCLE('',#36320,5.22940380211795) ;
#12608 = CIRCLE('',#36323,5.229403672641) ;
#12609 = CIRCLE('',#36357,1.25) ;
#12610 = CIRCLE('',#36358,1.25) ;
#12611 = CIRCLE('',#36359,1.25) ;
#12612 = CIRCLE('',#36360,1.25) ;
#12613 = CIRCLE('',#36361,1.25) ;
#12614 = CIRCLE('',#36363,1.25) ;
#12615 = CIRCLE('',#36364,1.25) ;
#12616 = CIRCLE('',#36365,1.25) ;
#12617 = CIRCLE('',#36366,1.25) ;
#12618 = CIRCLE('',#36367,1.25) ;
#12619 = CIRCLE('',#36383,1.5) ;
#12620 = CIRCLE('',#36399,1.17524047358084) ;
#12621 = CIRCLE('',#36416,1.17524047358084) ;
#12622 = CIRCLE('',#36418,1.17524047358084) ;
#12623 = CIRCLE('',#36420,1.17524047358084) ;
#12624 = CIRCLE('',#36422,1.5) ;
#12625 = CIRCLE('',#36424,0.930607966083863) ;
#12626 = CIRCLE('',#36425,1.4329043419966) ;
#12627 = CIRCLE('',#36427,0.930607966083863) ;
#12628 = CIRCLE('',#36428,1.4329043419966) ;
#12629 = CIRCLE('',#36430,2.85397350993377) ;
#12630 = CIRCLE('',#36431,0.449999999999999) ;
#12631 = CIRCLE('',#36432,3.) ;
#12632 = CIRCLE('',#36433,3.) ;
#12633 = CIRCLE('',#36435,1.4329043419966) ;
#12634 = CIRCLE('',#36436,4.22489174394716) ;
#12635 = CIRCLE('',#36437,4.21532021625621) ;
#12636 = CIRCLE('',#36438,4.21532021625621) ;
#12637 = CIRCLE('',#36439,4.22489174394716) ;
#12638 = CIRCLE('',#36440,4.22489174394716) ;
#12639 = CIRCLE('',#36441,4.21532021625621) ;
#12640 = CIRCLE('',#36442,4.21532021625621) ;
#12641 = CIRCLE('',#36443,4.22489174394716) ;
#12642 = CIRCLE('',#36444,4.22489174394716) ;
#12643 = CIRCLE('',#36445,4.21532021625621) ;
#12644 = CIRCLE('',#36446,4.21532021625621) ;
#12645 = CIRCLE('',#36447,4.22489174394717) ;
#12646 = CIRCLE('',#36448,1.4329043419966) ;
#12647 = CIRCLE('',#36449,4.22489174394716) ;
#12648 = CIRCLE('',#36450,4.21532021625621) ;
#12649 = CIRCLE('',#36451,4.21532021625621) ;
#12650 = CIRCLE('',#36452,4.22489174394716) ;
#12651 = CIRCLE('',#36454,3.) ;
#12652 = CIRCLE('',#36455,3.) ;
#12653 = CIRCLE('',#36457,0.45) ;
#12654 = CIRCLE('',#36458,2.55) ;
#12655 = CIRCLE('',#36462,0.930607966083863) ;
#12656 = CIRCLE('',#36468,0.930607966083863) ;
#12657 = CIRCLE('',#36488,2.9375) ;
#12658 = CIRCLE('',#36489,0.0625) ;
#12659 = CIRCLE('',#36490,3.) ;
#12660 = CIRCLE('',#36491,3.) ;
#12661 = CIRCLE('',#36493,3.) ;
#12662 = CIRCLE('',#36494,3.) ;
#12663 = CIRCLE('',#36496,1.6) ;
#12664 = CIRCLE('',#36498,0.0625) ;
#12665 = CIRCLE('',#36499,2.9375) ;
#12666 = CIRCLE('',#36501,1.6) ;
#12667 = VERTEX_POINT('',#46350) ;
#12668 = VERTEX_POINT('',#46351) ;
#12669 = VERTEX_POINT('',#46353) ;
#12670 = VERTEX_POINT('',#46355) ;
#12671 = VERTEX_POINT('',#46359) ;
#12672 = VERTEX_POINT('',#46361) ;
#12673 = VERTEX_POINT('',#46363) ;
#12674 = VERTEX_POINT('',#46365) ;
#12675 = VERTEX_POINT('',#46368) ;
#12676 = VERTEX_POINT('',#46369) ;
#12677 = VERTEX_POINT('',#46371) ;
#12678 = VERTEX_POINT('',#46379) ;
#12679 = VERTEX_POINT('',#46382) ;
#12680 = VERTEX_POINT('',#46383) ;
#12681 = VERTEX_POINT('',#46391) ;
#12682 = VERTEX_POINT('',#46393) ;
#12683 = VERTEX_POINT('',#46396) ;
#12684 = VERTEX_POINT('',#46397) ;
#12685 = VERTEX_POINT('',#46399) ;
#12686 = VERTEX_POINT('',#46401) ;
#12687 = VERTEX_POINT('',#46404) ;
#12688 = VERTEX_POINT('',#46405) ;
#12689 = VERTEX_POINT('',#46407) ;
#12690 = VERTEX_POINT('',#46409) ;
#12691 = VERTEX_POINT('',#46412) ;
#12692 = VERTEX_POINT('',#46413) ;
#12693 = VERTEX_POINT('',#46415) ;
#12694 = VERTEX_POINT('',#46417) ;
#12695 = VERTEX_POINT('',#46420) ;
#12696 = VERTEX_POINT('',#46421) ;
#12697 = VERTEX_POINT('',#46423) ;
#12698 = VERTEX_POINT('',#46425) ;
#12699 = VERTEX_POINT('',#46428) ;
#12700 = VERTEX_POINT('',#46429) ;
#12701 = VERTEX_POINT('',#46431) ;
#12702 = VERTEX_POINT('',#46433) ;
#12703 = VERTEX_POINT('',#46436) ;
#12704 = VERTEX_POINT('',#46437) ;
#12705 = VERTEX_POINT('',#46439) ;
#12706 = VERTEX_POINT('',#46441) ;
#12707 = VERTEX_POINT('',#46444) ;
#12708 = VERTEX_POINT('',#46445) ;
#12709 = VERTEX_POINT('',#46447) ;
#12710 = VERTEX_POINT('',#46449) ;
#12711 = VERTEX_POINT('',#46452) ;
#12712 = VERTEX_POINT('',#46453) ;
#12713 = VERTEX_POINT('',#46455) ;
#12714 = VERTEX_POINT('',#46457) ;
#12715 = VERTEX_POINT('',#46460) ;
#12716 = VERTEX_POINT('',#46462) ;
#12717 = VERTEX_POINT('',#46464) ;
#12718 = VERTEX_POINT('',#46466) ;
#12719 = VERTEX_POINT('',#46468) ;
#12720 = VERTEX_POINT('',#46470) ;
#12721 = VERTEX_POINT('',#46472) ;
#12722 = VERTEX_POINT('',#46473) ;
#12723 = VERTEX_POINT('',#46475) ;
#12724 = VERTEX_POINT('',#46477) ;
#12725 = VERTEX_POINT('',#46480) ;
#12726 = VERTEX_POINT('',#46481) ;
#12727 = VERTEX_POINT('',#46483) ;
#12728 = VERTEX_POINT('',#46485) ;
#12729 = VERTEX_POINT('',#46488) ;
#12730 = VERTEX_POINT('',#46489) ;
#12731 = VERTEX_POINT('',#46491) ;
#12732 = VERTEX_POINT('',#46493) ;
#12733 = VERTEX_POINT('',#46496) ;
#12734 = VERTEX_POINT('',#46497) ;
#12735 = VERTEX_POINT('',#46499) ;
#12736 = VERTEX_POINT('',#46501) ;
#12737 = VERTEX_POINT('',#46505) ;
#12738 = VERTEX_POINT('',#46507) ;
#12739 = VERTEX_POINT('',#46511) ;
#12740 = VERTEX_POINT('',#46513) ;
#12741 = VERTEX_POINT('',#46517) ;
#12742 = VERTEX_POINT('',#46519) ;
#12743 = VERTEX_POINT('',#46521) ;
#12744 = VERTEX_POINT('',#46523) ;
#12745 = VERTEX_POINT('',#46525) ;
#12746 = VERTEX_POINT('',#46527) ;
#12747 = VERTEX_POINT('',#46529) ;
#12748 = VERTEX_POINT('',#46531) ;
#12749 = VERTEX_POINT('',#46533) ;
#12750 = VERTEX_POINT('',#46535) ;
#12751 = VERTEX_POINT('',#46537) ;
#12752 = VERTEX_POINT('',#46539) ;
#12753 = VERTEX_POINT('',#46541) ;
#12754 = VERTEX_POINT('',#46543) ;
#12755 = VERTEX_POINT('',#46545) ;
#12756 = VERTEX_POINT('',#46547) ;
#12757 = VERTEX_POINT('',#46550) ;
#12758 = VERTEX_POINT('',#46552) ;
#12759 = VERTEX_POINT('',#46555) ;
#12760 = VERTEX_POINT('',#46556) ;
#12761 = VERTEX_POINT('',#46558) ;
#12762 = VERTEX_POINT('',#46560) ;
#12763 = VERTEX_POINT('',#46564) ;
#12764 = VERTEX_POINT('',#46566) ;
#12765 = VERTEX_POINT('',#46569) ;
#12766 = VERTEX_POINT('',#46573) ;
#12767 = VERTEX_POINT('',#46575) ;
#12768 = VERTEX_POINT('',#46577) ;
#12769 = VERTEX_POINT('',#46579) ;
#12770 = VERTEX_POINT('',#46581) ;
#12771 = VERTEX_POINT('',#46583) ;
#12772 = VERTEX_POINT('',#46585) ;
#12773 = VERTEX_POINT('',#46587) ;
#12774 = VERTEX_POINT('',#46589) ;
#12775 = VERTEX_POINT('',#46591) ;
#12776 = VERTEX_POINT('',#46593) ;
#12777 = VERTEX_POINT('',#46595) ;
#12778 = VERTEX_POINT('',#46597) ;
#12779 = VERTEX_POINT('',#46599) ;
#12780 = VERTEX_POINT('',#46601) ;
#12781 = VERTEX_POINT('',#46604) ;
#12782 = VERTEX_POINT('',#46606) ;
#12783 = VERTEX_POINT('',#46609) ;
#12784 = VERTEX_POINT('',#46610) ;
#12785 = VERTEX_POINT('',#46612) ;
#12786 = VERTEX_POINT('',#46614) ;
#12787 = VERTEX_POINT('',#46618) ;
#12788 = VERTEX_POINT('',#46621) ;
#12789 = VERTEX_POINT('',#46625) ;
#12790 = VERTEX_POINT('',#46627) ;
#12791 = VERTEX_POINT('',#46629) ;
#12792 = VERTEX_POINT('',#46631) ;
#12793 = VERTEX_POINT('',#46633) ;
#12794 = VERTEX_POINT('',#46635) ;
#12795 = VERTEX_POINT('',#46637) ;
#12796 = VERTEX_POINT('',#46639) ;
#12797 = VERTEX_POINT('',#46641) ;
#12798 = VERTEX_POINT('',#46643) ;
#12799 = VERTEX_POINT('',#46645) ;
#12800 = VERTEX_POINT('',#46647) ;
#12801 = VERTEX_POINT('',#46649) ;
#12802 = VERTEX_POINT('',#46651) ;
#12803 = VERTEX_POINT('',#46653) ;
#12804 = VERTEX_POINT('',#46656) ;
#12805 = VERTEX_POINT('',#46658) ;
#12806 = VERTEX_POINT('',#46661) ;
#12807 = VERTEX_POINT('',#46663) ;
#12808 = VERTEX_POINT('',#46667) ;
#12809 = VERTEX_POINT('',#46676) ;
#12810 = VERTEX_POINT('',#46677) ;
#12811 = VERTEX_POINT('',#46679) ;
#12812 = VERTEX_POINT('',#46681) ;
#12813 = VERTEX_POINT('',#46686) ;
#12814 = VERTEX_POINT('',#46688) ;
#12815 = VERTEX_POINT('',#46692) ;
#12816 = VERTEX_POINT('',#46695) ;
#12817 = VERTEX_POINT('',#46697) ;
#12818 = VERTEX_POINT('',#46699) ;
#12819 = VERTEX_POINT('',#46702) ;
#12820 = VERTEX_POINT('',#46703) ;
#12821 = VERTEX_POINT('',#46705) ;
#12822 = VERTEX_POINT('',#46707) ;
#12823 = VERTEX_POINT('',#46710) ;
#12824 = VERTEX_POINT('',#46712) ;
#12825 = VERTEX_POINT('',#46714) ;
#12826 = VERTEX_POINT('',#46715) ;
#12827 = VERTEX_POINT('',#46717) ;
#12828 = VERTEX_POINT('',#46719) ;
#12829 = VERTEX_POINT('',#46722) ;
#12830 = VERTEX_POINT('',#46723) ;
#12831 = VERTEX_POINT('',#46725) ;
#12832 = VERTEX_POINT('',#46727) ;
#12833 = VERTEX_POINT('',#46730) ;
#12834 = VERTEX_POINT('',#46731) ;
#12835 = VERTEX_POINT('',#46733) ;
#12836 = VERTEX_POINT('',#46735) ;
#12837 = VERTEX_POINT('',#46738) ;
#12838 = VERTEX_POINT('',#46739) ;
#12839 = VERTEX_POINT('',#46741) ;
#12840 = VERTEX_POINT('',#46743) ;
#12841 = VERTEX_POINT('',#46746) ;
#12842 = VERTEX_POINT('',#46747) ;
#12843 = VERTEX_POINT('',#46749) ;
#12844 = VERTEX_POINT('',#46751) ;
#12845 = VERTEX_POINT('',#46754) ;
#12846 = VERTEX_POINT('',#46755) ;
#12847 = VERTEX_POINT('',#46757) ;
#12848 = VERTEX_POINT('',#46759) ;
#12849 = VERTEX_POINT('',#46762) ;
#12850 = VERTEX_POINT('',#46764) ;
#12851 = VERTEX_POINT('',#46766) ;
#12852 = VERTEX_POINT('',#46768) ;
#12853 = VERTEX_POINT('',#46770) ;
#12854 = VERTEX_POINT('',#46771) ;
#12855 = VERTEX_POINT('',#46773) ;
#12856 = VERTEX_POINT('',#46775) ;
#12857 = VERTEX_POINT('',#46778) ;
#12858 = VERTEX_POINT('',#46779) ;
#12859 = VERTEX_POINT('',#46781) ;
#12860 = VERTEX_POINT('',#46783) ;
#12861 = VERTEX_POINT('',#46786) ;
#12862 = VERTEX_POINT('',#46787) ;
#12863 = VERTEX_POINT('',#46789) ;
#12864 = VERTEX_POINT('',#46791) ;
#12865 = VERTEX_POINT('',#46794) ;
#12866 = VERTEX_POINT('',#46795) ;
#12867 = VERTEX_POINT('',#46797) ;
#12868 = VERTEX_POINT('',#46799) ;
#12869 = VERTEX_POINT('',#46802) ;
#12870 = VERTEX_POINT('',#46803) ;
#12871 = VERTEX_POINT('',#46805) ;
#12872 = VERTEX_POINT('',#46807) ;
#12873 = VERTEX_POINT('',#46810) ;
#12874 = VERTEX_POINT('',#46811) ;
#12875 = VERTEX_POINT('',#46813) ;
#12876 = VERTEX_POINT('',#46815) ;
#12877 = VERTEX_POINT('',#46824) ;
#12878 = VERTEX_POINT('',#46825) ;
#12879 = VERTEX_POINT('',#46827) ;
#12880 = VERTEX_POINT('',#46829) ;
#12881 = VERTEX_POINT('',#46839) ;
#12882 = VERTEX_POINT('',#46841) ;
#12883 = VERTEX_POINT('',#46843) ;
#12884 = VERTEX_POINT('',#46845) ;
#12885 = VERTEX_POINT('',#46847) ;
#12886 = VERTEX_POINT('',#46849) ;
#12887 = VERTEX_POINT('',#46851) ;
#12888 = VERTEX_POINT('',#46853) ;
#12889 = VERTEX_POINT('',#46855) ;
#12890 = VERTEX_POINT('',#46857) ;
#12891 = VERTEX_POINT('',#46859) ;
#12892 = VERTEX_POINT('',#46862) ;
#12893 = VERTEX_POINT('',#46865) ;
#12894 = VERTEX_POINT('',#46867) ;
#12895 = VERTEX_POINT('',#46870) ;
#12896 = VERTEX_POINT('',#46872) ;
#12897 = VERTEX_POINT('',#46874) ;
#12898 = VERTEX_POINT('',#46960) ;
#12899 = VERTEX_POINT('',#46964) ;
#12900 = VERTEX_POINT('',#46968) ;
#12901 = VERTEX_POINT('',#46976) ;
#12902 = VERTEX_POINT('',#46977) ;
#12903 = VERTEX_POINT('',#46979) ;
#12904 = VERTEX_POINT('',#46981) ;
#12905 = VERTEX_POINT('',#46985) ;
#12906 = VERTEX_POINT('',#46987) ;
#12907 = VERTEX_POINT('',#46991) ;
#12908 = VERTEX_POINT('',#46993) ;
#12909 = VERTEX_POINT('',#46995) ;
#12910 = VERTEX_POINT('',#46999) ;
#12911 = VERTEX_POINT('',#47003) ;
#12912 = VERTEX_POINT('',#47058) ;
#12913 = VERTEX_POINT('',#47177) ;
#12914 = VERTEX_POINT('',#47178) ;
#12915 = VERTEX_POINT('',#47180) ;
#12916 = VERTEX_POINT('',#47191) ;
#12917 = VERTEX_POINT('',#47208) ;
#12918 = VERTEX_POINT('',#47209) ;
#12919 = VERTEX_POINT('',#47284) ;
#12920 = VERTEX_POINT('',#47285) ;
#12921 = VERTEX_POINT('',#47362) ;
#12922 = VERTEX_POINT('',#47363) ;
#12923 = VERTEX_POINT('',#47440) ;
#12924 = VERTEX_POINT('',#47441) ;
#12925 = VERTEX_POINT('',#47443) ;
#12926 = VERTEX_POINT('',#47458) ;
#12927 = VERTEX_POINT('',#47479) ;
#12928 = VERTEX_POINT('',#47480) ;
#12929 = VERTEX_POINT('',#47482) ;
#12930 = VERTEX_POINT('',#47499) ;
#12931 = VERTEX_POINT('',#47522) ;
#12932 = VERTEX_POINT('',#47523) ;
#12933 = VERTEX_POINT('',#47598) ;
#12934 = VERTEX_POINT('',#47599) ;
#12935 = VERTEX_POINT('',#47674) ;
#12936 = VERTEX_POINT('',#47675) ;
#12937 = VERTEX_POINT('',#47754) ;
#12938 = VERTEX_POINT('',#47755) ;
#12939 = VERTEX_POINT('',#47830) ;
#12940 = VERTEX_POINT('',#47831) ;
#12941 = VERTEX_POINT('',#47833) ;
#12942 = VERTEX_POINT('',#47854) ;
#12943 = VERTEX_POINT('',#47881) ;
#12944 = VERTEX_POINT('',#47882) ;
#12945 = VERTEX_POINT('',#47897) ;
#12946 = VERTEX_POINT('',#48156) ;
#12947 = VERTEX_POINT('',#48157) ;
#12948 = VERTEX_POINT('',#48159) ;
#12949 = VERTEX_POINT('',#48167) ;
#12950 = VERTEX_POINT('',#48168) ;
#12951 = VERTEX_POINT('',#48170) ;
#12952 = VERTEX_POINT('',#48518) ;
#12953 = VERTEX_POINT('',#48520) ;
#12954 = VERTEX_POINT('',#48522) ;
#12955 = VERTEX_POINT('',#48524) ;
#12956 = VERTEX_POINT('',#48528) ;
#12957 = VERTEX_POINT('',#48529) ;
#12958 = VERTEX_POINT('',#48531) ;
#12959 = VERTEX_POINT('',#48535) ;
#12960 = VERTEX_POINT('',#48539) ;
#12961 = VERTEX_POINT('',#48548) ;
#12962 = VERTEX_POINT('',#48552) ;
#12963 = VERTEX_POINT('',#48556) ;
#12964 = VERTEX_POINT('',#48573) ;
#12965 = VERTEX_POINT('',#48577) ;
#12966 = VERTEX_POINT('',#48583) ;
#12967 = VERTEX_POINT('',#48587) ;
#12968 = VERTEX_POINT('',#48591) ;
#12969 = VERTEX_POINT('',#48600) ;
#12970 = VERTEX_POINT('',#48637) ;
#12971 = VERTEX_POINT('',#48638) ;
#12972 = VERTEX_POINT('',#48640) ;
#12973 = VERTEX_POINT('',#48649) ;
#12974 = VERTEX_POINT('',#48650) ;
#12975 = VERTEX_POINT('',#48688) ;
#12976 = VERTEX_POINT('',#48725) ;
#12977 = VERTEX_POINT('',#48726) ;
#12978 = VERTEX_POINT('',#48801) ;
#12979 = VERTEX_POINT('',#48802) ;
#12980 = VERTEX_POINT('',#48877) ;
#12981 = VERTEX_POINT('',#48878) ;
#12982 = VERTEX_POINT('',#48953) ;
#12983 = VERTEX_POINT('',#48954) ;
#12984 = VERTEX_POINT('',#49029) ;
#12985 = VERTEX_POINT('',#49030) ;
#12986 = VERTEX_POINT('',#49032) ;
#12987 = VERTEX_POINT('',#49055) ;
#12988 = VERTEX_POINT('',#49057) ;
#12989 = VERTEX_POINT('',#49059) ;
#12990 = VERTEX_POINT('',#49062) ;
#12991 = VERTEX_POINT('',#49083) ;
#12992 = VERTEX_POINT('',#49084) ;
#12993 = VERTEX_POINT('',#49159) ;
#12994 = VERTEX_POINT('',#49160) ;
#12995 = VERTEX_POINT('',#49235) ;
#12996 = VERTEX_POINT('',#49236) ;
#12997 = VERTEX_POINT('',#49313) ;
#12998 = VERTEX_POINT('',#49314) ;
#12999 = VERTEX_POINT('',#49391) ;
#13000 = VERTEX_POINT('',#49422) ;
#13001 = VERTEX_POINT('',#49451) ;
#13002 = VERTEX_POINT('',#49488) ;
#13003 = VERTEX_POINT('',#49523) ;
#13004 = VERTEX_POINT('',#49525) ;
#13005 = VERTEX_POINT('',#49527) ;
#13006 = VERTEX_POINT('',#49533) ;
#13007 = VERTEX_POINT('',#49534) ;
#13008 = VERTEX_POINT('',#49536) ;
#13009 = VERTEX_POINT('',#49538) ;
#13010 = VERTEX_POINT('',#49540) ;
#13011 = VERTEX_POINT('',#49542) ;
#13012 = VERTEX_POINT('',#49544) ;
#13013 = VERTEX_POINT('',#49546) ;
#13014 = VERTEX_POINT('',#49548) ;
#13015 = VERTEX_POINT('',#49550) ;
#13016 = VERTEX_POINT('',#49552) ;
#13017 = VERTEX_POINT('',#49554) ;
#13018 = VERTEX_POINT('',#49556) ;
#13019 = VERTEX_POINT('',#49558) ;
#13020 = VERTEX_POINT('',#49560) ;
#13021 = VERTEX_POINT('',#49562) ;
#13022 = VERTEX_POINT('',#49564) ;
#13023 = VERTEX_POINT('',#49566) ;
#13024 = VERTEX_POINT('',#49568) ;
#13025 = VERTEX_POINT('',#49570) ;
#13026 = VERTEX_POINT('',#49574) ;
#13027 = VERTEX_POINT('',#49603) ;
#13028 = VERTEX_POINT('',#49637) ;
#13029 = VERTEX_POINT('',#49638) ;
#13030 = VERTEX_POINT('',#49640) ;
#13031 = VERTEX_POINT('',#49642) ;
#13032 = VERTEX_POINT('',#49646) ;
#13033 = VERTEX_POINT('',#49650) ;
#13034 = VERTEX_POINT('',#49654) ;
#13035 = VERTEX_POINT('',#49658) ;
#13036 = VERTEX_POINT('',#49660) ;
#13037 = VERTEX_POINT('',#49664) ;
#13038 = VERTEX_POINT('',#49668) ;
#13039 = VERTEX_POINT('',#49672) ;
#13040 = VERTEX_POINT('',#49676) ;
#13041 = VERTEX_POINT('',#49678) ;
#13042 = VERTEX_POINT('',#49682) ;
#13043 = VERTEX_POINT('',#49686) ;
#13044 = VERTEX_POINT('',#49690) ;
#13045 = VERTEX_POINT('',#49694) ;
#13046 = VERTEX_POINT('',#49696) ;
#13047 = VERTEX_POINT('',#49700) ;
#13048 = VERTEX_POINT('',#49704) ;
#13049 = VERTEX_POINT('',#49708) ;
#13050 = VERTEX_POINT('',#50226) ;
#13051 = VERTEX_POINT('',#50227) ;
#13052 = VERTEX_POINT('',#50229) ;
#13053 = VERTEX_POINT('',#50258) ;
#13054 = VERTEX_POINT('',#50297) ;
#13055 = VERTEX_POINT('',#50298) ;
#13056 = VERTEX_POINT('',#50300) ;
#13057 = VERTEX_POINT('',#50536) ;
#13058 = VERTEX_POINT('',#50537) ;
#13059 = VERTEX_POINT('',#50539) ;
#13060 = VERTEX_POINT('',#50631) ;
#13061 = VERTEX_POINT('',#50672) ;
#13062 = VERTEX_POINT('',#50749) ;
#13063 = VERTEX_POINT('',#50750) ;
#13064 = VERTEX_POINT('',#50752) ;
#13065 = VERTEX_POINT('',#50759) ;
#13066 = VERTEX_POINT('',#50780) ;
#13067 = VERTEX_POINT('',#50781) ;
#13068 = VERTEX_POINT('',#50783) ;
#13069 = VERTEX_POINT('',#50902) ;
#13070 = VERTEX_POINT('',#51022) ;
#13071 = VERTEX_POINT('',#51023) ;
#13072 = VERTEX_POINT('',#51025) ;
#13073 = VERTEX_POINT('',#51050) ;
#13074 = VERTEX_POINT('',#51142) ;
#13075 = VERTEX_POINT('',#51183) ;
#13076 = VERTEX_POINT('',#51185) ;
#13077 = VERTEX_POINT('',#51287) ;
#13078 = VERTEX_POINT('',#51288) ;
#13079 = VERTEX_POINT('',#51290) ;
#13080 = VERTEX_POINT('',#51319) ;
#13081 = VERTEX_POINT('',#51358) ;
#13082 = VERTEX_POINT('',#51359) ;
#13083 = VERTEX_POINT('',#51361) ;
#13084 = VERTEX_POINT('',#51599) ;
#13085 = VERTEX_POINT('',#51600) ;
#13086 = VERTEX_POINT('',#51602) ;
#13087 = VERTEX_POINT('',#51694) ;
#13088 = VERTEX_POINT('',#51735) ;
#13089 = VERTEX_POINT('',#51737) ;
#13090 = VERTEX_POINT('',#51823) ;
#13091 = VERTEX_POINT('',#51824) ;
#13092 = VERTEX_POINT('',#51826) ;
#13093 = VERTEX_POINT('',#51853) ;
#13094 = VERTEX_POINT('',#51892) ;
#13095 = VERTEX_POINT('',#51893) ;
#13096 = VERTEX_POINT('',#51895) ;
#13097 = VERTEX_POINT('',#52131) ;
#13098 = VERTEX_POINT('',#52132) ;
#13099 = VERTEX_POINT('',#52134) ;
#13100 = VERTEX_POINT('',#52226) ;
#13101 = VERTEX_POINT('',#52267) ;
#13102 = VERTEX_POINT('',#52346) ;
#13103 = VERTEX_POINT('',#52347) ;
#13104 = VERTEX_POINT('',#52349) ;
#13105 = VERTEX_POINT('',#52395) ;
#13106 = VERTEX_POINT('',#52396) ;
#13107 = VERTEX_POINT('',#52398) ;
#13108 = VERTEX_POINT('',#52704) ;
#13109 = VERTEX_POINT('',#52705) ;
#13110 = VERTEX_POINT('',#52707) ;
#13111 = VERTEX_POINT('',#52718) ;
#13112 = VERTEX_POINT('',#52849) ;
#13113 = VERTEX_POINT('',#52851) ;
#13114 = VERTEX_POINT('',#53060) ;
#13115 = VERTEX_POINT('',#53061) ;
#13116 = VERTEX_POINT('',#53063) ;
#13117 = VERTEX_POINT('',#53109) ;
#13118 = VERTEX_POINT('',#53110) ;
#13119 = VERTEX_POINT('',#53112) ;
#13120 = VERTEX_POINT('',#53418) ;
#13121 = VERTEX_POINT('',#53419) ;
#13122 = VERTEX_POINT('',#53421) ;
#13123 = VERTEX_POINT('',#53432) ;
#13124 = VERTEX_POINT('',#53563) ;
#13125 = VERTEX_POINT('',#53565) ;
#13126 = VERTEX_POINT('',#53774) ;
#13127 = VERTEX_POINT('',#53775) ;
#13128 = VERTEX_POINT('',#53777) ;
#13129 = VERTEX_POINT('',#53823) ;
#13130 = VERTEX_POINT('',#53824) ;
#13131 = VERTEX_POINT('',#53826) ;
#13132 = VERTEX_POINT('',#54132) ;
#13133 = VERTEX_POINT('',#54133) ;
#13134 = VERTEX_POINT('',#54135) ;
#13135 = VERTEX_POINT('',#54146) ;
#13136 = VERTEX_POINT('',#54277) ;
#13137 = VERTEX_POINT('',#54279) ;
#13138 = VERTEX_POINT('',#54488) ;
#13139 = VERTEX_POINT('',#54489) ;
#13140 = VERTEX_POINT('',#54491) ;
#13141 = VERTEX_POINT('',#54537) ;
#13142 = VERTEX_POINT('',#54538) ;
#13143 = VERTEX_POINT('',#54540) ;
#13144 = VERTEX_POINT('',#54846) ;
#13145 = VERTEX_POINT('',#54847) ;
#13146 = VERTEX_POINT('',#54849) ;
#13147 = VERTEX_POINT('',#54860) ;
#13148 = VERTEX_POINT('',#54991) ;
#13149 = VERTEX_POINT('',#54993) ;
#13150 = VERTEX_POINT('',#55202) ;
#13151 = VERTEX_POINT('',#55203) ;
#13152 = VERTEX_POINT('',#55205) ;
#13153 = VERTEX_POINT('',#55234) ;
#13154 = VERTEX_POINT('',#55273) ;
#13155 = VERTEX_POINT('',#55274) ;
#13156 = VERTEX_POINT('',#55276) ;
#13157 = VERTEX_POINT('',#55508) ;
#13158 = VERTEX_POINT('',#55509) ;
#13159 = VERTEX_POINT('',#55511) ;
#13160 = VERTEX_POINT('',#55603) ;
#13161 = VERTEX_POINT('',#55644) ;
#13162 = VERTEX_POINT('',#55721) ;
#13163 = VERTEX_POINT('',#55722) ;
#13164 = VERTEX_POINT('',#55724) ;
#13165 = VERTEX_POINT('',#55753) ;
#13166 = VERTEX_POINT('',#55792) ;
#13167 = VERTEX_POINT('',#55793) ;
#13168 = VERTEX_POINT('',#55795) ;
#13169 = VERTEX_POINT('',#56033) ;
#13170 = VERTEX_POINT('',#56034) ;
#13171 = VERTEX_POINT('',#56036) ;
#13172 = VERTEX_POINT('',#56128) ;
#13173 = VERTEX_POINT('',#56169) ;
#13174 = VERTEX_POINT('',#56171) ;
#13175 = VERTEX_POINT('',#56257) ;
#13176 = VERTEX_POINT('',#56258) ;
#13177 = VERTEX_POINT('',#56260) ;
#13178 = VERTEX_POINT('',#56306) ;
#13179 = VERTEX_POINT('',#56307) ;
#13180 = VERTEX_POINT('',#56309) ;
#13181 = VERTEX_POINT('',#56615) ;
#13182 = VERTEX_POINT('',#56616) ;
#13183 = VERTEX_POINT('',#56618) ;
#13184 = VERTEX_POINT('',#56629) ;
#13185 = VERTEX_POINT('',#56760) ;
#13186 = VERTEX_POINT('',#56762) ;
#13187 = VERTEX_POINT('',#56971) ;
#13188 = VERTEX_POINT('',#56972) ;
#13189 = VERTEX_POINT('',#56974) ;
#13190 = VERTEX_POINT('',#57020) ;
#13191 = VERTEX_POINT('',#57021) ;
#13192 = VERTEX_POINT('',#57023) ;
#13193 = VERTEX_POINT('',#57327) ;
#13194 = VERTEX_POINT('',#57328) ;
#13195 = VERTEX_POINT('',#57330) ;
#13196 = VERTEX_POINT('',#57341) ;
#13197 = VERTEX_POINT('',#57472) ;
#13198 = VERTEX_POINT('',#57474) ;
#13199 = VERTEX_POINT('',#57683) ;
#13200 = VERTEX_POINT('',#57684) ;
#13201 = VERTEX_POINT('',#57686) ;
#13202 = VERTEX_POINT('',#57713) ;
#13203 = VERTEX_POINT('',#57752) ;
#13204 = VERTEX_POINT('',#57753) ;
#13205 = VERTEX_POINT('',#57755) ;
#13206 = VERTEX_POINT('',#57995) ;
#13207 = VERTEX_POINT('',#57996) ;
#13208 = VERTEX_POINT('',#57998) ;
#13209 = VERTEX_POINT('',#58090) ;
#13210 = VERTEX_POINT('',#58131) ;
#13211 = VERTEX_POINT('',#58212) ;
#13212 = VERTEX_POINT('',#58213) ;
#13213 = VERTEX_POINT('',#58215) ;
#13214 = VERTEX_POINT('',#58242) ;
#13215 = VERTEX_POINT('',#58281) ;
#13216 = VERTEX_POINT('',#58282) ;
#13217 = VERTEX_POINT('',#58284) ;
#13218 = VERTEX_POINT('',#58522) ;
#13219 = VERTEX_POINT('',#58523) ;
#13220 = VERTEX_POINT('',#58525) ;
#13221 = VERTEX_POINT('',#58617) ;
#13222 = VERTEX_POINT('',#58658) ;
#13223 = VERTEX_POINT('',#58735) ;
#13224 = VERTEX_POINT('',#58736) ;
#13225 = VERTEX_POINT('',#58738) ;
#13226 = VERTEX_POINT('',#58784) ;
#13227 = VERTEX_POINT('',#58785) ;
#13228 = VERTEX_POINT('',#58787) ;
#13229 = VERTEX_POINT('',#59093) ;
#13230 = VERTEX_POINT('',#59094) ;
#13231 = VERTEX_POINT('',#59096) ;
#13232 = VERTEX_POINT('',#59107) ;
#13233 = VERTEX_POINT('',#59238) ;
#13234 = VERTEX_POINT('',#59240) ;
#13235 = VERTEX_POINT('',#59449) ;
#13236 = VERTEX_POINT('',#59450) ;
#13237 = VERTEX_POINT('',#59452) ;
#13238 = VERTEX_POINT('',#59498) ;
#13239 = VERTEX_POINT('',#59499) ;
#13240 = VERTEX_POINT('',#59501) ;
#13241 = VERTEX_POINT('',#59807) ;
#13242 = VERTEX_POINT('',#59808) ;
#13243 = VERTEX_POINT('',#59810) ;
#13244 = VERTEX_POINT('',#59821) ;
#13245 = VERTEX_POINT('',#59952) ;
#13246 = VERTEX_POINT('',#59954) ;
#13247 = VERTEX_POINT('',#61455) ;
#13248 = VERTEX_POINT('',#62981) ;
#13249 = VERTEX_POINT('',#63657) ;
#13250 = VERTEX_POINT('',#63658) ;
#13251 = VERTEX_POINT('',#63660) ;
#13252 = VERTEX_POINT('',#63662) ;
#13253 = VERTEX_POINT('',#63666) ;
#13254 = VERTEX_POINT('',#63667) ;
#13255 = VERTEX_POINT('',#63669) ;
#13256 = VERTEX_POINT('',#63671) ;
#13257 = VERTEX_POINT('',#63675) ;
#13258 = VERTEX_POINT('',#63676) ;
#13259 = VERTEX_POINT('',#63678) ;
#13260 = VERTEX_POINT('',#63680) ;
#13261 = VERTEX_POINT('',#63684) ;
#13262 = VERTEX_POINT('',#63685) ;
#13263 = VERTEX_POINT('',#63687) ;
#13264 = VERTEX_POINT('',#63689) ;
#13265 = VERTEX_POINT('',#63693) ;
#13266 = VERTEX_POINT('',#63694) ;
#13267 = VERTEX_POINT('',#63696) ;
#13268 = VERTEX_POINT('',#63698) ;
#13269 = VERTEX_POINT('',#63702) ;
#13270 = VERTEX_POINT('',#63704) ;
#13271 = VERTEX_POINT('',#63707) ;
#13272 = VERTEX_POINT('',#63709) ;
#13273 = VERTEX_POINT('',#63711) ;
#13274 = VERTEX_POINT('',#63713) ;
#13275 = VERTEX_POINT('',#63718) ;
#13276 = VERTEX_POINT('',#63719) ;
#13277 = VERTEX_POINT('',#63721) ;
#13278 = VERTEX_POINT('',#63723) ;
#13279 = VERTEX_POINT('',#63727) ;
#13280 = VERTEX_POINT('',#63728) ;
#13281 = VERTEX_POINT('',#63730) ;
#13282 = VERTEX_POINT('',#63732) ;
#13283 = VERTEX_POINT('',#63737) ;
#13284 = VERTEX_POINT('',#63739) ;
#13285 = VERTEX_POINT('',#63741) ;
#13286 = VERTEX_POINT('',#63743) ;
#13287 = VERTEX_POINT('',#63745) ;
#13288 = VERTEX_POINT('',#63747) ;
#13289 = VERTEX_POINT('',#63749) ;
#13290 = VERTEX_POINT('',#63751) ;
#13291 = VERTEX_POINT('',#63753) ;
#13292 = VERTEX_POINT('',#63755) ;
#13293 = VERTEX_POINT('',#63757) ;
#13294 = VERTEX_POINT('',#63760) ;
#13295 = VERTEX_POINT('',#63761) ;
#13296 = VERTEX_POINT('',#63763) ;
#13297 = VERTEX_POINT('',#63765) ;
#13298 = VERTEX_POINT('',#63767) ;
#13299 = VERTEX_POINT('',#63769) ;
#13300 = VERTEX_POINT('',#63771) ;
#13301 = VERTEX_POINT('',#63773) ;
#13302 = VERTEX_POINT('',#63775) ;
#13303 = VERTEX_POINT('',#63777) ;
#13304 = VERTEX_POINT('',#63779) ;
#13305 = VERTEX_POINT('',#63781) ;
#13306 = VERTEX_POINT('',#63783) ;
#13307 = VERTEX_POINT('',#63785) ;
#13308 = VERTEX_POINT('',#63788) ;
#13309 = VERTEX_POINT('',#63963) ;
#13310 = VERTEX_POINT('',#64138) ;
#13311 = VERTEX_POINT('',#64140) ;
#13312 = VERTEX_POINT('',#64141) ;
#13313 = VERTEX_POINT('',#64143) ;
#13314 = VERTEX_POINT('',#64145) ;
#13315 = VERTEX_POINT('',#64148) ;
#13316 = VERTEX_POINT('',#64149) ;
#13317 = VERTEX_POINT('',#64151) ;
#13318 = VERTEX_POINT('',#64153) ;
#13319 = VERTEX_POINT('',#64156) ;
#13320 = VERTEX_POINT('',#64157) ;
#13321 = VERTEX_POINT('',#64159) ;
#13322 = VERTEX_POINT('',#64161) ;
#13323 = VERTEX_POINT('',#64164) ;
#13324 = VERTEX_POINT('',#64167) ;
#13325 = VERTEX_POINT('',#64168) ;
#13326 = VERTEX_POINT('',#64170) ;
#13327 = VERTEX_POINT('',#64172) ;
#13328 = VERTEX_POINT('',#64177) ;
#13329 = VERTEX_POINT('',#64179) ;
#13330 = VERTEX_POINT('',#64182) ;
#13331 = VERTEX_POINT('',#64184) ;
#13332 = VERTEX_POINT('',#64186) ;
#13333 = VERTEX_POINT('',#64188) ;
#13334 = VERTEX_POINT('',#64190) ;
#13335 = VERTEX_POINT('',#64192) ;
#13336 = VERTEX_POINT('',#64194) ;
#13337 = VERTEX_POINT('',#64196) ;
#13338 = VERTEX_POINT('',#64198) ;
#13339 = VERTEX_POINT('',#64200) ;
#13340 = VERTEX_POINT('',#64202) ;
#13341 = VERTEX_POINT('',#64204) ;
#13342 = VERTEX_POINT('',#64206) ;
#13343 = VERTEX_POINT('',#64208) ;
#13344 = VERTEX_POINT('',#64211) ;
#13345 = VERTEX_POINT('',#64213) ;
#13346 = VERTEX_POINT('',#64214) ;
#13347 = VERTEX_POINT('',#64216) ;
#13348 = VERTEX_POINT('',#64218) ;
#13349 = VERTEX_POINT('',#64221) ;
#13350 = VERTEX_POINT('',#64222) ;
#13351 = VERTEX_POINT('',#64224) ;
#13352 = VERTEX_POINT('',#64226) ;
#13353 = VERTEX_POINT('',#64229) ;
#13354 = VERTEX_POINT('',#64230) ;
#13355 = VERTEX_POINT('',#64232) ;
#13356 = VERTEX_POINT('',#64234) ;
#13357 = VERTEX_POINT('',#64237) ;
#13358 = VERTEX_POINT('',#64238) ;
#13359 = VERTEX_POINT('',#64240) ;
#13360 = VERTEX_POINT('',#64242) ;
#13361 = VERTEX_POINT('',#64245) ;
#13362 = VERTEX_POINT('',#64247) ;
#13363 = VERTEX_POINT('',#64422) ;
#13364 = VERTEX_POINT('',#64597) ;
#13365 = VERTEX_POINT('',#64598) ;
#13366 = VERTEX_POINT('',#64600) ;
#13367 = VERTEX_POINT('',#64602) ;
#13368 = VERTEX_POINT('',#64604) ;
#13369 = VERTEX_POINT('',#64606) ;
#13370 = VERTEX_POINT('',#64608) ;
#13371 = VERTEX_POINT('',#64610) ;
#13372 = VERTEX_POINT('',#64613) ;
#13373 = VERTEX_POINT('',#64614) ;
#13374 = VERTEX_POINT('',#64616) ;
#13375 = VERTEX_POINT('',#64618) ;
#13376 = VERTEX_POINT('',#64620) ;
#13377 = VERTEX_POINT('',#64622) ;
#13378 = VERTEX_POINT('',#64624) ;
#13379 = VERTEX_POINT('',#64626) ;
#13380 = VERTEX_POINT('',#64628) ;
#13381 = VERTEX_POINT('',#64630) ;
#13382 = VERTEX_POINT('',#64634) ;
#13383 = VERTEX_POINT('',#64636) ;
#13384 = VERTEX_POINT('',#64638) ;
#13385 = VERTEX_POINT('',#64640) ;
#13386 = VERTEX_POINT('',#64642) ;
#13387 = VERTEX_POINT('',#64644) ;
#13388 = VERTEX_POINT('',#64646) ;
#13389 = VERTEX_POINT('',#64648) ;
#13390 = VERTEX_POINT('',#64650) ;
#13391 = VERTEX_POINT('',#64652) ;
#13392 = VERTEX_POINT('',#64654) ;
#13393 = VERTEX_POINT('',#64658) ;
#13394 = VERTEX_POINT('',#64660) ;
#13395 = VERTEX_POINT('',#64661) ;
#13396 = VERTEX_POINT('',#64663) ;
#13397 = VERTEX_POINT('',#64665) ;
#13398 = VERTEX_POINT('',#64668) ;
#13399 = VERTEX_POINT('',#64669) ;
#13400 = VERTEX_POINT('',#64671) ;
#13401 = VERTEX_POINT('',#64673) ;
#13402 = VERTEX_POINT('',#64676) ;
#13403 = VERTEX_POINT('',#64677) ;
#13404 = VERTEX_POINT('',#64679) ;
#13405 = VERTEX_POINT('',#64681) ;
#13406 = VERTEX_POINT('',#64684) ;
#13407 = VERTEX_POINT('',#64685) ;
#13408 = VERTEX_POINT('',#64687) ;
#13409 = VERTEX_POINT('',#64689) ;
#13410 = VERTEX_POINT('',#64691) ;
#13411 = VERTEX_POINT('',#64693) ;
#13412 = VERTEX_POINT('',#64696) ;
#13413 = VERTEX_POINT('',#64780) ;
#13414 = VERTEX_POINT('',#64955) ;
#13415 = VERTEX_POINT('',#65049) ;
#13416 = VERTEX_POINT('',#65051) ;
#13417 = VERTEX_POINT('',#65053) ;
#13418 = VERTEX_POINT('',#65055) ;
#13419 = VERTEX_POINT('',#65057) ;
#13420 = VERTEX_POINT('',#65059) ;
#13421 = VERTEX_POINT('',#65061) ;
#13422 = VERTEX_POINT('',#65063) ;
#13423 = VERTEX_POINT('',#65065) ;
#13424 = VERTEX_POINT('',#65067) ;
#13425 = VERTEX_POINT('',#65069) ;
#13426 = VERTEX_POINT('',#65071) ;
#13427 = VERTEX_POINT('',#65073) ;
#13428 = VERTEX_POINT('',#65075) ;
#13429 = VERTEX_POINT('',#65077) ;
#13430 = VERTEX_POINT('',#65079) ;
#13431 = VERTEX_POINT('',#65081) ;
#13432 = VERTEX_POINT('',#65083) ;
#13433 = VERTEX_POINT('',#65085) ;
#13434 = VERTEX_POINT('',#65089) ;
#13435 = VERTEX_POINT('',#65090) ;
#13436 = VERTEX_POINT('',#65092) ;
#13437 = VERTEX_POINT('',#65094) ;
#13438 = VERTEX_POINT('',#65096) ;
#13439 = VERTEX_POINT('',#65098) ;
#13440 = VERTEX_POINT('',#65100) ;
#13441 = VERTEX_POINT('',#65102) ;
#13442 = VERTEX_POINT('',#65187) ;
#13443 = VERTEX_POINT('',#65362) ;
#13444 = VERTEX_POINT('',#65455) ;
#13445 = VERTEX_POINT('',#65456) ;
#13446 = VERTEX_POINT('',#65458) ;
#13447 = VERTEX_POINT('',#65460) ;
#13448 = VERTEX_POINT('',#65462) ;
#13449 = VERTEX_POINT('',#65464) ;
#13450 = VERTEX_POINT('',#65467) ;
#13451 = VERTEX_POINT('',#65468) ;
#13452 = VERTEX_POINT('',#65470) ;
#13453 = VERTEX_POINT('',#65472) ;
#13454 = VERTEX_POINT('',#65475) ;
#13455 = VERTEX_POINT('',#65476) ;
#13456 = VERTEX_POINT('',#65478) ;
#13457 = VERTEX_POINT('',#65480) ;
#13458 = VERTEX_POINT('',#65483) ;
#13459 = VERTEX_POINT('',#65484) ;
#13460 = VERTEX_POINT('',#65486) ;
#13461 = VERTEX_POINT('',#65488) ;
#13462 = VERTEX_POINT('',#65491) ;
#13463 = VERTEX_POINT('',#65492) ;
#13464 = VERTEX_POINT('',#65494) ;
#13465 = VERTEX_POINT('',#65496) ;
#13466 = VERTEX_POINT('',#65499) ;
#13467 = VERTEX_POINT('',#65501) ;
#13468 = VERTEX_POINT('',#65504) ;
#13469 = VERTEX_POINT('',#65506) ;
#13470 = VERTEX_POINT('',#65512) ;
#13471 = VERTEX_POINT('',#65514) ;
#13472 = VERTEX_POINT('',#65516) ;
#13473 = VERTEX_POINT('',#65518) ;
#13474 = VERTEX_POINT('',#65529) ;
#13475 = VERTEX_POINT('',#65531) ;
#13476 = VERTEX_POINT('',#65535) ;
#13477 = VERTEX_POINT('',#65539) ;
#13478 = VERTEX_POINT('',#65543) ;
#13479 = VERTEX_POINT('',#65547) ;
#13480 = VERTEX_POINT('',#65549) ;
#13481 = VERTEX_POINT('',#65555) ;
#13482 = VERTEX_POINT('',#65557) ;
#13483 = VERTEX_POINT('',#65561) ;
#13484 = VERTEX_POINT('',#65608) ;
#13485 = VERTEX_POINT('',#65621) ;
#13486 = VERTEX_POINT('',#65625) ;
#13487 = VERTEX_POINT('',#65631) ;
#13488 = VERTEX_POINT('',#65640) ;
#13489 = VERTEX_POINT('',#65646) ;
#13490 = VERTEX_POINT('',#65648) ;
#13491 = VERTEX_POINT('',#65652) ;
#13492 = VERTEX_POINT('',#65654) ;
#13493 = VERTEX_POINT('',#65658) ;
#13494 = VERTEX_POINT('',#65660) ;
#13495 = VERTEX_POINT('',#65664) ;
#13496 = VERTEX_POINT('',#65668) ;
#13497 = VERTEX_POINT('',#65672) ;
#13498 = VERTEX_POINT('',#65676) ;
#13499 = VERTEX_POINT('',#65680) ;
#13500 = VERTEX_POINT('',#65682) ;
#13501 = VERTEX_POINT('',#65686) ;
#13502 = VERTEX_POINT('',#65690) ;
#13503 = VERTEX_POINT('',#65694) ;
#13504 = VERTEX_POINT('',#65698) ;
#13505 = VERTEX_POINT('',#65702) ;
#13506 = VERTEX_POINT('',#65704) ;
#13507 = VERTEX_POINT('',#65708) ;
#13508 = VERTEX_POINT('',#65712) ;
#13509 = VERTEX_POINT('',#65716) ;
#13510 = VERTEX_POINT('',#65720) ;
#13511 = VERTEX_POINT('',#65724) ;
#13512 = VERTEX_POINT('',#65726) ;
#13513 = VERTEX_POINT('',#65730) ;
#13514 = VERTEX_POINT('',#65734) ;
#13515 = VERTEX_POINT('',#65738) ;
#13516 = VERTEX_POINT('',#65742) ;
#13517 = VERTEX_POINT('',#65746) ;
#13518 = VERTEX_POINT('',#65747) ;
#13519 = VERTEX_POINT('',#65749) ;
#13520 = VERTEX_POINT('',#65751) ;
#13521 = VERTEX_POINT('',#65755) ;
#13522 = VERTEX_POINT('',#65757) ;
#13523 = VERTEX_POINT('',#65761) ;
#13524 = VERTEX_POINT('',#65763) ;
#13525 = VERTEX_POINT('',#65767) ;
#13526 = VERTEX_POINT('',#65769) ;
#13527 = VERTEX_POINT('',#65773) ;
#13528 = VERTEX_POINT('',#65775) ;
#13529 = VERTEX_POINT('',#65782) ;
#13530 = VERTEX_POINT('',#65783) ;
#13531 = VERTEX_POINT('',#65785) ;
#13532 = VERTEX_POINT('',#65787) ;
#13533 = VERTEX_POINT('',#65791) ;
#13534 = VERTEX_POINT('',#65793) ;
#13535 = VERTEX_POINT('',#65797) ;
#13536 = VERTEX_POINT('',#65799) ;
#13537 = VERTEX_POINT('',#65803) ;
#13538 = VERTEX_POINT('',#65805) ;
#13539 = VERTEX_POINT('',#65809) ;
#13540 = VERTEX_POINT('',#65811) ;
#13541 = VERTEX_POINT('',#65820) ;
#13542 = VERTEX_POINT('',#65822) ;
#13543 = VERTEX_POINT('',#65826) ;
#13544 = VERTEX_POINT('',#65828) ;
#13545 = VERTEX_POINT('',#65832) ;
#13546 = VERTEX_POINT('',#65836) ;
#13547 = VERTEX_POINT('',#65838) ;
#13548 = VERTEX_POINT('',#65842) ;
#13549 = VERTEX_POINT('',#65844) ;
#13550 = VERTEX_POINT('',#65848) ;
#13551 = VERTEX_POINT('',#65850) ;
#13552 = VERTEX_POINT('',#65855) ;
#13553 = VERTEX_POINT('',#65861) ;
#13554 = VERTEX_POINT('',#65867) ;
#13555 = VERTEX_POINT('',#65873) ;
#13556 = VERTEX_POINT('',#65877) ;
#13557 = VERTEX_POINT('',#65881) ;
#13558 = VERTEX_POINT('',#65883) ;
#13559 = VERTEX_POINT('',#65885) ;
#13560 = VERTEX_POINT('',#65889) ;
#13561 = VERTEX_POINT('',#65893) ;
#13562 = VERTEX_POINT('',#65894) ;
#13563 = VERTEX_POINT('',#65896) ;
#13564 = VERTEX_POINT('',#65898) ;
#13565 = VERTEX_POINT('',#65902) ;
#13566 = VERTEX_POINT('',#65903) ;
#13567 = VERTEX_POINT('',#65905) ;
#13568 = VERTEX_POINT('',#65907) ;
#13569 = VERTEX_POINT('',#65911) ;
#13570 = VERTEX_POINT('',#65912) ;
#13571 = VERTEX_POINT('',#65914) ;
#13572 = VERTEX_POINT('',#65916) ;
#13573 = VERTEX_POINT('',#65920) ;
#13574 = VERTEX_POINT('',#65921) ;
#13575 = VERTEX_POINT('',#65923) ;
#13576 = VERTEX_POINT('',#65925) ;
#13577 = VERTEX_POINT('',#65929) ;
#13578 = VERTEX_POINT('',#65931) ;
#13579 = VERTEX_POINT('',#65935) ;
#13580 = VERTEX_POINT('',#65936) ;
#13581 = VERTEX_POINT('',#65938) ;
#13582 = VERTEX_POINT('',#65940) ;
#13583 = VERTEX_POINT('',#65944) ;
#13584 = VERTEX_POINT('',#65946) ;
#13585 = VERTEX_POINT('',#66000) ;
#13586 = VERTEX_POINT('',#66005) ;
#13587 = VERTEX_POINT('',#66009) ;
#13588 = VERTEX_POINT('',#66013) ;
#13589 = VERTEX_POINT('',#66018) ;
#13590 = VERTEX_POINT('',#66022) ;
#13591 = VERTEX_POINT('',#66026) ;
#13592 = VERTEX_POINT('',#66030) ;
#13593 = VERTEX_POINT('',#66048) ;
#13594 = VERTEX_POINT('',#66049) ;
#13595 = VERTEX_POINT('',#66052) ;
#13596 = VERTEX_POINT('',#66054) ;
#13597 = VERTEX_POINT('',#66057) ;
#13598 = VERTEX_POINT('',#66059) ;
#13599 = VERTEX_POINT('',#66061) ;
#13600 = VERTEX_POINT('',#66063) ;
#13601 = VERTEX_POINT('',#66065) ;
#13602 = VERTEX_POINT('',#66067) ;
#13603 = VERTEX_POINT('',#66070) ;
#13604 = VERTEX_POINT('',#66072) ;
#13605 = VERTEX_POINT('',#66074) ;
#13606 = VERTEX_POINT('',#66076) ;
#13607 = VERTEX_POINT('',#66079) ;
#13608 = VERTEX_POINT('',#66081) ;
#13609 = VERTEX_POINT('',#66085) ;
#13610 = VERTEX_POINT('',#66087) ;
#13611 = VERTEX_POINT('',#66089) ;
#13612 = VERTEX_POINT('',#66095) ;
#13613 = VERTEX_POINT('',#66097) ;
#13614 = VERTEX_POINT('',#66099) ;
#13615 = VERTEX_POINT('',#66105) ;
#13616 = VERTEX_POINT('',#66107) ;
#13617 = VERTEX_POINT('',#66109) ;
#13618 = VERTEX_POINT('',#66115) ;
#13619 = VERTEX_POINT('',#66117) ;
#13620 = VERTEX_POINT('',#66119) ;
#13621 = VERTEX_POINT('',#66125) ;
#13622 = VERTEX_POINT('',#66126) ;
#13623 = VERTEX_POINT('',#66136) ;
#13624 = VERTEX_POINT('',#66153) ;
#13625 = VERTEX_POINT('',#66155) ;
#13626 = VERTEX_POINT('',#66190) ;
#13627 = VERTEX_POINT('',#66197) ;
#13628 = VERTEX_POINT('',#66208) ;
#13629 = VERTEX_POINT('',#66209) ;
#13630 = VERTEX_POINT('',#66214) ;
#13631 = VERTEX_POINT('',#66215) ;
#13632 = VERTEX_POINT('',#66958) ;
#13633 = VERTEX_POINT('',#66960) ;
#13634 = VERTEX_POINT('',#66964) ;
#13635 = VERTEX_POINT('',#66966) ;
#13636 = VERTEX_POINT('',#66970) ;
#13637 = VERTEX_POINT('',#66972) ;
#13638 = VERTEX_POINT('',#66976) ;
#13639 = VERTEX_POINT('',#66978) ;
#13640 = VERTEX_POINT('',#67006) ;
#13641 = VERTEX_POINT('',#67008) ;
#13642 = VERTEX_POINT('',#67014) ;
#13643 = VERTEX_POINT('',#67022) ;
#13644 = VERTEX_POINT('',#67026) ;
#13645 = VERTEX_POINT('',#67030) ;
#13646 = VERTEX_POINT('',#67032) ;
#13647 = VERTEX_POINT('',#67057) ;
#13648 = VERTEX_POINT('',#67059) ;
#13649 = VERTEX_POINT('',#67061) ;
#13650 = VERTEX_POINT('',#67261) ;
#13651 = VERTEX_POINT('',#67446) ;
#13652 = VERTEX_POINT('',#67795) ;
#13653 = VERTEX_POINT('',#67980) ;
#13654 = VERTEX_POINT('',#68329) ;
#13655 = VERTEX_POINT('',#68514) ;
#13656 = VERTEX_POINT('',#68690) ;
#13657 = VERTEX_POINT('',#68691) ;
#13658 = VERTEX_POINT('',#68693) ;
#13659 = VERTEX_POINT('',#68695) ;
#13660 = VERTEX_POINT('',#68697) ;
#13661 = VERTEX_POINT('',#68699) ;
#13662 = VERTEX_POINT('',#68702) ;
#13663 = VERTEX_POINT('',#68703) ;
#13664 = VERTEX_POINT('',#68705) ;
#13665 = VERTEX_POINT('',#68707) ;
#13666 = VERTEX_POINT('',#68709) ;
#13667 = VERTEX_POINT('',#68711) ;
#13668 = VERTEX_POINT('',#68714) ;
#13669 = VERTEX_POINT('',#68715) ;
#13670 = VERTEX_POINT('',#68717) ;
#13671 = VERTEX_POINT('',#68719) ;
#13672 = VERTEX_POINT('',#68721) ;
#13673 = VERTEX_POINT('',#68723) ;
#13674 = VERTEX_POINT('',#68808) ;
#13675 = VERTEX_POINT('',#69167) ;
#13676 = VERTEX_POINT('',#69261) ;
#13677 = VERTEX_POINT('',#69262) ;
#13678 = VERTEX_POINT('',#69267) ;
#13679 = VERTEX_POINT('',#69271) ;
#13680 = VERTEX_POINT('',#69275) ;
#13681 = VERTEX_POINT('',#69279) ;
#13682 = VERTEX_POINT('',#69285) ;
#13683 = VERTEX_POINT('',#69286) ;
#13684 = VERTEX_POINT('',#69291) ;
#13685 = VERTEX_POINT('',#69295) ;
#13686 = VERTEX_POINT('',#69299) ;
#13687 = VERTEX_POINT('',#69303) ;
#13688 = VERTEX_POINT('',#69309) ;
#13689 = VERTEX_POINT('',#69310) ;
#13690 = VERTEX_POINT('',#69312) ;
#13691 = VERTEX_POINT('',#69314) ;
#13692 = VERTEX_POINT('',#69316) ;
#13693 = VERTEX_POINT('',#69318) ;
#13694 = VERTEX_POINT('',#69341) ;
#13695 = VERTEX_POINT('',#69342) ;
#13696 = VERTEX_POINT('',#69344) ;
#13697 = VERTEX_POINT('',#69346) ;
#13698 = VERTEX_POINT('',#69350) ;
#13699 = VERTEX_POINT('',#69352) ;
#13700 = VERTEX_POINT('',#69356) ;
#13701 = VERTEX_POINT('',#69358) ;
#13702 = VERTEX_POINT('',#69364) ;
#13703 = VERTEX_POINT('',#69365) ;
#13704 = VERTEX_POINT('',#69367) ;
#13705 = VERTEX_POINT('',#69369) ;
#13706 = VERTEX_POINT('',#69373) ;
#13707 = VERTEX_POINT('',#69375) ;
#13708 = VERTEX_POINT('',#69379) ;
#13709 = VERTEX_POINT('',#69381) ;
#13710 = VERTEX_POINT('',#69387) ;
#13711 = VERTEX_POINT('',#69388) ;
#13712 = VERTEX_POINT('',#69390) ;
#13713 = VERTEX_POINT('',#69392) ;
#13714 = VERTEX_POINT('',#69396) ;
#13715 = VERTEX_POINT('',#69398) ;
#13716 = VERTEX_POINT('',#69402) ;
#13717 = VERTEX_POINT('',#69404) ;
#13718 = VERTEX_POINT('',#69410) ;
#13719 = VERTEX_POINT('',#69411) ;
#13720 = VERTEX_POINT('',#69413) ;
#13721 = VERTEX_POINT('',#69415) ;
#13722 = VERTEX_POINT('',#69419) ;
#13723 = VERTEX_POINT('',#69421) ;
#13724 = VERTEX_POINT('',#69425) ;
#13725 = VERTEX_POINT('',#69427) ;
#13726 = VERTEX_POINT('',#69433) ;
#13727 = VERTEX_POINT('',#69434) ;
#13728 = VERTEX_POINT('',#69436) ;
#13729 = VERTEX_POINT('',#69438) ;
#13730 = VERTEX_POINT('',#69442) ;
#13731 = VERTEX_POINT('',#69444) ;
#13732 = VERTEX_POINT('',#69448) ;
#13733 = VERTEX_POINT('',#69450) ;
#13734 = VERTEX_POINT('',#69456) ;
#13735 = VERTEX_POINT('',#69457) ;
#13736 = VERTEX_POINT('',#69459) ;
#13737 = VERTEX_POINT('',#69461) ;
#13738 = VERTEX_POINT('',#69465) ;
#13739 = VERTEX_POINT('',#69467) ;
#13740 = VERTEX_POINT('',#69471) ;
#13741 = VERTEX_POINT('',#69473) ;
#13742 = VERTEX_POINT('',#69479) ;
#13743 = VERTEX_POINT('',#69480) ;
#13744 = VERTEX_POINT('',#69482) ;
#13745 = VERTEX_POINT('',#69484) ;
#13746 = VERTEX_POINT('',#69488) ;
#13747 = VERTEX_POINT('',#69490) ;
#13748 = VERTEX_POINT('',#69494) ;
#13749 = VERTEX_POINT('',#69496) ;
#13750 = VERTEX_POINT('',#69502) ;
#13751 = VERTEX_POINT('',#69503) ;
#13752 = VERTEX_POINT('',#69505) ;
#13753 = VERTEX_POINT('',#69507) ;
#13754 = VERTEX_POINT('',#69511) ;
#13755 = VERTEX_POINT('',#69513) ;
#13756 = VERTEX_POINT('',#69517) ;
#13757 = VERTEX_POINT('',#69519) ;
#13758 = VERTEX_POINT('',#69525) ;
#13759 = VERTEX_POINT('',#69526) ;
#13760 = VERTEX_POINT('',#69528) ;
#13761 = VERTEX_POINT('',#69530) ;
#13762 = VERTEX_POINT('',#69534) ;
#13763 = VERTEX_POINT('',#69536) ;
#13764 = VERTEX_POINT('',#69540) ;
#13765 = VERTEX_POINT('',#69542) ;
#13766 = VERTEX_POINT('',#69554) ;
#13767 = VERTEX_POINT('',#69556) ;
#13768 = VERTEX_POINT('',#69558) ;
#13769 = VERTEX_POINT('',#69560) ;
#13770 = VERTEX_POINT('',#69562) ;
#13771 = VERTEX_POINT('',#69564) ;
#13772 = VERTEX_POINT('',#69566) ;
#13773 = VERTEX_POINT('',#69568) ;
#13774 = VERTEX_POINT('',#69570) ;
#13775 = VERTEX_POINT('',#69572) ;
#13776 = VERTEX_POINT('',#69574) ;
#13777 = VERTEX_POINT('',#69576) ;
#13778 = VERTEX_POINT('',#69578) ;
#13779 = VERTEX_POINT('',#69580) ;
#13780 = VERTEX_POINT('',#69582) ;
#13781 = VERTEX_POINT('',#69584) ;
#13782 = VERTEX_POINT('',#69586) ;
#13783 = VERTEX_POINT('',#69588) ;
#13784 = VERTEX_POINT('',#69590) ;
#13785 = VERTEX_POINT('',#69592) ;
#13786 = VERTEX_POINT('',#69594) ;
#13787 = VERTEX_POINT('',#69596) ;
#13788 = VERTEX_POINT('',#69598) ;
#13789 = VERTEX_POINT('',#69600) ;
#13790 = VERTEX_POINT('',#69602) ;
#13791 = VERTEX_POINT('',#69604) ;
#13792 = VERTEX_POINT('',#69606) ;
#13793 = VERTEX_POINT('',#69608) ;
#13794 = VERTEX_POINT('',#69610) ;
#13795 = VERTEX_POINT('',#69612) ;
#13796 = VERTEX_POINT('',#69614) ;
#13797 = VERTEX_POINT('',#69616) ;
#13798 = VERTEX_POINT('',#69618) ;
#13799 = VERTEX_POINT('',#69620) ;
#13800 = VERTEX_POINT('',#69622) ;
#13801 = VERTEX_POINT('',#69624) ;
#13802 = VERTEX_POINT('',#69626) ;
#13803 = VERTEX_POINT('',#69628) ;
#13804 = VERTEX_POINT('',#69630) ;
#13805 = VERTEX_POINT('',#69632) ;
#13806 = VERTEX_POINT('',#69638) ;
#13807 = VERTEX_POINT('',#69640) ;
#13808 = VERTEX_POINT('',#69644) ;
#13809 = VERTEX_POINT('',#69648) ;
#13810 = VERTEX_POINT('',#69649) ;
#13811 = VERTEX_POINT('',#69651) ;
#13812 = VERTEX_POINT('',#69653) ;
#13813 = VERTEX_POINT('',#69656) ;
#13814 = VERTEX_POINT('',#69657) ;
#13815 = VERTEX_POINT('',#69659) ;
#13816 = VERTEX_POINT('',#69661) ;
#13817 = VERTEX_POINT('',#69663) ;
#13818 = VERTEX_POINT('',#69665) ;
#13819 = VERTEX_POINT('',#69667) ;
#13820 = VERTEX_POINT('',#69669) ;
#13821 = VERTEX_POINT('',#69673) ;
#13822 = VERTEX_POINT('',#69675) ;
#13823 = VERTEX_POINT('',#69679) ;
#13824 = VERTEX_POINT('',#69683) ;
#13825 = VERTEX_POINT('',#69684) ;
#13826 = VERTEX_POINT('',#69686) ;
#13827 = VERTEX_POINT('',#69688) ;
#13828 = VERTEX_POINT('',#69691) ;
#13829 = VERTEX_POINT('',#69692) ;
#13830 = VERTEX_POINT('',#69694) ;
#13831 = VERTEX_POINT('',#69696) ;
#13832 = VERTEX_POINT('',#69698) ;
#13833 = VERTEX_POINT('',#69700) ;
#13834 = VERTEX_POINT('',#69702) ;
#13835 = VERTEX_POINT('',#69704) ;
#13836 = VERTEX_POINT('',#69708) ;
#13837 = VERTEX_POINT('',#69710) ;
#13838 = VERTEX_POINT('',#69714) ;
#13839 = VERTEX_POINT('',#69718) ;
#13840 = VERTEX_POINT('',#69719) ;
#13841 = VERTEX_POINT('',#69721) ;
#13842 = VERTEX_POINT('',#69723) ;
#13843 = VERTEX_POINT('',#69726) ;
#13844 = VERTEX_POINT('',#69727) ;
#13845 = VERTEX_POINT('',#69729) ;
#13846 = VERTEX_POINT('',#69731) ;
#13847 = VERTEX_POINT('',#69733) ;
#13848 = VERTEX_POINT('',#69735) ;
#13849 = VERTEX_POINT('',#69737) ;
#13850 = VERTEX_POINT('',#69739) ;
#13851 = VERTEX_POINT('',#69743) ;
#13852 = VERTEX_POINT('',#69745) ;
#13853 = VERTEX_POINT('',#69749) ;
#13854 = VERTEX_POINT('',#69753) ;
#13855 = VERTEX_POINT('',#69754) ;
#13856 = VERTEX_POINT('',#69756) ;
#13857 = VERTEX_POINT('',#69758) ;
#13858 = VERTEX_POINT('',#69761) ;
#13859 = VERTEX_POINT('',#69762) ;
#13860 = VERTEX_POINT('',#69764) ;
#13861 = VERTEX_POINT('',#69766) ;
#13862 = VERTEX_POINT('',#69768) ;
#13863 = VERTEX_POINT('',#69770) ;
#13864 = VERTEX_POINT('',#69772) ;
#13865 = VERTEX_POINT('',#69774) ;
#13866 = VERTEX_POINT('',#69778) ;
#13867 = VERTEX_POINT('',#69780) ;
#13868 = VERTEX_POINT('',#69784) ;
#13869 = VERTEX_POINT('',#69788) ;
#13870 = VERTEX_POINT('',#69789) ;
#13871 = VERTEX_POINT('',#69791) ;
#13872 = VERTEX_POINT('',#69793) ;
#13873 = VERTEX_POINT('',#69796) ;
#13874 = VERTEX_POINT('',#69797) ;
#13875 = VERTEX_POINT('',#69799) ;
#13876 = VERTEX_POINT('',#69801) ;
#13877 = VERTEX_POINT('',#69803) ;
#13878 = VERTEX_POINT('',#69805) ;
#13879 = VERTEX_POINT('',#69807) ;
#13880 = VERTEX_POINT('',#69809) ;
#13881 = VERTEX_POINT('',#69813) ;
#13882 = VERTEX_POINT('',#69815) ;
#13883 = VERTEX_POINT('',#69819) ;
#13884 = VERTEX_POINT('',#69823) ;
#13885 = VERTEX_POINT('',#69824) ;
#13886 = VERTEX_POINT('',#69826) ;
#13887 = VERTEX_POINT('',#69828) ;
#13888 = VERTEX_POINT('',#69831) ;
#13889 = VERTEX_POINT('',#69832) ;
#13890 = VERTEX_POINT('',#69834) ;
#13891 = VERTEX_POINT('',#69836) ;
#13892 = VERTEX_POINT('',#69838) ;
#13893 = VERTEX_POINT('',#69840) ;
#13894 = VERTEX_POINT('',#69842) ;
#13895 = VERTEX_POINT('',#69844) ;
#13896 = VERTEX_POINT('',#69848) ;
#13897 = VERTEX_POINT('',#69850) ;
#13898 = VERTEX_POINT('',#69854) ;
#13899 = VERTEX_POINT('',#69858) ;
#13900 = VERTEX_POINT('',#69859) ;
#13901 = VERTEX_POINT('',#69861) ;
#13902 = VERTEX_POINT('',#69863) ;
#13903 = VERTEX_POINT('',#69866) ;
#13904 = VERTEX_POINT('',#69867) ;
#13905 = VERTEX_POINT('',#69869) ;
#13906 = VERTEX_POINT('',#69871) ;
#13907 = VERTEX_POINT('',#69873) ;
#13908 = VERTEX_POINT('',#69875) ;
#13909 = VERTEX_POINT('',#69877) ;
#13910 = VERTEX_POINT('',#69879) ;
#13911 = VERTEX_POINT('',#69883) ;
#13912 = VERTEX_POINT('',#69885) ;
#13913 = VERTEX_POINT('',#69889) ;
#13914 = VERTEX_POINT('',#69893) ;
#13915 = VERTEX_POINT('',#69894) ;
#13916 = VERTEX_POINT('',#69896) ;
#13917 = VERTEX_POINT('',#69898) ;
#13918 = VERTEX_POINT('',#69901) ;
#13919 = VERTEX_POINT('',#69902) ;
#13920 = VERTEX_POINT('',#69904) ;
#13921 = VERTEX_POINT('',#69906) ;
#13922 = VERTEX_POINT('',#69908) ;
#13923 = VERTEX_POINT('',#69910) ;
#13924 = VERTEX_POINT('',#69912) ;
#13925 = VERTEX_POINT('',#69914) ;
#13926 = VERTEX_POINT('',#69918) ;
#13927 = VERTEX_POINT('',#69920) ;
#13928 = VERTEX_POINT('',#69924) ;
#13929 = VERTEX_POINT('',#69925) ;
#13930 = VERTEX_POINT('',#69927) ;
#13931 = VERTEX_POINT('',#69929) ;
#13932 = VERTEX_POINT('',#69932) ;
#13933 = VERTEX_POINT('',#69933) ;
#13934 = VERTEX_POINT('',#69935) ;
#13935 = VERTEX_POINT('',#69937) ;
#13936 = VERTEX_POINT('',#69939) ;
#13937 = VERTEX_POINT('',#69941) ;
#13938 = VERTEX_POINT('',#69943) ;
#13939 = VERTEX_POINT('',#69945) ;
#13940 = VERTEX_POINT('',#69949) ;
#13941 = VERTEX_POINT('',#69953) ;
#13942 = VERTEX_POINT('',#69956) ;
#13943 = VERTEX_POINT('',#69959) ;
#13944 = VERTEX_POINT('',#69962) ;
#13945 = VERTEX_POINT('',#69965) ;
#13946 = VERTEX_POINT('',#69968) ;
#13947 = VERTEX_POINT('',#69971) ;
#13948 = VERTEX_POINT('',#69974) ;
#13949 = VERTEX_POINT('',#69977) ;
#13950 = VERTEX_POINT('',#69979) ;
#13951 = VERTEX_POINT('',#69983) ;
#13952 = VERTEX_POINT('',#69987) ;
#13953 = VERTEX_POINT('',#69991) ;
#13954 = VERTEX_POINT('',#69995) ;
#13955 = VERTEX_POINT('',#69999) ;
#13956 = VERTEX_POINT('',#70003) ;
#13957 = VERTEX_POINT('',#70009) ;
#13958 = VERTEX_POINT('',#70011) ;
#13959 = VERTEX_POINT('',#70015) ;
#13960 = VERTEX_POINT('',#70017) ;
#13961 = VERTEX_POINT('',#70019) ;
#13962 = VERTEX_POINT('',#70021) ;
#13963 = VERTEX_POINT('',#70023) ;
#13964 = VERTEX_POINT('',#70025) ;
#13965 = VERTEX_POINT('',#70027) ;
#13966 = VERTEX_POINT('',#70031) ;
#13967 = VERTEX_POINT('',#70035) ;
#13968 = VERTEX_POINT('',#70039) ;
#13969 = VERTEX_POINT('',#70041) ;
#13970 = VERTEX_POINT('',#70045) ;
#13971 = VERTEX_POINT('',#70049) ;
#13972 = VERTEX_POINT('',#70053) ;
#13973 = VERTEX_POINT('',#70057) ;
#13974 = VERTEX_POINT('',#70061) ;
#13975 = VERTEX_POINT('',#70065) ;
#13976 = VERTEX_POINT('',#70071) ;
#13977 = VERTEX_POINT('',#70073) ;
#13978 = VERTEX_POINT('',#70077) ;
#13979 = VERTEX_POINT('',#70079) ;
#13980 = VERTEX_POINT('',#70081) ;
#13981 = VERTEX_POINT('',#70083) ;
#13982 = VERTEX_POINT('',#70085) ;
#13983 = VERTEX_POINT('',#70087) ;
#13984 = VERTEX_POINT('',#70089) ;
#13985 = VERTEX_POINT('',#70093) ;
#13986 = VERTEX_POINT('',#70097) ;
#13987 = VERTEX_POINT('',#70101) ;
#13988 = VERTEX_POINT('',#70103) ;
#13989 = VERTEX_POINT('',#70107) ;
#13990 = VERTEX_POINT('',#70111) ;
#13991 = VERTEX_POINT('',#70115) ;
#13992 = VERTEX_POINT('',#70119) ;
#13993 = VERTEX_POINT('',#70123) ;
#13994 = VERTEX_POINT('',#70127) ;
#13995 = VERTEX_POINT('',#70133) ;
#13996 = VERTEX_POINT('',#70135) ;
#13997 = VERTEX_POINT('',#70139) ;
#13998 = VERTEX_POINT('',#70141) ;
#13999 = VERTEX_POINT('',#70143) ;
#14000 = VERTEX_POINT('',#70145) ;
#14001 = VERTEX_POINT('',#70147) ;
#14002 = VERTEX_POINT('',#70149) ;
#14003 = VERTEX_POINT('',#70151) ;
#14004 = VERTEX_POINT('',#70155) ;
#14005 = VERTEX_POINT('',#70159) ;
#14006 = VERTEX_POINT('',#70163) ;
#14007 = VERTEX_POINT('',#70165) ;
#14008 = VERTEX_POINT('',#70169) ;
#14009 = VERTEX_POINT('',#70173) ;
#14010 = VERTEX_POINT('',#70177) ;
#14011 = VERTEX_POINT('',#70181) ;
#14012 = VERTEX_POINT('',#70185) ;
#14013 = VERTEX_POINT('',#70189) ;
#14014 = VERTEX_POINT('',#70195) ;
#14015 = VERTEX_POINT('',#70197) ;
#14016 = VERTEX_POINT('',#70201) ;
#14017 = VERTEX_POINT('',#70203) ;
#14018 = VERTEX_POINT('',#70205) ;
#14019 = VERTEX_POINT('',#70207) ;
#14020 = VERTEX_POINT('',#70209) ;
#14021 = VERTEX_POINT('',#70211) ;
#14022 = VERTEX_POINT('',#70213) ;
#14023 = VERTEX_POINT('',#70217) ;
#14024 = VERTEX_POINT('',#70221) ;
#14025 = VERTEX_POINT('',#70225) ;
#14026 = VERTEX_POINT('',#70227) ;
#14027 = VERTEX_POINT('',#70231) ;
#14028 = VERTEX_POINT('',#70235) ;
#14029 = VERTEX_POINT('',#70239) ;
#14030 = VERTEX_POINT('',#70243) ;
#14031 = VERTEX_POINT('',#70247) ;
#14032 = VERTEX_POINT('',#70251) ;
#14033 = VERTEX_POINT('',#70257) ;
#14034 = VERTEX_POINT('',#70259) ;
#14035 = VERTEX_POINT('',#70263) ;
#14036 = VERTEX_POINT('',#70265) ;
#14037 = VERTEX_POINT('',#70267) ;
#14038 = VERTEX_POINT('',#70269) ;
#14039 = VERTEX_POINT('',#70271) ;
#14040 = VERTEX_POINT('',#70273) ;
#14041 = VERTEX_POINT('',#70275) ;
#14042 = VERTEX_POINT('',#70279) ;
#14043 = VERTEX_POINT('',#70283) ;
#14044 = VERTEX_POINT('',#70287) ;
#14045 = VERTEX_POINT('',#70289) ;
#14046 = VERTEX_POINT('',#70293) ;
#14047 = VERTEX_POINT('',#70297) ;
#14048 = VERTEX_POINT('',#70301) ;
#14049 = VERTEX_POINT('',#70305) ;
#14050 = VERTEX_POINT('',#70309) ;
#14051 = VERTEX_POINT('',#70313) ;
#14052 = VERTEX_POINT('',#70319) ;
#14053 = VERTEX_POINT('',#70321) ;
#14054 = VERTEX_POINT('',#70325) ;
#14055 = VERTEX_POINT('',#70327) ;
#14056 = VERTEX_POINT('',#70329) ;
#14057 = VERTEX_POINT('',#70331) ;
#14058 = VERTEX_POINT('',#70333) ;
#14059 = VERTEX_POINT('',#70335) ;
#14060 = VERTEX_POINT('',#70337) ;
#14061 = VERTEX_POINT('',#70341) ;
#14062 = VERTEX_POINT('',#70345) ;
#14063 = VERTEX_POINT('',#70349) ;
#14064 = VERTEX_POINT('',#70351) ;
#14065 = VERTEX_POINT('',#70355) ;
#14066 = VERTEX_POINT('',#70359) ;
#14067 = VERTEX_POINT('',#70363) ;
#14068 = VERTEX_POINT('',#70367) ;
#14069 = VERTEX_POINT('',#70371) ;
#14070 = VERTEX_POINT('',#70375) ;
#14071 = VERTEX_POINT('',#70381) ;
#14072 = VERTEX_POINT('',#70383) ;
#14073 = VERTEX_POINT('',#70387) ;
#14074 = VERTEX_POINT('',#70389) ;
#14075 = VERTEX_POINT('',#70391) ;
#14076 = VERTEX_POINT('',#70393) ;
#14077 = VERTEX_POINT('',#70395) ;
#14078 = VERTEX_POINT('',#70397) ;
#14079 = VERTEX_POINT('',#70399) ;
#14080 = VERTEX_POINT('',#70403) ;
#14081 = VERTEX_POINT('',#70407) ;
#14082 = VERTEX_POINT('',#70411) ;
#14083 = VERTEX_POINT('',#70413) ;
#14084 = VERTEX_POINT('',#70417) ;
#14085 = VERTEX_POINT('',#70421) ;
#14086 = VERTEX_POINT('',#70425) ;
#14087 = VERTEX_POINT('',#70429) ;
#14088 = VERTEX_POINT('',#70433) ;
#14089 = VERTEX_POINT('',#70437) ;
#14090 = VERTEX_POINT('',#70443) ;
#14091 = VERTEX_POINT('',#70445) ;
#14092 = VERTEX_POINT('',#70449) ;
#14093 = VERTEX_POINT('',#70451) ;
#14094 = VERTEX_POINT('',#70453) ;
#14095 = VERTEX_POINT('',#70455) ;
#14096 = VERTEX_POINT('',#70457) ;
#14097 = VERTEX_POINT('',#70459) ;
#14098 = VERTEX_POINT('',#70461) ;
#14099 = VERTEX_POINT('',#70465) ;
#14100 = VERTEX_POINT('',#70469) ;
#14101 = VERTEX_POINT('',#70473) ;
#14102 = VERTEX_POINT('',#70475) ;
#14103 = VERTEX_POINT('',#70479) ;
#14104 = VERTEX_POINT('',#70483) ;
#14105 = VERTEX_POINT('',#70487) ;
#14106 = VERTEX_POINT('',#70491) ;
#14107 = VERTEX_POINT('',#70495) ;
#14108 = VERTEX_POINT('',#70499) ;
#14109 = VERTEX_POINT('',#70505) ;
#14110 = VERTEX_POINT('',#70507) ;
#14111 = VERTEX_POINT('',#70511) ;
#14112 = VERTEX_POINT('',#70512) ;
#14113 = VERTEX_POINT('',#70514) ;
#14114 = VERTEX_POINT('',#70516) ;
#14115 = VERTEX_POINT('',#70519) ;
#14116 = VERTEX_POINT('',#70521) ;
#14117 = VERTEX_POINT('',#70523) ;
#14118 = VERTEX_POINT('',#70527) ;
#14119 = VERTEX_POINT('',#70531) ;
#14120 = VERTEX_POINT('',#70535) ;
#14121 = VERTEX_POINT('',#70536) ;
#14122 = VERTEX_POINT('',#70538) ;
#14123 = VERTEX_POINT('',#70540) ;
#14124 = VERTEX_POINT('',#70544) ;
#14125 = VERTEX_POINT('',#70545) ;
#14126 = VERTEX_POINT('',#70550) ;
#14127 = VERTEX_POINT('',#70551) ;
#14128 = VERTEX_POINT('',#70556) ;
#14129 = VERTEX_POINT('',#70557) ;
#14130 = VERTEX_POINT('',#70562) ;
#14131 = VERTEX_POINT('',#70563) ;
#14132 = VERTEX_POINT('',#70568) ;
#14133 = VERTEX_POINT('',#70569) ;
#14134 = VERTEX_POINT('',#70574) ;
#14135 = VERTEX_POINT('',#70575) ;
#14136 = VERTEX_POINT('',#70583) ;
#14137 = VERTEX_POINT('',#70585) ;
#14138 = VERTEX_POINT('',#70589) ;
#14139 = VERTEX_POINT('',#70593) ;
#14140 = VERTEX_POINT('',#70597) ;
#14141 = VERTEX_POINT('',#70601) ;
#14142 = VERTEX_POINT('',#70602) ;
#14143 = VERTEX_POINT('',#70604) ;
#14144 = VERTEX_POINT('',#70606) ;
#14145 = VERTEX_POINT('',#70610) ;
#14146 = VERTEX_POINT('',#70611) ;
#14147 = VERTEX_POINT('',#70616) ;
#14148 = VERTEX_POINT('',#70617) ;
#14149 = VERTEX_POINT('',#70622) ;
#14150 = VERTEX_POINT('',#70623) ;
#14151 = VERTEX_POINT('',#70628) ;
#14152 = VERTEX_POINT('',#70629) ;
#14153 = VERTEX_POINT('',#70634) ;
#14154 = VERTEX_POINT('',#70635) ;
#14155 = VERTEX_POINT('',#70640) ;
#14156 = VERTEX_POINT('',#70641) ;
#14157 = VERTEX_POINT('',#70649) ;
#14158 = VERTEX_POINT('',#70651) ;
#14159 = VERTEX_POINT('',#70655) ;
#14160 = VERTEX_POINT('',#70659) ;
#14161 = VERTEX_POINT('',#70663) ;
#14162 = VERTEX_POINT('',#70667) ;
#14163 = VERTEX_POINT('',#70668) ;
#14164 = VERTEX_POINT('',#70670) ;
#14165 = VERTEX_POINT('',#70672) ;
#14166 = VERTEX_POINT('',#70676) ;
#14167 = VERTEX_POINT('',#70677) ;
#14168 = VERTEX_POINT('',#70682) ;
#14169 = VERTEX_POINT('',#70683) ;
#14170 = VERTEX_POINT('',#70688) ;
#14171 = VERTEX_POINT('',#70689) ;
#14172 = VERTEX_POINT('',#70694) ;
#14173 = VERTEX_POINT('',#70695) ;
#14174 = VERTEX_POINT('',#70700) ;
#14175 = VERTEX_POINT('',#70701) ;
#14176 = VERTEX_POINT('',#70706) ;
#14177 = VERTEX_POINT('',#70707) ;
#14178 = VERTEX_POINT('',#70715) ;
#14179 = VERTEX_POINT('',#70717) ;
#14180 = VERTEX_POINT('',#70721) ;
#14181 = VERTEX_POINT('',#70725) ;
#14182 = VERTEX_POINT('',#70729) ;
#14183 = VERTEX_POINT('',#70733) ;
#14184 = VERTEX_POINT('',#70734) ;
#14185 = VERTEX_POINT('',#70736) ;
#14186 = VERTEX_POINT('',#70738) ;
#14187 = VERTEX_POINT('',#70742) ;
#14188 = VERTEX_POINT('',#70743) ;
#14189 = VERTEX_POINT('',#70748) ;
#14190 = VERTEX_POINT('',#70749) ;
#14191 = VERTEX_POINT('',#70754) ;
#14192 = VERTEX_POINT('',#70755) ;
#14193 = VERTEX_POINT('',#70760) ;
#14194 = VERTEX_POINT('',#70761) ;
#14195 = VERTEX_POINT('',#70766) ;
#14196 = VERTEX_POINT('',#70767) ;
#14197 = VERTEX_POINT('',#70772) ;
#14198 = VERTEX_POINT('',#70773) ;
#14199 = VERTEX_POINT('',#70781) ;
#14200 = VERTEX_POINT('',#70783) ;
#14201 = VERTEX_POINT('',#70787) ;
#14202 = VERTEX_POINT('',#70791) ;
#14203 = VERTEX_POINT('',#70795) ;
#14204 = VERTEX_POINT('',#70799) ;
#14205 = VERTEX_POINT('',#70800) ;
#14206 = VERTEX_POINT('',#70802) ;
#14207 = VERTEX_POINT('',#70804) ;
#14208 = VERTEX_POINT('',#70808) ;
#14209 = VERTEX_POINT('',#70809) ;
#14210 = VERTEX_POINT('',#70814) ;
#14211 = VERTEX_POINT('',#70815) ;
#14212 = VERTEX_POINT('',#70820) ;
#14213 = VERTEX_POINT('',#70821) ;
#14214 = VERTEX_POINT('',#70826) ;
#14215 = VERTEX_POINT('',#70827) ;
#14216 = VERTEX_POINT('',#70832) ;
#14217 = VERTEX_POINT('',#70833) ;
#14218 = VERTEX_POINT('',#70838) ;
#14219 = VERTEX_POINT('',#70839) ;
#14220 = VERTEX_POINT('',#70847) ;
#14221 = VERTEX_POINT('',#70849) ;
#14222 = VERTEX_POINT('',#70853) ;
#14223 = VERTEX_POINT('',#70857) ;
#14224 = VERTEX_POINT('',#70861) ;
#14225 = VERTEX_POINT('',#70865) ;
#14226 = VERTEX_POINT('',#70866) ;
#14227 = VERTEX_POINT('',#70868) ;
#14228 = VERTEX_POINT('',#70870) ;
#14229 = VERTEX_POINT('',#70874) ;
#14230 = VERTEX_POINT('',#70875) ;
#14231 = VERTEX_POINT('',#70880) ;
#14232 = VERTEX_POINT('',#70881) ;
#14233 = VERTEX_POINT('',#70886) ;
#14234 = VERTEX_POINT('',#70887) ;
#14235 = VERTEX_POINT('',#70892) ;
#14236 = VERTEX_POINT('',#70893) ;
#14237 = VERTEX_POINT('',#70898) ;
#14238 = VERTEX_POINT('',#70899) ;
#14239 = VERTEX_POINT('',#70904) ;
#14240 = VERTEX_POINT('',#70905) ;
#14241 = VERTEX_POINT('',#70913) ;
#14242 = VERTEX_POINT('',#70915) ;
#14243 = VERTEX_POINT('',#70919) ;
#14244 = VERTEX_POINT('',#70923) ;
#14245 = VERTEX_POINT('',#70927) ;
#14246 = VERTEX_POINT('',#70931) ;
#14247 = VERTEX_POINT('',#70932) ;
#14248 = VERTEX_POINT('',#70934) ;
#14249 = VERTEX_POINT('',#70936) ;
#14250 = VERTEX_POINT('',#70940) ;
#14251 = VERTEX_POINT('',#70941) ;
#14252 = VERTEX_POINT('',#70946) ;
#14253 = VERTEX_POINT('',#70947) ;
#14254 = VERTEX_POINT('',#70952) ;
#14255 = VERTEX_POINT('',#70953) ;
#14256 = VERTEX_POINT('',#70958) ;
#14257 = VERTEX_POINT('',#70959) ;
#14258 = VERTEX_POINT('',#70964) ;
#14259 = VERTEX_POINT('',#70965) ;
#14260 = VERTEX_POINT('',#70970) ;
#14261 = VERTEX_POINT('',#70971) ;
#14262 = VERTEX_POINT('',#70979) ;
#14263 = VERTEX_POINT('',#70981) ;
#14264 = VERTEX_POINT('',#70985) ;
#14265 = VERTEX_POINT('',#70989) ;
#14266 = VERTEX_POINT('',#70993) ;
#14267 = VERTEX_POINT('',#70997) ;
#14268 = VERTEX_POINT('',#70998) ;
#14269 = VERTEX_POINT('',#71000) ;
#14270 = VERTEX_POINT('',#71002) ;
#14271 = VERTEX_POINT('',#71006) ;
#14272 = VERTEX_POINT('',#71007) ;
#14273 = VERTEX_POINT('',#71012) ;
#14274 = VERTEX_POINT('',#71013) ;
#14275 = VERTEX_POINT('',#71018) ;
#14276 = VERTEX_POINT('',#71019) ;
#14277 = VERTEX_POINT('',#71024) ;
#14278 = VERTEX_POINT('',#71025) ;
#14279 = VERTEX_POINT('',#71030) ;
#14280 = VERTEX_POINT('',#71031) ;
#14281 = VERTEX_POINT('',#71036) ;
#14282 = VERTEX_POINT('',#71037) ;
#14283 = VERTEX_POINT('',#71045) ;
#14284 = VERTEX_POINT('',#71047) ;
#14285 = VERTEX_POINT('',#71051) ;
#14286 = VERTEX_POINT('',#71055) ;
#14287 = VERTEX_POINT('',#71059) ;
#14288 = VERTEX_POINT('',#71063) ;
#14289 = VERTEX_POINT('',#71064) ;
#14290 = VERTEX_POINT('',#71066) ;
#14291 = VERTEX_POINT('',#71068) ;
#14292 = VERTEX_POINT('',#71072) ;
#14293 = VERTEX_POINT('',#71073) ;
#14294 = VERTEX_POINT('',#71078) ;
#14295 = VERTEX_POINT('',#71079) ;
#14296 = VERTEX_POINT('',#71084) ;
#14297 = VERTEX_POINT('',#71085) ;
#14298 = VERTEX_POINT('',#71090) ;
#14299 = VERTEX_POINT('',#71091) ;
#14300 = VERTEX_POINT('',#71096) ;
#14301 = VERTEX_POINT('',#71101) ;
#14302 = VERTEX_POINT('',#71108) ;
#14303 = VERTEX_POINT('',#71110) ;
#14304 = VERTEX_POINT('',#71114) ;
#14305 = VERTEX_POINT('',#71116) ;
#14306 = VERTEX_POINT('',#71119) ;
#14307 = VERTEX_POINT('',#71121) ;
#14308 = VERTEX_POINT('',#71123) ;
#14309 = VERTEX_POINT('',#71127) ;
#14310 = VERTEX_POINT('',#71131) ;
#14311 = VERTEX_POINT('',#71135) ;
#14312 = VERTEX_POINT('',#71136) ;
#14313 = VERTEX_POINT('',#71138) ;
#14314 = VERTEX_POINT('',#71140) ;
#14315 = VERTEX_POINT('',#71144) ;
#14316 = VERTEX_POINT('',#71145) ;
#14317 = VERTEX_POINT('',#71150) ;
#14318 = VERTEX_POINT('',#71151) ;
#14319 = VERTEX_POINT('',#71156) ;
#14320 = VERTEX_POINT('',#71157) ;
#14321 = VERTEX_POINT('',#71162) ;
#14322 = VERTEX_POINT('',#71163) ;
#14323 = VERTEX_POINT('',#71168) ;
#14324 = VERTEX_POINT('',#71173) ;
#14325 = VERTEX_POINT('',#71180) ;
#14326 = VERTEX_POINT('',#71182) ;
#14327 = VERTEX_POINT('',#71186) ;
#14328 = VERTEX_POINT('',#71188) ;
#14329 = VERTEX_POINT('',#71191) ;
#14330 = VERTEX_POINT('',#71193) ;
#14331 = VERTEX_POINT('',#71195) ;
#14332 = VERTEX_POINT('',#71199) ;
#14333 = VERTEX_POINT('',#71203) ;
#14334 = VERTEX_POINT('',#71207) ;
#14335 = VERTEX_POINT('',#71208) ;
#14336 = VERTEX_POINT('',#71210) ;
#14337 = VERTEX_POINT('',#71212) ;
#14338 = VERTEX_POINT('',#71216) ;
#14339 = VERTEX_POINT('',#71217) ;
#14340 = VERTEX_POINT('',#71222) ;
#14341 = VERTEX_POINT('',#71223) ;
#14342 = VERTEX_POINT('',#71228) ;
#14343 = VERTEX_POINT('',#71229) ;
#14344 = VERTEX_POINT('',#71234) ;
#14345 = VERTEX_POINT('',#71235) ;
#14346 = VERTEX_POINT('',#71240) ;
#14347 = VERTEX_POINT('',#71245) ;
#14348 = VERTEX_POINT('',#71252) ;
#14349 = VERTEX_POINT('',#71254) ;
#14350 = VERTEX_POINT('',#71258) ;
#14351 = VERTEX_POINT('',#71260) ;
#14352 = VERTEX_POINT('',#71263) ;
#14353 = VERTEX_POINT('',#71265) ;
#14354 = VERTEX_POINT('',#71267) ;
#14355 = VERTEX_POINT('',#71271) ;
#14356 = VERTEX_POINT('',#71275) ;
#14357 = VERTEX_POINT('',#71279) ;
#14358 = VERTEX_POINT('',#71280) ;
#14359 = VERTEX_POINT('',#71282) ;
#14360 = VERTEX_POINT('',#71284) ;
#14361 = VERTEX_POINT('',#71288) ;
#14362 = VERTEX_POINT('',#71289) ;
#14363 = VERTEX_POINT('',#71294) ;
#14364 = VERTEX_POINT('',#71295) ;
#14365 = VERTEX_POINT('',#71300) ;
#14366 = VERTEX_POINT('',#71301) ;
#14367 = VERTEX_POINT('',#71306) ;
#14368 = VERTEX_POINT('',#71307) ;
#14369 = VERTEX_POINT('',#71312) ;
#14370 = VERTEX_POINT('',#71317) ;
#14371 = VERTEX_POINT('',#71324) ;
#14372 = VERTEX_POINT('',#71326) ;
#14373 = VERTEX_POINT('',#71330) ;
#14374 = VERTEX_POINT('',#71332) ;
#14375 = VERTEX_POINT('',#71335) ;
#14376 = VERTEX_POINT('',#71337) ;
#14377 = VERTEX_POINT('',#71339) ;
#14378 = VERTEX_POINT('',#71343) ;
#14379 = VERTEX_POINT('',#71347) ;
#14380 = VERTEX_POINT('',#71351) ;
#14381 = VERTEX_POINT('',#71352) ;
#14382 = VERTEX_POINT('',#71354) ;
#14383 = VERTEX_POINT('',#71356) ;
#14384 = VERTEX_POINT('',#71360) ;
#14385 = VERTEX_POINT('',#71361) ;
#14386 = VERTEX_POINT('',#71366) ;
#14387 = VERTEX_POINT('',#71367) ;
#14388 = VERTEX_POINT('',#71372) ;
#14389 = VERTEX_POINT('',#71373) ;
#14390 = VERTEX_POINT('',#71378) ;
#14391 = VERTEX_POINT('',#71379) ;
#14392 = VERTEX_POINT('',#71384) ;
#14393 = VERTEX_POINT('',#71389) ;
#14394 = VERTEX_POINT('',#71396) ;
#14395 = VERTEX_POINT('',#71398) ;
#14396 = VERTEX_POINT('',#71402) ;
#14397 = VERTEX_POINT('',#71404) ;
#14398 = VERTEX_POINT('',#71407) ;
#14399 = VERTEX_POINT('',#71409) ;
#14400 = VERTEX_POINT('',#71411) ;
#14401 = VERTEX_POINT('',#71415) ;
#14402 = VERTEX_POINT('',#71419) ;
#14403 = VERTEX_POINT('',#71423) ;
#14404 = VERTEX_POINT('',#71424) ;
#14405 = VERTEX_POINT('',#71426) ;
#14406 = VERTEX_POINT('',#71428) ;
#14407 = VERTEX_POINT('',#71432) ;
#14408 = VERTEX_POINT('',#71433) ;
#14409 = VERTEX_POINT('',#71438) ;
#14410 = VERTEX_POINT('',#71439) ;
#14411 = VERTEX_POINT('',#71444) ;
#14412 = VERTEX_POINT('',#71445) ;
#14413 = VERTEX_POINT('',#71450) ;
#14414 = VERTEX_POINT('',#71451) ;
#14415 = VERTEX_POINT('',#71456) ;
#14416 = VERTEX_POINT('',#71461) ;
#14417 = VERTEX_POINT('',#71468) ;
#14418 = VERTEX_POINT('',#71470) ;
#14419 = VERTEX_POINT('',#71474) ;
#14420 = VERTEX_POINT('',#71476) ;
#14421 = VERTEX_POINT('',#71479) ;
#14422 = VERTEX_POINT('',#71481) ;
#14423 = VERTEX_POINT('',#71483) ;
#14424 = VERTEX_POINT('',#71487) ;
#14425 = VERTEX_POINT('',#71491) ;
#14426 = VERTEX_POINT('',#71495) ;
#14427 = VERTEX_POINT('',#71496) ;
#14428 = VERTEX_POINT('',#71498) ;
#14429 = VERTEX_POINT('',#71500) ;
#14430 = VERTEX_POINT('',#71504) ;
#14431 = VERTEX_POINT('',#71505) ;
#14432 = VERTEX_POINT('',#71510) ;
#14433 = VERTEX_POINT('',#71511) ;
#14434 = VERTEX_POINT('',#71516) ;
#14435 = VERTEX_POINT('',#71517) ;
#14436 = VERTEX_POINT('',#71522) ;
#14437 = VERTEX_POINT('',#71523) ;
#14438 = VERTEX_POINT('',#71528) ;
#14439 = VERTEX_POINT('',#71533) ;
#14440 = VERTEX_POINT('',#71540) ;
#14441 = VERTEX_POINT('',#71542) ;
#14442 = VERTEX_POINT('',#71546) ;
#14443 = VERTEX_POINT('',#71548) ;
#14444 = VERTEX_POINT('',#71551) ;
#14445 = VERTEX_POINT('',#71553) ;
#14446 = VERTEX_POINT('',#71555) ;
#14447 = VERTEX_POINT('',#71559) ;
#14448 = VERTEX_POINT('',#71563) ;
#14449 = VERTEX_POINT('',#71567) ;
#14450 = VERTEX_POINT('',#71568) ;
#14451 = VERTEX_POINT('',#71570) ;
#14452 = VERTEX_POINT('',#71572) ;
#14453 = VERTEX_POINT('',#71576) ;
#14454 = VERTEX_POINT('',#71577) ;
#14455 = VERTEX_POINT('',#71582) ;
#14456 = VERTEX_POINT('',#71583) ;
#14457 = VERTEX_POINT('',#71588) ;
#14458 = VERTEX_POINT('',#71589) ;
#14459 = VERTEX_POINT('',#71594) ;
#14460 = VERTEX_POINT('',#71595) ;
#14461 = VERTEX_POINT('',#71600) ;
#14462 = VERTEX_POINT('',#71605) ;
#14463 = VERTEX_POINT('',#71612) ;
#14464 = VERTEX_POINT('',#71614) ;
#14465 = VERTEX_POINT('',#71618) ;
#14466 = VERTEX_POINT('',#71620) ;
#14467 = VERTEX_POINT('',#71623) ;
#14468 = VERTEX_POINT('',#71625) ;
#14469 = VERTEX_POINT('',#71627) ;
#14470 = VERTEX_POINT('',#71631) ;
#14471 = VERTEX_POINT('',#71635) ;
#14472 = VERTEX_POINT('',#71639) ;
#14473 = VERTEX_POINT('',#71640) ;
#14474 = VERTEX_POINT('',#71642) ;
#14475 = VERTEX_POINT('',#71644) ;
#14476 = VERTEX_POINT('',#71648) ;
#14477 = VERTEX_POINT('',#71649) ;
#14478 = VERTEX_POINT('',#71654) ;
#14479 = VERTEX_POINT('',#71655) ;
#14480 = VERTEX_POINT('',#71660) ;
#14481 = VERTEX_POINT('',#71661) ;
#14482 = VERTEX_POINT('',#71666) ;
#14483 = VERTEX_POINT('',#71667) ;
#14484 = VERTEX_POINT('',#71672) ;
#14485 = VERTEX_POINT('',#71673) ;
#14486 = VERTEX_POINT('',#71678) ;
#14487 = VERTEX_POINT('',#71679) ;
#14488 = VERTEX_POINT('',#71687) ;
#14489 = VERTEX_POINT('',#71689) ;
#14490 = VERTEX_POINT('',#71693) ;
#14491 = VERTEX_POINT('',#71697) ;
#14492 = VERTEX_POINT('',#71701) ;
#14493 = VERTEX_POINT('',#71705) ;
#14494 = VERTEX_POINT('',#71706) ;
#14495 = VERTEX_POINT('',#71708) ;
#14496 = VERTEX_POINT('',#71710) ;
#14497 = VERTEX_POINT('',#71713) ;
#14498 = VERTEX_POINT('',#71714) ;
#14499 = VERTEX_POINT('',#71716) ;
#14500 = VERTEX_POINT('',#71718) ;
#14501 = VERTEX_POINT('',#71720) ;
#14502 = VERTEX_POINT('',#71722) ;
#14503 = VERTEX_POINT('',#71724) ;
#14504 = VERTEX_POINT('',#71726) ;
#14505 = VERTEX_POINT('',#71729) ;
#14506 = VERTEX_POINT('',#71732) ;
#14507 = VERTEX_POINT('',#71734) ;
#14508 = VERTEX_POINT('',#71738) ;
#14509 = VERTEX_POINT('',#71742) ;
#14510 = VERTEX_POINT('',#71746) ;
#14511 = VERTEX_POINT('',#71750) ;
#14512 = VERTEX_POINT('',#71761) ;
#14513 = VERTEX_POINT('',#71763) ;
#14514 = VERTEX_POINT('',#71767) ;
#14515 = VERTEX_POINT('',#71769) ;
#14516 = VERTEX_POINT('',#71771) ;
#14517 = VERTEX_POINT('',#71774) ;
#14518 = VERTEX_POINT('',#71776) ;
#14519 = VERTEX_POINT('',#71780) ;
#14520 = VERTEX_POINT('',#71784) ;
#14521 = VERTEX_POINT('',#71788) ;
#14522 = VERTEX_POINT('',#71796) ;
#14523 = VERTEX_POINT('',#71800) ;
#14524 = VERTEX_POINT('',#71804) ;
#14525 = VERTEX_POINT('',#71810) ;
#14526 = VERTEX_POINT('',#71815) ;
#14527 = VERTEX_POINT('',#71817) ;
#14528 = VERTEX_POINT('',#71821) ;
#14529 = VERTEX_POINT('',#71825) ;
#14530 = VERTEX_POINT('',#71829) ;
#14531 = VERTEX_POINT('',#71833) ;
#14532 = VERTEX_POINT('',#71834) ;
#14533 = VERTEX_POINT('',#71844) ;
#14534 = VERTEX_POINT('',#71854) ;
#14535 = VERTEX_POINT('',#71871) ;
#14536 = VERTEX_POINT('',#71872) ;
#14537 = VERTEX_POINT('',#71874) ;
#14538 = VERTEX_POINT('',#71876) ;
#14539 = VERTEX_POINT('',#71898) ;
#14540 = VERTEX_POINT('',#71899) ;
#14541 = VERTEX_POINT('',#71902) ;
#14542 = VERTEX_POINT('',#71906) ;
#14543 = VERTEX_POINT('',#71910) ;
#14544 = VERTEX_POINT('',#71914) ;
#14545 = VERTEX_POINT('',#71918) ;
#14546 = VERTEX_POINT('',#71919) ;
#14547 = VERTEX_POINT('',#71929) ;
#14548 = VERTEX_POINT('',#71939) ;
#14549 = VERTEX_POINT('',#71958) ;
#14550 = VERTEX_POINT('',#71959) ;
#14551 = VERTEX_POINT('',#71961) ;
#14552 = VERTEX_POINT('',#71963) ;
#14553 = VERTEX_POINT('',#71967) ;
#14554 = VERTEX_POINT('',#71969) ;
#14555 = VERTEX_POINT('',#71973) ;
#14556 = VERTEX_POINT('',#71992) ;
#14557 = VERTEX_POINT('',#71993) ;
#14558 = VERTEX_POINT('',#71996) ;
#14559 = VERTEX_POINT('',#72000) ;
#14560 = VERTEX_POINT('',#72004) ;
#14561 = VERTEX_POINT('',#72008) ;
#14562 = VERTEX_POINT('',#72012) ;
#14563 = VERTEX_POINT('',#72013) ;
#14564 = VERTEX_POINT('',#72023) ;
#14565 = VERTEX_POINT('',#72033) ;
#14566 = VERTEX_POINT('',#72052) ;
#14567 = VERTEX_POINT('',#72053) ;
#14568 = VERTEX_POINT('',#72055) ;
#14569 = VERTEX_POINT('',#72057) ;
#14570 = VERTEX_POINT('',#72061) ;
#14571 = VERTEX_POINT('',#72063) ;
#14572 = VERTEX_POINT('',#72067) ;
#14573 = VERTEX_POINT('',#72086) ;
#14574 = VERTEX_POINT('',#72087) ;
#14575 = VERTEX_POINT('',#72090) ;
#14576 = VERTEX_POINT('',#72094) ;
#14577 = VERTEX_POINT('',#72098) ;
#14578 = VERTEX_POINT('',#72102) ;
#14579 = VERTEX_POINT('',#72106) ;
#14580 = VERTEX_POINT('',#72107) ;
#14581 = VERTEX_POINT('',#72117) ;
#14582 = VERTEX_POINT('',#72127) ;
#14583 = VERTEX_POINT('',#72146) ;
#14584 = VERTEX_POINT('',#72147) ;
#14585 = VERTEX_POINT('',#72149) ;
#14586 = VERTEX_POINT('',#72151) ;
#14587 = VERTEX_POINT('',#72155) ;
#14588 = VERTEX_POINT('',#72157) ;
#14589 = VERTEX_POINT('',#72161) ;
#14590 = VERTEX_POINT('',#72180) ;
#14591 = VERTEX_POINT('',#72181) ;
#14592 = VERTEX_POINT('',#72184) ;
#14593 = VERTEX_POINT('',#72188) ;
#14594 = VERTEX_POINT('',#72192) ;
#14595 = VERTEX_POINT('',#72196) ;
#14596 = VERTEX_POINT('',#72200) ;
#14597 = VERTEX_POINT('',#72201) ;
#14598 = VERTEX_POINT('',#72211) ;
#14599 = VERTEX_POINT('',#72221) ;
#14600 = VERTEX_POINT('',#72240) ;
#14601 = VERTEX_POINT('',#72241) ;
#14602 = VERTEX_POINT('',#72243) ;
#14603 = VERTEX_POINT('',#72245) ;
#14604 = VERTEX_POINT('',#72249) ;
#14605 = VERTEX_POINT('',#72251) ;
#14606 = VERTEX_POINT('',#72255) ;
#14607 = VERTEX_POINT('',#72274) ;
#14608 = VERTEX_POINT('',#72275) ;
#14609 = VERTEX_POINT('',#72278) ;
#14610 = VERTEX_POINT('',#72282) ;
#14611 = VERTEX_POINT('',#72286) ;
#14612 = VERTEX_POINT('',#72290) ;
#14613 = VERTEX_POINT('',#72294) ;
#14614 = VERTEX_POINT('',#72295) ;
#14615 = VERTEX_POINT('',#72305) ;
#14616 = VERTEX_POINT('',#72315) ;
#14617 = VERTEX_POINT('',#72334) ;
#14618 = VERTEX_POINT('',#72335) ;
#14619 = VERTEX_POINT('',#72337) ;
#14620 = VERTEX_POINT('',#72339) ;
#14621 = VERTEX_POINT('',#72343) ;
#14622 = VERTEX_POINT('',#72345) ;
#14623 = VERTEX_POINT('',#72349) ;
#14624 = VERTEX_POINT('',#72368) ;
#14625 = VERTEX_POINT('',#72369) ;
#14626 = VERTEX_POINT('',#72372) ;
#14627 = VERTEX_POINT('',#72376) ;
#14628 = VERTEX_POINT('',#72380) ;
#14629 = VERTEX_POINT('',#72384) ;
#14630 = VERTEX_POINT('',#72388) ;
#14631 = VERTEX_POINT('',#72389) ;
#14632 = VERTEX_POINT('',#72399) ;
#14633 = VERTEX_POINT('',#72409) ;
#14634 = VERTEX_POINT('',#72428) ;
#14635 = VERTEX_POINT('',#72429) ;
#14636 = VERTEX_POINT('',#72431) ;
#14637 = VERTEX_POINT('',#72433) ;
#14638 = VERTEX_POINT('',#72437) ;
#14639 = VERTEX_POINT('',#72439) ;
#14640 = VERTEX_POINT('',#72443) ;
#14641 = VERTEX_POINT('',#72462) ;
#14642 = VERTEX_POINT('',#72463) ;
#14643 = VERTEX_POINT('',#72466) ;
#14644 = VERTEX_POINT('',#72470) ;
#14645 = VERTEX_POINT('',#72474) ;
#14646 = VERTEX_POINT('',#72478) ;
#14647 = VERTEX_POINT('',#72482) ;
#14648 = VERTEX_POINT('',#72483) ;
#14649 = VERTEX_POINT('',#72493) ;
#14650 = VERTEX_POINT('',#72503) ;
#14651 = VERTEX_POINT('',#72522) ;
#14652 = VERTEX_POINT('',#72523) ;
#14653 = VERTEX_POINT('',#72525) ;
#14654 = VERTEX_POINT('',#72527) ;
#14655 = VERTEX_POINT('',#72531) ;
#14656 = VERTEX_POINT('',#72533) ;
#14657 = VERTEX_POINT('',#72537) ;
#14658 = VERTEX_POINT('',#72556) ;
#14659 = VERTEX_POINT('',#72557) ;
#14660 = VERTEX_POINT('',#72560) ;
#14661 = VERTEX_POINT('',#72564) ;
#14662 = VERTEX_POINT('',#72568) ;
#14663 = VERTEX_POINT('',#72572) ;
#14664 = VERTEX_POINT('',#72576) ;
#14665 = VERTEX_POINT('',#72577) ;
#14666 = VERTEX_POINT('',#72587) ;
#14667 = VERTEX_POINT('',#72597) ;
#14668 = VERTEX_POINT('',#72616) ;
#14669 = VERTEX_POINT('',#72617) ;
#14670 = VERTEX_POINT('',#72619) ;
#14671 = VERTEX_POINT('',#72621) ;
#14672 = VERTEX_POINT('',#72625) ;
#14673 = VERTEX_POINT('',#72627) ;
#14674 = VERTEX_POINT('',#72631) ;
#14675 = VERTEX_POINT('',#72711) ;
#14676 = VERTEX_POINT('',#72712) ;
#14677 = VERTEX_POINT('',#72714) ;
#14678 = VERTEX_POINT('',#72716) ;
#14679 = VERTEX_POINT('',#72718) ;
#14680 = VERTEX_POINT('',#72720) ;
#14681 = VERTEX_POINT('',#72722) ;
#14682 = VERTEX_POINT('',#72724) ;
#14683 = VERTEX_POINT('',#72726) ;
#14684 = VERTEX_POINT('',#72728) ;
#14685 = VERTEX_POINT('',#72730) ;
#14686 = VERTEX_POINT('',#72732) ;
#14687 = VERTEX_POINT('',#72734) ;
#14688 = VERTEX_POINT('',#72736) ;
#14689 = VERTEX_POINT('',#72738) ;
#14690 = VERTEX_POINT('',#72740) ;
#14691 = VERTEX_POINT('',#72742) ;
#14692 = VERTEX_POINT('',#72744) ;
#14693 = VERTEX_POINT('',#72746) ;
#14694 = VERTEX_POINT('',#72748) ;
#14695 = VERTEX_POINT('',#72750) ;
#14696 = VERTEX_POINT('',#72752) ;
#14697 = VERTEX_POINT('',#72754) ;
#14698 = VERTEX_POINT('',#72756) ;
#14699 = VERTEX_POINT('',#72758) ;
#14700 = VERTEX_POINT('',#72760) ;
#14701 = VERTEX_POINT('',#72762) ;
#14702 = VERTEX_POINT('',#72764) ;
#14703 = VERTEX_POINT('',#72766) ;
#14704 = VERTEX_POINT('',#72768) ;
#14705 = VERTEX_POINT('',#72770) ;
#14706 = VERTEX_POINT('',#72772) ;
#14707 = VERTEX_POINT('',#72774) ;
#14708 = VERTEX_POINT('',#72776) ;
#14709 = VERTEX_POINT('',#72778) ;
#14710 = VERTEX_POINT('',#72780) ;
#14711 = VERTEX_POINT('',#72782) ;
#14712 = VERTEX_POINT('',#72784) ;
#14713 = VERTEX_POINT('',#72786) ;
#14714 = VERTEX_POINT('',#72788) ;
#14715 = VERTEX_POINT('',#72792) ;
#14716 = VERTEX_POINT('',#72794) ;
#14717 = VERTEX_POINT('',#72799) ;
#14718 = VERTEX_POINT('',#72803) ;
#14719 = VERTEX_POINT('',#72804) ;
#14720 = VERTEX_POINT('',#72809) ;
#14721 = VERTEX_POINT('',#72811) ;
#14722 = VERTEX_POINT('',#72815) ;
#14723 = VERTEX_POINT('',#72817) ;
#14724 = VERTEX_POINT('',#72821) ;
#14725 = VERTEX_POINT('',#72822) ;
#14726 = VERTEX_POINT('',#72827) ;
#14727 = VERTEX_POINT('',#72828) ;
#14728 = VERTEX_POINT('',#72833) ;
#14729 = VERTEX_POINT('',#72834) ;
#14730 = VERTEX_POINT('',#72839) ;
#14731 = VERTEX_POINT('',#72841) ;
#14732 = VERTEX_POINT('',#72845) ;
#14733 = VERTEX_POINT('',#72846) ;
#14734 = VERTEX_POINT('',#72851) ;
#14735 = VERTEX_POINT('',#72853) ;
#14736 = VERTEX_POINT('',#72858) ;
#14737 = VERTEX_POINT('',#72864) ;
#14738 = VERTEX_POINT('',#72865) ;
#14739 = VERTEX_POINT('',#72867) ;
#14740 = VERTEX_POINT('',#72869) ;
#14741 = VERTEX_POINT('',#72873) ;
#14742 = VERTEX_POINT('',#72874) ;
#14743 = VERTEX_POINT('',#72876) ;
#14744 = VERTEX_POINT('',#72878) ;
#14745 = VERTEX_POINT('',#72882) ;
#14746 = VERTEX_POINT('',#72883) ;
#14747 = VERTEX_POINT('',#72885) ;
#14748 = VERTEX_POINT('',#72887) ;
#14749 = VERTEX_POINT('',#72891) ;
#14750 = VERTEX_POINT('',#72892) ;
#14751 = VERTEX_POINT('',#72894) ;
#14752 = VERTEX_POINT('',#72896) ;
#14753 = VERTEX_POINT('',#72900) ;
#14754 = VERTEX_POINT('',#72901) ;
#14755 = VERTEX_POINT('',#72903) ;
#14756 = VERTEX_POINT('',#72905) ;
#14757 = VERTEX_POINT('',#72909) ;
#14758 = VERTEX_POINT('',#72910) ;
#14759 = VERTEX_POINT('',#72912) ;
#14760 = VERTEX_POINT('',#72914) ;
#14761 = VERTEX_POINT('',#72918) ;
#14762 = VERTEX_POINT('',#72919) ;
#14763 = VERTEX_POINT('',#72921) ;
#14764 = VERTEX_POINT('',#72923) ;
#14765 = VERTEX_POINT('',#72927) ;
#14766 = VERTEX_POINT('',#72928) ;
#14767 = VERTEX_POINT('',#72930) ;
#14768 = VERTEX_POINT('',#72932) ;
#14769 = VERTEX_POINT('',#72940) ;
#14770 = VERTEX_POINT('',#72944) ;
#14771 = VERTEX_POINT('',#72950) ;
#14772 = VERTEX_POINT('',#72954) ;
#14773 = VERTEX_POINT('',#72960) ;
#14774 = VERTEX_POINT('',#72964) ;
#14775 = VERTEX_POINT('',#72970) ;
#14776 = VERTEX_POINT('',#72974) ;
#14777 = VERTEX_POINT('',#72980) ;
#14778 = VERTEX_POINT('',#72984) ;
#14779 = VERTEX_POINT('',#72990) ;
#14780 = VERTEX_POINT('',#72994) ;
#14781 = VERTEX_POINT('',#73000) ;
#14782 = VERTEX_POINT('',#73004) ;
#14783 = VERTEX_POINT('',#73010) ;
#14784 = VERTEX_POINT('',#73014) ;
#14785 = VERTEX_POINT('',#73038) ;
#14786 = VERTEX_POINT('',#73041) ;
#14787 = VERTEX_POINT('',#73042) ;
#14788 = VERTEX_POINT('',#73047) ;
#14789 = VERTEX_POINT('',#73056) ;
#14790 = VERTEX_POINT('',#73059) ;
#14791 = VERTEX_POINT('',#73060) ;
#14792 = VERTEX_POINT('',#73065) ;
#14793 = VERTEX_POINT('',#73074) ;
#14794 = VERTEX_POINT('',#73077) ;
#14795 = VERTEX_POINT('',#73078) ;
#14796 = VERTEX_POINT('',#73083) ;
#14797 = VERTEX_POINT('',#73092) ;
#14798 = VERTEX_POINT('',#73095) ;
#14799 = VERTEX_POINT('',#73096) ;
#14800 = VERTEX_POINT('',#73101) ;
#14801 = VERTEX_POINT('',#73110) ;
#14802 = VERTEX_POINT('',#73113) ;
#14803 = VERTEX_POINT('',#73114) ;
#14804 = VERTEX_POINT('',#73119) ;
#14805 = VERTEX_POINT('',#73128) ;
#14806 = VERTEX_POINT('',#73131) ;
#14807 = VERTEX_POINT('',#73132) ;
#14808 = VERTEX_POINT('',#73137) ;
#14809 = VERTEX_POINT('',#73146) ;
#14810 = VERTEX_POINT('',#73149) ;
#14811 = VERTEX_POINT('',#73150) ;
#14812 = VERTEX_POINT('',#73155) ;
#14813 = VERTEX_POINT('',#73164) ;
#14814 = VERTEX_POINT('',#73167) ;
#14815 = VERTEX_POINT('',#73168) ;
#14816 = VERTEX_POINT('',#73173) ;
#14817 = VERTEX_POINT('',#73182) ;
#14818 = VERTEX_POINT('',#73183) ;
#14819 = VERTEX_POINT('',#73188) ;
#14820 = VERTEX_POINT('',#73263) ;
#14821 = VERTEX_POINT('',#73264) ;
#14822 = VERTEX_POINT('',#73266) ;
#14823 = VERTEX_POINT('',#73297) ;
#14824 = VERTEX_POINT('',#73334) ;
#14825 = VERTEX_POINT('',#73335) ;
#14826 = VERTEX_POINT('',#73410) ;
#14827 = VERTEX_POINT('',#73411) ;
#14828 = VERTEX_POINT('',#73486) ;
#14829 = VERTEX_POINT('',#73487) ;
#14830 = VERTEX_POINT('',#73562) ;
#14831 = VERTEX_POINT('',#73563) ;
#14832 = VERTEX_POINT('',#73638) ;
#14833 = VERTEX_POINT('',#73639) ;
#14834 = VERTEX_POINT('',#73714) ;
#14835 = VERTEX_POINT('',#73715) ;
#14836 = VERTEX_POINT('',#73790) ;
#14837 = VERTEX_POINT('',#73791) ;
#14838 = VERTEX_POINT('',#73793) ;
#14839 = VERTEX_POINT('',#73866) ;
#14840 = VERTEX_POINT('',#73867) ;
#14841 = VERTEX_POINT('',#73869) ;
#14842 = VERTEX_POINT('',#73894) ;
#14843 = VERTEX_POINT('',#73917) ;
#14844 = VERTEX_POINT('',#73918) ;
#14845 = VERTEX_POINT('',#73993) ;
#14846 = VERTEX_POINT('',#73994) ;
#14847 = VERTEX_POINT('',#74069) ;
#14848 = VERTEX_POINT('',#74070) ;
#14849 = VERTEX_POINT('',#74145) ;
#14850 = VERTEX_POINT('',#74146) ;
#14851 = VERTEX_POINT('',#74221) ;
#14852 = VERTEX_POINT('',#74222) ;
#14853 = VERTEX_POINT('',#74297) ;
#14854 = VERTEX_POINT('',#74298) ;
#14855 = VERTEX_POINT('',#74373) ;
#14856 = VERTEX_POINT('',#74398) ;
#14857 = VERTEX_POINT('',#74400) ;
#14858 = VERTEX_POINT('',#74432) ;
#14859 = VERTEX_POINT('',#74462) ;
#14860 = VERTEX_POINT('',#74463) ;
#14861 = VERTEX_POINT('',#74465) ;
#14862 = VERTEX_POINT('',#74498) ;
#14863 = VERTEX_POINT('',#74503) ;
#14864 = VERTEX_POINT('',#74538) ;
#14865 = VERTEX_POINT('',#74539) ;
#14866 = VERTEX_POINT('',#74571) ;
#14867 = VERTEX_POINT('',#74572) ;
#14868 = VERTEX_POINT('',#74648) ;
#14869 = VERTEX_POINT('',#74649) ;
#14870 = VERTEX_POINT('',#74651) ;
#14871 = VERTEX_POINT('',#74681) ;
#14872 = VERTEX_POINT('',#74682) ;
#14873 = VERTEX_POINT('',#74771) ;
#14874 = VERTEX_POINT('',#74775) ;
#14875 = VERTEX_POINT('',#74776) ;
#14876 = VERTEX_POINT('',#74778) ;
#14877 = VERTEX_POINT('',#74785) ;
#14878 = VERTEX_POINT('',#74787) ;
#14879 = VERTEX_POINT('',#74789) ;
#14880 = VERTEX_POINT('',#74791) ;
#14881 = VERTEX_POINT('',#74799) ;
#14882 = VERTEX_POINT('',#74801) ;
#14883 = VERTEX_POINT('',#74803) ;
#14884 = VERTEX_POINT('',#74811) ;
#14885 = VERTEX_POINT('',#74815) ;
#14886 = VERTEX_POINT('',#74817) ;
#14887 = VERTEX_POINT('',#74819) ;
#14888 = VERTEX_POINT('',#74850) ;
#14889 = VERTEX_POINT('',#74878) ;
#14890 = VERTEX_POINT('',#74915) ;
#14891 = VERTEX_POINT('',#74942) ;
#14892 = VERTEX_POINT('',#74990) ;
#14893 = VERTEX_POINT('',#74991) ;
#14894 = VERTEX_POINT('',#75014) ;
#14895 = VERTEX_POINT('',#75037) ;
#14896 = VERTEX_POINT('',#75039) ;
#14897 = VERTEX_POINT('',#75112) ;
#14898 = VERTEX_POINT('',#75114) ;
#14899 = VERTEX_POINT('',#75118) ;
#14900 = VERTEX_POINT('',#75120) ;
#14901 = VERTEX_POINT('',#75122) ;
#14902 = VERTEX_POINT('',#75153) ;
#14903 = VERTEX_POINT('',#75181) ;
#14904 = VERTEX_POINT('',#75186) ;
#14905 = VERTEX_POINT('',#75221) ;
#14906 = VERTEX_POINT('',#75222) ;
#14907 = VERTEX_POINT('',#75254) ;
#14908 = VERTEX_POINT('',#75255) ;
#14909 = VERTEX_POINT('',#75304) ;
#14910 = VERTEX_POINT('',#75305) ;
#14911 = VERTEX_POINT('',#75307) ;
#14912 = VERTEX_POINT('',#75390) ;
#14913 = VERTEX_POINT('',#75391) ;
#14914 = VERTEX_POINT('',#75480) ;
#14915 = VERTEX_POINT('',#75482) ;
#14916 = VERTEX_POINT('',#75484) ;
#14917 = VERTEX_POINT('',#75515) ;
#14918 = VERTEX_POINT('',#75543) ;
#14919 = VERTEX_POINT('',#75580) ;
#14920 = VERTEX_POINT('',#75607) ;
#14921 = VERTEX_POINT('',#75655) ;
#14922 = VERTEX_POINT('',#75656) ;
#14923 = VERTEX_POINT('',#75679) ;
#14924 = VERTEX_POINT('',#75702) ;
#14925 = VERTEX_POINT('',#75704) ;
#14926 = VERTEX_POINT('',#75777) ;
#14927 = VERTEX_POINT('',#75779) ;
#14928 = VERTEX_POINT('',#75783) ;
#14929 = VERTEX_POINT('',#75785) ;
#14930 = VERTEX_POINT('',#75787) ;
#14931 = VERTEX_POINT('',#75806) ;
#14932 = VERTEX_POINT('',#75807) ;
#14933 = VERTEX_POINT('',#75809) ;
#14934 = VERTEX_POINT('',#75813) ;
#14935 = VERTEX_POINT('',#75815) ;
#14936 = VERTEX_POINT('',#75819) ;
#14937 = VERTEX_POINT('',#75823) ;
#14938 = VERTEX_POINT('',#75825) ;
#14939 = VERTEX_POINT('',#75834) ;
#14940 = VERTEX_POINT('',#75836) ;
#14941 = VERTEX_POINT('',#75843) ;
#14942 = VERTEX_POINT('',#75876) ;
#14943 = VERTEX_POINT('',#75904) ;
#14944 = VERTEX_POINT('',#75927) ;
#14945 = VERTEX_POINT('',#75940) ;
#14946 = VERTEX_POINT('',#75941) ;
#14947 = VERTEX_POINT('',#75943) ;
#14948 = VERTEX_POINT('',#75966) ;
#14949 = VERTEX_POINT('',#75967) ;
#14950 = VERTEX_POINT('',#76001) ;
#14951 = VERTEX_POINT('',#76002) ;
#14952 = VERTEX_POINT('',#76036) ;
#14953 = VERTEX_POINT('',#76050) ;
#14954 = VERTEX_POINT('',#76052) ;
#14955 = VERTEX_POINT('',#76056) ;
#14956 = VERTEX_POINT('',#76060) ;
#14957 = VERTEX_POINT('',#76079) ;
#14958 = VERTEX_POINT('',#76083) ;
#14959 = VERTEX_POINT('',#76089) ;
#14960 = VERTEX_POINT('',#76091) ;
#14961 = VERTEX_POINT('',#76093) ;
#14962 = VERTEX_POINT('',#76095) ;
#14963 = VERTEX_POINT('',#76099) ;
#14964 = VERTEX_POINT('',#76103) ;
#14965 = VERTEX_POINT('',#76104) ;
#14966 = VERTEX_POINT('',#76106) ;
#14967 = VERTEX_POINT('',#76129) ;
#14968 = VERTEX_POINT('',#76130) ;
#14969 = VERTEX_POINT('',#76164) ;
#14970 = VERTEX_POINT('',#76166) ;
#14971 = VERTEX_POINT('',#76199) ;
#14972 = VERTEX_POINT('',#76213) ;
#14973 = VERTEX_POINT('',#76215) ;
#14974 = VERTEX_POINT('',#76217) ;
#14975 = VERTEX_POINT('',#76226) ;
#14976 = VERTEX_POINT('',#76237) ;
#14977 = VERTEX_POINT('',#76241) ;
#14978 = VERTEX_POINT('',#76243) ;
#14979 = VERTEX_POINT('',#76247) ;
#14980 = VERTEX_POINT('',#76270) ;
#14981 = VERTEX_POINT('',#76296) ;
#14982 = VERTEX_POINT('',#76336) ;
#14983 = VERTEX_POINT('',#76338) ;
#14984 = VERTEX_POINT('',#76342) ;
#14985 = VERTEX_POINT('',#76346) ;
#14986 = VERTEX_POINT('',#76365) ;
#14987 = VERTEX_POINT('',#76369) ;
#14988 = VERTEX_POINT('',#76375) ;
#14989 = VERTEX_POINT('',#76377) ;
#14990 = VERTEX_POINT('',#76379) ;
#14991 = VERTEX_POINT('',#76381) ;
#14992 = VERTEX_POINT('',#76385) ;
#14993 = VERTEX_POINT('',#76404) ;
#14994 = VERTEX_POINT('',#76408) ;
#14995 = VERTEX_POINT('',#76410) ;
#14996 = VERTEX_POINT('',#76414) ;
#14997 = VERTEX_POINT('',#76420) ;
#14998 = VERTEX_POINT('',#76422) ;
#14999 = VERTEX_POINT('',#76465) ;
#15000 = VERTEX_POINT('',#76466) ;
#15001 = VERTEX_POINT('',#76475) ;
#15002 = VERTEX_POINT('',#76486) ;
#15003 = VERTEX_POINT('',#76494) ;
#15004 = VERTEX_POINT('',#76496) ;
#15005 = VERTEX_POINT('',#76498) ;
#15006 = VERTEX_POINT('',#76517) ;
#15007 = VERTEX_POINT('',#76563) ;
#15008 = VERTEX_POINT('',#76681) ;
#15009 = VERTEX_POINT('',#76686) ;
#15010 = VERTEX_POINT('',#76693) ;
#15011 = VERTEX_POINT('',#77323) ;
#15012 = VERTEX_POINT('',#77324) ;
#15013 = VERTEX_POINT('',#77326) ;
#15014 = VERTEX_POINT('',#77328) ;
#15015 = VERTEX_POINT('',#77330) ;
#15016 = VERTEX_POINT('',#77332) ;
#15017 = VERTEX_POINT('',#77334) ;
#15018 = VERTEX_POINT('',#77336) ;
#15019 = VERTEX_POINT('',#77338) ;
#15020 = VERTEX_POINT('',#77361) ;
#15021 = VERTEX_POINT('',#77362) ;
#15022 = VERTEX_POINT('',#77386) ;
#15023 = VERTEX_POINT('',#77388) ;
#15024 = VERTEX_POINT('',#77392) ;
#15025 = VERTEX_POINT('',#77396) ;
#15026 = VERTEX_POINT('',#77398) ;
#15027 = VERTEX_POINT('',#77402) ;
#15028 = VERTEX_POINT('',#77406) ;
#15029 = VERTEX_POINT('',#77408) ;
#15030 = VERTEX_POINT('',#77413) ;
#15031 = VERTEX_POINT('',#77422) ;
#15032 = VERTEX_POINT('',#77423) ;
#15033 = VERTEX_POINT('',#77425) ;
#15034 = VERTEX_POINT('',#77448) ;
#15035 = VERTEX_POINT('',#77449) ;
#15036 = VERTEX_POINT('',#77473) ;
#15037 = VERTEX_POINT('',#77507) ;
#15038 = VERTEX_POINT('',#77519) ;
#15039 = VERTEX_POINT('',#77521) ;
#15040 = VERTEX_POINT('',#77525) ;
#15041 = VERTEX_POINT('',#77529) ;
#15042 = VERTEX_POINT('',#77533) ;
#15043 = VERTEX_POINT('',#77536) ;
#15044 = VERTEX_POINT('',#77555) ;
#15045 = VERTEX_POINT('',#77559) ;
#15046 = VERTEX_POINT('',#77560) ;
#15047 = VERTEX_POINT('',#77590) ;
#15048 = VERTEX_POINT('',#77595) ;
#15049 = VERTEX_POINT('',#77599) ;
#15050 = VERTEX_POINT('',#77605) ;
#15051 = VERTEX_POINT('',#77610) ;
#15052 = VERTEX_POINT('',#77661) ;
#15053 = VERTEX_POINT('',#77666) ;
#15054 = VERTEX_POINT('',#77670) ;
#15055 = VERTEX_POINT('',#77674) ;
#15056 = VERTEX_POINT('',#77676) ;
#15057 = VERTEX_POINT('',#77701) ;
#15058 = VERTEX_POINT('',#77703) ;
#15059 = VERTEX_POINT('',#77707) ;
#15060 = VERTEX_POINT('',#77713) ;
#15061 = VERTEX_POINT('',#77715) ;
#15062 = VERTEX_POINT('',#77740) ;
#15063 = VERTEX_POINT('',#77780) ;
#15064 = VERTEX_POINT('',#77782) ;
#15065 = VERTEX_POINT('',#77809) ;
#15066 = VERTEX_POINT('',#77810) ;
#15067 = VERTEX_POINT('',#77812) ;
#15068 = VERTEX_POINT('',#77814) ;
#15069 = VERTEX_POINT('',#77816) ;
#15070 = VERTEX_POINT('',#77818) ;
#15071 = VERTEX_POINT('',#77820) ;
#15072 = VERTEX_POINT('',#77822) ;
#15073 = VERTEX_POINT('',#77824) ;
#15074 = VERTEX_POINT('',#77847) ;
#15075 = VERTEX_POINT('',#77848) ;
#15076 = VERTEX_POINT('',#77872) ;
#15077 = VERTEX_POINT('',#77874) ;
#15078 = VERTEX_POINT('',#77878) ;
#15079 = VERTEX_POINT('',#77882) ;
#15080 = VERTEX_POINT('',#77884) ;
#15081 = VERTEX_POINT('',#77888) ;
#15082 = VERTEX_POINT('',#77892) ;
#15083 = VERTEX_POINT('',#77894) ;
#15084 = VERTEX_POINT('',#77899) ;
#15085 = VERTEX_POINT('',#77908) ;
#15086 = VERTEX_POINT('',#77909) ;
#15087 = VERTEX_POINT('',#77911) ;
#15088 = VERTEX_POINT('',#77934) ;
#15089 = VERTEX_POINT('',#77935) ;
#15090 = VERTEX_POINT('',#77959) ;
#15091 = VERTEX_POINT('',#77993) ;
#15092 = VERTEX_POINT('',#78005) ;
#15093 = VERTEX_POINT('',#78007) ;
#15094 = VERTEX_POINT('',#78011) ;
#15095 = VERTEX_POINT('',#78015) ;
#15096 = VERTEX_POINT('',#78020) ;
#15097 = VERTEX_POINT('',#78024) ;
#15098 = VERTEX_POINT('',#78025) ;
#15099 = VERTEX_POINT('',#78027) ;
#15100 = VERTEX_POINT('',#78029) ;
#15101 = VERTEX_POINT('',#78048) ;
#15102 = VERTEX_POINT('',#78077) ;
#15103 = VERTEX_POINT('',#78082) ;
#15104 = VERTEX_POINT('',#78086) ;
#15105 = VERTEX_POINT('',#78095) ;
#15106 = VERTEX_POINT('',#78100) ;
#15107 = VERTEX_POINT('',#78156) ;
#15108 = VERTEX_POINT('',#78160) ;
#15109 = VERTEX_POINT('',#78164) ;
#15110 = VERTEX_POINT('',#78166) ;
#15111 = VERTEX_POINT('',#78191) ;
#15112 = VERTEX_POINT('',#78193) ;
#15113 = VERTEX_POINT('',#78197) ;
#15114 = VERTEX_POINT('',#78205) ;
#15115 = VERTEX_POINT('',#78207) ;
#15116 = VERTEX_POINT('',#78232) ;
#15117 = VERTEX_POINT('',#78253) ;
#15118 = VERTEX_POINT('',#78290) ;
#15119 = VERTEX_POINT('',#78356) ;
#15120 = VERTEX_POINT('',#78410) ;
#15121 = VERTEX_POINT('',#78436) ;
#15122 = VERTEX_POINT('',#78457) ;
#15123 = VERTEX_POINT('',#78789) ;
#15124 = VERTEX_POINT('',#78790) ;
#15125 = VERTEX_POINT('',#78792) ;
#15126 = VERTEX_POINT('',#78809) ;
#15127 = VERTEX_POINT('',#78832) ;
#15128 = VERTEX_POINT('',#78833) ;
#15129 = VERTEX_POINT('',#78908) ;
#15130 = VERTEX_POINT('',#78909) ;
#15131 = VERTEX_POINT('',#78984) ;
#15132 = VERTEX_POINT('',#78985) ;
#15133 = VERTEX_POINT('',#78987) ;
#15134 = VERTEX_POINT('',#79002) ;
#15135 = VERTEX_POINT('',#79023) ;
#15136 = VERTEX_POINT('',#79024) ;
#15137 = VERTEX_POINT('',#79026) ;
#15138 = VERTEX_POINT('',#79037) ;
#15139 = VERTEX_POINT('',#79066) ;
#15140 = VERTEX_POINT('',#79067) ;
#15141 = VERTEX_POINT('',#79142) ;
#15142 = VERTEX_POINT('',#79143) ;
#15143 = VERTEX_POINT('',#79218) ;
#15144 = VERTEX_POINT('',#79219) ;
#15145 = VERTEX_POINT('',#79221) ;
#15146 = VERTEX_POINT('',#79230) ;
#15147 = VERTEX_POINT('',#79403) ;
#15148 = VERTEX_POINT('',#79404) ;
#15149 = VERTEX_POINT('',#79406) ;
#15150 = VERTEX_POINT('',#79408) ;
#15151 = VERTEX_POINT('',#79412) ;
#15152 = VERTEX_POINT('',#79413) ;
#15153 = VERTEX_POINT('',#79415) ;
#15154 = VERTEX_POINT('',#79417) ;
#15155 = VERTEX_POINT('',#79421) ;
#15156 = VERTEX_POINT('',#79422) ;
#15157 = VERTEX_POINT('',#79427) ;
#15158 = VERTEX_POINT('',#79428) ;
#15159 = VERTEX_POINT('',#79430) ;
#15160 = VERTEX_POINT('',#79432) ;
#15161 = VERTEX_POINT('',#79436) ;
#15162 = VERTEX_POINT('',#79437) ;
#15163 = VERTEX_POINT('',#79439) ;
#15164 = VERTEX_POINT('',#79441) ;
#15165 = VERTEX_POINT('',#79445) ;
#15166 = VERTEX_POINT('',#79446) ;
#15167 = VERTEX_POINT('',#79451) ;
#15168 = VERTEX_POINT('',#79452) ;
#15169 = VERTEX_POINT('',#79460) ;
#15170 = VERTEX_POINT('',#79465) ;
#15171 = VERTEX_POINT('',#79466) ;
#15172 = VERTEX_POINT('',#79468) ;
#15173 = VERTEX_POINT('',#79470) ;
#15174 = VERTEX_POINT('',#79474) ;
#15175 = VERTEX_POINT('',#79479) ;
#15176 = VERTEX_POINT('',#79480) ;
#15177 = VERTEX_POINT('',#79485) ;
#15178 = VERTEX_POINT('',#79486) ;
#15179 = VERTEX_POINT('',#79497) ;
#15180 = VERTEX_POINT('',#79498) ;
#15181 = VERTEX_POINT('',#79510) ;
#15182 = VERTEX_POINT('',#79512) ;
#15183 = VERTEX_POINT('',#79523) ;
#15184 = VERTEX_POINT('',#79525) ;
#15185 = VERTEX_POINT('',#79529) ;
#15186 = VERTEX_POINT('',#79531) ;
#15187 = VERTEX_POINT('',#79536) ;
#15188 = VERTEX_POINT('',#79543) ;
#15189 = VERTEX_POINT('',#79547) ;
#15190 = VERTEX_POINT('',#79556) ;
#15191 = VERTEX_POINT('',#79560) ;
#15192 = VERTEX_POINT('',#79562) ;
#15193 = VERTEX_POINT('',#79566) ;
#15194 = VERTEX_POINT('',#79568) ;
#15195 = VERTEX_POINT('',#79570) ;
#15196 = VERTEX_POINT('',#79572) ;
#15197 = VERTEX_POINT('',#79574) ;
#15198 = VERTEX_POINT('',#79576) ;
#15199 = VERTEX_POINT('',#79582) ;
#15200 = VERTEX_POINT('',#79583) ;
#15201 = VERTEX_POINT('',#79585) ;
#15202 = VERTEX_POINT('',#79587) ;
#15203 = VERTEX_POINT('',#79592) ;
#15204 = VERTEX_POINT('',#79594) ;
#15205 = VERTEX_POINT('',#79601) ;
#15206 = VERTEX_POINT('',#79602) ;
#15207 = VERTEX_POINT('',#79604) ;
#15208 = VERTEX_POINT('',#79606) ;
#15209 = VERTEX_POINT('',#79610) ;
#15210 = VERTEX_POINT('',#79611) ;
#15211 = VERTEX_POINT('',#79613) ;
#15212 = VERTEX_POINT('',#79615) ;
#15213 = VERTEX_POINT('',#79617) ;
#15214 = VERTEX_POINT('',#79619) ;
#15215 = VERTEX_POINT('',#79621) ;
#15216 = VERTEX_POINT('',#79623) ;
#15217 = VERTEX_POINT('',#79625) ;
#15218 = VERTEX_POINT('',#79627) ;
#15219 = VERTEX_POINT('',#79631) ;
#15220 = VERTEX_POINT('',#79632) ;
#15221 = VERTEX_POINT('',#79634) ;
#15222 = VERTEX_POINT('',#79636) ;
#15223 = VERTEX_POINT('',#79668) ;
#15224 = VERTEX_POINT('',#79681) ;
#15225 = VERTEX_POINT('',#79696) ;
#15226 = VERTEX_POINT('',#79709) ;
#15227 = VERTEX_POINT('',#79724) ;
#15228 = VERTEX_POINT('',#79725) ;
#15229 = VERTEX_POINT('',#79727) ;
#15230 = VERTEX_POINT('',#79729) ;
#15231 = VERTEX_POINT('',#79736) ;
#15232 = VERTEX_POINT('',#79737) ;
#15233 = VERTEX_POINT('',#79739) ;
#15234 = VERTEX_POINT('',#79741) ;
#15235 = VERTEX_POINT('',#79743) ;
#15236 = VERTEX_POINT('',#79745) ;
#15237 = VERTEX_POINT('',#79749) ;
#15238 = VERTEX_POINT('',#79750) ;
#15239 = VERTEX_POINT('',#79752) ;
#15240 = VERTEX_POINT('',#79754) ;
#15241 = VERTEX_POINT('',#79756) ;
#15242 = VERTEX_POINT('',#79758) ;
#15243 = VERTEX_POINT('',#79762) ;
#15244 = VERTEX_POINT('',#79764) ;
#15245 = VERTEX_POINT('',#79768) ;
#15246 = VERTEX_POINT('',#79770) ;
#15247 = VERTEX_POINT('',#79774) ;
#15248 = VERTEX_POINT('',#79778) ;
#15249 = VERTEX_POINT('',#79782) ;
#15250 = VERTEX_POINT('',#79789) ;
#15251 = VERTEX_POINT('',#79797) ;
#15252 = VERTEX_POINT('',#79801) ;
#15253 = VERTEX_POINT('',#79805) ;
#15254 = VERTEX_POINT('',#79811) ;
#15255 = VERTEX_POINT('',#79826) ;
#15256 = VERTEX_POINT('',#79832) ;
#15257 = VERTEX_POINT('',#79847) ;
#15258 = VERTEX_POINT('',#79866) ;
#15259 = VERTEX_POINT('',#79886) ;
#15260 = VERTEX_POINT('',#79888) ;
#15261 = VERTEX_POINT('',#79892) ;
#15262 = VERTEX_POINT('',#79895) ;
#15263 = VERTEX_POINT('',#79896) ;
#15264 = VERTEX_POINT('',#80831) ;
#15265 = VERTEX_POINT('',#80832) ;
#15266 = VERTEX_POINT('',#80839) ;
#15267 = VERTEX_POINT('',#80841) ;
#15268 = VERTEX_POINT('',#80874) ;
#15269 = VERTEX_POINT('',#80875) ;
#15270 = VERTEX_POINT('',#80882) ;
#15271 = VERTEX_POINT('',#80884) ;
#15272 = VERTEX_POINT('',#80919) ;
#15273 = VERTEX_POINT('',#80921) ;
#15274 = VERTEX_POINT('',#80956) ;
#15275 = VERTEX_POINT('',#80957) ;
#15276 = VERTEX_POINT('',#80964) ;
#15277 = VERTEX_POINT('',#80966) ;
#15278 = VERTEX_POINT('',#81001) ;
#15279 = VERTEX_POINT('',#81002) ;
#15280 = VERTEX_POINT('',#81009) ;
#15281 = VERTEX_POINT('',#81011) ;
#15282 = VERTEX_POINT('',#81020) ;
#15283 = VERTEX_POINT('',#81022) ;
#15284 = VERTEX_POINT('',#81026) ;
#15285 = VERTEX_POINT('',#81028) ;
#15286 = VERTEX_POINT('',#81030) ;
#15287 = VERTEX_POINT('',#81032) ;
#15288 = VERTEX_POINT('',#81035) ;
#15289 = VERTEX_POINT('',#81037) ;
#15290 = VERTEX_POINT('',#81039) ;
#15291 = VERTEX_POINT('',#81041) ;
#15292 = VERTEX_POINT('',#81044) ;
#15293 = VERTEX_POINT('',#81046) ;
#15294 = VERTEX_POINT('',#81048) ;
#15295 = VERTEX_POINT('',#81050) ;
#15296 = VERTEX_POINT('',#81053) ;
#15297 = VERTEX_POINT('',#81055) ;
#15298 = VERTEX_POINT('',#81057) ;
#15299 = VERTEX_POINT('',#81059) ;
#15300 = VERTEX_POINT('',#81063) ;
#15301 = VERTEX_POINT('',#81064) ;
#15302 = VERTEX_POINT('',#81066) ;
#15303 = VERTEX_POINT('',#81068) ;
#15304 = VERTEX_POINT('',#81072) ;
#15305 = VERTEX_POINT('',#81073) ;
#15306 = VERTEX_POINT('',#81075) ;
#15307 = VERTEX_POINT('',#81077) ;
#15308 = VERTEX_POINT('',#81081) ;
#15309 = VERTEX_POINT('',#81082) ;
#15310 = VERTEX_POINT('',#81084) ;
#15311 = VERTEX_POINT('',#81086) ;
#15312 = VERTEX_POINT('',#81090) ;
#15313 = VERTEX_POINT('',#81091) ;
#15314 = VERTEX_POINT('',#81093) ;
#15315 = VERTEX_POINT('',#81095) ;
#15316 = VERTEX_POINT('',#81099) ;
#15317 = VERTEX_POINT('',#81101) ;
#15318 = VERTEX_POINT('',#81105) ;
#15319 = VERTEX_POINT('',#81109) ;
#15320 = VERTEX_POINT('',#81113) ;
#15321 = VERTEX_POINT('',#81115) ;
#15322 = VERTEX_POINT('',#81119) ;
#15323 = VERTEX_POINT('',#81123) ;
#15324 = VERTEX_POINT('',#81127) ;
#15325 = VERTEX_POINT('',#81129) ;
#15326 = VERTEX_POINT('',#81133) ;
#15327 = VERTEX_POINT('',#81137) ;
#15328 = VERTEX_POINT('',#81141) ;
#15329 = VERTEX_POINT('',#81142) ;
#15330 = VERTEX_POINT('',#81147) ;
#15331 = VERTEX_POINT('',#81148) ;
#15332 = VERTEX_POINT('',#81162) ;
#15333 = VERTEX_POINT('',#81163) ;
#15334 = VERTEX_POINT('',#81165) ;
#15335 = VERTEX_POINT('',#81167) ;
#15336 = VERTEX_POINT('',#81171) ;
#15337 = VERTEX_POINT('',#81172) ;
#15338 = VERTEX_POINT('',#81174) ;
#15339 = VERTEX_POINT('',#81176) ;
#15340 = VERTEX_POINT('',#81188) ;
#15341 = VERTEX_POINT('',#81189) ;
#15342 = VERTEX_POINT('',#81194) ;
#15343 = VERTEX_POINT('',#81195) ;
#15344 = VERTEX_POINT('',#81209) ;
#15345 = VERTEX_POINT('',#81210) ;
#15346 = VERTEX_POINT('',#81215) ;
#15347 = VERTEX_POINT('',#81216) ;
#15348 = VERTEX_POINT('',#81239) ;
#15349 = VERTEX_POINT('',#81240) ;
#15350 = VERTEX_POINT('',#81242) ;
#15351 = VERTEX_POINT('',#81244) ;
#15352 = VERTEX_POINT('',#81248) ;
#15353 = VERTEX_POINT('',#81249) ;
#15354 = VERTEX_POINT('',#81251) ;
#15355 = VERTEX_POINT('',#81255) ;
#15356 = VERTEX_POINT('',#81256) ;
#15357 = VERTEX_POINT('',#81258) ;
#15358 = VERTEX_POINT('',#81260) ;
#15359 = VERTEX_POINT('',#81274) ;
#15360 = VERTEX_POINT('',#81275) ;
#15361 = VERTEX_POINT('',#81277) ;
#15362 = VERTEX_POINT('',#81279) ;
#15363 = VERTEX_POINT('',#81283) ;
#15364 = VERTEX_POINT('',#81284) ;
#15365 = VERTEX_POINT('',#81286) ;
#15366 = VERTEX_POINT('',#81290) ;
#15367 = VERTEX_POINT('',#81291) ;
#15368 = VERTEX_POINT('',#81293) ;
#15369 = VERTEX_POINT('',#81295) ;
#15370 = VERTEX_POINT('',#81309) ;
#15371 = VERTEX_POINT('',#81310) ;
#15372 = VERTEX_POINT('',#81312) ;
#15373 = VERTEX_POINT('',#81314) ;
#15374 = VERTEX_POINT('',#81318) ;
#15375 = VERTEX_POINT('',#81319) ;
#15376 = VERTEX_POINT('',#81321) ;
#15377 = VERTEX_POINT('',#81325) ;
#15378 = VERTEX_POINT('',#81326) ;
#15379 = VERTEX_POINT('',#81328) ;
#15380 = VERTEX_POINT('',#81330) ;
#15381 = VERTEX_POINT('',#81344) ;
#15382 = VERTEX_POINT('',#81345) ;
#15383 = VERTEX_POINT('',#81347) ;
#15384 = VERTEX_POINT('',#81349) ;
#15385 = VERTEX_POINT('',#81353) ;
#15386 = VERTEX_POINT('',#81354) ;
#15387 = VERTEX_POINT('',#81356) ;
#15388 = VERTEX_POINT('',#81360) ;
#15389 = VERTEX_POINT('',#81361) ;
#15390 = VERTEX_POINT('',#81363) ;
#15391 = VERTEX_POINT('',#81365) ;
#15392 = VERTEX_POINT('',#81379) ;
#15393 = VERTEX_POINT('',#81381) ;
#15394 = VERTEX_POINT('',#81383) ;
#15395 = VERTEX_POINT('',#81386) ;
#15396 = VERTEX_POINT('',#81390) ;
#15397 = VERTEX_POINT('',#81392) ;
#15398 = VERTEX_POINT('',#81394) ;
#15399 = VERTEX_POINT('',#81397) ;
#15400 = VERTEX_POINT('',#81401) ;
#15401 = VERTEX_POINT('',#81403) ;
#15402 = VERTEX_POINT('',#81405) ;
#15403 = VERTEX_POINT('',#81408) ;
#15404 = VERTEX_POINT('',#81412) ;
#15405 = VERTEX_POINT('',#81414) ;
#15406 = VERTEX_POINT('',#81416) ;
#15407 = VERTEX_POINT('',#81419) ;
#15408 = VERTEX_POINT('',#81424) ;
#15409 = VERTEX_POINT('',#81456) ;
#15410 = VERTEX_POINT('',#81457) ;
#15411 = VERTEX_POINT('',#81502) ;
#15412 = VERTEX_POINT('',#81503) ;
#15413 = VERTEX_POINT('',#81548) ;
#15414 = VERTEX_POINT('',#81549) ;
#15415 = VERTEX_POINT('',#81588) ;
#15416 = VERTEX_POINT('',#81627) ;
#15417 = VERTEX_POINT('',#81628) ;
#15418 = VERTEX_POINT('',#81665) ;
#15419 = VERTEX_POINT('',#81666) ;
#15420 = VERTEX_POINT('',#81668) ;
#15421 = VERTEX_POINT('',#81670) ;
#15422 = VERTEX_POINT('',#81672) ;
#15423 = VERTEX_POINT('',#81674) ;
#15424 = VERTEX_POINT('',#81678) ;
#15425 = VERTEX_POINT('',#81680) ;
#15426 = VERTEX_POINT('',#81682) ;
#15427 = VERTEX_POINT('',#81684) ;
#15428 = VERTEX_POINT('',#81688) ;
#15429 = VERTEX_POINT('',#81690) ;
#15430 = VERTEX_POINT('',#81692) ;
#15431 = VERTEX_POINT('',#81696) ;
#15432 = VERTEX_POINT('',#81700) ;
#15433 = VERTEX_POINT('',#81701) ;
#15434 = VERTEX_POINT('',#81703) ;
#15435 = VERTEX_POINT('',#81708) ;
#15436 = VERTEX_POINT('',#81710) ;
#15437 = VERTEX_POINT('',#81712) ;
#15438 = VERTEX_POINT('',#81716) ;
#15439 = VERTEX_POINT('',#81717) ;
#15440 = VERTEX_POINT('',#81719) ;
#15441 = VERTEX_POINT('',#81722) ;
#15442 = VERTEX_POINT('',#81726) ;
#15443 = VERTEX_POINT('',#81731) ;
#15444 = VERTEX_POINT('',#81735) ;
#15445 = VERTEX_POINT('',#81737) ;
#15446 = VERTEX_POINT('',#81739) ;
#15447 = VERTEX_POINT('',#81743) ;
#15448 = VERTEX_POINT('',#81749) ;
#15449 = VERTEX_POINT('',#81751) ;
#15450 = VERTEX_POINT('',#81753) ;
#15451 = VERTEX_POINT('',#81755) ;
#15452 = VERTEX_POINT('',#81757) ;
#15453 = VERTEX_POINT('',#81761) ;
#15454 = VERTEX_POINT('',#81763) ;
#15455 = VERTEX_POINT('',#81765) ;
#15456 = VERTEX_POINT('',#81767) ;
#15457 = VERTEX_POINT('',#81769) ;
#15458 = VERTEX_POINT('',#81772) ;
#15459 = VERTEX_POINT('',#81776) ;
#15460 = VERTEX_POINT('',#81798) ;
#15461 = VERTEX_POINT('',#81799) ;
#15462 = VERTEX_POINT('',#81801) ;
#15463 = VERTEX_POINT('',#81826) ;
#15464 = VERTEX_POINT('',#81851) ;
#15465 = VERTEX_POINT('',#81852) ;
#15466 = VERTEX_POINT('',#81927) ;
#15467 = VERTEX_POINT('',#81928) ;
#15468 = VERTEX_POINT('',#82005) ;
#15469 = VERTEX_POINT('',#82006) ;
#15470 = VERTEX_POINT('',#82083) ;
#15471 = VERTEX_POINT('',#82084) ;
#15472 = VERTEX_POINT('',#82159) ;
#15473 = VERTEX_POINT('',#82160) ;
#15474 = VERTEX_POINT('',#82235) ;
#15475 = VERTEX_POINT('',#82236) ;
#15476 = VERTEX_POINT('',#82311) ;
#15477 = VERTEX_POINT('',#82312) ;
#15478 = VERTEX_POINT('',#82387) ;
#15479 = VERTEX_POINT('',#82388) ;
#15480 = VERTEX_POINT('',#82465) ;
#15481 = VERTEX_POINT('',#82466) ;
#15482 = VERTEX_POINT('',#82541) ;
#15483 = VERTEX_POINT('',#82542) ;
#15484 = VERTEX_POINT('',#82619) ;
#15485 = VERTEX_POINT('',#82620) ;
#15486 = VERTEX_POINT('',#82695) ;
#15487 = VERTEX_POINT('',#82696) ;
#15488 = VERTEX_POINT('',#82771) ;
#15489 = VERTEX_POINT('',#82772) ;
#15490 = VERTEX_POINT('',#82847) ;
#15491 = VERTEX_POINT('',#82848) ;
#15492 = VERTEX_POINT('',#82923) ;
#15493 = VERTEX_POINT('',#82924) ;
#15494 = VERTEX_POINT('',#82926) ;
#15495 = VERTEX_POINT('',#82959) ;
#15496 = VERTEX_POINT('',#82961) ;
#15497 = VERTEX_POINT('',#83072) ;
#15498 = VERTEX_POINT('',#83073) ;
#15499 = VERTEX_POINT('',#83148) ;
#15500 = VERTEX_POINT('',#83149) ;
#15501 = VERTEX_POINT('',#83224) ;
#15502 = VERTEX_POINT('',#83225) ;
#15503 = VERTEX_POINT('',#83300) ;
#15504 = VERTEX_POINT('',#83301) ;
#15505 = VERTEX_POINT('',#83376) ;
#15506 = VERTEX_POINT('',#83377) ;
#15507 = VERTEX_POINT('',#83454) ;
#15508 = VERTEX_POINT('',#83455) ;
#15509 = VERTEX_POINT('',#83530) ;
#15510 = VERTEX_POINT('',#83531) ;
#15511 = VERTEX_POINT('',#83606) ;
#15512 = VERTEX_POINT('',#83607) ;
#15513 = VERTEX_POINT('',#83684) ;
#15514 = VERTEX_POINT('',#83685) ;
#15515 = VERTEX_POINT('',#83760) ;
#15516 = VERTEX_POINT('',#83761) ;
#15517 = VERTEX_POINT('',#83836) ;
#15518 = VERTEX_POINT('',#83837) ;
#15519 = VERTEX_POINT('',#83912) ;
#15520 = VERTEX_POINT('',#83913) ;
#15521 = VERTEX_POINT('',#83988) ;
#15522 = VERTEX_POINT('',#83989) ;
#15523 = VERTEX_POINT('',#84066) ;
#15524 = VERTEX_POINT('',#84067) ;
#15525 = VERTEX_POINT('',#84142) ;
#15526 = VERTEX_POINT('',#84143) ;
#15527 = VERTEX_POINT('',#84220) ;
#15528 = VERTEX_POINT('',#84221) ;
#15529 = VERTEX_POINT('',#84223) ;
#15530 = VERTEX_POINT('',#84286) ;
#15531 = VERTEX_POINT('',#84301) ;
#15532 = VERTEX_POINT('',#84314) ;
#15533 = VERTEX_POINT('',#84345) ;
#15534 = VERTEX_POINT('',#84376) ;
#15535 = VERTEX_POINT('',#84377) ;
#15536 = VERTEX_POINT('',#84379) ;
#15537 = VERTEX_POINT('',#84383) ;
#15538 = VERTEX_POINT('',#84389) ;
#15539 = VERTEX_POINT('',#84390) ;
#15540 = VERTEX_POINT('',#84392) ;
#15541 = VERTEX_POINT('',#84396) ;
#15542 = VERTEX_POINT('',#84402) ;
#15543 = VERTEX_POINT('',#84404) ;
#15544 = VERTEX_POINT('',#84406) ;
#15545 = VERTEX_POINT('',#84410) ;
#15546 = VERTEX_POINT('',#84411) ;
#15547 = VERTEX_POINT('',#84413) ;
#15548 = VERTEX_POINT('',#84415) ;
#15549 = VERTEX_POINT('',#84417) ;
#15550 = VERTEX_POINT('',#84420) ;
#15551 = VERTEX_POINT('',#84422) ;
#15552 = VERTEX_POINT('',#84424) ;
#15553 = VERTEX_POINT('',#84427) ;
#15554 = VERTEX_POINT('',#84429) ;
#15555 = VERTEX_POINT('',#84431) ;
#15556 = VERTEX_POINT('',#84433) ;
#15557 = VERTEX_POINT('',#84435) ;
#15558 = VERTEX_POINT('',#84437) ;
#15559 = VERTEX_POINT('',#84439) ;
#15560 = VERTEX_POINT('',#84441) ;
#15561 = VERTEX_POINT('',#84445) ;
#15562 = VERTEX_POINT('',#84446) ;
#15563 = VERTEX_POINT('',#84451) ;
#15564 = VERTEX_POINT('',#85384) ;
#15565 = VERTEX_POINT('',#85388) ;
#15566 = VERTEX_POINT('',#85394) ;
#15567 = VERTEX_POINT('',#85398) ;
#15568 = VERTEX_POINT('',#85402) ;
#15569 = VERTEX_POINT('',#85408) ;
#15570 = VERTEX_POINT('',#85410) ;
#15571 = VERTEX_POINT('',#85412) ;
#15572 = VERTEX_POINT('',#85414) ;
#15573 = VERTEX_POINT('',#85416) ;
#15574 = VERTEX_POINT('',#85418) ;
#15575 = VERTEX_POINT('',#85420) ;
#15576 = VERTEX_POINT('',#85422) ;
#15577 = VERTEX_POINT('',#85424) ;
#15578 = VERTEX_POINT('',#85427) ;
#15579 = VERTEX_POINT('',#85429) ;
#15580 = VERTEX_POINT('',#85462) ;
#15581 = VERTEX_POINT('',#85463) ;
#15582 = VERTEX_POINT('',#85465) ;
#15583 = VERTEX_POINT('',#85467) ;
#15584 = VERTEX_POINT('',#85471) ;
#15585 = VERTEX_POINT('',#85472) ;
#15586 = VERTEX_POINT('',#85474) ;
#15587 = VERTEX_POINT('',#85476) ;
#15588 = VERTEX_POINT('',#86234) ;
#15589 = VERTEX_POINT('',#86236) ;
#15590 = VERTEX_POINT('',#86238) ;
#15591 = VERTEX_POINT('',#86242) ;
#15592 = VERTEX_POINT('',#86243) ;
#15593 = VERTEX_POINT('',#86248) ;
#15594 = VERTEX_POINT('',#86251) ;
#15595 = VERTEX_POINT('',#86255) ;
#15596 = EDGE_CURVE('',#12667,#12668,#10873,.T.) ;
#15597 = EDGE_CURVE('',#12668,#12669,#6235,.T.) ;
#15598 = EDGE_CURVE('',#12669,#12670,#10874,.T.) ;
#15599 = EDGE_CURVE('',#12670,#12667,#6236,.T.) ;
#15600 = EDGE_CURVE('',#12671,#12668,#6237,.T.) ;
#15601 = EDGE_CURVE('',#12672,#12671,#6238,.T.) ;
#15602 = EDGE_CURVE('',#12672,#12673,#6239,.T.) ;
#15603 = EDGE_CURVE('',#12674,#12673,#6240,.T.) ;
#15604 = EDGE_CURVE('',#12674,#12669,#6241,.T.) ;
#15605 = EDGE_CURVE('',#12675,#12676,#10875,.F.) ;
#15606 = EDGE_CURVE('',#12677,#12676,#1189,.T.) ;
#15607 = EDGE_CURVE('',#12677,#12678,#10876,.T.) ;
#15608 = EDGE_CURVE('',#12675,#12678,#10877,.T.) ;
#15609 = EDGE_CURVE('',#12679,#12680,#1190,.T.) ;
#15610 = EDGE_CURVE('',#12679,#12681,#10878,.T.) ;
#15611 = EDGE_CURVE('',#12682,#12681,#10879,.T.) ;
#15612 = EDGE_CURVE('',#12682,#12680,#10880,.F.) ;
#15613 = EDGE_CURVE('',#12683,#12684,#10881,.T.) ;
#15614 = EDGE_CURVE('',#12683,#12685,#10882,.T.) ;
#15615 = EDGE_CURVE('',#12686,#12685,#10883,.T.) ;
#15616 = EDGE_CURVE('',#12686,#12684,#10884,.F.) ;
#15617 = EDGE_CURVE('',#12687,#12688,#10885,.F.) ;
#15618 = EDGE_CURVE('',#12689,#12688,#10886,.F.) ;
#15619 = EDGE_CURVE('',#12689,#12690,#10887,.T.) ;
#15620 = EDGE_CURVE('',#12687,#12690,#10888,.F.) ;
#15621 = EDGE_CURVE('',#12691,#12692,#6242,.F.) ;
#15622 = EDGE_CURVE('',#12691,#12693,#10889,.T.) ;
#15623 = EDGE_CURVE('',#12694,#12693,#6243,.F.) ;
#15624 = EDGE_CURVE('',#12694,#12692,#10890,.T.) ;
#15625 = EDGE_CURVE('',#12695,#12696,#6244,.F.) ;
#15626 = EDGE_CURVE('',#12695,#12697,#10891,.T.) ;
#15627 = EDGE_CURVE('',#12698,#12697,#6245,.F.) ;
#15628 = EDGE_CURVE('',#12698,#12696,#10892,.T.) ;
#15629 = EDGE_CURVE('',#12699,#12700,#6246,.F.) ;
#15630 = EDGE_CURVE('',#12699,#12701,#10893,.T.) ;
#15631 = EDGE_CURVE('',#12702,#12701,#6247,.F.) ;
#15632 = EDGE_CURVE('',#12702,#12700,#10894,.T.) ;
#15633 = EDGE_CURVE('',#12703,#12704,#6248,.F.) ;
#15634 = EDGE_CURVE('',#12703,#12705,#10895,.T.) ;
#15635 = EDGE_CURVE('',#12706,#12705,#6249,.F.) ;
#15636 = EDGE_CURVE('',#12706,#12704,#10896,.T.) ;
#15637 = EDGE_CURVE('',#12707,#12708,#6250,.F.) ;
#15638 = EDGE_CURVE('',#12707,#12709,#10897,.T.) ;
#15639 = EDGE_CURVE('',#12710,#12709,#6251,.F.) ;
#15640 = EDGE_CURVE('',#12710,#12708,#10898,.T.) ;
#15641 = EDGE_CURVE('',#12711,#12712,#6252,.F.) ;
#15642 = EDGE_CURVE('',#12711,#12713,#10899,.T.) ;
#15643 = EDGE_CURVE('',#12714,#12713,#6253,.F.) ;
#15644 = EDGE_CURVE('',#12714,#12712,#10900,.T.) ;
#15645 = EDGE_CURVE('',#12715,#12715,#10901,.T.) ;
#15646 = EDGE_CURVE('',#12716,#12716,#10902,.T.) ;
#15647 = EDGE_CURVE('',#12717,#12717,#10903,.T.) ;
#15648 = EDGE_CURVE('',#12718,#12718,#10904,.T.) ;
#15649 = EDGE_CURVE('',#12719,#12719,#10905,.T.) ;
#15650 = EDGE_CURVE('',#12720,#12720,#10906,.T.) ;
#15651 = EDGE_CURVE('',#12721,#12722,#10907,.F.) ;
#15652 = EDGE_CURVE('',#12721,#12723,#10908,.T.) ;
#15653 = EDGE_CURVE('',#12724,#12723,#10909,.F.) ;
#15654 = EDGE_CURVE('',#12724,#12722,#10910,.F.) ;
#15655 = EDGE_CURVE('',#12725,#12726,#10911,.F.) ;
#15656 = EDGE_CURVE('',#12725,#12727,#10912,.T.) ;
#15657 = EDGE_CURVE('',#12728,#12727,#10913,.F.) ;
#15658 = EDGE_CURVE('',#12728,#12726,#10914,.F.) ;
#15659 = EDGE_CURVE('',#12729,#12730,#10915,.F.) ;
#15660 = EDGE_CURVE('',#12729,#12731,#10916,.T.) ;
#15661 = EDGE_CURVE('',#12732,#12731,#10917,.F.) ;
#15662 = EDGE_CURVE('',#12732,#12730,#10918,.F.) ;
#15663 = EDGE_CURVE('',#12733,#12734,#10919,.F.) ;
#15664 = EDGE_CURVE('',#12735,#12734,#10920,.T.) ;
#15665 = EDGE_CURVE('',#12735,#12736,#10921,.T.) ;
#15666 = EDGE_CURVE('',#12733,#12736,#10922,.T.) ;
#15667 = EDGE_CURVE('',#12737,#12674,#10923,.T.) ;
#15668 = EDGE_CURVE('',#12673,#12738,#10924,.T.) ;
#15669 = EDGE_CURVE('',#12738,#12737,#6254,.T.) ;
#15670 = EDGE_CURVE('',#12671,#12739,#10925,.T.) ;
#15671 = EDGE_CURVE('',#12739,#12740,#6255,.T.) ;
#15672 = EDGE_CURVE('',#12740,#12672,#10926,.T.) ;
#15673 = EDGE_CURVE('',#12739,#12741,#6256,.F.) ;
#15674 = EDGE_CURVE('',#12742,#12741,#10927,.T.) ;
#15675 = EDGE_CURVE('',#12742,#12743,#6257,.F.) ;
#15676 = EDGE_CURVE('',#12744,#12743,#10928,.T.) ;
#15677 = EDGE_CURVE('',#12744,#12745,#6258,.F.) ;
#15678 = EDGE_CURVE('',#12746,#12745,#10929,.T.) ;
#15679 = EDGE_CURVE('',#12747,#12746,#6259,.T.) ;
#15680 = EDGE_CURVE('',#12748,#12747,#10930,.T.) ;
#15681 = EDGE_CURVE('',#12748,#12749,#6260,.F.) ;
#15682 = EDGE_CURVE('',#12750,#12749,#10931,.T.) ;
#15683 = EDGE_CURVE('',#12750,#12751,#6261,.F.) ;
#15684 = EDGE_CURVE('',#12752,#12751,#10932,.T.) ;
#15685 = EDGE_CURVE('',#12752,#12753,#6262,.F.) ;
#15686 = EDGE_CURVE('',#12754,#12753,#10933,.T.) ;
#15687 = EDGE_CURVE('',#12755,#12754,#6263,.T.) ;
#15688 = EDGE_CURVE('',#12756,#12755,#10934,.T.) ;
#15689 = EDGE_CURVE('',#12756,#12740,#6264,.F.) ;
#15690 = EDGE_CURVE('',#12757,#12757,#10935,.F.) ;
#15691 = EDGE_CURVE('',#12758,#12758,#10936,.F.) ;
#15692 = EDGE_CURVE('',#12759,#12760,#10937,.T.) ;
#15693 = EDGE_CURVE('',#12760,#12761,#6265,.T.) ;
#15694 = EDGE_CURVE('',#12761,#12762,#10938,.T.) ;
#15695 = EDGE_CURVE('',#12762,#12759,#6266,.T.) ;
#15696 = EDGE_CURVE('',#12763,#12759,#6267,.T.) ;
#15697 = EDGE_CURVE('',#12764,#12763,#6268,.T.) ;
#15698 = EDGE_CURVE('',#12670,#12764,#6269,.T.) ;
#15699 = EDGE_CURVE('',#12765,#12674,#6270,.F.) ;
#15700 = EDGE_CURVE('',#12760,#12765,#6271,.T.) ;
#15701 = EDGE_CURVE('',#12762,#12766,#6272,.T.) ;
#15702 = EDGE_CURVE('',#12767,#12766,#10939,.T.) ;
#15703 = EDGE_CURVE('',#12768,#12767,#6273,.T.) ;
#15704 = EDGE_CURVE('',#12769,#12768,#10940,.T.) ;
#15705 = EDGE_CURVE('',#12770,#12769,#6274,.T.) ;
#15706 = EDGE_CURVE('',#12771,#12770,#10941,.T.) ;
#15707 = EDGE_CURVE('',#12772,#12771,#6275,.F.) ;
#15708 = EDGE_CURVE('',#12773,#12772,#10942,.T.) ;
#15709 = EDGE_CURVE('',#12774,#12773,#6276,.T.) ;
#15710 = EDGE_CURVE('',#12775,#12774,#10943,.T.) ;
#15711 = EDGE_CURVE('',#12776,#12775,#6277,.T.) ;
#15712 = EDGE_CURVE('',#12777,#12776,#10944,.T.) ;
#15713 = EDGE_CURVE('',#12777,#12778,#6278,.T.) ;
#15714 = EDGE_CURVE('',#12779,#12778,#10945,.T.) ;
#15715 = EDGE_CURVE('',#12780,#12779,#6279,.T.) ;
#15716 = EDGE_CURVE('',#12763,#12780,#10946,.T.) ;
#15717 = EDGE_CURVE('',#12781,#12781,#10947,.T.) ;
#15718 = EDGE_CURVE('',#12782,#12782,#10948,.T.) ;
#15719 = EDGE_CURVE('',#12783,#12784,#10949,.T.) ;
#15720 = EDGE_CURVE('',#12784,#12785,#6280,.T.) ;
#15721 = EDGE_CURVE('',#12785,#12786,#10950,.T.) ;
#15722 = EDGE_CURVE('',#12786,#12783,#6281,.T.) ;
#15723 = EDGE_CURVE('',#12787,#12783,#6282,.T.) ;
#15724 = EDGE_CURVE('',#12741,#12787,#6283,.T.) ;
#15725 = EDGE_CURVE('',#12788,#12671,#6284,.T.) ;
#15726 = EDGE_CURVE('',#12784,#12788,#6285,.T.) ;
#15727 = EDGE_CURVE('',#12789,#12786,#6286,.T.) ;
#15728 = EDGE_CURVE('',#12790,#12789,#10951,.T.) ;
#15729 = EDGE_CURVE('',#12791,#12790,#6287,.T.) ;
#15730 = EDGE_CURVE('',#12792,#12791,#10952,.T.) ;
#15731 = EDGE_CURVE('',#12792,#12793,#6288,.T.) ;
#15732 = EDGE_CURVE('',#12794,#12793,#10953,.T.) ;
#15733 = EDGE_CURVE('',#12794,#12795,#6289,.T.) ;
#15734 = EDGE_CURVE('',#12796,#12795,#10954,.T.) ;
#15735 = EDGE_CURVE('',#12796,#12797,#6290,.T.) ;
#15736 = EDGE_CURVE('',#12798,#12797,#10955,.T.) ;
#15737 = EDGE_CURVE('',#12799,#12798,#6291,.T.) ;
#15738 = EDGE_CURVE('',#12800,#12799,#10956,.T.) ;
#15739 = EDGE_CURVE('',#12800,#12801,#6292,.T.) ;
#15740 = EDGE_CURVE('',#12802,#12801,#10957,.T.) ;
#15741 = EDGE_CURVE('',#12802,#12803,#6293,.T.) ;
#15742 = EDGE_CURVE('',#12787,#12803,#10958,.T.) ;
#15743 = EDGE_CURVE('',#12804,#12804,#10959,.T.) ;
#15744 = EDGE_CURVE('',#12805,#12805,#10960,.T.) ;
#15745 = EDGE_CURVE('',#12768,#12806,#6294,.T.) ;
#15746 = EDGE_CURVE('',#12806,#12807,#10961,.T.) ;
#15747 = EDGE_CURVE('',#12807,#12769,#6295,.T.) ;
#15748 = EDGE_CURVE('',#12808,#12767,#6296,.T.) ;
#15749 = EDGE_CURVE('',#12806,#12808,#6297,.T.) ;
#15750 = EDGE_CURVE('',#12743,#12802,#6298,.T.) ;
#15751 = EDGE_CURVE('',#12801,#12744,#6299,.T.) ;
#15752 = EDGE_CURVE('',#12803,#12742,#6300,.T.) ;
#15753 = EDGE_CURVE('',#12809,#12810,#10962,.T.) ;
#15754 = EDGE_CURVE('',#12810,#12811,#6301,.T.) ;
#15755 = EDGE_CURVE('',#12811,#12812,#10963,.T.) ;
#15756 = EDGE_CURVE('',#12812,#12809,#6302,.T.) ;
#15757 = EDGE_CURVE('',#12811,#12765,#6303,.F.) ;
#15758 = EDGE_CURVE('',#12813,#12737,#6304,.F.) ;
#15759 = EDGE_CURVE('',#12814,#12813,#6305,.T.) ;
#15760 = EDGE_CURVE('',#12812,#12814,#6306,.F.) ;
#15761 = EDGE_CURVE('',#12815,#12810,#6307,.F.) ;
#15762 = EDGE_CURVE('',#12785,#12815,#6308,.T.) ;
#15763 = EDGE_CURVE('',#12816,#12788,#6309,.T.) ;
#15764 = EDGE_CURVE('',#12817,#12816,#6310,.T.) ;
#15765 = EDGE_CURVE('',#12818,#12817,#6311,.T.) ;
#15766 = EDGE_CURVE('',#12761,#12818,#6312,.T.) ;
#15767 = EDGE_CURVE('',#12819,#12820,#10964,.T.) ;
#15768 = EDGE_CURVE('',#12821,#12820,#10965,.T.) ;
#15769 = EDGE_CURVE('',#12822,#12821,#10966,.T.) ;
#15770 = EDGE_CURVE('',#12819,#12822,#10967,.T.) ;
#15771 = EDGE_CURVE('',#12823,#12823,#10968,.T.) ;
#15772 = EDGE_CURVE('',#12824,#12824,#10969,.T.) ;
#15773 = EDGE_CURVE('',#12825,#12826,#10970,.T.) ;
#15774 = EDGE_CURVE('',#12827,#12826,#6313,.T.) ;
#15775 = EDGE_CURVE('',#12827,#12828,#10971,.T.) ;
#15776 = EDGE_CURVE('',#12825,#12828,#6314,.T.) ;
#15777 = EDGE_CURVE('',#12829,#12830,#10972,.T.) ;
#15778 = EDGE_CURVE('',#12831,#12830,#6315,.T.) ;
#15779 = EDGE_CURVE('',#12831,#12832,#10973,.T.) ;
#15780 = EDGE_CURVE('',#12829,#12832,#6316,.T.) ;
#15781 = EDGE_CURVE('',#12833,#12834,#10974,.T.) ;
#15782 = EDGE_CURVE('',#12835,#12834,#6317,.T.) ;
#15783 = EDGE_CURVE('',#12835,#12836,#10975,.T.) ;
#15784 = EDGE_CURVE('',#12833,#12836,#6318,.T.) ;
#15785 = EDGE_CURVE('',#12837,#12838,#10976,.T.) ;
#15786 = EDGE_CURVE('',#12839,#12838,#6319,.T.) ;
#15787 = EDGE_CURVE('',#12839,#12840,#10977,.T.) ;
#15788 = EDGE_CURVE('',#12837,#12840,#6320,.T.) ;
#15789 = EDGE_CURVE('',#12841,#12842,#10978,.T.) ;
#15790 = EDGE_CURVE('',#12843,#12842,#6321,.T.) ;
#15791 = EDGE_CURVE('',#12843,#12844,#10979,.T.) ;
#15792 = EDGE_CURVE('',#12841,#12844,#6322,.T.) ;
#15793 = EDGE_CURVE('',#12845,#12846,#10980,.T.) ;
#15794 = EDGE_CURVE('',#12847,#12846,#6323,.T.) ;
#15795 = EDGE_CURVE('',#12847,#12848,#10981,.T.) ;
#15796 = EDGE_CURVE('',#12845,#12848,#6324,.T.) ;
#15797 = EDGE_CURVE('',#12849,#12849,#10982,.T.) ;
#15798 = EDGE_CURVE('',#12850,#12850,#10983,.T.) ;
#15799 = EDGE_CURVE('',#12851,#12851,#10984,.T.) ;
#15800 = EDGE_CURVE('',#12852,#12852,#10985,.T.) ;
#15801 = EDGE_CURVE('',#12853,#12854,#10986,.T.) ;
#15802 = EDGE_CURVE('',#12855,#12854,#10987,.T.) ;
#15803 = EDGE_CURVE('',#12855,#12856,#10988,.T.) ;
#15804 = EDGE_CURVE('',#12853,#12856,#10989,.T.) ;
#15805 = EDGE_CURVE('',#12857,#12858,#10990,.T.) ;
#15806 = EDGE_CURVE('',#12857,#12859,#10991,.T.) ;
#15807 = EDGE_CURVE('',#12860,#12859,#10992,.T.) ;
#15808 = EDGE_CURVE('',#12860,#12858,#10993,.T.) ;
#15809 = EDGE_CURVE('',#12861,#12862,#10994,.T.) ;
#15810 = EDGE_CURVE('',#12861,#12863,#10995,.T.) ;
#15811 = EDGE_CURVE('',#12864,#12863,#10996,.T.) ;
#15812 = EDGE_CURVE('',#12864,#12862,#10997,.T.) ;
#15813 = EDGE_CURVE('',#12865,#12866,#10998,.T.) ;
#15814 = EDGE_CURVE('',#12865,#12867,#10999,.T.) ;
#15815 = EDGE_CURVE('',#12868,#12867,#11000,.T.) ;
#15816 = EDGE_CURVE('',#12868,#12866,#11001,.T.) ;
#15817 = EDGE_CURVE('',#12869,#12870,#11002,.T.) ;
#15818 = EDGE_CURVE('',#12871,#12870,#11003,.T.) ;
#15819 = EDGE_CURVE('',#12872,#12871,#11004,.T.) ;
#15820 = EDGE_CURVE('',#12869,#12872,#11005,.T.) ;
#15821 = EDGE_CURVE('',#12873,#12874,#11006,.T.) ;
#15822 = EDGE_CURVE('',#12875,#12874,#11007,.T.) ;
#15823 = EDGE_CURVE('',#12876,#12875,#11008,.T.) ;
#15824 = EDGE_CURVE('',#12873,#12876,#1191,.T.) ;
#15825 = EDGE_CURVE('',#12877,#12878,#11009,.T.) ;
#15826 = EDGE_CURVE('',#12879,#12878,#11010,.T.) ;
#15827 = EDGE_CURVE('',#12880,#12879,#11011,.T.) ;
#15828 = EDGE_CURVE('',#12877,#12880,#1192,.T.) ;
#15829 = EDGE_CURVE('',#12881,#12764,#11012,.T.) ;
#15830 = EDGE_CURVE('',#12882,#12881,#6325,.T.) ;
#15831 = EDGE_CURVE('',#12883,#12882,#11013,.T.) ;
#15832 = EDGE_CURVE('',#12883,#12884,#6326,.F.) ;
#15833 = EDGE_CURVE('',#12885,#12884,#11014,.T.) ;
#15834 = EDGE_CURVE('',#12885,#12886,#6327,.T.) ;
#15835 = EDGE_CURVE('',#12887,#12886,#11015,.T.) ;
#15836 = EDGE_CURVE('',#12887,#12888,#6328,.F.) ;
#15837 = EDGE_CURVE('',#12889,#12888,#11016,.T.) ;
#15838 = EDGE_CURVE('',#12889,#12890,#6329,.F.) ;
#15839 = EDGE_CURVE('',#12891,#12890,#11017,.T.) ;
#15840 = EDGE_CURVE('',#12891,#12807,#6330,.F.) ;
#15841 = EDGE_CURVE('',#12892,#12808,#11018,.T.) ;
#15842 = EDGE_CURVE('',#12892,#12667,#6331,.T.) ;
#15843 = EDGE_CURVE('',#12893,#12893,#11019,.F.) ;
#15844 = EDGE_CURVE('',#12894,#12894,#11020,.T.) ;
#15845 = EDGE_CURVE('',#12738,#12895,#6332,.F.) ;
#15846 = EDGE_CURVE('',#12896,#12895,#11021,.T.) ;
#15847 = EDGE_CURVE('',#12896,#12897,#6333,.F.) ;
#15848 = EDGE_CURVE('',#12813,#12897,#11022,.T.) ;
#15849 = EDGE_CURVE('',#12736,#12821,#6334,.T.) ;
#15850 = EDGE_CURVE('',#12733,#12820,#6335,.T.) ;
#15851 = EDGE_CURVE('',#12822,#12735,#6336,.T.) ;
#15852 = EDGE_CURVE('',#12872,#12683,#6337,.T.) ;
#15853 = EDGE_CURVE('',#12684,#12869,#6338,.T.) ;
#15854 = EDGE_CURVE('',#12685,#12871,#6339,.T.) ;
#15855 = EDGE_CURVE('',#12686,#12870,#6340,.T.) ;
#15856 = EDGE_CURVE('',#12876,#12679,#6341,.T.) ;
#15857 = EDGE_CURVE('',#12680,#12873,#6342,.T.) ;
#15858 = EDGE_CURVE('',#12681,#12875,#6343,.T.) ;
#15859 = EDGE_CURVE('',#12682,#12874,#6344,.T.) ;
#15860 = EDGE_CURVE('',#12880,#12677,#6345,.T.) ;
#15861 = EDGE_CURVE('',#12676,#12877,#6346,.T.) ;
#15862 = EDGE_CURVE('',#12678,#12879,#6347,.T.) ;
#15863 = EDGE_CURVE('',#12675,#12878,#6348,.T.) ;
#15864 = EDGE_CURVE('',#12734,#12819,#6349,.T.) ;
#15865 = EDGE_CURVE('',#12897,#12898,#6350,.T.) ;
#15866 = EDGE_CURVE('',#12898,#12814,#11023,.T.) ;
#15867 = EDGE_CURVE('',#12899,#12896,#6351,.T.) ;
#15868 = EDGE_CURVE('',#12898,#12899,#6352,.F.) ;
#15869 = EDGE_CURVE('',#12895,#12900,#6353,.T.) ;
#15870 = EDGE_CURVE('',#12900,#12899,#11024,.T.) ;
#15871 = EDGE_CURVE('',#12809,#12900,#6354,.T.) ;
#15872 = EDGE_CURVE('',#12815,#12673,#6355,.T.) ;
#15873 = EDGE_CURVE('',#12901,#12902,#11025,.T.) ;
#15874 = EDGE_CURVE('',#12902,#12903,#6356,.T.) ;
#15875 = EDGE_CURVE('',#12903,#12904,#11026,.T.) ;
#15876 = EDGE_CURVE('',#12904,#12901,#6357,.T.) ;
#15877 = EDGE_CURVE('',#12902,#12905,#6358,.F.) ;
#15878 = EDGE_CURVE('',#12906,#12905,#6359,.T.) ;
#15879 = EDGE_CURVE('',#12906,#12903,#6360,.T.) ;
#15880 = EDGE_CURVE('',#12901,#12907,#6361,.T.) ;
#15881 = EDGE_CURVE('',#12908,#12907,#6362,.T.) ;
#15882 = EDGE_CURVE('',#12908,#12909,#6363,.T.) ;
#15883 = EDGE_CURVE('',#12905,#12909,#11027,.T.) ;
#15884 = EDGE_CURVE('',#12910,#12906,#11028,.T.) ;
#15885 = EDGE_CURVE('',#12909,#12910,#6364,.T.) ;
#15886 = EDGE_CURVE('',#12817,#12911,#11029,.T.) ;
#15887 = EDGE_CURVE('',#12911,#12910,#6365,.T.) ;
#15888 = EDGE_CURVE('',#12668,#12908,#11030,.T.) ;
#15889 = EDGE_CURVE('',#12818,#12668,#6366,.F.) ;
#15890 = EDGE_CURVE('',#12766,#12892,#6367,.T.) ;
#15891 = EDGE_CURVE('',#12799,#12746,#6368,.T.) ;
#15892 = EDGE_CURVE('',#12745,#12800,#6369,.T.) ;
#15893 = EDGE_CURVE('',#12747,#12798,#6370,.T.) ;
#15894 = EDGE_CURVE('',#12749,#12796,#6371,.T.) ;
#15895 = EDGE_CURVE('',#12795,#12750,#6372,.T.) ;
#15896 = EDGE_CURVE('',#12797,#12748,#6373,.T.) ;
#15897 = EDGE_CURVE('',#12791,#12754,#6374,.T.) ;
#15898 = EDGE_CURVE('',#12753,#12792,#6375,.T.) ;
#15899 = EDGE_CURVE('',#12755,#12790,#6376,.T.) ;
#15900 = EDGE_CURVE('',#12751,#12794,#6377,.T.) ;
#15901 = EDGE_CURVE('',#12793,#12752,#6378,.T.) ;
#15902 = EDGE_CURVE('',#12789,#12756,#6379,.T.) ;
#15903 = EDGE_CURVE('',#12884,#12777,#6380,.T.) ;
#15904 = EDGE_CURVE('',#12776,#12885,#6381,.T.) ;
#15905 = EDGE_CURVE('',#12778,#12883,#6382,.T.) ;
#15906 = EDGE_CURVE('',#12882,#12779,#6383,.T.) ;
#15907 = EDGE_CURVE('',#12780,#12881,#6384,.T.) ;
#15908 = EDGE_CURVE('',#12774,#12887,#6385,.T.) ;
#15909 = EDGE_CURVE('',#12886,#12775,#6386,.T.) ;
#15910 = EDGE_CURVE('',#12888,#12773,#6387,.T.) ;
#15911 = EDGE_CURVE('',#12772,#12889,#6388,.T.) ;
#15912 = EDGE_CURVE('',#12770,#12891,#6389,.T.) ;
#15913 = EDGE_CURVE('',#12890,#12771,#6390,.T.) ;
#15914 = EDGE_CURVE('',#12907,#12671,#11031,.T.) ;
#15915 = EDGE_CURVE('',#12912,#12904,#6391,.T.) ;
#15916 = EDGE_CURVE('',#12912,#12816,#11032,.T.) ;
#15917 = EDGE_CURVE('',#12758,#12805,#6392,.T.) ;
#15918 = EDGE_CURVE('',#12757,#12804,#6393,.T.) ;
#15919 = EDGE_CURVE('',#12782,#12894,#6394,.T.) ;
#15920 = EDGE_CURVE('',#12853,#12688,#6395,.T.) ;
#15921 = EDGE_CURVE('',#12856,#12689,#6396,.T.) ;
#15922 = EDGE_CURVE('',#12855,#12690,#6397,.T.) ;
#15923 = EDGE_CURVE('',#12687,#12854,#6398,.T.) ;
#15924 = EDGE_CURVE('',#12716,#12823,#6399,.T.) ;
#15925 = EDGE_CURVE('',#12715,#12824,#6400,.T.) ;
#15926 = EDGE_CURVE('',#12717,#12852,#6401,.T.) ;
#15927 = EDGE_CURVE('',#12718,#12851,#6402,.T.) ;
#15928 = EDGE_CURVE('',#12719,#12850,#6403,.T.) ;
#15929 = EDGE_CURVE('',#12720,#12849,#6404,.T.) ;
#15930 = EDGE_CURVE('',#12847,#12713,#6405,.T.) ;
#15931 = EDGE_CURVE('',#12711,#12848,#6406,.T.) ;
#15932 = EDGE_CURVE('',#12714,#12846,#6407,.T.) ;
#15933 = EDGE_CURVE('',#12845,#12712,#6408,.T.) ;
#15934 = EDGE_CURVE('',#12843,#12709,#6409,.T.) ;
#15935 = EDGE_CURVE('',#12707,#12844,#6410,.T.) ;
#15936 = EDGE_CURVE('',#12710,#12842,#6411,.T.) ;
#15937 = EDGE_CURVE('',#12841,#12708,#6412,.T.) ;
#15938 = EDGE_CURVE('',#12839,#12705,#6413,.T.) ;
#15939 = EDGE_CURVE('',#12703,#12840,#6414,.T.) ;
#15940 = EDGE_CURVE('',#12706,#12838,#6415,.T.) ;
#15941 = EDGE_CURVE('',#12837,#12704,#6416,.T.) ;
#15942 = EDGE_CURVE('',#12835,#12701,#6417,.T.) ;
#15943 = EDGE_CURVE('',#12699,#12836,#6418,.T.) ;
#15944 = EDGE_CURVE('',#12702,#12834,#6419,.T.) ;
#15945 = EDGE_CURVE('',#12833,#12700,#6420,.T.) ;
#15946 = EDGE_CURVE('',#12831,#12697,#6421,.T.) ;
#15947 = EDGE_CURVE('',#12695,#12832,#6422,.T.) ;
#15948 = EDGE_CURVE('',#12698,#12830,#6423,.T.) ;
#15949 = EDGE_CURVE('',#12829,#12696,#6424,.T.) ;
#15950 = EDGE_CURVE('',#12827,#12693,#6425,.T.) ;
#15951 = EDGE_CURVE('',#12691,#12828,#6426,.T.) ;
#15952 = EDGE_CURVE('',#12694,#12826,#6427,.T.) ;
#15953 = EDGE_CURVE('',#12825,#12692,#6428,.T.) ;
#15954 = EDGE_CURVE('',#12912,#12911,#6429,.T.) ;
#15955 = EDGE_CURVE('',#12781,#12893,#6430,.T.) ;
#15956 = EDGE_CURVE('',#12857,#12722,#6431,.T.) ;
#15957 = EDGE_CURVE('',#12858,#12721,#6432,.T.) ;
#15958 = EDGE_CURVE('',#12860,#12723,#6433,.T.) ;
#15959 = EDGE_CURVE('',#12724,#12859,#6434,.T.) ;
#15960 = EDGE_CURVE('',#12861,#12726,#6435,.T.) ;
#15961 = EDGE_CURVE('',#12862,#12725,#6436,.T.) ;
#15962 = EDGE_CURVE('',#12864,#12727,#6437,.T.) ;
#15963 = EDGE_CURVE('',#12728,#12863,#6438,.T.) ;
#15964 = EDGE_CURVE('',#12865,#12730,#6439,.T.) ;
#15965 = EDGE_CURVE('',#12866,#12729,#6440,.T.) ;
#15966 = EDGE_CURVE('',#12868,#12731,#6441,.T.) ;
#15967 = EDGE_CURVE('',#12732,#12867,#6442,.T.) ;
#15968 = EDGE_CURVE('',#12913,#12914,#6443,.T.) ;
#15969 = EDGE_CURVE('',#12914,#12915,#1193,.T.) ;
#15970 = EDGE_CURVE('',#12915,#12916,#11033,.T.) ;
#15971 = EDGE_CURVE('',#12913,#12916,#1194,.F.) ;
#15972 = EDGE_CURVE('',#12917,#12918,#6444,.T.) ;
#15973 = EDGE_CURVE('',#12918,#12914,#1195,.T.) ;
#15974 = EDGE_CURVE('',#12917,#12913,#1196,.F.) ;
#15975 = EDGE_CURVE('',#12919,#12920,#6445,.T.) ;
#15976 = EDGE_CURVE('',#12920,#12918,#1197,.T.) ;
#15977 = EDGE_CURVE('',#12919,#12917,#1198,.F.) ;
#15978 = EDGE_CURVE('',#12921,#12922,#6446,.T.) ;
#15979 = EDGE_CURVE('',#12922,#12920,#1199,.T.) ;
#15980 = EDGE_CURVE('',#12921,#12919,#1200,.F.) ;
#15981 = EDGE_CURVE('',#12923,#12924,#6447,.T.) ;
#15982 = EDGE_CURVE('',#12925,#12923,#1201,.F.) ;
#15983 = EDGE_CURVE('',#12926,#12925,#11034,.T.) ;
#15984 = EDGE_CURVE('',#12926,#12924,#1202,.T.) ;
#15985 = EDGE_CURVE('',#12927,#12928,#6448,.T.) ;
#15986 = EDGE_CURVE('',#12929,#12928,#1203,.F.) ;
#15987 = EDGE_CURVE('',#12930,#12929,#11035,.T.) ;
#15988 = EDGE_CURVE('',#12927,#12930,#1204,.F.) ;
#15989 = EDGE_CURVE('',#12931,#12932,#6449,.T.) ;
#15990 = EDGE_CURVE('',#12928,#12932,#1205,.F.) ;
#15991 = EDGE_CURVE('',#12931,#12927,#1206,.F.) ;
#15992 = EDGE_CURVE('',#12933,#12934,#6450,.T.) ;
#15993 = EDGE_CURVE('',#12932,#12934,#1207,.F.) ;
#15994 = EDGE_CURVE('',#12933,#12931,#1208,.F.) ;
#15995 = EDGE_CURVE('',#12935,#12936,#6451,.T.) ;
#15996 = EDGE_CURVE('',#12934,#12936,#1209,.F.) ;
#15997 = EDGE_CURVE('',#12935,#12933,#1210,.F.) ;
#15998 = EDGE_CURVE('',#12937,#12938,#6452,.T.) ;
#15999 = EDGE_CURVE('',#12936,#12938,#1211,.F.) ;
#16000 = EDGE_CURVE('',#12937,#12935,#1212,.F.) ;
#16001 = EDGE_CURVE('',#12939,#12940,#6453,.T.) ;
#16002 = EDGE_CURVE('',#12941,#12939,#1213,.F.) ;
#16003 = EDGE_CURVE('',#12941,#12942,#11036,.T.) ;
#16004 = EDGE_CURVE('',#12940,#12942,#1214,.F.) ;
#16005 = EDGE_CURVE('',#12943,#12944,#6454,.T.) ;
#16006 = EDGE_CURVE('',#12943,#12926,#1215,.F.) ;
#16007 = EDGE_CURVE('',#12925,#12944,#1216,.T.) ;
#16008 = EDGE_CURVE('',#12945,#12930,#6455,.T.) ;
#16009 = EDGE_CURVE('',#12916,#12945,#1217,.T.) ;
#16010 = EDGE_CURVE('',#12930,#12915,#1218,.T.) ;
#16011 = EDGE_CURVE('',#12929,#12930,#11037,.T.) ;
#16012 = EDGE_CURVE('',#12945,#12929,#1219,.T.) ;
#16013 = EDGE_CURVE('',#12944,#12942,#1220,.T.) ;
#16014 = EDGE_CURVE('',#12942,#12941,#11038,.T.) ;
#16015 = EDGE_CURVE('',#12941,#12943,#1221,.F.) ;
#16016 = EDGE_CURVE('',#12938,#12940,#1222,.F.) ;
#16017 = EDGE_CURVE('',#12939,#12937,#1223,.F.) ;
#16018 = EDGE_CURVE('',#12924,#12922,#1224,.T.) ;
#16019 = EDGE_CURVE('',#12923,#12921,#1225,.F.) ;
#16020 = EDGE_CURVE('',#12946,#12947,#11039,.T.) ;
#16021 = EDGE_CURVE('',#12948,#12946,#764,.T.) ;
#16022 = EDGE_CURVE('',#12947,#12948,#765,.T.) ;
#16023 = EDGE_CURVE('',#12949,#12950,#11040,.T.) ;
#16024 = EDGE_CURVE('',#12949,#12951,#766,.T.) ;
#16025 = EDGE_CURVE('',#12951,#12950,#767,.T.) ;
#16026 = EDGE_CURVE('',#12950,#12952,#11041,.T.) ;
#16027 = EDGE_CURVE('',#12952,#12953,#11042,.T.) ;
#16028 = EDGE_CURVE('',#12953,#12954,#11043,.T.) ;
#16029 = EDGE_CURVE('',#12954,#12955,#11044,.T.) ;
#16030 = EDGE_CURVE('',#12955,#12949,#11045,.T.) ;
#16031 = EDGE_CURVE('',#12956,#12957,#6456,.T.) ;
#16032 = EDGE_CURVE('',#12957,#12958,#768,.T.) ;
#16033 = EDGE_CURVE('',#12958,#12959,#769,.T.) ;
#16034 = EDGE_CURVE('',#12960,#12959,#6457,.T.) ;
#16035 = EDGE_CURVE('',#12954,#12960,#770,.T.) ;
#16036 = EDGE_CURVE('',#12956,#12954,#771,.T.) ;
#16037 = EDGE_CURVE('',#12959,#12961,#772,.T.) ;
#16038 = EDGE_CURVE('',#12961,#12962,#773,.T.) ;
#16039 = EDGE_CURVE('',#12963,#12962,#6458,.T.) ;
#16040 = EDGE_CURVE('',#12955,#12963,#774,.T.) ;
#16041 = EDGE_CURVE('',#12960,#12955,#775,.T.) ;
#16042 = EDGE_CURVE('',#12962,#12947,#776,.T.) ;
#16043 = EDGE_CURVE('',#12951,#12948,#6459,.T.) ;
#16044 = EDGE_CURVE('',#12963,#12949,#777,.T.) ;
#16045 = EDGE_CURVE('',#12946,#12964,#778,.T.) ;
#16046 = EDGE_CURVE('',#12965,#12964,#6460,.T.) ;
#16047 = EDGE_CURVE('',#12950,#12965,#779,.T.) ;
#16048 = EDGE_CURVE('',#12964,#12966,#780,.T.) ;
#16049 = EDGE_CURVE('',#12966,#12967,#781,.T.) ;
#16050 = EDGE_CURVE('',#12968,#12967,#6461,.T.) ;
#16051 = EDGE_CURVE('',#12952,#12968,#782,.T.) ;
#16052 = EDGE_CURVE('',#12965,#12952,#783,.T.) ;
#16053 = EDGE_CURVE('',#12967,#12969,#784,.T.) ;
#16054 = EDGE_CURVE('',#12969,#12957,#785,.T.) ;
#16055 = EDGE_CURVE('',#12953,#12956,#786,.T.) ;
#16056 = EDGE_CURVE('',#12968,#12953,#787,.T.) ;
#16057 = EDGE_CURVE('',#12947,#12961,#11046,.T.) ;
#16058 = EDGE_CURVE('',#12961,#12958,#11047,.T.) ;
#16059 = EDGE_CURVE('',#12958,#12969,#11048,.T.) ;
#16060 = EDGE_CURVE('',#12969,#12966,#11049,.T.) ;
#16061 = EDGE_CURVE('',#12946,#12966,#11050,.T.) ;
#16062 = EDGE_CURVE('',#12970,#12971,#6462,.T.) ;
#16063 = EDGE_CURVE('',#12970,#12972,#1226,.T.) ;
#16064 = EDGE_CURVE('',#12972,#12971,#11051,.T.) ;
#16065 = EDGE_CURVE('',#12973,#12974,#6463,.T.) ;
#16066 = EDGE_CURVE('',#12973,#12970,#1227,.T.) ;
#16067 = EDGE_CURVE('',#12971,#12975,#11052,.T.) ;
#16068 = EDGE_CURVE('',#12974,#12975,#1228,.F.) ;
#16069 = EDGE_CURVE('',#12976,#12977,#6464,.T.) ;
#16070 = EDGE_CURVE('',#12976,#12973,#1229,.T.) ;
#16071 = EDGE_CURVE('',#12977,#12974,#1230,.F.) ;
#16072 = EDGE_CURVE('',#12978,#12979,#6465,.T.) ;
#16073 = EDGE_CURVE('',#12978,#12976,#1231,.T.) ;
#16074 = EDGE_CURVE('',#12979,#12977,#1232,.F.) ;
#16075 = EDGE_CURVE('',#12980,#12981,#6466,.T.) ;
#16076 = EDGE_CURVE('',#12980,#12978,#1233,.T.) ;
#16077 = EDGE_CURVE('',#12981,#12979,#1234,.F.) ;
#16078 = EDGE_CURVE('',#12982,#12983,#6467,.T.) ;
#16079 = EDGE_CURVE('',#12982,#12980,#1235,.T.) ;
#16080 = EDGE_CURVE('',#12983,#12981,#1236,.F.) ;
#16081 = EDGE_CURVE('',#12984,#12985,#6468,.T.) ;
#16082 = EDGE_CURVE('',#12986,#12984,#1237,.F.) ;
#16083 = EDGE_CURVE('',#12986,#12987,#11053,.T.) ;
#16084 = EDGE_CURVE('',#12987,#12988,#6469,.T.) ;
#16085 = EDGE_CURVE('',#12988,#12989,#11054,.T.) ;
#16086 = EDGE_CURVE('',#12989,#12988,#11055,.T.) ;
#16087 = EDGE_CURVE('',#12987,#12990,#11056,.T.) ;
#16088 = EDGE_CURVE('',#12985,#12990,#1238,.F.) ;
#16089 = EDGE_CURVE('',#12991,#12992,#6470,.T.) ;
#16090 = EDGE_CURVE('',#12984,#12991,#1239,.F.) ;
#16091 = EDGE_CURVE('',#12992,#12985,#1240,.F.) ;
#16092 = EDGE_CURVE('',#12993,#12994,#6471,.T.) ;
#16093 = EDGE_CURVE('',#12991,#12993,#1241,.F.) ;
#16094 = EDGE_CURVE('',#12994,#12992,#1242,.F.) ;
#16095 = EDGE_CURVE('',#12995,#12996,#6472,.T.) ;
#16096 = EDGE_CURVE('',#12993,#12995,#1243,.F.) ;
#16097 = EDGE_CURVE('',#12996,#12994,#1244,.F.) ;
#16098 = EDGE_CURVE('',#12997,#12998,#6473,.T.) ;
#16099 = EDGE_CURVE('',#12995,#12997,#1245,.F.) ;
#16100 = EDGE_CURVE('',#12998,#12996,#1246,.F.) ;
#16101 = EDGE_CURVE('',#12999,#12998,#1247,.F.) ;
#16102 = EDGE_CURVE('',#13000,#12999,#11057,.T.) ;
#16103 = EDGE_CURVE('',#12997,#13000,#1248,.F.) ;
#16104 = EDGE_CURVE('',#13001,#12983,#1249,.F.) ;
#16105 = EDGE_CURVE('',#13002,#13001,#11058,.T.) ;
#16106 = EDGE_CURVE('',#13002,#12982,#1250,.T.) ;
#16107 = EDGE_CURVE('',#13003,#13003,#11059,.T.) ;
#16108 = EDGE_CURVE('',#13003,#13004,#11060,.T.) ;
#16109 = EDGE_CURVE('',#13004,#13005,#11061,.T.) ;
#16110 = EDGE_CURVE('',#13005,#13004,#11062,.T.) ;
#16111 = EDGE_CURVE('',#13005,#12989,#6474,.T.) ;
#16112 = EDGE_CURVE('',#13006,#13007,#11063,.T.) ;
#16113 = EDGE_CURVE('',#13006,#13008,#6475,.T.) ;
#16114 = EDGE_CURVE('',#13008,#13009,#6476,.T.) ;
#16115 = EDGE_CURVE('',#13009,#13010,#6477,.T.) ;
#16116 = EDGE_CURVE('',#13011,#13010,#6478,.T.) ;
#16117 = EDGE_CURVE('',#13012,#13011,#11064,.T.) ;
#16118 = EDGE_CURVE('',#13012,#13013,#6479,.T.) ;
#16119 = EDGE_CURVE('',#13013,#13014,#6480,.T.) ;
#16120 = EDGE_CURVE('',#13014,#13015,#6481,.T.) ;
#16121 = EDGE_CURVE('',#13016,#13015,#6482,.T.) ;
#16122 = EDGE_CURVE('',#13017,#13016,#11065,.T.) ;
#16123 = EDGE_CURVE('',#13017,#13018,#6483,.T.) ;
#16124 = EDGE_CURVE('',#13018,#13019,#6484,.T.) ;
#16125 = EDGE_CURVE('',#13019,#13020,#6485,.T.) ;
#16126 = EDGE_CURVE('',#13021,#13020,#6486,.T.) ;
#16127 = EDGE_CURVE('',#13021,#13022,#11066,.T.) ;
#16128 = EDGE_CURVE('',#13022,#13023,#6487,.T.) ;
#16129 = EDGE_CURVE('',#13023,#13024,#6488,.T.) ;
#16130 = EDGE_CURVE('',#13024,#13025,#6489,.T.) ;
#16131 = EDGE_CURVE('',#13007,#13025,#6490,.T.) ;
#16132 = EDGE_CURVE('',#12999,#13026,#1251,.F.) ;
#16133 = EDGE_CURVE('',#13026,#13027,#6491,.T.) ;
#16134 = EDGE_CURVE('',#13027,#13027,#11067,.T.) ;
#16135 = EDGE_CURVE('',#13026,#13002,#1252,.F.) ;
#16136 = EDGE_CURVE('',#13001,#13000,#1253,.T.) ;
#16137 = EDGE_CURVE('',#13028,#13029,#6492,.T.) ;
#16138 = EDGE_CURVE('',#13029,#13030,#11068,.T.) ;
#16139 = EDGE_CURVE('',#13031,#13030,#788,.T.) ;
#16140 = EDGE_CURVE('',#13031,#13032,#789,.T.) ;
#16141 = EDGE_CURVE('',#13032,#13033,#790,.T.) ;
#16142 = EDGE_CURVE('',#13033,#13034,#791,.T.) ;
#16143 = EDGE_CURVE('',#13035,#13034,#11069,.T.) ;
#16144 = EDGE_CURVE('',#13036,#13035,#792,.T.) ;
#16145 = EDGE_CURVE('',#13036,#13037,#793,.T.) ;
#16146 = EDGE_CURVE('',#13037,#13038,#794,.T.) ;
#16147 = EDGE_CURVE('',#13038,#13039,#795,.T.) ;
#16148 = EDGE_CURVE('',#13040,#13039,#11070,.T.) ;
#16149 = EDGE_CURVE('',#13041,#13040,#796,.T.) ;
#16150 = EDGE_CURVE('',#13041,#13042,#797,.T.) ;
#16151 = EDGE_CURVE('',#13042,#13043,#798,.T.) ;
#16152 = EDGE_CURVE('',#13043,#13044,#799,.T.) ;
#16153 = EDGE_CURVE('',#13045,#13044,#11071,.T.) ;
#16154 = EDGE_CURVE('',#13046,#13045,#800,.T.) ;
#16155 = EDGE_CURVE('',#13046,#13047,#801,.T.) ;
#16156 = EDGE_CURVE('',#13047,#13048,#802,.T.) ;
#16157 = EDGE_CURVE('',#13048,#13049,#803,.T.) ;
#16158 = EDGE_CURVE('',#13049,#13029,#11072,.T.) ;
#16159 = EDGE_CURVE('',#13044,#13006,#122,.T.) ;
#16160 = EDGE_CURVE('',#13045,#13007,#123,.T.) ;
#16161 = EDGE_CURVE('',#13034,#13017,#124,.T.) ;
#16162 = EDGE_CURVE('',#13035,#13016,#125,.T.) ;
#16163 = EDGE_CURVE('',#13039,#13012,#126,.T.) ;
#16164 = EDGE_CURVE('',#13040,#13011,#127,.T.) ;
#16165 = EDGE_CURVE('',#13042,#13009,#6493,.T.) ;
#16166 = EDGE_CURVE('',#13043,#13008,#6494,.T.) ;
#16167 = EDGE_CURVE('',#13041,#13010,#6495,.T.) ;
#16168 = EDGE_CURVE('',#13038,#13013,#6496,.T.) ;
#16169 = EDGE_CURVE('',#13037,#13014,#6497,.T.) ;
#16170 = EDGE_CURVE('',#13036,#13015,#6498,.T.) ;
#16171 = EDGE_CURVE('',#13033,#13018,#6499,.T.) ;
#16172 = EDGE_CURVE('',#13032,#13019,#6500,.T.) ;
#16173 = EDGE_CURVE('',#13031,#13020,#6501,.T.) ;
#16174 = EDGE_CURVE('',#13030,#13021,#128,.T.) ;
#16175 = EDGE_CURVE('',#13049,#13022,#129,.T.) ;
#16176 = EDGE_CURVE('',#13048,#13023,#6502,.T.) ;
#16177 = EDGE_CURVE('',#13047,#13024,#6503,.T.) ;
#16178 = EDGE_CURVE('',#13046,#13025,#6504,.T.) ;
#16179 = EDGE_CURVE('',#12990,#12972,#1254,.T.) ;
#16180 = EDGE_CURVE('',#12975,#12986,#1255,.T.) ;
#16181 = EDGE_CURVE('',#13050,#13051,#6505,.T.) ;
#16182 = EDGE_CURVE('',#13051,#13052,#1256,.T.) ;
#16183 = EDGE_CURVE('',#13053,#13052,#11073,.T.) ;
#16184 = EDGE_CURVE('',#13050,#13053,#1257,.F.) ;
#16185 = EDGE_CURVE('',#13054,#13055,#6506,.T.) ;
#16186 = EDGE_CURVE('',#13055,#13056,#1258,.T.) ;
#16187 = EDGE_CURVE('',#13056,#13051,#1259,.T.) ;
#16188 = EDGE_CURVE('',#13054,#13050,#1260,.F.) ;
#16189 = EDGE_CURVE('',#13057,#13058,#6507,.T.) ;
#16190 = EDGE_CURVE('',#13059,#13057,#1261,.T.) ;
#16191 = EDGE_CURVE('',#13060,#13059,#1262,.T.) ;
#16192 = EDGE_CURVE('',#13061,#13060,#11074,.T.) ;
#16193 = EDGE_CURVE('',#13061,#13058,#1263,.T.) ;
#16194 = EDGE_CURVE('',#13062,#13063,#6508,.T.) ;
#16195 = EDGE_CURVE('',#13063,#13064,#1264,.T.) ;
#16196 = EDGE_CURVE('',#13065,#13064,#11075,.T.) ;
#16197 = EDGE_CURVE('',#13062,#13065,#1265,.F.) ;
#16198 = EDGE_CURVE('',#13066,#13067,#6509,.T.) ;
#16199 = EDGE_CURVE('',#13067,#13068,#1266,.T.) ;
#16200 = EDGE_CURVE('',#13068,#13063,#1267,.T.) ;
#16201 = EDGE_CURVE('',#13069,#13062,#1268,.F.) ;
#16202 = EDGE_CURVE('',#13066,#13069,#1269,.F.) ;
#16203 = EDGE_CURVE('',#13070,#13071,#6510,.T.) ;
#16204 = EDGE_CURVE('',#13072,#13070,#1270,.F.) ;
#16205 = EDGE_CURVE('',#13073,#13072,#1271,.T.) ;
#16206 = EDGE_CURVE('',#13074,#13073,#1272,.T.) ;
#16207 = EDGE_CURVE('',#13075,#13074,#11076,.T.) ;
#16208 = EDGE_CURVE('',#13075,#13076,#1273,.T.) ;
#16209 = EDGE_CURVE('',#13076,#13071,#1274,.T.) ;
#16210 = EDGE_CURVE('',#13077,#13078,#6511,.T.) ;
#16211 = EDGE_CURVE('',#13078,#13079,#1275,.T.) ;
#16212 = EDGE_CURVE('',#13080,#13079,#11077,.T.) ;
#16213 = EDGE_CURVE('',#13077,#13080,#1276,.F.) ;
#16214 = EDGE_CURVE('',#13081,#13082,#6512,.T.) ;
#16215 = EDGE_CURVE('',#13082,#13083,#1277,.T.) ;
#16216 = EDGE_CURVE('',#13083,#13078,#1278,.T.) ;
#16217 = EDGE_CURVE('',#13081,#13077,#1279,.F.) ;
#16218 = EDGE_CURVE('',#13084,#13085,#6513,.T.) ;
#16219 = EDGE_CURVE('',#13086,#13084,#1280,.T.) ;
#16220 = EDGE_CURVE('',#13087,#13086,#1281,.T.) ;
#16221 = EDGE_CURVE('',#13088,#13087,#11078,.T.) ;
#16222 = EDGE_CURVE('',#13088,#13089,#1282,.T.) ;
#16223 = EDGE_CURVE('',#13089,#13085,#1283,.T.) ;
#16224 = EDGE_CURVE('',#13090,#13091,#6514,.T.) ;
#16225 = EDGE_CURVE('',#13091,#13092,#1284,.T.) ;
#16226 = EDGE_CURVE('',#13093,#13092,#11079,.T.) ;
#16227 = EDGE_CURVE('',#13090,#13093,#1285,.F.) ;
#16228 = EDGE_CURVE('',#13094,#13095,#6515,.T.) ;
#16229 = EDGE_CURVE('',#13095,#13096,#1286,.T.) ;
#16230 = EDGE_CURVE('',#13096,#13091,#1287,.T.) ;
#16231 = EDGE_CURVE('',#13094,#13090,#1288,.F.) ;
#16232 = EDGE_CURVE('',#13097,#13098,#6516,.T.) ;
#16233 = EDGE_CURVE('',#13099,#13097,#1289,.T.) ;
#16234 = EDGE_CURVE('',#13100,#13099,#1290,.T.) ;
#16235 = EDGE_CURVE('',#13101,#13100,#11080,.T.) ;
#16236 = EDGE_CURVE('',#13101,#13098,#1291,.T.) ;
#16237 = EDGE_CURVE('',#13102,#13103,#6517,.T.) ;
#16238 = EDGE_CURVE('',#13104,#13103,#11081,.T.) ;
#16239 = EDGE_CURVE('',#13104,#13102,#1292,.T.) ;
#16240 = EDGE_CURVE('',#13105,#13106,#6518,.T.) ;
#16241 = EDGE_CURVE('',#13106,#13107,#1293,.T.) ;
#16242 = EDGE_CURVE('',#13103,#13107,#11082,.T.) ;
#16243 = EDGE_CURVE('',#13102,#13105,#1294,.F.) ;
#16244 = EDGE_CURVE('',#13108,#13109,#6519,.T.) ;
#16245 = EDGE_CURVE('',#13108,#13110,#1295,.F.) ;
#16246 = EDGE_CURVE('',#13110,#13111,#1296,.T.) ;
#16247 = EDGE_CURVE('',#13112,#13111,#11083,.T.) ;
#16248 = EDGE_CURVE('',#13112,#13113,#1297,.T.) ;
#16249 = EDGE_CURVE('',#13113,#13109,#1298,.T.) ;
#16250 = EDGE_CURVE('',#13114,#13115,#6520,.T.) ;
#16251 = EDGE_CURVE('',#13116,#13115,#11084,.T.) ;
#16252 = EDGE_CURVE('',#13116,#13114,#1299,.T.) ;
#16253 = EDGE_CURVE('',#13117,#13118,#6521,.T.) ;
#16254 = EDGE_CURVE('',#13118,#13119,#1300,.T.) ;
#16255 = EDGE_CURVE('',#13115,#13119,#11085,.T.) ;
#16256 = EDGE_CURVE('',#13114,#13117,#1301,.F.) ;
#16257 = EDGE_CURVE('',#13120,#13121,#6522,.T.) ;
#16258 = EDGE_CURVE('',#13120,#13122,#1302,.F.) ;
#16259 = EDGE_CURVE('',#13122,#13123,#1303,.T.) ;
#16260 = EDGE_CURVE('',#13124,#13123,#11086,.T.) ;
#16261 = EDGE_CURVE('',#13124,#13125,#1304,.T.) ;
#16262 = EDGE_CURVE('',#13125,#13121,#1305,.T.) ;
#16263 = EDGE_CURVE('',#13126,#13127,#6523,.T.) ;
#16264 = EDGE_CURVE('',#13128,#13127,#11087,.T.) ;
#16265 = EDGE_CURVE('',#13128,#13126,#1306,.T.) ;
#16266 = EDGE_CURVE('',#13129,#13130,#6524,.T.) ;
#16267 = EDGE_CURVE('',#13130,#13131,#1307,.T.) ;
#16268 = EDGE_CURVE('',#13127,#13131,#11088,.T.) ;
#16269 = EDGE_CURVE('',#13126,#13129,#1308,.F.) ;
#16270 = EDGE_CURVE('',#13132,#13133,#6525,.T.) ;
#16271 = EDGE_CURVE('',#13132,#13134,#1309,.F.) ;
#16272 = EDGE_CURVE('',#13134,#13135,#1310,.T.) ;
#16273 = EDGE_CURVE('',#13136,#13135,#11089,.T.) ;
#16274 = EDGE_CURVE('',#13136,#13137,#1311,.T.) ;
#16275 = EDGE_CURVE('',#13137,#13133,#1312,.T.) ;
#16276 = EDGE_CURVE('',#13138,#13139,#6526,.T.) ;
#16277 = EDGE_CURVE('',#13140,#13139,#11090,.T.) ;
#16278 = EDGE_CURVE('',#13140,#13138,#1313,.T.) ;
#16279 = EDGE_CURVE('',#13141,#13142,#6527,.T.) ;
#16280 = EDGE_CURVE('',#13142,#13143,#1314,.T.) ;
#16281 = EDGE_CURVE('',#13139,#13143,#11091,.T.) ;
#16282 = EDGE_CURVE('',#13138,#13141,#1315,.F.) ;
#16283 = EDGE_CURVE('',#13144,#13145,#6528,.T.) ;
#16284 = EDGE_CURVE('',#13144,#13146,#1316,.F.) ;
#16285 = EDGE_CURVE('',#13146,#13147,#1317,.T.) ;
#16286 = EDGE_CURVE('',#13148,#13147,#11092,.T.) ;
#16287 = EDGE_CURVE('',#13148,#13149,#1318,.T.) ;
#16288 = EDGE_CURVE('',#13149,#13145,#1319,.T.) ;
#16289 = EDGE_CURVE('',#13150,#13151,#6529,.T.) ;
#16290 = EDGE_CURVE('',#13151,#13152,#1320,.T.) ;
#16291 = EDGE_CURVE('',#13153,#13152,#11093,.T.) ;
#16292 = EDGE_CURVE('',#13150,#13153,#1321,.F.) ;
#16293 = EDGE_CURVE('',#13154,#13155,#6530,.T.) ;
#16294 = EDGE_CURVE('',#13155,#13156,#1322,.T.) ;
#16295 = EDGE_CURVE('',#13156,#13151,#1323,.T.) ;
#16296 = EDGE_CURVE('',#13154,#13150,#1324,.F.) ;
#16297 = EDGE_CURVE('',#13157,#13158,#6531,.T.) ;
#16298 = EDGE_CURVE('',#13159,#13157,#1325,.T.) ;
#16299 = EDGE_CURVE('',#13160,#13159,#1326,.T.) ;
#16300 = EDGE_CURVE('',#13161,#13160,#11094,.T.) ;
#16301 = EDGE_CURVE('',#13161,#13158,#1327,.T.) ;
#16302 = EDGE_CURVE('',#13162,#13163,#6532,.T.) ;
#16303 = EDGE_CURVE('',#13163,#13164,#1328,.T.) ;
#16304 = EDGE_CURVE('',#13165,#13164,#11095,.T.) ;
#16305 = EDGE_CURVE('',#13162,#13165,#1329,.F.) ;
#16306 = EDGE_CURVE('',#13166,#13167,#6533,.T.) ;
#16307 = EDGE_CURVE('',#13167,#13168,#1330,.T.) ;
#16308 = EDGE_CURVE('',#13168,#13163,#1331,.T.) ;
#16309 = EDGE_CURVE('',#13166,#13162,#1332,.F.) ;
#16310 = EDGE_CURVE('',#13169,#13170,#6534,.T.) ;
#16311 = EDGE_CURVE('',#13171,#13169,#1333,.T.) ;
#16312 = EDGE_CURVE('',#13172,#13171,#1334,.T.) ;
#16313 = EDGE_CURVE('',#13173,#13172,#11096,.T.) ;
#16314 = EDGE_CURVE('',#13173,#13174,#1335,.T.) ;
#16315 = EDGE_CURVE('',#13174,#13170,#1336,.T.) ;
#16316 = EDGE_CURVE('',#13175,#13176,#6535,.T.) ;
#16317 = EDGE_CURVE('',#13177,#13176,#11097,.T.) ;
#16318 = EDGE_CURVE('',#13177,#13175,#1337,.T.) ;
#16319 = EDGE_CURVE('',#13178,#13179,#6536,.T.) ;
#16320 = EDGE_CURVE('',#13179,#13180,#1338,.T.) ;
#16321 = EDGE_CURVE('',#13176,#13180,#11098,.T.) ;
#16322 = EDGE_CURVE('',#13175,#13178,#1339,.F.) ;
#16323 = EDGE_CURVE('',#13181,#13182,#6537,.T.) ;
#16324 = EDGE_CURVE('',#13181,#13183,#1340,.F.) ;
#16325 = EDGE_CURVE('',#13183,#13184,#1341,.T.) ;
#16326 = EDGE_CURVE('',#13185,#13184,#11099,.T.) ;
#16327 = EDGE_CURVE('',#13185,#13186,#1342,.T.) ;
#16328 = EDGE_CURVE('',#13186,#13182,#1343,.T.) ;
#16329 = EDGE_CURVE('',#13187,#13188,#6538,.T.) ;
#16330 = EDGE_CURVE('',#13189,#13188,#11100,.T.) ;
#16331 = EDGE_CURVE('',#13189,#13187,#1344,.T.) ;
#16332 = EDGE_CURVE('',#13190,#13191,#6539,.T.) ;
#16333 = EDGE_CURVE('',#13191,#13192,#1345,.T.) ;
#16334 = EDGE_CURVE('',#13188,#13192,#11101,.T.) ;
#16335 = EDGE_CURVE('',#13187,#13190,#1346,.F.) ;
#16336 = EDGE_CURVE('',#13193,#13194,#6540,.T.) ;
#16337 = EDGE_CURVE('',#13193,#13195,#1347,.F.) ;
#16338 = EDGE_CURVE('',#13195,#13196,#1348,.T.) ;
#16339 = EDGE_CURVE('',#13197,#13196,#11102,.T.) ;
#16340 = EDGE_CURVE('',#13197,#13198,#1349,.T.) ;
#16341 = EDGE_CURVE('',#13198,#13194,#1350,.T.) ;
#16342 = EDGE_CURVE('',#13199,#13200,#6541,.T.) ;
#16343 = EDGE_CURVE('',#13200,#13201,#1351,.T.) ;
#16344 = EDGE_CURVE('',#13202,#13201,#11103,.T.) ;
#16345 = EDGE_CURVE('',#13199,#13202,#1352,.F.) ;
#16346 = EDGE_CURVE('',#13203,#13204,#6542,.T.) ;
#16347 = EDGE_CURVE('',#13204,#13205,#1353,.T.) ;
#16348 = EDGE_CURVE('',#13205,#13200,#1354,.T.) ;
#16349 = EDGE_CURVE('',#13203,#13199,#1355,.F.) ;
#16350 = EDGE_CURVE('',#13206,#13207,#6543,.T.) ;
#16351 = EDGE_CURVE('',#13208,#13206,#1356,.T.) ;
#16352 = EDGE_CURVE('',#13209,#13208,#1357,.T.) ;
#16353 = EDGE_CURVE('',#13210,#13209,#11104,.T.) ;
#16354 = EDGE_CURVE('',#13210,#13207,#1358,.T.) ;
#16355 = EDGE_CURVE('',#13211,#13212,#6544,.T.) ;
#16356 = EDGE_CURVE('',#13212,#13213,#1359,.T.) ;
#16357 = EDGE_CURVE('',#13214,#13213,#11105,.T.) ;
#16358 = EDGE_CURVE('',#13211,#13214,#1360,.F.) ;
#16359 = EDGE_CURVE('',#13215,#13216,#6545,.T.) ;
#16360 = EDGE_CURVE('',#13216,#13217,#1361,.T.) ;
#16361 = EDGE_CURVE('',#13217,#13212,#1362,.T.) ;
#16362 = EDGE_CURVE('',#13215,#13211,#1363,.F.) ;
#16363 = EDGE_CURVE('',#13218,#13219,#6546,.T.) ;
#16364 = EDGE_CURVE('',#13220,#13218,#1364,.T.) ;
#16365 = EDGE_CURVE('',#13221,#13220,#1365,.T.) ;
#16366 = EDGE_CURVE('',#13222,#13221,#11106,.T.) ;
#16367 = EDGE_CURVE('',#13222,#13219,#1366,.T.) ;
#16368 = EDGE_CURVE('',#13223,#13224,#6547,.T.) ;
#16369 = EDGE_CURVE('',#13225,#13224,#11107,.T.) ;
#16370 = EDGE_CURVE('',#13225,#13223,#1367,.T.) ;
#16371 = EDGE_CURVE('',#13226,#13227,#6548,.T.) ;
#16372 = EDGE_CURVE('',#13227,#13228,#1368,.T.) ;
#16373 = EDGE_CURVE('',#13224,#13228,#11108,.T.) ;
#16374 = EDGE_CURVE('',#13223,#13226,#1369,.F.) ;
#16375 = EDGE_CURVE('',#13229,#13230,#6549,.T.) ;
#16376 = EDGE_CURVE('',#13229,#13231,#1370,.F.) ;
#16377 = EDGE_CURVE('',#13231,#13232,#1371,.T.) ;
#16378 = EDGE_CURVE('',#13233,#13232,#11109,.T.) ;
#16379 = EDGE_CURVE('',#13233,#13234,#1372,.T.) ;
#16380 = EDGE_CURVE('',#13234,#13230,#1373,.T.) ;
#16381 = EDGE_CURVE('',#13235,#13236,#6550,.T.) ;
#16382 = EDGE_CURVE('',#13237,#13236,#11110,.T.) ;
#16383 = EDGE_CURVE('',#13237,#13235,#1374,.T.) ;
#16384 = EDGE_CURVE('',#13238,#13239,#6551,.T.) ;
#16385 = EDGE_CURVE('',#13239,#13240,#1375,.T.) ;
#16386 = EDGE_CURVE('',#13236,#13240,#11111,.T.) ;
#16387 = EDGE_CURVE('',#13235,#13238,#1376,.F.) ;
#16388 = EDGE_CURVE('',#13241,#13242,#6552,.T.) ;
#16389 = EDGE_CURVE('',#13241,#13243,#1377,.F.) ;
#16390 = EDGE_CURVE('',#13243,#13244,#1378,.T.) ;
#16391 = EDGE_CURVE('',#13245,#13244,#11112,.T.) ;
#16392 = EDGE_CURVE('',#13245,#13246,#1379,.T.) ;
#16393 = EDGE_CURVE('',#13246,#13242,#1380,.T.) ;
#16394 = EDGE_CURVE('',#13242,#13239,#1381,.T.) ;
#16395 = EDGE_CURVE('',#13238,#13241,#1382,.F.) ;
#16396 = EDGE_CURVE('',#13230,#13227,#1383,.T.) ;
#16397 = EDGE_CURVE('',#13226,#13229,#1384,.F.) ;
#16398 = EDGE_CURVE('',#13219,#13216,#1385,.T.) ;
#16399 = EDGE_CURVE('',#13218,#13215,#1386,.F.) ;
#16400 = EDGE_CURVE('',#13207,#13204,#1387,.T.) ;
#16401 = EDGE_CURVE('',#13206,#13203,#1388,.F.) ;
#16402 = EDGE_CURVE('',#13194,#13191,#1389,.T.) ;
#16403 = EDGE_CURVE('',#13190,#13193,#1390,.F.) ;
#16404 = EDGE_CURVE('',#13182,#13179,#1391,.T.) ;
#16405 = EDGE_CURVE('',#13178,#13181,#1392,.F.) ;
#16406 = EDGE_CURVE('',#13170,#13247,#1393,.T.) ;
#16407 = EDGE_CURVE('',#13247,#13167,#1394,.T.) ;
#16408 = EDGE_CURVE('',#13169,#13166,#1395,.F.) ;
#16409 = EDGE_CURVE('',#13158,#13155,#1396,.T.) ;
#16410 = EDGE_CURVE('',#13157,#13154,#1397,.F.) ;
#16411 = EDGE_CURVE('',#13145,#13142,#1398,.T.) ;
#16412 = EDGE_CURVE('',#13141,#13144,#1399,.F.) ;
#16413 = EDGE_CURVE('',#13133,#13130,#1400,.T.) ;
#16414 = EDGE_CURVE('',#13129,#13132,#1401,.F.) ;
#16415 = EDGE_CURVE('',#13121,#13118,#1402,.T.) ;
#16416 = EDGE_CURVE('',#13117,#13120,#1403,.F.) ;
#16417 = EDGE_CURVE('',#13109,#13106,#1404,.T.) ;
#16418 = EDGE_CURVE('',#13105,#13108,#1405,.F.) ;
#16419 = EDGE_CURVE('',#13098,#13095,#1406,.T.) ;
#16420 = EDGE_CURVE('',#13097,#13094,#1407,.F.) ;
#16421 = EDGE_CURVE('',#13085,#13248,#1408,.T.) ;
#16422 = EDGE_CURVE('',#13248,#13082,#1409,.T.) ;
#16423 = EDGE_CURVE('',#13084,#13081,#1410,.F.) ;
#16424 = EDGE_CURVE('',#13071,#13067,#1411,.T.) ;
#16425 = EDGE_CURVE('',#13070,#13066,#1412,.F.) ;
#16426 = EDGE_CURVE('',#13058,#13055,#1413,.T.) ;
#16427 = EDGE_CURVE('',#13057,#13054,#1414,.F.) ;
#16428 = EDGE_CURVE('',#13249,#13250,#11113,.T.) ;
#16429 = EDGE_CURVE('',#13249,#13251,#6553,.T.) ;
#16430 = EDGE_CURVE('',#13251,#13252,#11114,.T.) ;
#16431 = EDGE_CURVE('',#13252,#13250,#6554,.T.) ;
#16432 = EDGE_CURVE('',#13253,#13254,#11115,.T.) ;
#16433 = EDGE_CURVE('',#13253,#13255,#6555,.T.) ;
#16434 = EDGE_CURVE('',#13256,#13255,#11116,.T.) ;
#16435 = EDGE_CURVE('',#13256,#13254,#6556,.T.) ;
#16436 = EDGE_CURVE('',#13257,#13258,#11117,.T.) ;
#16437 = EDGE_CURVE('',#13257,#13259,#6557,.T.) ;
#16438 = EDGE_CURVE('',#13260,#13259,#11118,.T.) ;
#16439 = EDGE_CURVE('',#13260,#13258,#6558,.T.) ;
#16440 = EDGE_CURVE('',#13261,#13262,#11119,.T.) ;
#16441 = EDGE_CURVE('',#13261,#13263,#6559,.T.) ;
#16442 = EDGE_CURVE('',#13264,#13263,#11120,.T.) ;
#16443 = EDGE_CURVE('',#13264,#13262,#6560,.T.) ;
#16444 = EDGE_CURVE('',#13265,#13266,#11121,.T.) ;
#16445 = EDGE_CURVE('',#13265,#13267,#6561,.T.) ;
#16446 = EDGE_CURVE('',#13268,#13267,#11122,.T.) ;
#16447 = EDGE_CURVE('',#13268,#13266,#6562,.T.) ;
#16448 = EDGE_CURVE('',#13269,#13250,#6563,.T.) ;
#16449 = EDGE_CURVE('',#13270,#13269,#11123,.T.) ;
#16450 = EDGE_CURVE('',#13258,#13270,#6564,.T.) ;
#16451 = EDGE_CURVE('',#13271,#13260,#6565,.T.) ;
#16452 = EDGE_CURVE('',#13272,#13271,#11124,.T.) ;
#16453 = EDGE_CURVE('',#13273,#13272,#6566,.T.) ;
#16454 = EDGE_CURVE('',#13274,#13273,#11125,.T.) ;
#16455 = EDGE_CURVE('',#13263,#13274,#6567,.T.) ;
#16456 = EDGE_CURVE('',#13249,#13261,#6568,.T.) ;
#16457 = EDGE_CURVE('',#13275,#13276,#11126,.T.) ;
#16458 = EDGE_CURVE('',#13275,#13277,#6569,.T.) ;
#16459 = EDGE_CURVE('',#13278,#13277,#11127,.T.) ;
#16460 = EDGE_CURVE('',#13276,#13278,#6570,.T.) ;
#16461 = EDGE_CURVE('',#13279,#13280,#11128,.T.) ;
#16462 = EDGE_CURVE('',#13280,#13281,#6571,.T.) ;
#16463 = EDGE_CURVE('',#13282,#13281,#11129,.T.) ;
#16464 = EDGE_CURVE('',#13282,#13279,#6572,.T.) ;
#16465 = EDGE_CURVE('',#13257,#13254,#6573,.T.) ;
#16466 = EDGE_CURVE('',#13283,#13270,#6574,.T.) ;
#16467 = EDGE_CURVE('',#13283,#13284,#6575,.F.) ;
#16468 = EDGE_CURVE('',#13284,#13285,#11130,.F.) ;
#16469 = EDGE_CURVE('',#13285,#13286,#6576,.T.) ;
#16470 = EDGE_CURVE('',#13287,#13286,#6577,.T.) ;
#16471 = EDGE_CURVE('',#13287,#13288,#6578,.F.) ;
#16472 = EDGE_CURVE('',#13288,#13289,#11131,.F.) ;
#16473 = EDGE_CURVE('',#13289,#13290,#6579,.T.) ;
#16474 = EDGE_CURVE('',#13291,#13290,#6580,.T.) ;
#16475 = EDGE_CURVE('',#13292,#13291,#6581,.T.) ;
#16476 = EDGE_CURVE('',#13293,#13292,#6582,.T.) ;
#16477 = EDGE_CURVE('',#13253,#13293,#6583,.T.) ;
#16478 = EDGE_CURVE('',#13294,#13295,#6584,.T.) ;
#16479 = EDGE_CURVE('',#13296,#13295,#6585,.T.) ;
#16480 = EDGE_CURVE('',#13296,#13297,#6586,.T.) ;
#16481 = EDGE_CURVE('',#13298,#13297,#6587,.T.) ;
#16482 = EDGE_CURVE('',#13298,#13299,#6588,.T.) ;
#16483 = EDGE_CURVE('',#13300,#13299,#6589,.T.) ;
#16484 = EDGE_CURVE('',#13301,#13300,#11132,.T.) ;
#16485 = EDGE_CURVE('',#13302,#13301,#6590,.T.) ;
#16486 = EDGE_CURVE('',#13303,#13302,#11133,.T.) ;
#16487 = EDGE_CURVE('',#13304,#13303,#6591,.T.) ;
#16488 = EDGE_CURVE('',#13304,#13305,#6592,.T.) ;
#16489 = EDGE_CURVE('',#13306,#13305,#6593,.T.) ;
#16490 = EDGE_CURVE('',#13306,#13307,#6594,.T.) ;
#16491 = EDGE_CURVE('',#13294,#13307,#6595,.T.) ;
#16492 = EDGE_CURVE('',#13152,#13308,#1415,.T.) ;
#16493 = EDGE_CURVE('',#13308,#13189,#1416,.T.) ;
#16494 = EDGE_CURVE('',#13192,#13153,#1417,.T.) ;
#16495 = EDGE_CURVE('',#13164,#13309,#1418,.T.) ;
#16496 = EDGE_CURVE('',#13309,#13177,#1419,.T.) ;
#16497 = EDGE_CURVE('',#13180,#13165,#1420,.T.) ;
#16498 = EDGE_CURVE('',#13310,#13310,#11134,.T.) ;
#16499 = EDGE_CURVE('',#13311,#13312,#6596,.T.) ;
#16500 = EDGE_CURVE('',#13313,#13311,#6597,.T.) ;
#16501 = EDGE_CURVE('',#13314,#13313,#6598,.T.) ;
#16502 = EDGE_CURVE('',#13312,#13314,#6599,.T.) ;
#16503 = EDGE_CURVE('',#13315,#13316,#6600,.T.) ;
#16504 = EDGE_CURVE('',#13317,#13315,#6601,.T.) ;
#16505 = EDGE_CURVE('',#13318,#13317,#6602,.T.) ;
#16506 = EDGE_CURVE('',#13316,#13318,#6603,.T.) ;
#16507 = EDGE_CURVE('',#13319,#13320,#6604,.T.) ;
#16508 = EDGE_CURVE('',#13321,#13319,#6605,.T.) ;
#16509 = EDGE_CURVE('',#13322,#13321,#6606,.T.) ;
#16510 = EDGE_CURVE('',#13320,#13322,#6607,.T.) ;
#16511 = EDGE_CURVE('',#13323,#13323,#11135,.T.) ;
#16512 = EDGE_CURVE('',#13324,#13325,#11136,.T.) ;
#16513 = EDGE_CURVE('',#13324,#13326,#6608,.T.) ;
#16514 = EDGE_CURVE('',#13326,#13327,#11137,.T.) ;
#16515 = EDGE_CURVE('',#13327,#13325,#6609,.T.) ;
#16516 = EDGE_CURVE('',#13265,#13262,#6610,.T.) ;
#16517 = EDGE_CURVE('',#13328,#13266,#6611,.T.) ;
#16518 = EDGE_CURVE('',#13329,#13328,#6612,.T.) ;
#16519 = EDGE_CURVE('',#13325,#13329,#6613,.T.) ;
#16520 = EDGE_CURVE('',#13327,#13330,#6614,.F.) ;
#16521 = EDGE_CURVE('',#13330,#13331,#11138,.F.) ;
#16522 = EDGE_CURVE('',#13331,#13332,#6615,.F.) ;
#16523 = EDGE_CURVE('',#13333,#13332,#6616,.T.) ;
#16524 = EDGE_CURVE('',#13333,#13334,#6617,.F.) ;
#16525 = EDGE_CURVE('',#13334,#13335,#11139,.F.) ;
#16526 = EDGE_CURVE('',#13335,#13336,#6618,.F.) ;
#16527 = EDGE_CURVE('',#13337,#13336,#6619,.T.) ;
#16528 = EDGE_CURVE('',#13337,#13338,#6620,.T.) ;
#16529 = EDGE_CURVE('',#13338,#13339,#11140,.F.) ;
#16530 = EDGE_CURVE('',#13339,#13340,#6621,.F.) ;
#16531 = EDGE_CURVE('',#13341,#13340,#6622,.T.) ;
#16532 = EDGE_CURVE('',#13341,#13342,#6623,.T.) ;
#16533 = EDGE_CURVE('',#13342,#13343,#11141,.F.) ;
#16534 = EDGE_CURVE('',#13343,#13251,#6624,.F.) ;
#16535 = EDGE_CURVE('',#13344,#13344,#11142,.T.) ;
#16536 = EDGE_CURVE('',#13345,#13346,#6625,.T.) ;
#16537 = EDGE_CURVE('',#13347,#13345,#6626,.T.) ;
#16538 = EDGE_CURVE('',#13348,#13347,#6627,.T.) ;
#16539 = EDGE_CURVE('',#13346,#13348,#6628,.T.) ;
#16540 = EDGE_CURVE('',#13349,#13350,#6629,.T.) ;
#16541 = EDGE_CURVE('',#13351,#13349,#6630,.T.) ;
#16542 = EDGE_CURVE('',#13352,#13351,#6631,.T.) ;
#16543 = EDGE_CURVE('',#13350,#13352,#6632,.T.) ;
#16544 = EDGE_CURVE('',#13353,#13354,#6633,.T.) ;
#16545 = EDGE_CURVE('',#13355,#13353,#6634,.T.) ;
#16546 = EDGE_CURVE('',#13356,#13355,#6635,.T.) ;
#16547 = EDGE_CURVE('',#13354,#13356,#6636,.T.) ;
#16548 = EDGE_CURVE('',#13357,#13358,#6637,.T.) ;
#16549 = EDGE_CURVE('',#13359,#13357,#6638,.T.) ;
#16550 = EDGE_CURVE('',#13360,#13359,#6639,.T.) ;
#16551 = EDGE_CURVE('',#13358,#13360,#6640,.T.) ;
#16552 = EDGE_CURVE('',#13361,#13361,#11143,.T.) ;
#16553 = EDGE_CURVE('',#13213,#13362,#1421,.T.) ;
#16554 = EDGE_CURVE('',#13362,#13225,#1422,.T.) ;
#16555 = EDGE_CURVE('',#13228,#13214,#1423,.T.) ;
#16556 = EDGE_CURVE('',#13201,#13363,#1424,.T.) ;
#16557 = EDGE_CURVE('',#13363,#13237,#1425,.T.) ;
#16558 = EDGE_CURVE('',#13240,#13202,#1426,.T.) ;
#16559 = EDGE_CURVE('',#13364,#13365,#6641,.T.) ;
#16560 = EDGE_CURVE('',#13366,#13365,#11144,.T.) ;
#16561 = EDGE_CURVE('',#13366,#13367,#6642,.T.) ;
#16562 = EDGE_CURVE('',#13368,#13367,#11145,.T.) ;
#16563 = EDGE_CURVE('',#13368,#13369,#6643,.T.) ;
#16564 = EDGE_CURVE('',#13370,#13369,#11146,.T.) ;
#16565 = EDGE_CURVE('',#13370,#13371,#6644,.T.) ;
#16566 = EDGE_CURVE('',#13364,#13371,#11147,.T.) ;
#16567 = EDGE_CURVE('',#13372,#13373,#6645,.T.) ;
#16568 = EDGE_CURVE('',#13374,#13373,#6646,.T.) ;
#16569 = EDGE_CURVE('',#13374,#13375,#6647,.T.) ;
#16570 = EDGE_CURVE('',#13376,#13375,#6648,.T.) ;
#16571 = EDGE_CURVE('',#13376,#13377,#6649,.T.) ;
#16572 = EDGE_CURVE('',#13378,#13377,#6650,.T.) ;
#16573 = EDGE_CURVE('',#13379,#13378,#11148,.T.) ;
#16574 = EDGE_CURVE('',#13380,#13379,#6651,.T.) ;
#16575 = EDGE_CURVE('',#13381,#13380,#11149,.T.) ;
#16576 = EDGE_CURVE('',#13372,#13381,#6652,.T.) ;
#16577 = EDGE_CURVE('',#13382,#13255,#6653,.T.) ;
#16578 = EDGE_CURVE('',#13383,#13382,#6654,.T.) ;
#16579 = EDGE_CURVE('',#13384,#13383,#6655,.T.) ;
#16580 = EDGE_CURVE('',#13384,#13385,#6656,.T.) ;
#16581 = EDGE_CURVE('',#13385,#13386,#6657,.T.) ;
#16582 = EDGE_CURVE('',#13386,#13387,#11150,.T.) ;
#16583 = EDGE_CURVE('',#13388,#13387,#6658,.T.) ;
#16584 = EDGE_CURVE('',#13389,#13388,#6659,.T.) ;
#16585 = EDGE_CURVE('',#13389,#13390,#6660,.T.) ;
#16586 = EDGE_CURVE('',#13390,#13391,#11151,.T.) ;
#16587 = EDGE_CURVE('',#13391,#13392,#6661,.T.) ;
#16588 = EDGE_CURVE('',#13392,#13271,#6662,.T.) ;
#16589 = EDGE_CURVE('',#13256,#13259,#6663,.T.) ;
#16590 = EDGE_CURVE('',#13393,#13393,#11152,.T.) ;
#16591 = EDGE_CURVE('',#13394,#13395,#6664,.T.) ;
#16592 = EDGE_CURVE('',#13396,#13394,#6665,.T.) ;
#16593 = EDGE_CURVE('',#13397,#13396,#6666,.T.) ;
#16594 = EDGE_CURVE('',#13395,#13397,#6667,.T.) ;
#16595 = EDGE_CURVE('',#13398,#13399,#6668,.T.) ;
#16596 = EDGE_CURVE('',#13400,#13398,#6669,.T.) ;
#16597 = EDGE_CURVE('',#13401,#13400,#6670,.T.) ;
#16598 = EDGE_CURVE('',#13399,#13401,#6671,.T.) ;
#16599 = EDGE_CURVE('',#13402,#13403,#6672,.T.) ;
#16600 = EDGE_CURVE('',#13404,#13402,#6673,.T.) ;
#16601 = EDGE_CURVE('',#13405,#13404,#6674,.T.) ;
#16602 = EDGE_CURVE('',#13403,#13405,#6675,.T.) ;
#16603 = EDGE_CURVE('',#13406,#13407,#11153,.T.) ;
#16604 = EDGE_CURVE('',#13408,#13407,#6676,.T.) ;
#16605 = EDGE_CURVE('',#13408,#13409,#11154,.T.) ;
#16606 = EDGE_CURVE('',#13410,#13409,#6677,.T.) ;
#16607 = EDGE_CURVE('',#13411,#13410,#6678,.T.) ;
#16608 = EDGE_CURVE('',#13406,#13411,#6679,.T.) ;
#16609 = EDGE_CURVE('',#13412,#13412,#11155,.T.) ;
#16610 = EDGE_CURVE('',#13196,#13161,#1427,.T.) ;
#16611 = EDGE_CURVE('',#13160,#13413,#1428,.T.) ;
#16612 = EDGE_CURVE('',#13413,#13197,#1429,.T.) ;
#16613 = EDGE_CURVE('',#13184,#13173,#1430,.T.) ;
#16614 = EDGE_CURVE('',#13172,#13414,#1431,.T.) ;
#16615 = EDGE_CURVE('',#13414,#13185,#1432,.T.) ;
#16616 = EDGE_CURVE('',#13415,#13274,#6680,.T.) ;
#16617 = EDGE_CURVE('',#13415,#13416,#6681,.T.) ;
#16618 = EDGE_CURVE('',#13416,#13417,#11156,.T.) ;
#16619 = EDGE_CURVE('',#13417,#13418,#6682,.T.) ;
#16620 = EDGE_CURVE('',#13418,#13419,#6683,.T.) ;
#16621 = EDGE_CURVE('',#13419,#13420,#6684,.T.) ;
#16622 = EDGE_CURVE('',#13420,#13421,#11157,.T.) ;
#16623 = EDGE_CURVE('',#13422,#13421,#6685,.T.) ;
#16624 = EDGE_CURVE('',#13423,#13422,#6686,.T.) ;
#16625 = EDGE_CURVE('',#13423,#13424,#6687,.T.) ;
#16626 = EDGE_CURVE('',#13424,#13425,#11158,.T.) ;
#16627 = EDGE_CURVE('',#13425,#13426,#6688,.T.) ;
#16628 = EDGE_CURVE('',#13427,#13426,#6689,.T.) ;
#16629 = EDGE_CURVE('',#13427,#13428,#6690,.T.) ;
#16630 = EDGE_CURVE('',#13428,#13429,#11159,.T.) ;
#16631 = EDGE_CURVE('',#13429,#13430,#6691,.T.) ;
#16632 = EDGE_CURVE('',#13431,#13430,#6692,.T.) ;
#16633 = EDGE_CURVE('',#13432,#13431,#6693,.T.) ;
#16634 = EDGE_CURVE('',#13433,#13432,#6694,.T.) ;
#16635 = EDGE_CURVE('',#13268,#13433,#6695,.T.) ;
#16636 = EDGE_CURVE('',#13264,#13267,#6696,.T.) ;
#16637 = EDGE_CURVE('',#13434,#13435,#11160,.T.) ;
#16638 = EDGE_CURVE('',#13436,#13434,#6697,.T.) ;
#16639 = EDGE_CURVE('',#13437,#13436,#11161,.T.) ;
#16640 = EDGE_CURVE('',#13438,#13437,#6698,.T.) ;
#16641 = EDGE_CURVE('',#13439,#13438,#11162,.T.) ;
#16642 = EDGE_CURVE('',#13440,#13439,#6699,.T.) ;
#16643 = EDGE_CURVE('',#13441,#13440,#11163,.T.) ;
#16644 = EDGE_CURVE('',#13435,#13441,#6700,.T.) ;
#16645 = EDGE_CURVE('',#13232,#13222,#1433,.T.) ;
#16646 = EDGE_CURVE('',#13221,#13442,#1434,.T.) ;
#16647 = EDGE_CURVE('',#13442,#13233,#1435,.T.) ;
#16648 = EDGE_CURVE('',#13244,#13210,#1436,.T.) ;
#16649 = EDGE_CURVE('',#13209,#13443,#1437,.T.) ;
#16650 = EDGE_CURVE('',#13443,#13245,#1438,.T.) ;
#16651 = EDGE_CURVE('',#13444,#13445,#11164,.T.) ;
#16652 = EDGE_CURVE('',#13446,#13445,#6701,.T.) ;
#16653 = EDGE_CURVE('',#13446,#13447,#11165,.T.) ;
#16654 = EDGE_CURVE('',#13448,#13447,#6702,.T.) ;
#16655 = EDGE_CURVE('',#13449,#13448,#6703,.T.) ;
#16656 = EDGE_CURVE('',#13444,#13449,#6704,.T.) ;
#16657 = EDGE_CURVE('',#13450,#13451,#6705,.T.) ;
#16658 = EDGE_CURVE('',#13452,#13450,#6706,.T.) ;
#16659 = EDGE_CURVE('',#13453,#13452,#6707,.T.) ;
#16660 = EDGE_CURVE('',#13451,#13453,#6708,.T.) ;
#16661 = EDGE_CURVE('',#13454,#13455,#6709,.T.) ;
#16662 = EDGE_CURVE('',#13456,#13454,#6710,.T.) ;
#16663 = EDGE_CURVE('',#13457,#13456,#6711,.T.) ;
#16664 = EDGE_CURVE('',#13455,#13457,#6712,.T.) ;
#16665 = EDGE_CURVE('',#13458,#13459,#6713,.T.) ;
#16666 = EDGE_CURVE('',#13460,#13458,#6714,.T.) ;
#16667 = EDGE_CURVE('',#13461,#13460,#6715,.T.) ;
#16668 = EDGE_CURVE('',#13459,#13461,#6716,.T.) ;
#16669 = EDGE_CURVE('',#13462,#13463,#6717,.T.) ;
#16670 = EDGE_CURVE('',#13464,#13462,#6718,.T.) ;
#16671 = EDGE_CURVE('',#13465,#13464,#6719,.T.) ;
#16672 = EDGE_CURVE('',#13463,#13465,#6720,.T.) ;
#16673 = EDGE_CURVE('',#13466,#13466,#11166,.T.) ;
#16674 = EDGE_CURVE('',#13467,#13467,#11167,.T.) ;
#16675 = EDGE_CURVE('',#13431,#13468,#11168,.T.) ;
#16676 = EDGE_CURVE('',#13469,#13468,#6721,.T.) ;
#16677 = EDGE_CURVE('',#13281,#13469,#6722,.T.) ;
#16678 = EDGE_CURVE('',#13281,#13324,#6723,.T.) ;
#16679 = EDGE_CURVE('',#13329,#13432,#6724,.T.) ;
#16680 = EDGE_CURVE('',#13470,#13279,#6725,.T.) ;
#16681 = EDGE_CURVE('',#13282,#13471,#6726,.T.) ;
#16682 = EDGE_CURVE('',#13471,#13472,#6727,.T.) ;
#16683 = EDGE_CURVE('',#13472,#13473,#1439,.T.) ;
#16684 = EDGE_CURVE('',#13474,#13473,#6728,.T.) ;
#16685 = EDGE_CURVE('',#13474,#13475,#6729,.T.) ;
#16686 = EDGE_CURVE('',#13475,#13470,#6730,.T.) ;
#16687 = EDGE_CURVE('',#13476,#13430,#11169,.T.) ;
#16688 = EDGE_CURVE('',#13468,#13476,#6731,.T.) ;
#16689 = EDGE_CURVE('',#13477,#13273,#6732,.T.) ;
#16690 = EDGE_CURVE('',#13415,#13477,#11170,.T.) ;
#16691 = EDGE_CURVE('',#13478,#13392,#11171,.T.) ;
#16692 = EDGE_CURVE('',#13478,#13272,#6733,.T.) ;
#16693 = EDGE_CURVE('',#13290,#13479,#11172,.T.) ;
#16694 = EDGE_CURVE('',#13480,#13479,#6734,.T.) ;
#16695 = EDGE_CURVE('',#13291,#13480,#11173,.T.) ;
#16696 = EDGE_CURVE('',#13433,#13328,#6735,.T.) ;
#16697 = EDGE_CURVE('',#13473,#13481,#6736,.T.) ;
#16698 = EDGE_CURVE('',#13481,#13482,#6737,.T.) ;
#16699 = EDGE_CURVE('',#13482,#13474,#6738,.T.) ;
#16700 = EDGE_CURVE('',#13483,#13475,#6739,.T.) ;
#16701 = EDGE_CURVE('',#13483,#13482,#6740,.T.) ;
#16702 = EDGE_CURVE('',#13472,#13484,#6741,.T.) ;
#16703 = EDGE_CURVE('',#13481,#13484,#1440,.T.) ;
#16704 = EDGE_CURVE('',#13470,#13485,#6742,.T.) ;
#16705 = EDGE_CURVE('',#13485,#13483,#6743,.T.) ;
#16706 = EDGE_CURVE('',#13486,#13276,#6744,.T.) ;
#16707 = EDGE_CURVE('',#13486,#13280,#6745,.T.) ;
#16708 = EDGE_CURVE('',#13275,#13485,#6746,.T.) ;
#16709 = EDGE_CURVE('',#13480,#13280,#6747,.T.) ;
#16710 = EDGE_CURVE('',#13487,#13486,#6748,.T.) ;
#16711 = EDGE_CURVE('',#13487,#13384,#11174,.T.) ;
#16712 = EDGE_CURVE('',#13383,#13292,#6749,.T.) ;
#16713 = EDGE_CURVE('',#13293,#13382,#6750,.T.) ;
#16714 = EDGE_CURVE('',#13278,#13469,#6751,.T.) ;
#16715 = EDGE_CURVE('',#13488,#13277,#6752,.T.) ;
#16716 = EDGE_CURVE('',#13488,#13471,#6753,.T.) ;
#16717 = EDGE_CURVE('',#13484,#13488,#6754,.T.) ;
#16718 = EDGE_CURVE('',#13307,#13489,#11175,.T.) ;
#16719 = EDGE_CURVE('',#13489,#13490,#6755,.T.) ;
#16720 = EDGE_CURVE('',#13490,#13294,#11176,.T.) ;
#16721 = EDGE_CURVE('',#13489,#13491,#6756,.T.) ;
#16722 = EDGE_CURVE('',#13492,#13491,#6757,.T.) ;
#16723 = EDGE_CURVE('',#13490,#13492,#6758,.T.) ;
#16724 = EDGE_CURVE('',#13493,#13300,#11177,.T.) ;
#16725 = EDGE_CURVE('',#13299,#13494,#11178,.T.) ;
#16726 = EDGE_CURVE('',#13494,#13493,#6759,.T.) ;
#16727 = EDGE_CURVE('',#13495,#13301,#11179,.T.) ;
#16728 = EDGE_CURVE('',#13493,#13495,#11180,.T.) ;
#16729 = EDGE_CURVE('',#13496,#13302,#11181,.T.) ;
#16730 = EDGE_CURVE('',#13495,#13496,#6760,.T.) ;
#16731 = EDGE_CURVE('',#13497,#13303,#11182,.T.) ;
#16732 = EDGE_CURVE('',#13496,#13497,#11183,.T.) ;
#16733 = EDGE_CURVE('',#13304,#13498,#11184,.F.) ;
#16734 = EDGE_CURVE('',#13497,#13498,#6761,.T.) ;
#16735 = EDGE_CURVE('',#13499,#13497,#6762,.T.) ;
#16736 = EDGE_CURVE('',#13500,#13499,#6763,.T.) ;
#16737 = EDGE_CURVE('',#13500,#13498,#6764,.T.) ;
#16738 = EDGE_CURVE('',#13496,#13501,#6765,.T.) ;
#16739 = EDGE_CURVE('',#13499,#13501,#11185,.T.) ;
#16740 = EDGE_CURVE('',#13502,#13495,#6766,.T.) ;
#16741 = EDGE_CURVE('',#13501,#13502,#6767,.T.) ;
#16742 = EDGE_CURVE('',#13493,#13503,#6768,.T.) ;
#16743 = EDGE_CURVE('',#13502,#13503,#11186,.T.) ;
#16744 = EDGE_CURVE('',#13494,#13504,#6769,.T.) ;
#16745 = EDGE_CURVE('',#13503,#13504,#6770,.T.) ;
#16746 = EDGE_CURVE('',#13505,#13378,#11187,.T.) ;
#16747 = EDGE_CURVE('',#13377,#13506,#11188,.T.) ;
#16748 = EDGE_CURVE('',#13506,#13505,#6771,.T.) ;
#16749 = EDGE_CURVE('',#13507,#13379,#11189,.T.) ;
#16750 = EDGE_CURVE('',#13505,#13507,#11190,.T.) ;
#16751 = EDGE_CURVE('',#13508,#13380,#11191,.T.) ;
#16752 = EDGE_CURVE('',#13507,#13508,#6772,.T.) ;
#16753 = EDGE_CURVE('',#13509,#13381,#11192,.T.) ;
#16754 = EDGE_CURVE('',#13508,#13509,#11193,.T.) ;
#16755 = EDGE_CURVE('',#13510,#13372,#11194,.T.) ;
#16756 = EDGE_CURVE('',#13509,#13510,#6773,.T.) ;
#16757 = EDGE_CURVE('',#13511,#13509,#6774,.T.) ;
#16758 = EDGE_CURVE('',#13512,#13511,#6775,.T.) ;
#16759 = EDGE_CURVE('',#13512,#13510,#6776,.T.) ;
#16760 = EDGE_CURVE('',#13508,#13513,#6777,.T.) ;
#16761 = EDGE_CURVE('',#13511,#13513,#11195,.T.) ;
#16762 = EDGE_CURVE('',#13514,#13507,#6778,.T.) ;
#16763 = EDGE_CURVE('',#13513,#13514,#6779,.T.) ;
#16764 = EDGE_CURVE('',#13505,#13515,#6780,.T.) ;
#16765 = EDGE_CURVE('',#13514,#13515,#11196,.T.) ;
#16766 = EDGE_CURVE('',#13506,#13516,#6781,.T.) ;
#16767 = EDGE_CURVE('',#13515,#13516,#6782,.T.) ;
#16768 = EDGE_CURVE('',#13517,#13518,#6783,.T.) ;
#16769 = EDGE_CURVE('',#13517,#13519,#6784,.T.) ;
#16770 = EDGE_CURVE('',#13520,#13519,#6785,.T.) ;
#16771 = EDGE_CURVE('',#13518,#13520,#6786,.T.) ;
#16772 = EDGE_CURVE('',#13518,#13521,#6787,.T.) ;
#16773 = EDGE_CURVE('',#13522,#13520,#6788,.T.) ;
#16774 = EDGE_CURVE('',#13521,#13522,#6789,.T.) ;
#16775 = EDGE_CURVE('',#13521,#13523,#6790,.T.) ;
#16776 = EDGE_CURVE('',#13524,#13522,#6791,.T.) ;
#16777 = EDGE_CURVE('',#13523,#13524,#6792,.T.) ;
#16778 = EDGE_CURVE('',#13523,#13525,#6793,.T.) ;
#16779 = EDGE_CURVE('',#13526,#13524,#6794,.T.) ;
#16780 = EDGE_CURVE('',#13525,#13526,#6795,.T.) ;
#16781 = EDGE_CURVE('',#13527,#13517,#6796,.T.) ;
#16782 = EDGE_CURVE('',#13527,#13528,#6797,.T.) ;
#16783 = EDGE_CURVE('',#13519,#13528,#6798,.T.) ;
#16784 = EDGE_CURVE('',#13525,#13527,#6799,.T.) ;
#16785 = EDGE_CURVE('',#13528,#13526,#6800,.T.) ;
#16786 = EDGE_CURVE('',#13529,#13530,#6801,.T.) ;
#16787 = EDGE_CURVE('',#13529,#13531,#6802,.T.) ;
#16788 = EDGE_CURVE('',#13532,#13531,#6803,.T.) ;
#16789 = EDGE_CURVE('',#13530,#13532,#6804,.T.) ;
#16790 = EDGE_CURVE('',#13530,#13533,#6805,.T.) ;
#16791 = EDGE_CURVE('',#13534,#13532,#6806,.T.) ;
#16792 = EDGE_CURVE('',#13533,#13534,#6807,.T.) ;
#16793 = EDGE_CURVE('',#13533,#13535,#6808,.T.) ;
#16794 = EDGE_CURVE('',#13536,#13534,#6809,.T.) ;
#16795 = EDGE_CURVE('',#13535,#13536,#6810,.T.) ;
#16796 = EDGE_CURVE('',#13535,#13537,#6811,.T.) ;
#16797 = EDGE_CURVE('',#13538,#13536,#6812,.T.) ;
#16798 = EDGE_CURVE('',#13537,#13538,#6813,.T.) ;
#16799 = EDGE_CURVE('',#13539,#13529,#6814,.T.) ;
#16800 = EDGE_CURVE('',#13539,#13540,#6815,.T.) ;
#16801 = EDGE_CURVE('',#13531,#13540,#6816,.T.) ;
#16802 = EDGE_CURVE('',#13537,#13539,#6817,.T.) ;
#16803 = EDGE_CURVE('',#13540,#13538,#6818,.T.) ;
#16804 = EDGE_CURVE('',#13541,#13333,#11197,.T.) ;
#16805 = EDGE_CURVE('',#13332,#13542,#11198,.T.) ;
#16806 = EDGE_CURVE('',#13542,#13541,#6819,.T.) ;
#16807 = EDGE_CURVE('',#13543,#13287,#11199,.T.) ;
#16808 = EDGE_CURVE('',#13286,#13544,#11200,.T.) ;
#16809 = EDGE_CURVE('',#13544,#13543,#6820,.T.) ;
#16810 = EDGE_CURVE('',#13269,#13545,#6821,.T.) ;
#16811 = EDGE_CURVE('',#13545,#13283,#11201,.T.) ;
#16812 = EDGE_CURVE('',#13546,#13341,#11202,.T.) ;
#16813 = EDGE_CURVE('',#13340,#13547,#11203,.T.) ;
#16814 = EDGE_CURVE('',#13547,#13546,#6822,.T.) ;
#16815 = EDGE_CURVE('',#13336,#13548,#11204,.T.) ;
#16816 = EDGE_CURVE('',#13548,#13549,#6823,.T.) ;
#16817 = EDGE_CURVE('',#13549,#13337,#11205,.T.) ;
#16818 = EDGE_CURVE('',#13550,#13326,#6824,.T.) ;
#16819 = EDGE_CURVE('',#13551,#13550,#6825,.T.) ;
#16820 = EDGE_CURVE('',#13476,#13551,#6826,.T.) ;
#16821 = EDGE_CURVE('',#13330,#13429,#6827,.T.) ;
#16822 = EDGE_CURVE('',#13552,#13552,#11206,.T.) ;
#16823 = EDGE_CURVE('',#13552,#13412,#6828,.T.) ;
#16824 = EDGE_CURVE('',#13323,#13552,#6829,.T.) ;
#16825 = EDGE_CURVE('',#13553,#13553,#11207,.T.) ;
#16826 = EDGE_CURVE('',#13553,#13466,#6830,.T.) ;
#16827 = EDGE_CURVE('',#13553,#13361,#6831,.T.) ;
#16828 = EDGE_CURVE('',#13554,#13554,#11208,.T.) ;
#16829 = EDGE_CURVE('',#13554,#13393,#6832,.T.) ;
#16830 = EDGE_CURVE('',#13310,#13554,#6833,.T.) ;
#16831 = EDGE_CURVE('',#13512,#13555,#6834,.T.) ;
#16832 = EDGE_CURVE('',#13373,#13555,#11209,.T.) ;
#16833 = EDGE_CURVE('',#13556,#13516,#6835,.T.) ;
#16834 = EDGE_CURVE('',#13376,#13556,#11210,.T.) ;
#16835 = EDGE_CURVE('',#13557,#13557,#11211,.F.) ;
#16836 = EDGE_CURVE('',#13557,#13558,#6836,.T.) ;
#16837 = EDGE_CURVE('',#13558,#13559,#11212,.T.) ;
#16838 = EDGE_CURVE('',#13559,#13558,#11213,.T.) ;
#16839 = EDGE_CURVE('',#13559,#13560,#6837,.T.) ;
#16840 = EDGE_CURVE('',#13560,#13560,#11214,.T.) ;
#16841 = EDGE_CURVE('',#13561,#13562,#11215,.T.) ;
#16842 = EDGE_CURVE('',#13561,#13563,#6838,.T.) ;
#16843 = EDGE_CURVE('',#13564,#13563,#11216,.T.) ;
#16844 = EDGE_CURVE('',#13564,#13562,#6839,.T.) ;
#16845 = EDGE_CURVE('',#13565,#13566,#11217,.T.) ;
#16846 = EDGE_CURVE('',#13565,#13567,#6840,.T.) ;
#16847 = EDGE_CURVE('',#13568,#13567,#11218,.T.) ;
#16848 = EDGE_CURVE('',#13568,#13566,#6841,.T.) ;
#16849 = EDGE_CURVE('',#13569,#13570,#11219,.T.) ;
#16850 = EDGE_CURVE('',#13569,#13571,#6842,.T.) ;
#16851 = EDGE_CURVE('',#13572,#13571,#11220,.T.) ;
#16852 = EDGE_CURVE('',#13572,#13570,#6843,.T.) ;
#16853 = EDGE_CURVE('',#13573,#13574,#11221,.T.) ;
#16854 = EDGE_CURVE('',#13573,#13575,#6844,.T.) ;
#16855 = EDGE_CURVE('',#13576,#13575,#11222,.T.) ;
#16856 = EDGE_CURVE('',#13576,#13574,#6845,.T.) ;
#16857 = EDGE_CURVE('',#13577,#13551,#11223,.T.) ;
#16858 = EDGE_CURVE('',#13578,#13550,#11224,.T.) ;
#16859 = EDGE_CURVE('',#13578,#13577,#6846,.T.) ;
#16860 = EDGE_CURVE('',#13579,#13580,#11225,.T.) ;
#16861 = EDGE_CURVE('',#13580,#13581,#6847,.T.) ;
#16862 = EDGE_CURVE('',#13582,#13581,#11226,.T.) ;
#16863 = EDGE_CURVE('',#13582,#13579,#6848,.T.) ;
#16864 = EDGE_CURVE('',#13583,#13447,#11227,.T.) ;
#16865 = EDGE_CURVE('',#13446,#13584,#11228,.T.) ;
#16866 = EDGE_CURVE('',#13583,#13584,#11229,.T.) ;
#16867 = EDGE_CURVE('',#13448,#13375,#11230,.T.) ;
#16868 = EDGE_CURVE('',#13583,#13556,#6849,.T.) ;
#16869 = EDGE_CURVE('',#13334,#13425,#6850,.T.) ;
#16870 = EDGE_CURVE('',#13424,#13335,#6851,.T.) ;
#16871 = EDGE_CURVE('',#13420,#13339,#6852,.T.) ;
#16872 = EDGE_CURVE('',#13338,#13421,#6853,.T.) ;
#16873 = EDGE_CURVE('',#13416,#13343,#6854,.T.) ;
#16874 = EDGE_CURVE('',#13342,#13417,#6855,.T.) ;
#16875 = EDGE_CURVE('',#13428,#13331,#6856,.T.) ;
#16876 = EDGE_CURVE('',#13463,#13352,#6857,.T.) ;
#16877 = EDGE_CURVE('',#13350,#13465,#6858,.T.) ;
#16878 = EDGE_CURVE('',#13349,#13464,#6859,.T.) ;
#16879 = EDGE_CURVE('',#13351,#13462,#6860,.T.) ;
#16880 = EDGE_CURVE('',#13459,#13356,#6861,.T.) ;
#16881 = EDGE_CURVE('',#13354,#13461,#6862,.T.) ;
#16882 = EDGE_CURVE('',#13353,#13460,#6863,.T.) ;
#16883 = EDGE_CURVE('',#13355,#13458,#6864,.T.) ;
#16884 = EDGE_CURVE('',#13455,#13360,#6865,.T.) ;
#16885 = EDGE_CURVE('',#13358,#13457,#6866,.T.) ;
#16886 = EDGE_CURVE('',#13357,#13456,#6867,.T.) ;
#16887 = EDGE_CURVE('',#13359,#13454,#6868,.T.) ;
#16888 = EDGE_CURVE('',#13374,#13449,#11231,.T.) ;
#16889 = EDGE_CURVE('',#13345,#13452,#6869,.T.) ;
#16890 = EDGE_CURVE('',#13347,#13450,#6870,.T.) ;
#16891 = EDGE_CURVE('',#13451,#13348,#6871,.T.) ;
#16892 = EDGE_CURVE('',#13346,#13453,#6872,.T.) ;
#16893 = EDGE_CURVE('',#13581,#13541,#6873,.T.) ;
#16894 = EDGE_CURVE('',#13585,#13580,#6874,.T.) ;
#16895 = EDGE_CURVE('',#13585,#13426,#11232,.T.) ;
#16896 = EDGE_CURVE('',#13546,#13566,#6875,.T.) ;
#16897 = EDGE_CURVE('',#13586,#13568,#6876,.T.) ;
#16898 = EDGE_CURVE('',#13586,#13418,#11233,.T.) ;
#16899 = EDGE_CURVE('',#13419,#13587,#11234,.T.) ;
#16900 = EDGE_CURVE('',#13586,#13587,#6877,.T.) ;
#16901 = EDGE_CURVE('',#13588,#13585,#6878,.T.) ;
#16902 = EDGE_CURVE('',#13427,#13588,#11235,.T.) ;
#16903 = EDGE_CURVE('',#13562,#13549,#6879,.T.) ;
#16904 = EDGE_CURVE('',#13589,#13564,#6880,.T.) ;
#16905 = EDGE_CURVE('',#13589,#13422,#11236,.T.) ;
#16906 = EDGE_CURVE('',#13590,#13589,#6881,.T.) ;
#16907 = EDGE_CURVE('',#13423,#13590,#11237,.T.) ;
#16908 = EDGE_CURVE('',#13591,#13445,#11238,.T.) ;
#16909 = EDGE_CURVE('',#13591,#13584,#6882,.T.) ;
#16910 = EDGE_CURVE('',#13444,#13592,#11239,.T.) ;
#16911 = EDGE_CURVE('',#13591,#13592,#11240,.T.) ;
#16912 = EDGE_CURVE('',#13555,#13592,#6883,.T.) ;
#16913 = EDGE_CURVE('',#13561,#13547,#6884,.T.) ;
#16914 = EDGE_CURVE('',#13563,#13587,#6885,.T.) ;
#16915 = EDGE_CURVE('',#13565,#13252,#6886,.T.) ;
#16916 = EDGE_CURVE('',#13567,#13477,#6887,.T.) ;
#16917 = EDGE_CURVE('',#13579,#13590,#6888,.T.) ;
#16918 = EDGE_CURVE('',#13548,#13582,#6889,.T.) ;
#16919 = EDGE_CURVE('',#13577,#13588,#6890,.T.) ;
#16920 = EDGE_CURVE('',#13542,#13578,#6891,.T.) ;
#16921 = EDGE_CURVE('',#13593,#13594,#6892,.T.) ;
#16922 = EDGE_CURVE('',#13593,#13492,#6893,.T.) ;
#16923 = EDGE_CURVE('',#13595,#13492,#6894,.T.) ;
#16924 = EDGE_CURVE('',#13595,#13596,#6895,.T.) ;
#16925 = EDGE_CURVE('',#13504,#13596,#6896,.T.) ;
#16926 = EDGE_CURVE('',#13504,#13597,#6897,.T.) ;
#16927 = EDGE_CURVE('',#13598,#13597,#6898,.T.) ;
#16928 = EDGE_CURVE('',#13598,#13599,#11241,.T.) ;
#16929 = EDGE_CURVE('',#13600,#13599,#6899,.T.) ;
#16930 = EDGE_CURVE('',#13600,#13601,#11242,.T.) ;
#16931 = EDGE_CURVE('',#13602,#13601,#6900,.T.) ;
#16932 = EDGE_CURVE('',#13602,#13594,#6901,.T.) ;
#16933 = EDGE_CURVE('',#13603,#13603,#11243,.T.) ;
#16934 = EDGE_CURVE('',#13604,#13604,#11244,.T.) ;
#16935 = EDGE_CURVE('',#13605,#13605,#11245,.T.) ;
#16936 = EDGE_CURVE('',#13606,#13606,#11246,.T.) ;
#16937 = EDGE_CURVE('',#13607,#13595,#11247,.T.) ;
#16938 = EDGE_CURVE('',#13608,#13607,#6902,.T.) ;
#16939 = EDGE_CURVE('',#13596,#13608,#11248,.T.) ;
#16940 = EDGE_CURVE('',#13609,#13609,#11249,.F.) ;
#16941 = EDGE_CURVE('',#13609,#13610,#6903,.T.) ;
#16942 = EDGE_CURVE('',#13611,#13610,#11250,.T.) ;
#16943 = EDGE_CURVE('',#13610,#13611,#11251,.T.) ;
#16944 = EDGE_CURVE('',#13611,#13606,#6904,.T.) ;
#16945 = EDGE_CURVE('',#13612,#13612,#11252,.F.) ;
#16946 = EDGE_CURVE('',#13612,#13613,#6905,.T.) ;
#16947 = EDGE_CURVE('',#13614,#13613,#11253,.T.) ;
#16948 = EDGE_CURVE('',#13613,#13614,#11254,.T.) ;
#16949 = EDGE_CURVE('',#13614,#13605,#6906,.T.) ;
#16950 = EDGE_CURVE('',#13615,#13615,#11255,.F.) ;
#16951 = EDGE_CURVE('',#13615,#13616,#6907,.T.) ;
#16952 = EDGE_CURVE('',#13617,#13616,#11256,.T.) ;
#16953 = EDGE_CURVE('',#13616,#13617,#11257,.T.) ;
#16954 = EDGE_CURVE('',#13617,#13604,#6908,.T.) ;
#16955 = EDGE_CURVE('',#13618,#13618,#11258,.F.) ;
#16956 = EDGE_CURVE('',#13618,#13619,#6909,.T.) ;
#16957 = EDGE_CURVE('',#13620,#13619,#11259,.T.) ;
#16958 = EDGE_CURVE('',#13619,#13620,#11260,.T.) ;
#16959 = EDGE_CURVE('',#13620,#13603,#6910,.T.) ;
#16960 = EDGE_CURVE('',#13621,#13622,#6911,.T.) ;
#16961 = EDGE_CURVE('',#13594,#13622,#6912,.T.) ;
#16962 = EDGE_CURVE('',#13621,#13602,#6913,.T.) ;
#16963 = EDGE_CURVE('',#13295,#13593,#11261,.T.) ;
#16964 = EDGE_CURVE('',#13298,#13597,#11262,.T.) ;
#16965 = EDGE_CURVE('',#13390,#13285,#6914,.T.) ;
#16966 = EDGE_CURVE('',#13389,#13623,#11263,.T.) ;
#16967 = EDGE_CURVE('',#13570,#13623,#6915,.T.) ;
#16968 = EDGE_CURVE('',#13544,#13572,#6916,.T.) ;
#16969 = EDGE_CURVE('',#13571,#13545,#6917,.T.) ;
#16970 = EDGE_CURVE('',#13478,#13569,#6918,.T.) ;
#16971 = EDGE_CURVE('',#13284,#13391,#6919,.T.) ;
#16972 = EDGE_CURVE('',#13320,#13397,#6920,.T.) ;
#16973 = EDGE_CURVE('',#13319,#13396,#6921,.T.) ;
#16974 = EDGE_CURVE('',#13395,#13322,#6922,.T.) ;
#16975 = EDGE_CURVE('',#13321,#13394,#6923,.T.) ;
#16976 = EDGE_CURVE('',#13305,#13624,#6924,.T.) ;
#16977 = EDGE_CURVE('',#13625,#13624,#6925,.T.) ;
#16978 = EDGE_CURVE('',#13306,#13625,#6926,.T.) ;
#16979 = EDGE_CURVE('',#13288,#13387,#6927,.T.) ;
#16980 = EDGE_CURVE('',#13386,#13289,#6928,.T.) ;
#16981 = EDGE_CURVE('',#13296,#13411,#11264,.T.) ;
#16982 = EDGE_CURVE('',#13410,#13297,#11265,.T.) ;
#16983 = EDGE_CURVE('',#13313,#13398,#6929,.T.) ;
#16984 = EDGE_CURVE('',#13399,#13314,#6930,.T.) ;
#16985 = EDGE_CURVE('',#13311,#13400,#6931,.T.) ;
#16986 = EDGE_CURVE('',#13312,#13401,#6932,.T.) ;
#16987 = EDGE_CURVE('',#13317,#13402,#6933,.T.) ;
#16988 = EDGE_CURVE('',#13403,#13318,#6934,.T.) ;
#16989 = EDGE_CURVE('',#13315,#13404,#6935,.T.) ;
#16990 = EDGE_CURVE('',#13316,#13405,#6936,.T.) ;
#16991 = EDGE_CURVE('',#13600,#13407,#11266,.T.) ;
#16992 = EDGE_CURVE('',#13406,#13601,#11267,.T.) ;
#16993 = EDGE_CURVE('',#13408,#13599,#11268,.T.) ;
#16994 = EDGE_CURVE('',#13598,#13409,#11269,.T.) ;
#16995 = EDGE_CURVE('',#13487,#13626,#6937,.T.) ;
#16996 = EDGE_CURVE('',#13385,#13626,#11270,.T.) ;
#16997 = EDGE_CURVE('',#13574,#13626,#6938,.T.) ;
#16998 = EDGE_CURVE('',#13479,#13576,#6939,.T.) ;
#16999 = EDGE_CURVE('',#13627,#13388,#11271,.T.) ;
#17000 = EDGE_CURVE('',#13623,#13627,#6940,.T.) ;
#17001 = EDGE_CURVE('',#13575,#13543,#6941,.T.) ;
#17002 = EDGE_CURVE('',#13627,#13573,#6942,.T.) ;
#17003 = EDGE_CURVE('',#13625,#13594,#11272,.T.) ;
#17004 = EDGE_CURVE('',#13602,#13624,#11273,.T.) ;
#17005 = EDGE_CURVE('',#13628,#13629,#6943,.T.) ;
#17006 = EDGE_CURVE('',#13629,#13516,#6944,.T.) ;
#17007 = EDGE_CURVE('',#13628,#13512,#6945,.T.) ;
#17008 = EDGE_CURVE('',#13630,#13631,#11274,.T.) ;
#17009 = EDGE_CURVE('',#13630,#13344,#6946,.T.) ;
#17010 = EDGE_CURVE('',#13631,#13630,#11275,.T.) ;
#17011 = EDGE_CURVE('',#13631,#13467,#6947,.T.) ;
#17012 = EDGE_CURVE('',#13371,#13632,#6948,.T.) ;
#17013 = EDGE_CURVE('',#13633,#13370,#6949,.T.) ;
#17014 = EDGE_CURVE('',#13632,#13633,#6950,.T.) ;
#17015 = EDGE_CURVE('',#13369,#13634,#6951,.T.) ;
#17016 = EDGE_CURVE('',#13635,#13368,#6952,.T.) ;
#17017 = EDGE_CURVE('',#13634,#13635,#6953,.T.) ;
#17018 = EDGE_CURVE('',#13636,#13366,#6954,.T.) ;
#17019 = EDGE_CURVE('',#13637,#13636,#6955,.T.) ;
#17020 = EDGE_CURVE('',#13367,#13637,#6956,.T.) ;
#17021 = EDGE_CURVE('',#13638,#13364,#6957,.T.) ;
#17022 = EDGE_CURVE('',#13639,#13638,#6958,.T.) ;
#17023 = EDGE_CURVE('',#13365,#13639,#6959,.T.) ;
#17024 = EDGE_CURVE('',#13637,#13635,#11276,.F.) ;
#17025 = EDGE_CURVE('',#13639,#13636,#11277,.F.) ;
#17026 = EDGE_CURVE('',#13636,#13440,#11278,.T.) ;
#17027 = EDGE_CURVE('',#13439,#13637,#11279,.T.) ;
#17028 = EDGE_CURVE('',#13634,#13633,#11280,.F.) ;
#17029 = EDGE_CURVE('',#13633,#13436,#11281,.T.) ;
#17030 = EDGE_CURVE('',#13434,#13632,#11282,.T.) ;
#17031 = EDGE_CURVE('',#13632,#13638,#11283,.F.) ;
#17032 = EDGE_CURVE('',#13638,#13435,#11284,.T.) ;
#17033 = EDGE_CURVE('',#13441,#13639,#11285,.T.) ;
#17034 = EDGE_CURVE('',#13635,#13438,#11286,.T.) ;
#17035 = EDGE_CURVE('',#13437,#13634,#11287,.T.) ;
#17036 = EDGE_CURVE('',#13640,#13628,#11288,.T.) ;
#17037 = EDGE_CURVE('',#13641,#13640,#6960,.T.) ;
#17038 = EDGE_CURVE('',#13629,#13641,#11289,.T.) ;
#17039 = EDGE_CURVE('',#13621,#13500,#11290,.T.) ;
#17040 = EDGE_CURVE('',#13642,#13499,#11291,.T.) ;
#17041 = EDGE_CURVE('',#13642,#13621,#6961,.T.) ;
#17042 = EDGE_CURVE('',#13491,#13622,#11292,.T.) ;
#17043 = EDGE_CURVE('',#13622,#13607,#6962,.T.) ;
#17044 = EDGE_CURVE('',#13515,#13643,#11293,.T.) ;
#17045 = EDGE_CURVE('',#13641,#13643,#6963,.T.) ;
#17046 = EDGE_CURVE('',#13503,#13644,#11294,.T.) ;
#17047 = EDGE_CURVE('',#13608,#13644,#6964,.T.) ;
#17048 = EDGE_CURVE('',#13645,#13642,#11295,.T.) ;
#17049 = EDGE_CURVE('',#13646,#13645,#6965,.T.) ;
#17050 = EDGE_CURVE('',#13644,#13646,#11296,.T.) ;
#17051 = EDGE_CURVE('',#13502,#13646,#11297,.T.) ;
#17052 = EDGE_CURVE('',#13501,#13645,#11298,.T.) ;
#17053 = EDGE_CURVE('',#13643,#13647,#11299,.T.) ;
#17054 = EDGE_CURVE('',#13648,#13640,#6966,.T.) ;
#17055 = EDGE_CURVE('',#13649,#13648,#11300,.T.) ;
#17056 = EDGE_CURVE('',#13647,#13649,#6967,.T.) ;
#17057 = EDGE_CURVE('',#13648,#13511,#11301,.T.) ;
#17058 = EDGE_CURVE('',#13514,#13647,#11302,.T.) ;
#17059 = EDGE_CURVE('',#13513,#13649,#11303,.T.) ;
#17060 = EDGE_CURVE('',#13143,#13093,#1441,.T.) ;
#17061 = EDGE_CURVE('',#13650,#13148,#1442,.T.) ;
#17062 = EDGE_CURVE('',#13100,#13650,#1443,.T.) ;
#17063 = EDGE_CURVE('',#13092,#13651,#1444,.T.) ;
#17064 = EDGE_CURVE('',#13147,#13101,#1445,.T.) ;
#17065 = EDGE_CURVE('',#13651,#13140,#1446,.T.) ;
#17066 = EDGE_CURVE('',#13119,#13080,#1447,.T.) ;
#17067 = EDGE_CURVE('',#13652,#13124,#1448,.T.) ;
#17068 = EDGE_CURVE('',#13087,#13652,#1449,.T.) ;
#17069 = EDGE_CURVE('',#13079,#13653,#1450,.T.) ;
#17070 = EDGE_CURVE('',#13123,#13088,#1451,.T.) ;
#17071 = EDGE_CURVE('',#13653,#13116,#1452,.T.) ;
#17072 = EDGE_CURVE('',#13107,#13065,#1453,.T.) ;
#17073 = EDGE_CURVE('',#13654,#13112,#1454,.T.) ;
#17074 = EDGE_CURVE('',#13074,#13654,#1455,.T.) ;
#17075 = EDGE_CURVE('',#13064,#13655,#1456,.T.) ;
#17076 = EDGE_CURVE('',#13111,#13075,#1457,.T.) ;
#17077 = EDGE_CURVE('',#13655,#13104,#1458,.T.) ;
#17078 = EDGE_CURVE('',#13656,#13657,#6968,.T.) ;
#17079 = EDGE_CURVE('',#13657,#13658,#6969,.T.) ;
#17080 = EDGE_CURVE('',#13658,#13659,#6970,.T.) ;
#17081 = EDGE_CURVE('',#13659,#13660,#6971,.T.) ;
#17082 = EDGE_CURVE('',#13660,#13661,#6972,.T.) ;
#17083 = EDGE_CURVE('',#13661,#13656,#6973,.T.) ;
#17084 = EDGE_CURVE('',#13662,#13663,#6974,.T.) ;
#17085 = EDGE_CURVE('',#13663,#13664,#6975,.T.) ;
#17086 = EDGE_CURVE('',#13664,#13665,#6976,.T.) ;
#17087 = EDGE_CURVE('',#13665,#13666,#6977,.T.) ;
#17088 = EDGE_CURVE('',#13666,#13667,#6978,.T.) ;
#17089 = EDGE_CURVE('',#13667,#13662,#6979,.T.) ;
#17090 = EDGE_CURVE('',#13668,#13669,#6980,.T.) ;
#17091 = EDGE_CURVE('',#13669,#13670,#6981,.T.) ;
#17092 = EDGE_CURVE('',#13670,#13671,#6982,.T.) ;
#17093 = EDGE_CURVE('',#13671,#13672,#6983,.T.) ;
#17094 = EDGE_CURVE('',#13672,#13673,#6984,.T.) ;
#17095 = EDGE_CURVE('',#13673,#13668,#6985,.T.) ;
#17096 = EDGE_CURVE('',#13135,#13061,#1459,.T.) ;
#17097 = EDGE_CURVE('',#13060,#13674,#1460,.T.) ;
#17098 = EDGE_CURVE('',#13674,#13136,#1461,.T.) ;
#17099 = EDGE_CURVE('',#13131,#13053,#1462,.T.) ;
#17100 = EDGE_CURVE('',#13052,#13675,#1463,.T.) ;
#17101 = EDGE_CURVE('',#13675,#13128,#1464,.T.) ;
#17102 = EDGE_CURVE('',#13676,#13677,#6986,.T.) ;
#17103 = EDGE_CURVE('',#13676,#13668,#6987,.T.) ;
#17104 = EDGE_CURVE('',#13677,#13673,#6988,.T.) ;
#17105 = EDGE_CURVE('',#13677,#13678,#6989,.T.) ;
#17106 = EDGE_CURVE('',#13678,#13672,#6990,.T.) ;
#17107 = EDGE_CURVE('',#13679,#13676,#6991,.T.) ;
#17108 = EDGE_CURVE('',#13679,#13669,#6992,.T.) ;
#17109 = EDGE_CURVE('',#13680,#13679,#6993,.T.) ;
#17110 = EDGE_CURVE('',#13680,#13670,#6994,.T.) ;
#17111 = EDGE_CURVE('',#13681,#13680,#6995,.T.) ;
#17112 = EDGE_CURVE('',#13681,#13671,#6996,.T.) ;
#17113 = EDGE_CURVE('',#13678,#13681,#6997,.T.) ;
#17114 = EDGE_CURVE('',#13682,#13683,#6998,.T.) ;
#17115 = EDGE_CURVE('',#13682,#13656,#6999,.T.) ;
#17116 = EDGE_CURVE('',#13683,#13661,#7000,.T.) ;
#17117 = EDGE_CURVE('',#13683,#13684,#7001,.T.) ;
#17118 = EDGE_CURVE('',#13684,#13660,#7002,.T.) ;
#17119 = EDGE_CURVE('',#13685,#13682,#7003,.T.) ;
#17120 = EDGE_CURVE('',#13685,#13657,#7004,.T.) ;
#17121 = EDGE_CURVE('',#13686,#13685,#7005,.T.) ;
#17122 = EDGE_CURVE('',#13686,#13658,#7006,.T.) ;
#17123 = EDGE_CURVE('',#13687,#13686,#7007,.T.) ;
#17124 = EDGE_CURVE('',#13687,#13659,#7008,.T.) ;
#17125 = EDGE_CURVE('',#13684,#13687,#7009,.T.) ;
#17126 = EDGE_CURVE('',#13688,#13689,#7010,.T.) ;
#17127 = EDGE_CURVE('',#13689,#13690,#7011,.T.) ;
#17128 = EDGE_CURVE('',#13690,#13691,#7012,.T.) ;
#17129 = EDGE_CURVE('',#13691,#13692,#7013,.T.) ;
#17130 = EDGE_CURVE('',#13692,#13693,#7014,.T.) ;
#17131 = EDGE_CURVE('',#13693,#13688,#7015,.T.) ;
#17132 = EDGE_CURVE('',#13689,#13662,#7016,.T.) ;
#17133 = EDGE_CURVE('',#13690,#13667,#7017,.T.) ;
#17134 = EDGE_CURVE('',#13691,#13666,#7018,.T.) ;
#17135 = EDGE_CURVE('',#13688,#13663,#7019,.T.) ;
#17136 = EDGE_CURVE('',#13693,#13664,#7020,.T.) ;
#17137 = EDGE_CURVE('',#13692,#13665,#7021,.T.) ;
#17138 = EDGE_CURVE('',#13694,#13695,#7022,.T.) ;
#17139 = EDGE_CURVE('',#13694,#13696,#7023,.T.) ;
#17140 = EDGE_CURVE('',#13696,#13697,#7024,.T.) ;
#17141 = EDGE_CURVE('',#13695,#13697,#7025,.T.) ;
#17142 = EDGE_CURVE('',#13698,#13694,#7026,.T.) ;
#17143 = EDGE_CURVE('',#13699,#13698,#7027,.T.) ;
#17144 = EDGE_CURVE('',#13699,#13696,#7028,.T.) ;
#17145 = EDGE_CURVE('',#13695,#13700,#7029,.T.) ;
#17146 = EDGE_CURVE('',#13697,#13701,#7030,.T.) ;
#17147 = EDGE_CURVE('',#13700,#13701,#7031,.T.) ;
#17148 = EDGE_CURVE('',#13701,#13699,#7032,.T.) ;
#17149 = EDGE_CURVE('',#13702,#13703,#7033,.T.) ;
#17150 = EDGE_CURVE('',#13702,#13704,#7034,.T.) ;
#17151 = EDGE_CURVE('',#13704,#13705,#7035,.T.) ;
#17152 = EDGE_CURVE('',#13703,#13705,#7036,.T.) ;
#17153 = EDGE_CURVE('',#13706,#13702,#7037,.T.) ;
#17154 = EDGE_CURVE('',#13707,#13706,#7038,.T.) ;
#17155 = EDGE_CURVE('',#13707,#13704,#7039,.T.) ;
#17156 = EDGE_CURVE('',#13703,#13708,#7040,.T.) ;
#17157 = EDGE_CURVE('',#13705,#13709,#7041,.T.) ;
#17158 = EDGE_CURVE('',#13708,#13709,#7042,.T.) ;
#17159 = EDGE_CURVE('',#13709,#13707,#7043,.T.) ;
#17160 = EDGE_CURVE('',#13710,#13711,#7044,.T.) ;
#17161 = EDGE_CURVE('',#13710,#13712,#7045,.T.) ;
#17162 = EDGE_CURVE('',#13712,#13713,#7046,.T.) ;
#17163 = EDGE_CURVE('',#13711,#13713,#7047,.T.) ;
#17164 = EDGE_CURVE('',#13714,#13710,#7048,.T.) ;
#17165 = EDGE_CURVE('',#13714,#13715,#7049,.T.) ;
#17166 = EDGE_CURVE('',#13715,#13712,#7050,.T.) ;
#17167 = EDGE_CURVE('',#13716,#13714,#7051,.T.) ;
#17168 = EDGE_CURVE('',#13717,#13716,#7052,.T.) ;
#17169 = EDGE_CURVE('',#13717,#13715,#7053,.T.) ;
#17170 = EDGE_CURVE('',#13713,#13717,#7054,.T.) ;
#17171 = EDGE_CURVE('',#13718,#13719,#7055,.T.) ;
#17172 = EDGE_CURVE('',#13718,#13720,#7056,.T.) ;
#17173 = EDGE_CURVE('',#13720,#13721,#7057,.T.) ;
#17174 = EDGE_CURVE('',#13719,#13721,#7058,.T.) ;
#17175 = EDGE_CURVE('',#13722,#13718,#7059,.T.) ;
#17176 = EDGE_CURVE('',#13723,#13722,#7060,.T.) ;
#17177 = EDGE_CURVE('',#13723,#13720,#7061,.T.) ;
#17178 = EDGE_CURVE('',#13719,#13724,#7062,.T.) ;
#17179 = EDGE_CURVE('',#13721,#13725,#7063,.T.) ;
#17180 = EDGE_CURVE('',#13724,#13725,#7064,.T.) ;
#17181 = EDGE_CURVE('',#13725,#13723,#7065,.T.) ;
#17182 = EDGE_CURVE('',#13726,#13727,#7066,.T.) ;
#17183 = EDGE_CURVE('',#13726,#13728,#7067,.T.) ;
#17184 = EDGE_CURVE('',#13728,#13729,#7068,.T.) ;
#17185 = EDGE_CURVE('',#13727,#13729,#7069,.T.) ;
#17186 = EDGE_CURVE('',#13730,#13726,#7070,.T.) ;
#17187 = EDGE_CURVE('',#13731,#13730,#7071,.T.) ;
#17188 = EDGE_CURVE('',#13731,#13728,#7072,.T.) ;
#17189 = EDGE_CURVE('',#13727,#13732,#7073,.T.) ;
#17190 = EDGE_CURVE('',#13729,#13733,#7074,.T.) ;
#17191 = EDGE_CURVE('',#13732,#13733,#7075,.T.) ;
#17192 = EDGE_CURVE('',#13733,#13731,#7076,.T.) ;
#17193 = EDGE_CURVE('',#13734,#13735,#7077,.T.) ;
#17194 = EDGE_CURVE('',#13734,#13736,#7078,.T.) ;
#17195 = EDGE_CURVE('',#13736,#13737,#7079,.T.) ;
#17196 = EDGE_CURVE('',#13735,#13737,#7080,.T.) ;
#17197 = EDGE_CURVE('',#13738,#13734,#7081,.T.) ;
#17198 = EDGE_CURVE('',#13739,#13738,#7082,.T.) ;
#17199 = EDGE_CURVE('',#13739,#13736,#7083,.T.) ;
#17200 = EDGE_CURVE('',#13735,#13740,#7084,.T.) ;
#17201 = EDGE_CURVE('',#13737,#13741,#7085,.T.) ;
#17202 = EDGE_CURVE('',#13740,#13741,#7086,.T.) ;
#17203 = EDGE_CURVE('',#13741,#13739,#7087,.T.) ;
#17204 = EDGE_CURVE('',#13742,#13743,#7088,.T.) ;
#17205 = EDGE_CURVE('',#13742,#13744,#7089,.T.) ;
#17206 = EDGE_CURVE('',#13744,#13745,#7090,.T.) ;
#17207 = EDGE_CURVE('',#13743,#13745,#7091,.T.) ;
#17208 = EDGE_CURVE('',#13746,#13742,#7092,.T.) ;
#17209 = EDGE_CURVE('',#13746,#13747,#7093,.T.) ;
#17210 = EDGE_CURVE('',#13747,#13744,#7094,.T.) ;
#17211 = EDGE_CURVE('',#13748,#13746,#7095,.T.) ;
#17212 = EDGE_CURVE('',#13749,#13748,#7096,.T.) ;
#17213 = EDGE_CURVE('',#13749,#13747,#7097,.T.) ;
#17214 = EDGE_CURVE('',#13745,#13749,#7098,.T.) ;
#17215 = EDGE_CURVE('',#13750,#13751,#7099,.T.) ;
#17216 = EDGE_CURVE('',#13750,#13752,#7100,.T.) ;
#17217 = EDGE_CURVE('',#13752,#13753,#7101,.T.) ;
#17218 = EDGE_CURVE('',#13751,#13753,#7102,.T.) ;
#17219 = EDGE_CURVE('',#13754,#13750,#7103,.T.) ;
#17220 = EDGE_CURVE('',#13755,#13754,#7104,.T.) ;
#17221 = EDGE_CURVE('',#13755,#13752,#7105,.T.) ;
#17222 = EDGE_CURVE('',#13751,#13756,#7106,.T.) ;
#17223 = EDGE_CURVE('',#13753,#13757,#7107,.T.) ;
#17224 = EDGE_CURVE('',#13756,#13757,#7108,.T.) ;
#17225 = EDGE_CURVE('',#13757,#13755,#7109,.T.) ;
#17226 = EDGE_CURVE('',#13758,#13759,#7110,.T.) ;
#17227 = EDGE_CURVE('',#13758,#13760,#7111,.T.) ;
#17228 = EDGE_CURVE('',#13760,#13761,#7112,.T.) ;
#17229 = EDGE_CURVE('',#13759,#13761,#7113,.T.) ;
#17230 = EDGE_CURVE('',#13762,#13758,#7114,.T.) ;
#17231 = EDGE_CURVE('',#13763,#13762,#7115,.T.) ;
#17232 = EDGE_CURVE('',#13763,#13760,#7116,.T.) ;
#17233 = EDGE_CURVE('',#13759,#13764,#7117,.T.) ;
#17234 = EDGE_CURVE('',#13761,#13765,#7118,.T.) ;
#17235 = EDGE_CURVE('',#13764,#13765,#7119,.T.) ;
#17236 = EDGE_CURVE('',#13765,#13763,#7120,.T.) ;
#17237 = EDGE_CURVE('',#13724,#13698,#7121,.T.) ;
#17238 = EDGE_CURVE('',#13756,#13722,#7122,.T.) ;
#17239 = EDGE_CURVE('',#13740,#13754,#7123,.T.) ;
#17240 = EDGE_CURVE('',#13708,#13738,#7124,.T.) ;
#17241 = EDGE_CURVE('',#13711,#13706,#7125,.T.) ;
#17242 = EDGE_CURVE('',#13743,#13716,#7126,.T.) ;
#17243 = EDGE_CURVE('',#13766,#13748,#7127,.T.) ;
#17244 = EDGE_CURVE('',#13767,#13766,#7128,.T.) ;
#17245 = EDGE_CURVE('',#13767,#13768,#7129,.T.) ;
#17246 = EDGE_CURVE('',#13768,#13769,#7130,.T.) ;
#17247 = EDGE_CURVE('',#13769,#13770,#7131,.T.) ;
#17248 = EDGE_CURVE('',#13770,#13771,#7132,.T.) ;
#17249 = EDGE_CURVE('',#13771,#13772,#7133,.T.) ;
#17250 = EDGE_CURVE('',#13772,#13773,#7134,.T.) ;
#17251 = EDGE_CURVE('',#13773,#13774,#7135,.T.) ;
#17252 = EDGE_CURVE('',#13774,#13775,#7136,.T.) ;
#17253 = EDGE_CURVE('',#13775,#13776,#7137,.T.) ;
#17254 = EDGE_CURVE('',#13776,#13777,#7138,.T.) ;
#17255 = EDGE_CURVE('',#13777,#13778,#7139,.T.) ;
#17256 = EDGE_CURVE('',#13778,#13779,#7140,.T.) ;
#17257 = EDGE_CURVE('',#13779,#13780,#7141,.T.) ;
#17258 = EDGE_CURVE('',#13780,#13781,#7142,.T.) ;
#17259 = EDGE_CURVE('',#13781,#13782,#7143,.T.) ;
#17260 = EDGE_CURVE('',#13782,#13783,#7144,.T.) ;
#17261 = EDGE_CURVE('',#13783,#13784,#7145,.T.) ;
#17262 = EDGE_CURVE('',#13784,#13785,#7146,.T.) ;
#17263 = EDGE_CURVE('',#13785,#13786,#7147,.T.) ;
#17264 = EDGE_CURVE('',#13786,#13787,#7148,.T.) ;
#17265 = EDGE_CURVE('',#13787,#13788,#7149,.T.) ;
#17266 = EDGE_CURVE('',#13788,#13789,#7150,.T.) ;
#17267 = EDGE_CURVE('',#13789,#13790,#7151,.T.) ;
#17268 = EDGE_CURVE('',#13790,#13791,#7152,.T.) ;
#17269 = EDGE_CURVE('',#13791,#13792,#7153,.T.) ;
#17270 = EDGE_CURVE('',#13792,#13793,#7154,.T.) ;
#17271 = EDGE_CURVE('',#13793,#13794,#7155,.T.) ;
#17272 = EDGE_CURVE('',#13794,#13795,#7156,.T.) ;
#17273 = EDGE_CURVE('',#13795,#13796,#7157,.T.) ;
#17274 = EDGE_CURVE('',#13796,#13797,#7158,.T.) ;
#17275 = EDGE_CURVE('',#13797,#13798,#7159,.T.) ;
#17276 = EDGE_CURVE('',#13798,#13799,#7160,.T.) ;
#17277 = EDGE_CURVE('',#13799,#13800,#7161,.T.) ;
#17278 = EDGE_CURVE('',#13800,#13801,#7162,.T.) ;
#17279 = EDGE_CURVE('',#13801,#13802,#7163,.T.) ;
#17280 = EDGE_CURVE('',#13802,#13803,#7164,.T.) ;
#17281 = EDGE_CURVE('',#13803,#13804,#7165,.T.) ;
#17282 = EDGE_CURVE('',#13804,#13805,#7166,.T.) ;
#17283 = EDGE_CURVE('',#13764,#13805,#7167,.T.) ;
#17284 = EDGE_CURVE('',#13732,#13762,#7168,.T.) ;
#17285 = EDGE_CURVE('',#13700,#13730,#7169,.T.) ;
#17286 = EDGE_CURVE('',#13806,#13806,#11304,.T.) ;
#17287 = EDGE_CURVE('',#13806,#13807,#11305,.T.) ;
#17288 = EDGE_CURVE('',#13807,#13807,#11306,.T.) ;
#17289 = EDGE_CURVE('',#13808,#13808,#11307,.T.) ;
#17290 = EDGE_CURVE('',#13808,#13806,#7170,.T.) ;
#17291 = EDGE_CURVE('',#13809,#13810,#7171,.T.) ;
#17292 = EDGE_CURVE('',#13811,#13809,#7172,.T.) ;
#17293 = EDGE_CURVE('',#13812,#13811,#7173,.T.) ;
#17294 = EDGE_CURVE('',#13810,#13812,#7174,.T.) ;
#17295 = EDGE_CURVE('',#13813,#13814,#7175,.T.) ;
#17296 = EDGE_CURVE('',#13815,#13814,#11308,.T.) ;
#17297 = EDGE_CURVE('',#13815,#13816,#7176,.T.) ;
#17298 = EDGE_CURVE('',#13817,#13816,#11309,.T.) ;
#17299 = EDGE_CURVE('',#13817,#13818,#7177,.T.) ;
#17300 = EDGE_CURVE('',#13819,#13818,#11310,.T.) ;
#17301 = EDGE_CURVE('',#13819,#13820,#7178,.T.) ;
#17302 = EDGE_CURVE('',#13813,#13820,#11311,.T.) ;
#17303 = EDGE_CURVE('',#13821,#13821,#11312,.T.) ;
#17304 = EDGE_CURVE('',#13821,#13822,#11313,.T.) ;
#17305 = EDGE_CURVE('',#13822,#13822,#11314,.T.) ;
#17306 = EDGE_CURVE('',#13823,#13823,#11315,.T.) ;
#17307 = EDGE_CURVE('',#13823,#13821,#7179,.T.) ;
#17308 = EDGE_CURVE('',#13824,#13825,#7180,.T.) ;
#17309 = EDGE_CURVE('',#13826,#13824,#7181,.T.) ;
#17310 = EDGE_CURVE('',#13827,#13826,#7182,.T.) ;
#17311 = EDGE_CURVE('',#13825,#13827,#7183,.T.) ;
#17312 = EDGE_CURVE('',#13828,#13829,#7184,.T.) ;
#17313 = EDGE_CURVE('',#13830,#13829,#11316,.T.) ;
#17314 = EDGE_CURVE('',#13830,#13831,#7185,.T.) ;
#17315 = EDGE_CURVE('',#13832,#13831,#11317,.T.) ;
#17316 = EDGE_CURVE('',#13832,#13833,#7186,.T.) ;
#17317 = EDGE_CURVE('',#13834,#13833,#11318,.T.) ;
#17318 = EDGE_CURVE('',#13834,#13835,#7187,.T.) ;
#17319 = EDGE_CURVE('',#13828,#13835,#11319,.T.) ;
#17320 = EDGE_CURVE('',#13836,#13836,#11320,.T.) ;
#17321 = EDGE_CURVE('',#13836,#13837,#11321,.T.) ;
#17322 = EDGE_CURVE('',#13837,#13837,#11322,.T.) ;
#17323 = EDGE_CURVE('',#13838,#13838,#11323,.T.) ;
#17324 = EDGE_CURVE('',#13838,#13836,#7188,.T.) ;
#17325 = EDGE_CURVE('',#13839,#13840,#7189,.T.) ;
#17326 = EDGE_CURVE('',#13841,#13839,#7190,.T.) ;
#17327 = EDGE_CURVE('',#13842,#13841,#7191,.T.) ;
#17328 = EDGE_CURVE('',#13840,#13842,#7192,.T.) ;
#17329 = EDGE_CURVE('',#13843,#13844,#7193,.T.) ;
#17330 = EDGE_CURVE('',#13845,#13844,#11324,.T.) ;
#17331 = EDGE_CURVE('',#13845,#13846,#7194,.T.) ;
#17332 = EDGE_CURVE('',#13847,#13846,#11325,.T.) ;
#17333 = EDGE_CURVE('',#13847,#13848,#7195,.T.) ;
#17334 = EDGE_CURVE('',#13849,#13848,#11326,.T.) ;
#17335 = EDGE_CURVE('',#13849,#13850,#7196,.T.) ;
#17336 = EDGE_CURVE('',#13843,#13850,#11327,.T.) ;
#17337 = EDGE_CURVE('',#13851,#13851,#11328,.T.) ;
#17338 = EDGE_CURVE('',#13851,#13852,#11329,.T.) ;
#17339 = EDGE_CURVE('',#13852,#13852,#11330,.T.) ;
#17340 = EDGE_CURVE('',#13853,#13853,#11331,.T.) ;
#17341 = EDGE_CURVE('',#13853,#13851,#7197,.T.) ;
#17342 = EDGE_CURVE('',#13854,#13855,#7198,.T.) ;
#17343 = EDGE_CURVE('',#13856,#13854,#7199,.T.) ;
#17344 = EDGE_CURVE('',#13857,#13856,#7200,.T.) ;
#17345 = EDGE_CURVE('',#13855,#13857,#7201,.T.) ;
#17346 = EDGE_CURVE('',#13858,#13859,#7202,.T.) ;
#17347 = EDGE_CURVE('',#13860,#13859,#11332,.T.) ;
#17348 = EDGE_CURVE('',#13860,#13861,#7203,.T.) ;
#17349 = EDGE_CURVE('',#13862,#13861,#11333,.T.) ;
#17350 = EDGE_CURVE('',#13862,#13863,#7204,.T.) ;
#17351 = EDGE_CURVE('',#13864,#13863,#11334,.T.) ;
#17352 = EDGE_CURVE('',#13864,#13865,#7205,.T.) ;
#17353 = EDGE_CURVE('',#13858,#13865,#11335,.T.) ;
#17354 = EDGE_CURVE('',#13866,#13866,#11336,.T.) ;
#17355 = EDGE_CURVE('',#13866,#13867,#11337,.T.) ;
#17356 = EDGE_CURVE('',#13867,#13867,#11338,.T.) ;
#17357 = EDGE_CURVE('',#13868,#13868,#11339,.T.) ;
#17358 = EDGE_CURVE('',#13868,#13866,#7206,.T.) ;
#17359 = EDGE_CURVE('',#13869,#13870,#7207,.T.) ;
#17360 = EDGE_CURVE('',#13871,#13869,#7208,.T.) ;
#17361 = EDGE_CURVE('',#13872,#13871,#7209,.T.) ;
#17362 = EDGE_CURVE('',#13870,#13872,#7210,.T.) ;
#17363 = EDGE_CURVE('',#13873,#13874,#7211,.T.) ;
#17364 = EDGE_CURVE('',#13875,#13874,#11340,.T.) ;
#17365 = EDGE_CURVE('',#13875,#13876,#7212,.T.) ;
#17366 = EDGE_CURVE('',#13877,#13876,#11341,.T.) ;
#17367 = EDGE_CURVE('',#13877,#13878,#7213,.T.) ;
#17368 = EDGE_CURVE('',#13879,#13878,#11342,.T.) ;
#17369 = EDGE_CURVE('',#13879,#13880,#7214,.T.) ;
#17370 = EDGE_CURVE('',#13873,#13880,#11343,.T.) ;
#17371 = EDGE_CURVE('',#13881,#13881,#11344,.T.) ;
#17372 = EDGE_CURVE('',#13881,#13882,#11345,.T.) ;
#17373 = EDGE_CURVE('',#13882,#13882,#11346,.T.) ;
#17374 = EDGE_CURVE('',#13883,#13883,#11347,.T.) ;
#17375 = EDGE_CURVE('',#13883,#13881,#7215,.T.) ;
#17376 = EDGE_CURVE('',#13884,#13885,#7216,.T.) ;
#17377 = EDGE_CURVE('',#13886,#13884,#7217,.T.) ;
#17378 = EDGE_CURVE('',#13887,#13886,#7218,.T.) ;
#17379 = EDGE_CURVE('',#13885,#13887,#7219,.T.) ;
#17380 = EDGE_CURVE('',#13888,#13889,#7220,.T.) ;
#17381 = EDGE_CURVE('',#13890,#13889,#11348,.T.) ;
#17382 = EDGE_CURVE('',#13890,#13891,#7221,.T.) ;
#17383 = EDGE_CURVE('',#13892,#13891,#11349,.T.) ;
#17384 = EDGE_CURVE('',#13892,#13893,#7222,.T.) ;
#17385 = EDGE_CURVE('',#13894,#13893,#11350,.T.) ;
#17386 = EDGE_CURVE('',#13894,#13895,#7223,.T.) ;
#17387 = EDGE_CURVE('',#13888,#13895,#11351,.T.) ;
#17388 = EDGE_CURVE('',#13896,#13896,#11352,.T.) ;
#17389 = EDGE_CURVE('',#13896,#13897,#11353,.T.) ;
#17390 = EDGE_CURVE('',#13897,#13897,#11354,.T.) ;
#17391 = EDGE_CURVE('',#13898,#13898,#11355,.T.) ;
#17392 = EDGE_CURVE('',#13898,#13896,#7224,.T.) ;
#17393 = EDGE_CURVE('',#13899,#13900,#7225,.T.) ;
#17394 = EDGE_CURVE('',#13901,#13899,#7226,.T.) ;
#17395 = EDGE_CURVE('',#13902,#13901,#7227,.T.) ;
#17396 = EDGE_CURVE('',#13900,#13902,#7228,.T.) ;
#17397 = EDGE_CURVE('',#13903,#13904,#7229,.T.) ;
#17398 = EDGE_CURVE('',#13905,#13904,#11356,.T.) ;
#17399 = EDGE_CURVE('',#13905,#13906,#7230,.T.) ;
#17400 = EDGE_CURVE('',#13907,#13906,#11357,.T.) ;
#17401 = EDGE_CURVE('',#13907,#13908,#7231,.T.) ;
#17402 = EDGE_CURVE('',#13909,#13908,#11358,.T.) ;
#17403 = EDGE_CURVE('',#13909,#13910,#7232,.T.) ;
#17404 = EDGE_CURVE('',#13903,#13910,#11359,.T.) ;
#17405 = EDGE_CURVE('',#13911,#13911,#11360,.T.) ;
#17406 = EDGE_CURVE('',#13911,#13912,#11361,.T.) ;
#17407 = EDGE_CURVE('',#13912,#13912,#11362,.T.) ;
#17408 = EDGE_CURVE('',#13913,#13913,#11363,.T.) ;
#17409 = EDGE_CURVE('',#13913,#13911,#7233,.T.) ;
#17410 = EDGE_CURVE('',#13914,#13915,#7234,.T.) ;
#17411 = EDGE_CURVE('',#13916,#13914,#7235,.T.) ;
#17412 = EDGE_CURVE('',#13917,#13916,#7236,.T.) ;
#17413 = EDGE_CURVE('',#13915,#13917,#7237,.T.) ;
#17414 = EDGE_CURVE('',#13918,#13919,#7238,.T.) ;
#17415 = EDGE_CURVE('',#13920,#13919,#11364,.T.) ;
#17416 = EDGE_CURVE('',#13920,#13921,#7239,.T.) ;
#17417 = EDGE_CURVE('',#13922,#13921,#11365,.T.) ;
#17418 = EDGE_CURVE('',#13922,#13923,#7240,.T.) ;
#17419 = EDGE_CURVE('',#13924,#13923,#11366,.T.) ;
#17420 = EDGE_CURVE('',#13924,#13925,#7241,.T.) ;
#17421 = EDGE_CURVE('',#13918,#13925,#11367,.T.) ;
#17422 = EDGE_CURVE('',#13926,#13926,#11368,.T.) ;
#17423 = EDGE_CURVE('',#13926,#13927,#11369,.T.) ;
#17424 = EDGE_CURVE('',#13927,#13927,#11370,.T.) ;
#17425 = EDGE_CURVE('',#13928,#13929,#7242,.T.) ;
#17426 = EDGE_CURVE('',#13930,#13928,#7243,.T.) ;
#17427 = EDGE_CURVE('',#13931,#13930,#7244,.T.) ;
#17428 = EDGE_CURVE('',#13929,#13931,#7245,.T.) ;
#17429 = EDGE_CURVE('',#13932,#13933,#7246,.T.) ;
#17430 = EDGE_CURVE('',#13934,#13932,#11371,.T.) ;
#17431 = EDGE_CURVE('',#13935,#13934,#7247,.T.) ;
#17432 = EDGE_CURVE('',#13936,#13935,#11372,.T.) ;
#17433 = EDGE_CURVE('',#13937,#13936,#7248,.T.) ;
#17434 = EDGE_CURVE('',#13938,#13937,#11373,.T.) ;
#17435 = EDGE_CURVE('',#13939,#13938,#7249,.T.) ;
#17436 = EDGE_CURVE('',#13933,#13939,#11374,.T.) ;
#17437 = EDGE_CURVE('',#13940,#13940,#11375,.F.) ;
#17438 = EDGE_CURVE('',#13940,#13926,#7250,.T.) ;
#17439 = EDGE_CURVE('',#13941,#13941,#11376,.T.) ;
#17440 = EDGE_CURVE('',#13942,#13942,#11377,.T.) ;
#17441 = EDGE_CURVE('',#13943,#13943,#11378,.T.) ;
#17442 = EDGE_CURVE('',#13944,#13944,#11379,.T.) ;
#17443 = EDGE_CURVE('',#13945,#13945,#11380,.T.) ;
#17444 = EDGE_CURVE('',#13946,#13946,#11381,.T.) ;
#17445 = EDGE_CURVE('',#13947,#13947,#11382,.T.) ;
#17446 = EDGE_CURVE('',#13948,#13948,#11383,.T.) ;
#17447 = EDGE_CURVE('',#13813,#13949,#11384,.T.) ;
#17448 = EDGE_CURVE('',#13949,#13950,#7251,.T.) ;
#17449 = EDGE_CURVE('',#13950,#13814,#11385,.T.) ;
#17450 = EDGE_CURVE('',#13951,#13815,#11386,.T.) ;
#17451 = EDGE_CURVE('',#13951,#13950,#11387,.T.) ;
#17452 = EDGE_CURVE('',#13952,#13816,#11388,.T.) ;
#17453 = EDGE_CURVE('',#13951,#13952,#7252,.T.) ;
#17454 = EDGE_CURVE('',#13953,#13817,#11389,.T.) ;
#17455 = EDGE_CURVE('',#13952,#13953,#11390,.T.) ;
#17456 = EDGE_CURVE('',#13954,#13818,#11391,.T.) ;
#17457 = EDGE_CURVE('',#13953,#13954,#7253,.T.) ;
#17458 = EDGE_CURVE('',#13955,#13819,#11392,.T.) ;
#17459 = EDGE_CURVE('',#13955,#13954,#11393,.T.) ;
#17460 = EDGE_CURVE('',#13956,#13820,#11394,.T.) ;
#17461 = EDGE_CURVE('',#13955,#13956,#7254,.T.) ;
#17462 = EDGE_CURVE('',#13956,#13949,#11395,.T.) ;
#17463 = EDGE_CURVE('',#13957,#13952,#7255,.T.) ;
#17464 = EDGE_CURVE('',#13958,#13957,#11396,.T.) ;
#17465 = EDGE_CURVE('',#13953,#13958,#7256,.T.) ;
#17466 = EDGE_CURVE('',#13951,#13959,#7257,.T.) ;
#17467 = EDGE_CURVE('',#13959,#13960,#11397,.T.) ;
#17468 = EDGE_CURVE('',#13960,#13961,#7258,.T.) ;
#17469 = EDGE_CURVE('',#13961,#13962,#7259,.T.) ;
#17470 = EDGE_CURVE('',#13963,#13962,#7260,.T.) ;
#17471 = EDGE_CURVE('',#13963,#13964,#7261,.T.) ;
#17472 = EDGE_CURVE('',#13964,#13965,#7262,.T.) ;
#17473 = EDGE_CURVE('',#13965,#13957,#11398,.T.) ;
#17474 = EDGE_CURVE('',#13966,#13950,#7263,.T.) ;
#17475 = EDGE_CURVE('',#13959,#13966,#11399,.T.) ;
#17476 = EDGE_CURVE('',#13949,#13967,#7264,.T.) ;
#17477 = EDGE_CURVE('',#13967,#13966,#7265,.T.) ;
#17478 = EDGE_CURVE('',#13828,#13968,#11400,.T.) ;
#17479 = EDGE_CURVE('',#13968,#13969,#7266,.T.) ;
#17480 = EDGE_CURVE('',#13969,#13829,#11401,.T.) ;
#17481 = EDGE_CURVE('',#13970,#13830,#11402,.T.) ;
#17482 = EDGE_CURVE('',#13970,#13969,#11403,.T.) ;
#17483 = EDGE_CURVE('',#13971,#13831,#11404,.T.) ;
#17484 = EDGE_CURVE('',#13970,#13971,#7267,.T.) ;
#17485 = EDGE_CURVE('',#13972,#13832,#11405,.T.) ;
#17486 = EDGE_CURVE('',#13971,#13972,#11406,.T.) ;
#17487 = EDGE_CURVE('',#13973,#13833,#11407,.T.) ;
#17488 = EDGE_CURVE('',#13972,#13973,#7268,.T.) ;
#17489 = EDGE_CURVE('',#13974,#13834,#11408,.T.) ;
#17490 = EDGE_CURVE('',#13974,#13973,#11409,.T.) ;
#17491 = EDGE_CURVE('',#13975,#13835,#11410,.T.) ;
#17492 = EDGE_CURVE('',#13974,#13975,#7269,.T.) ;
#17493 = EDGE_CURVE('',#13975,#13968,#11411,.T.) ;
#17494 = EDGE_CURVE('',#13976,#13971,#7270,.T.) ;
#17495 = EDGE_CURVE('',#13977,#13976,#11412,.T.) ;
#17496 = EDGE_CURVE('',#13972,#13977,#7271,.T.) ;
#17497 = EDGE_CURVE('',#13970,#13978,#7272,.T.) ;
#17498 = EDGE_CURVE('',#13978,#13979,#11413,.T.) ;
#17499 = EDGE_CURVE('',#13979,#13980,#7273,.T.) ;
#17500 = EDGE_CURVE('',#13980,#13981,#7274,.T.) ;
#17501 = EDGE_CURVE('',#13982,#13981,#7275,.T.) ;
#17502 = EDGE_CURVE('',#13982,#13983,#7276,.T.) ;
#17503 = EDGE_CURVE('',#13983,#13984,#7277,.T.) ;
#17504 = EDGE_CURVE('',#13984,#13976,#11414,.T.) ;
#17505 = EDGE_CURVE('',#13985,#13969,#7278,.T.) ;
#17506 = EDGE_CURVE('',#13978,#13985,#11415,.T.) ;
#17507 = EDGE_CURVE('',#13968,#13986,#7279,.T.) ;
#17508 = EDGE_CURVE('',#13986,#13985,#7280,.T.) ;
#17509 = EDGE_CURVE('',#13843,#13987,#11416,.T.) ;
#17510 = EDGE_CURVE('',#13987,#13988,#7281,.T.) ;
#17511 = EDGE_CURVE('',#13988,#13844,#11417,.T.) ;
#17512 = EDGE_CURVE('',#13989,#13845,#11418,.T.) ;
#17513 = EDGE_CURVE('',#13989,#13988,#11419,.T.) ;
#17514 = EDGE_CURVE('',#13990,#13846,#11420,.T.) ;
#17515 = EDGE_CURVE('',#13989,#13990,#7282,.T.) ;
#17516 = EDGE_CURVE('',#13991,#13847,#11421,.T.) ;
#17517 = EDGE_CURVE('',#13990,#13991,#11422,.T.) ;
#17518 = EDGE_CURVE('',#13992,#13848,#11423,.T.) ;
#17519 = EDGE_CURVE('',#13991,#13992,#7283,.T.) ;
#17520 = EDGE_CURVE('',#13993,#13849,#11424,.T.) ;
#17521 = EDGE_CURVE('',#13993,#13992,#11425,.T.) ;
#17522 = EDGE_CURVE('',#13994,#13850,#11426,.T.) ;
#17523 = EDGE_CURVE('',#13993,#13994,#7284,.T.) ;
#17524 = EDGE_CURVE('',#13994,#13987,#11427,.T.) ;
#17525 = EDGE_CURVE('',#13995,#13990,#7285,.T.) ;
#17526 = EDGE_CURVE('',#13996,#13995,#11428,.T.) ;
#17527 = EDGE_CURVE('',#13991,#13996,#7286,.T.) ;
#17528 = EDGE_CURVE('',#13989,#13997,#7287,.T.) ;
#17529 = EDGE_CURVE('',#13997,#13998,#11429,.T.) ;
#17530 = EDGE_CURVE('',#13998,#13999,#7288,.T.) ;
#17531 = EDGE_CURVE('',#13999,#14000,#7289,.T.) ;
#17532 = EDGE_CURVE('',#14001,#14000,#7290,.T.) ;
#17533 = EDGE_CURVE('',#14001,#14002,#7291,.T.) ;
#17534 = EDGE_CURVE('',#14002,#14003,#7292,.T.) ;
#17535 = EDGE_CURVE('',#14003,#13995,#11430,.T.) ;
#17536 = EDGE_CURVE('',#14004,#13988,#7293,.T.) ;
#17537 = EDGE_CURVE('',#13997,#14004,#11431,.T.) ;
#17538 = EDGE_CURVE('',#13987,#14005,#7294,.T.) ;
#17539 = EDGE_CURVE('',#14005,#14004,#7295,.T.) ;
#17540 = EDGE_CURVE('',#13858,#14006,#11432,.T.) ;
#17541 = EDGE_CURVE('',#14006,#14007,#7296,.T.) ;
#17542 = EDGE_CURVE('',#14007,#13859,#11433,.T.) ;
#17543 = EDGE_CURVE('',#14008,#13860,#11434,.T.) ;
#17544 = EDGE_CURVE('',#14008,#14007,#11435,.T.) ;
#17545 = EDGE_CURVE('',#14009,#13861,#11436,.T.) ;
#17546 = EDGE_CURVE('',#14008,#14009,#7297,.T.) ;
#17547 = EDGE_CURVE('',#14010,#13862,#11437,.T.) ;
#17548 = EDGE_CURVE('',#14009,#14010,#11438,.T.) ;
#17549 = EDGE_CURVE('',#14011,#13863,#11439,.T.) ;
#17550 = EDGE_CURVE('',#14010,#14011,#7298,.T.) ;
#17551 = EDGE_CURVE('',#14012,#13864,#11440,.T.) ;
#17552 = EDGE_CURVE('',#14012,#14011,#11441,.T.) ;
#17553 = EDGE_CURVE('',#14013,#13865,#11442,.T.) ;
#17554 = EDGE_CURVE('',#14012,#14013,#7299,.T.) ;
#17555 = EDGE_CURVE('',#14013,#14006,#11443,.T.) ;
#17556 = EDGE_CURVE('',#14014,#14009,#7300,.T.) ;
#17557 = EDGE_CURVE('',#14015,#14014,#11444,.T.) ;
#17558 = EDGE_CURVE('',#14010,#14015,#7301,.T.) ;
#17559 = EDGE_CURVE('',#14008,#14016,#7302,.T.) ;
#17560 = EDGE_CURVE('',#14016,#14017,#11445,.T.) ;
#17561 = EDGE_CURVE('',#14017,#14018,#7303,.T.) ;
#17562 = EDGE_CURVE('',#14018,#14019,#7304,.T.) ;
#17563 = EDGE_CURVE('',#14020,#14019,#7305,.T.) ;
#17564 = EDGE_CURVE('',#14020,#14021,#7306,.T.) ;
#17565 = EDGE_CURVE('',#14021,#14022,#7307,.T.) ;
#17566 = EDGE_CURVE('',#14022,#14014,#11446,.T.) ;
#17567 = EDGE_CURVE('',#14023,#14007,#7308,.T.) ;
#17568 = EDGE_CURVE('',#14016,#14023,#11447,.T.) ;
#17569 = EDGE_CURVE('',#14006,#14024,#7309,.T.) ;
#17570 = EDGE_CURVE('',#14024,#14023,#7310,.T.) ;
#17571 = EDGE_CURVE('',#13873,#14025,#11448,.T.) ;
#17572 = EDGE_CURVE('',#14025,#14026,#7311,.T.) ;
#17573 = EDGE_CURVE('',#14026,#13874,#11449,.T.) ;
#17574 = EDGE_CURVE('',#14027,#13875,#11450,.T.) ;
#17575 = EDGE_CURVE('',#14027,#14026,#11451,.T.) ;
#17576 = EDGE_CURVE('',#14028,#13876,#11452,.T.) ;
#17577 = EDGE_CURVE('',#14027,#14028,#7312,.T.) ;
#17578 = EDGE_CURVE('',#14029,#13877,#11453,.T.) ;
#17579 = EDGE_CURVE('',#14028,#14029,#11454,.T.) ;
#17580 = EDGE_CURVE('',#14030,#13878,#11455,.T.) ;
#17581 = EDGE_CURVE('',#14029,#14030,#7313,.T.) ;
#17582 = EDGE_CURVE('',#14031,#13879,#11456,.T.) ;
#17583 = EDGE_CURVE('',#14031,#14030,#11457,.T.) ;
#17584 = EDGE_CURVE('',#14032,#13880,#11458,.T.) ;
#17585 = EDGE_CURVE('',#14031,#14032,#7314,.T.) ;
#17586 = EDGE_CURVE('',#14032,#14025,#11459,.T.) ;
#17587 = EDGE_CURVE('',#14033,#14028,#7315,.T.) ;
#17588 = EDGE_CURVE('',#14034,#14033,#11460,.T.) ;
#17589 = EDGE_CURVE('',#14029,#14034,#7316,.T.) ;
#17590 = EDGE_CURVE('',#14027,#14035,#7317,.T.) ;
#17591 = EDGE_CURVE('',#14035,#14036,#11461,.T.) ;
#17592 = EDGE_CURVE('',#14036,#14037,#7318,.T.) ;
#17593 = EDGE_CURVE('',#14037,#14038,#7319,.T.) ;
#17594 = EDGE_CURVE('',#14039,#14038,#7320,.T.) ;
#17595 = EDGE_CURVE('',#14039,#14040,#7321,.T.) ;
#17596 = EDGE_CURVE('',#14040,#14041,#7322,.T.) ;
#17597 = EDGE_CURVE('',#14041,#14033,#11462,.T.) ;
#17598 = EDGE_CURVE('',#14042,#14026,#7323,.T.) ;
#17599 = EDGE_CURVE('',#14035,#14042,#11463,.T.) ;
#17600 = EDGE_CURVE('',#14025,#14043,#7324,.T.) ;
#17601 = EDGE_CURVE('',#14043,#14042,#7325,.T.) ;
#17602 = EDGE_CURVE('',#13888,#14044,#11464,.T.) ;
#17603 = EDGE_CURVE('',#14044,#14045,#7326,.T.) ;
#17604 = EDGE_CURVE('',#14045,#13889,#11465,.T.) ;
#17605 = EDGE_CURVE('',#14046,#13890,#11466,.T.) ;
#17606 = EDGE_CURVE('',#14046,#14045,#11467,.T.) ;
#17607 = EDGE_CURVE('',#14047,#13891,#11468,.T.) ;
#17608 = EDGE_CURVE('',#14046,#14047,#7327,.T.) ;
#17609 = EDGE_CURVE('',#14048,#13892,#11469,.T.) ;
#17610 = EDGE_CURVE('',#14047,#14048,#11470,.T.) ;
#17611 = EDGE_CURVE('',#14049,#13893,#11471,.T.) ;
#17612 = EDGE_CURVE('',#14048,#14049,#7328,.T.) ;
#17613 = EDGE_CURVE('',#14050,#13894,#11472,.T.) ;
#17614 = EDGE_CURVE('',#14050,#14049,#11473,.T.) ;
#17615 = EDGE_CURVE('',#14051,#13895,#11474,.T.) ;
#17616 = EDGE_CURVE('',#14050,#14051,#7329,.T.) ;
#17617 = EDGE_CURVE('',#14051,#14044,#11475,.T.) ;
#17618 = EDGE_CURVE('',#14052,#14047,#7330,.T.) ;
#17619 = EDGE_CURVE('',#14053,#14052,#11476,.T.) ;
#17620 = EDGE_CURVE('',#14048,#14053,#7331,.T.) ;
#17621 = EDGE_CURVE('',#14046,#14054,#7332,.T.) ;
#17622 = EDGE_CURVE('',#14054,#14055,#11477,.T.) ;
#17623 = EDGE_CURVE('',#14055,#14056,#7333,.T.) ;
#17624 = EDGE_CURVE('',#14056,#14057,#7334,.T.) ;
#17625 = EDGE_CURVE('',#14058,#14057,#7335,.T.) ;
#17626 = EDGE_CURVE('',#14058,#14059,#7336,.T.) ;
#17627 = EDGE_CURVE('',#14059,#14060,#7337,.T.) ;
#17628 = EDGE_CURVE('',#14060,#14052,#11478,.T.) ;
#17629 = EDGE_CURVE('',#14061,#14045,#7338,.T.) ;
#17630 = EDGE_CURVE('',#14054,#14061,#11479,.T.) ;
#17631 = EDGE_CURVE('',#14044,#14062,#7339,.T.) ;
#17632 = EDGE_CURVE('',#14062,#14061,#7340,.T.) ;
#17633 = EDGE_CURVE('',#13903,#14063,#11480,.T.) ;
#17634 = EDGE_CURVE('',#14063,#14064,#7341,.T.) ;
#17635 = EDGE_CURVE('',#14064,#13904,#11481,.T.) ;
#17636 = EDGE_CURVE('',#14065,#13905,#11482,.T.) ;
#17637 = EDGE_CURVE('',#14065,#14064,#11483,.T.) ;
#17638 = EDGE_CURVE('',#14066,#13906,#11484,.T.) ;
#17639 = EDGE_CURVE('',#14065,#14066,#7342,.T.) ;
#17640 = EDGE_CURVE('',#14067,#13907,#11485,.T.) ;
#17641 = EDGE_CURVE('',#14066,#14067,#11486,.T.) ;
#17642 = EDGE_CURVE('',#14068,#13908,#11487,.T.) ;
#17643 = EDGE_CURVE('',#14067,#14068,#7343,.T.) ;
#17644 = EDGE_CURVE('',#14069,#13909,#11488,.T.) ;
#17645 = EDGE_CURVE('',#14069,#14068,#11489,.T.) ;
#17646 = EDGE_CURVE('',#14070,#13910,#11490,.T.) ;
#17647 = EDGE_CURVE('',#14069,#14070,#7344,.T.) ;
#17648 = EDGE_CURVE('',#14070,#14063,#11491,.T.) ;
#17649 = EDGE_CURVE('',#14071,#14066,#7345,.T.) ;
#17650 = EDGE_CURVE('',#14072,#14071,#11492,.T.) ;
#17651 = EDGE_CURVE('',#14067,#14072,#7346,.T.) ;
#17652 = EDGE_CURVE('',#14065,#14073,#7347,.T.) ;
#17653 = EDGE_CURVE('',#14073,#14074,#11493,.T.) ;
#17654 = EDGE_CURVE('',#14074,#14075,#7348,.T.) ;
#17655 = EDGE_CURVE('',#14075,#14076,#7349,.T.) ;
#17656 = EDGE_CURVE('',#14077,#14076,#7350,.T.) ;
#17657 = EDGE_CURVE('',#14077,#14078,#7351,.T.) ;
#17658 = EDGE_CURVE('',#14078,#14079,#7352,.T.) ;
#17659 = EDGE_CURVE('',#14079,#14071,#11494,.T.) ;
#17660 = EDGE_CURVE('',#14080,#14064,#7353,.T.) ;
#17661 = EDGE_CURVE('',#14073,#14080,#11495,.T.) ;
#17662 = EDGE_CURVE('',#14063,#14081,#7354,.T.) ;
#17663 = EDGE_CURVE('',#14081,#14080,#7355,.T.) ;
#17664 = EDGE_CURVE('',#13918,#14082,#11496,.T.) ;
#17665 = EDGE_CURVE('',#14082,#14083,#7356,.T.) ;
#17666 = EDGE_CURVE('',#14083,#13919,#11497,.T.) ;
#17667 = EDGE_CURVE('',#14084,#13920,#11498,.T.) ;
#17668 = EDGE_CURVE('',#14084,#14083,#11499,.T.) ;
#17669 = EDGE_CURVE('',#14085,#13921,#11500,.T.) ;
#17670 = EDGE_CURVE('',#14084,#14085,#7357,.T.) ;
#17671 = EDGE_CURVE('',#14086,#13922,#11501,.T.) ;
#17672 = EDGE_CURVE('',#14085,#14086,#11502,.T.) ;
#17673 = EDGE_CURVE('',#14087,#13923,#11503,.T.) ;
#17674 = EDGE_CURVE('',#14086,#14087,#7358,.T.) ;
#17675 = EDGE_CURVE('',#14088,#13924,#11504,.T.) ;
#17676 = EDGE_CURVE('',#14088,#14087,#11505,.T.) ;
#17677 = EDGE_CURVE('',#14089,#13925,#11506,.T.) ;
#17678 = EDGE_CURVE('',#14088,#14089,#7359,.T.) ;
#17679 = EDGE_CURVE('',#14089,#14082,#11507,.T.) ;
#17680 = EDGE_CURVE('',#14090,#14085,#7360,.T.) ;
#17681 = EDGE_CURVE('',#14091,#14090,#11508,.T.) ;
#17682 = EDGE_CURVE('',#14086,#14091,#7361,.T.) ;
#17683 = EDGE_CURVE('',#14084,#14092,#7362,.T.) ;
#17684 = EDGE_CURVE('',#14092,#14093,#11509,.T.) ;
#17685 = EDGE_CURVE('',#14093,#14094,#7363,.T.) ;
#17686 = EDGE_CURVE('',#14094,#14095,#7364,.T.) ;
#17687 = EDGE_CURVE('',#14096,#14095,#7365,.T.) ;
#17688 = EDGE_CURVE('',#14096,#14097,#7366,.T.) ;
#17689 = EDGE_CURVE('',#14097,#14098,#7367,.T.) ;
#17690 = EDGE_CURVE('',#14098,#14090,#11510,.T.) ;
#17691 = EDGE_CURVE('',#14099,#14083,#7368,.T.) ;
#17692 = EDGE_CURVE('',#14092,#14099,#11511,.T.) ;
#17693 = EDGE_CURVE('',#14082,#14100,#7369,.T.) ;
#17694 = EDGE_CURVE('',#14100,#14099,#7370,.T.) ;
#17695 = EDGE_CURVE('',#13933,#14101,#11512,.T.) ;
#17696 = EDGE_CURVE('',#14101,#14102,#7371,.T.) ;
#17697 = EDGE_CURVE('',#14102,#13932,#11513,.T.) ;
#17698 = EDGE_CURVE('',#14103,#13934,#11514,.T.) ;
#17699 = EDGE_CURVE('',#14102,#14103,#11515,.T.) ;
#17700 = EDGE_CURVE('',#14104,#13935,#11516,.T.) ;
#17701 = EDGE_CURVE('',#14103,#14104,#7372,.T.) ;
#17702 = EDGE_CURVE('',#14105,#13936,#11517,.T.) ;
#17703 = EDGE_CURVE('',#14104,#14105,#11518,.T.) ;
#17704 = EDGE_CURVE('',#14106,#13937,#11519,.T.) ;
#17705 = EDGE_CURVE('',#14105,#14106,#7373,.T.) ;
#17706 = EDGE_CURVE('',#14107,#13938,#11520,.T.) ;
#17707 = EDGE_CURVE('',#14106,#14107,#11521,.T.) ;
#17708 = EDGE_CURVE('',#14108,#13939,#11522,.T.) ;
#17709 = EDGE_CURVE('',#14107,#14108,#7374,.T.) ;
#17710 = EDGE_CURVE('',#14108,#14101,#11523,.T.) ;
#17711 = EDGE_CURVE('',#14109,#14104,#7375,.T.) ;
#17712 = EDGE_CURVE('',#14110,#14109,#11524,.T.) ;
#17713 = EDGE_CURVE('',#14105,#14110,#7376,.T.) ;
#17714 = EDGE_CURVE('',#14111,#14112,#7377,.T.) ;
#17715 = EDGE_CURVE('',#14111,#14113,#7378,.T.) ;
#17716 = EDGE_CURVE('',#14113,#14114,#7379,.T.) ;
#17717 = EDGE_CURVE('',#14114,#14109,#11525,.T.) ;
#17718 = EDGE_CURVE('',#14103,#14115,#7380,.T.) ;
#17719 = EDGE_CURVE('',#14115,#14116,#11526,.T.) ;
#17720 = EDGE_CURVE('',#14116,#14117,#7381,.T.) ;
#17721 = EDGE_CURVE('',#14117,#14112,#7382,.T.) ;
#17722 = EDGE_CURVE('',#14118,#14102,#7383,.T.) ;
#17723 = EDGE_CURVE('',#14115,#14118,#11527,.T.) ;
#17724 = EDGE_CURVE('',#14101,#14119,#7384,.T.) ;
#17725 = EDGE_CURVE('',#14119,#14118,#7385,.T.) ;
#17726 = EDGE_CURVE('',#14120,#14121,#11528,.T.) ;
#17727 = EDGE_CURVE('',#14121,#14122,#7386,.T.) ;
#17728 = EDGE_CURVE('',#14122,#14123,#11529,.T.) ;
#17729 = EDGE_CURVE('',#14120,#14123,#7387,.T.) ;
#17730 = EDGE_CURVE('',#14124,#14125,#11530,.T.) ;
#17731 = EDGE_CURVE('',#14125,#14123,#11531,.T.) ;
#17732 = EDGE_CURVE('',#14122,#14124,#11532,.T.) ;
#17733 = EDGE_CURVE('',#14126,#14127,#11533,.T.) ;
#17734 = EDGE_CURVE('',#14125,#14127,#7388,.T.) ;
#17735 = EDGE_CURVE('',#14124,#14126,#7389,.T.) ;
#17736 = EDGE_CURVE('',#14128,#14129,#11534,.T.) ;
#17737 = EDGE_CURVE('',#14129,#14127,#11535,.T.) ;
#17738 = EDGE_CURVE('',#14128,#14126,#11536,.T.) ;
#17739 = EDGE_CURVE('',#14130,#14131,#11537,.T.) ;
#17740 = EDGE_CURVE('',#14129,#14131,#7390,.T.) ;
#17741 = EDGE_CURVE('',#14128,#14130,#7391,.T.) ;
#17742 = EDGE_CURVE('',#14132,#14133,#11538,.T.) ;
#17743 = EDGE_CURVE('',#14133,#14131,#11539,.T.) ;
#17744 = EDGE_CURVE('',#14130,#14132,#11540,.T.) ;
#17745 = EDGE_CURVE('',#14134,#14135,#11541,.T.) ;
#17746 = EDGE_CURVE('',#14133,#14135,#7392,.T.) ;
#17747 = EDGE_CURVE('',#14132,#14134,#7393,.T.) ;
#17748 = EDGE_CURVE('',#14120,#14135,#11542,.T.) ;
#17749 = EDGE_CURVE('',#14121,#14134,#11543,.T.) ;
#17750 = EDGE_CURVE('',#14136,#14126,#7394,.T.) ;
#17751 = EDGE_CURVE('',#14137,#14136,#11544,.F.) ;
#17752 = EDGE_CURVE('',#14128,#14137,#7395,.T.) ;
#17753 = EDGE_CURVE('',#14124,#14138,#7396,.T.) ;
#17754 = EDGE_CURVE('',#14138,#14136,#7397,.T.) ;
#17755 = EDGE_CURVE('',#14139,#14122,#7398,.T.) ;
#17756 = EDGE_CURVE('',#14138,#14139,#11545,.F.) ;
#17757 = EDGE_CURVE('',#14121,#14140,#7399,.T.) ;
#17758 = EDGE_CURVE('',#14140,#14139,#7400,.T.) ;
#17759 = EDGE_CURVE('',#14141,#14142,#11546,.T.) ;
#17760 = EDGE_CURVE('',#14142,#14143,#7401,.T.) ;
#17761 = EDGE_CURVE('',#14143,#14144,#11547,.T.) ;
#17762 = EDGE_CURVE('',#14141,#14144,#7402,.T.) ;
#17763 = EDGE_CURVE('',#14145,#14146,#11548,.T.) ;
#17764 = EDGE_CURVE('',#14146,#14144,#11549,.T.) ;
#17765 = EDGE_CURVE('',#14143,#14145,#11550,.T.) ;
#17766 = EDGE_CURVE('',#14147,#14148,#11551,.T.) ;
#17767 = EDGE_CURVE('',#14146,#14148,#7403,.T.) ;
#17768 = EDGE_CURVE('',#14145,#14147,#7404,.T.) ;
#17769 = EDGE_CURVE('',#14149,#14150,#11552,.T.) ;
#17770 = EDGE_CURVE('',#14150,#14148,#11553,.T.) ;
#17771 = EDGE_CURVE('',#14149,#14147,#11554,.T.) ;
#17772 = EDGE_CURVE('',#14151,#14152,#11555,.T.) ;
#17773 = EDGE_CURVE('',#14150,#14152,#7405,.T.) ;
#17774 = EDGE_CURVE('',#14149,#14151,#7406,.T.) ;
#17775 = EDGE_CURVE('',#14153,#14154,#11556,.T.) ;
#17776 = EDGE_CURVE('',#14154,#14152,#11557,.T.) ;
#17777 = EDGE_CURVE('',#14151,#14153,#11558,.T.) ;
#17778 = EDGE_CURVE('',#14155,#14156,#11559,.T.) ;
#17779 = EDGE_CURVE('',#14154,#14156,#7407,.T.) ;
#17780 = EDGE_CURVE('',#14153,#14155,#7408,.T.) ;
#17781 = EDGE_CURVE('',#14141,#14156,#11560,.T.) ;
#17782 = EDGE_CURVE('',#14142,#14155,#11561,.T.) ;
#17783 = EDGE_CURVE('',#14157,#14147,#7409,.T.) ;
#17784 = EDGE_CURVE('',#14158,#14157,#11562,.F.) ;
#17785 = EDGE_CURVE('',#14149,#14158,#7410,.T.) ;
#17786 = EDGE_CURVE('',#14145,#14159,#7411,.T.) ;
#17787 = EDGE_CURVE('',#14159,#14157,#7412,.T.) ;
#17788 = EDGE_CURVE('',#14160,#14143,#7413,.T.) ;
#17789 = EDGE_CURVE('',#14159,#14160,#11563,.F.) ;
#17790 = EDGE_CURVE('',#14142,#14161,#7414,.T.) ;
#17791 = EDGE_CURVE('',#14161,#14160,#7415,.T.) ;
#17792 = EDGE_CURVE('',#14162,#14163,#11564,.T.) ;
#17793 = EDGE_CURVE('',#14163,#14164,#7416,.T.) ;
#17794 = EDGE_CURVE('',#14164,#14165,#11565,.T.) ;
#17795 = EDGE_CURVE('',#14162,#14165,#7417,.T.) ;
#17796 = EDGE_CURVE('',#14166,#14167,#11566,.T.) ;
#17797 = EDGE_CURVE('',#14167,#14165,#11567,.T.) ;
#17798 = EDGE_CURVE('',#14164,#14166,#11568,.T.) ;
#17799 = EDGE_CURVE('',#14168,#14169,#11569,.T.) ;
#17800 = EDGE_CURVE('',#14167,#14169,#7418,.T.) ;
#17801 = EDGE_CURVE('',#14166,#14168,#7419,.T.) ;
#17802 = EDGE_CURVE('',#14170,#14171,#11570,.T.) ;
#17803 = EDGE_CURVE('',#14171,#14169,#11571,.T.) ;
#17804 = EDGE_CURVE('',#14170,#14168,#11572,.T.) ;
#17805 = EDGE_CURVE('',#14172,#14173,#11573,.T.) ;
#17806 = EDGE_CURVE('',#14171,#14173,#7420,.T.) ;
#17807 = EDGE_CURVE('',#14170,#14172,#7421,.T.) ;
#17808 = EDGE_CURVE('',#14174,#14175,#11574,.T.) ;
#17809 = EDGE_CURVE('',#14175,#14173,#11575,.T.) ;
#17810 = EDGE_CURVE('',#14172,#14174,#11576,.T.) ;
#17811 = EDGE_CURVE('',#14176,#14177,#11577,.T.) ;
#17812 = EDGE_CURVE('',#14175,#14177,#7422,.T.) ;
#17813 = EDGE_CURVE('',#14174,#14176,#7423,.T.) ;
#17814 = EDGE_CURVE('',#14162,#14177,#11578,.T.) ;
#17815 = EDGE_CURVE('',#14163,#14176,#11579,.T.) ;
#17816 = EDGE_CURVE('',#14178,#14168,#7424,.T.) ;
#17817 = EDGE_CURVE('',#14179,#14178,#11580,.F.) ;
#17818 = EDGE_CURVE('',#14170,#14179,#7425,.T.) ;
#17819 = EDGE_CURVE('',#14166,#14180,#7426,.T.) ;
#17820 = EDGE_CURVE('',#14180,#14178,#7427,.T.) ;
#17821 = EDGE_CURVE('',#14181,#14164,#7428,.T.) ;
#17822 = EDGE_CURVE('',#14180,#14181,#11581,.F.) ;
#17823 = EDGE_CURVE('',#14163,#14182,#7429,.T.) ;
#17824 = EDGE_CURVE('',#14182,#14181,#7430,.T.) ;
#17825 = EDGE_CURVE('',#14183,#14184,#11582,.T.) ;
#17826 = EDGE_CURVE('',#14184,#14185,#7431,.T.) ;
#17827 = EDGE_CURVE('',#14185,#14186,#11583,.T.) ;
#17828 = EDGE_CURVE('',#14183,#14186,#7432,.T.) ;
#17829 = EDGE_CURVE('',#14187,#14188,#11584,.T.) ;
#17830 = EDGE_CURVE('',#14188,#14186,#11585,.T.) ;
#17831 = EDGE_CURVE('',#14185,#14187,#11586,.T.) ;
#17832 = EDGE_CURVE('',#14189,#14190,#11587,.T.) ;
#17833 = EDGE_CURVE('',#14188,#14190,#7433,.T.) ;
#17834 = EDGE_CURVE('',#14187,#14189,#7434,.T.) ;
#17835 = EDGE_CURVE('',#14191,#14192,#11588,.T.) ;
#17836 = EDGE_CURVE('',#14192,#14190,#11589,.T.) ;
#17837 = EDGE_CURVE('',#14191,#14189,#11590,.T.) ;
#17838 = EDGE_CURVE('',#14193,#14194,#11591,.T.) ;
#17839 = EDGE_CURVE('',#14192,#14194,#7435,.T.) ;
#17840 = EDGE_CURVE('',#14191,#14193,#7436,.T.) ;
#17841 = EDGE_CURVE('',#14195,#14196,#11592,.T.) ;
#17842 = EDGE_CURVE('',#14196,#14194,#11593,.T.) ;
#17843 = EDGE_CURVE('',#14193,#14195,#11594,.T.) ;
#17844 = EDGE_CURVE('',#14197,#14198,#11595,.T.) ;
#17845 = EDGE_CURVE('',#14196,#14198,#7437,.T.) ;
#17846 = EDGE_CURVE('',#14195,#14197,#7438,.T.) ;
#17847 = EDGE_CURVE('',#14183,#14198,#11596,.T.) ;
#17848 = EDGE_CURVE('',#14184,#14197,#11597,.T.) ;
#17849 = EDGE_CURVE('',#14199,#14189,#7439,.T.) ;
#17850 = EDGE_CURVE('',#14200,#14199,#11598,.F.) ;
#17851 = EDGE_CURVE('',#14191,#14200,#7440,.T.) ;
#17852 = EDGE_CURVE('',#14187,#14201,#7441,.T.) ;
#17853 = EDGE_CURVE('',#14201,#14199,#7442,.T.) ;
#17854 = EDGE_CURVE('',#14202,#14185,#7443,.T.) ;
#17855 = EDGE_CURVE('',#14201,#14202,#11599,.F.) ;
#17856 = EDGE_CURVE('',#14184,#14203,#7444,.T.) ;
#17857 = EDGE_CURVE('',#14203,#14202,#7445,.T.) ;
#17858 = EDGE_CURVE('',#14204,#14205,#11600,.T.) ;
#17859 = EDGE_CURVE('',#14205,#14206,#7446,.T.) ;
#17860 = EDGE_CURVE('',#14206,#14207,#11601,.T.) ;
#17861 = EDGE_CURVE('',#14204,#14207,#7447,.T.) ;
#17862 = EDGE_CURVE('',#14208,#14209,#11602,.T.) ;
#17863 = EDGE_CURVE('',#14209,#14207,#11603,.T.) ;
#17864 = EDGE_CURVE('',#14206,#14208,#11604,.T.) ;
#17865 = EDGE_CURVE('',#14210,#14211,#11605,.T.) ;
#17866 = EDGE_CURVE('',#14209,#14211,#7448,.T.) ;
#17867 = EDGE_CURVE('',#14208,#14210,#7449,.T.) ;
#17868 = EDGE_CURVE('',#14212,#14213,#11606,.T.) ;
#17869 = EDGE_CURVE('',#14213,#14211,#11607,.T.) ;
#17870 = EDGE_CURVE('',#14212,#14210,#11608,.T.) ;
#17871 = EDGE_CURVE('',#14214,#14215,#11609,.T.) ;
#17872 = EDGE_CURVE('',#14213,#14215,#7450,.T.) ;
#17873 = EDGE_CURVE('',#14212,#14214,#7451,.T.) ;
#17874 = EDGE_CURVE('',#14216,#14217,#11610,.T.) ;
#17875 = EDGE_CURVE('',#14217,#14215,#11611,.T.) ;
#17876 = EDGE_CURVE('',#14214,#14216,#11612,.T.) ;
#17877 = EDGE_CURVE('',#14218,#14219,#11613,.T.) ;
#17878 = EDGE_CURVE('',#14217,#14219,#7452,.T.) ;
#17879 = EDGE_CURVE('',#14216,#14218,#7453,.T.) ;
#17880 = EDGE_CURVE('',#14204,#14219,#11614,.T.) ;
#17881 = EDGE_CURVE('',#14205,#14218,#11615,.T.) ;
#17882 = EDGE_CURVE('',#14220,#14210,#7454,.T.) ;
#17883 = EDGE_CURVE('',#14221,#14220,#11616,.F.) ;
#17884 = EDGE_CURVE('',#14212,#14221,#7455,.T.) ;
#17885 = EDGE_CURVE('',#14208,#14222,#7456,.T.) ;
#17886 = EDGE_CURVE('',#14222,#14220,#7457,.T.) ;
#17887 = EDGE_CURVE('',#14223,#14206,#7458,.T.) ;
#17888 = EDGE_CURVE('',#14222,#14223,#11617,.F.) ;
#17889 = EDGE_CURVE('',#14205,#14224,#7459,.T.) ;
#17890 = EDGE_CURVE('',#14224,#14223,#7460,.T.) ;
#17891 = EDGE_CURVE('',#14225,#14226,#11618,.T.) ;
#17892 = EDGE_CURVE('',#14226,#14227,#7461,.T.) ;
#17893 = EDGE_CURVE('',#14227,#14228,#11619,.T.) ;
#17894 = EDGE_CURVE('',#14225,#14228,#7462,.T.) ;
#17895 = EDGE_CURVE('',#14229,#14230,#11620,.T.) ;
#17896 = EDGE_CURVE('',#14230,#14228,#11621,.T.) ;
#17897 = EDGE_CURVE('',#14227,#14229,#11622,.T.) ;
#17898 = EDGE_CURVE('',#14231,#14232,#11623,.T.) ;
#17899 = EDGE_CURVE('',#14230,#14232,#7463,.T.) ;
#17900 = EDGE_CURVE('',#14229,#14231,#7464,.T.) ;
#17901 = EDGE_CURVE('',#14233,#14234,#11624,.T.) ;
#17902 = EDGE_CURVE('',#14234,#14232,#11625,.T.) ;
#17903 = EDGE_CURVE('',#14233,#14231,#11626,.T.) ;
#17904 = EDGE_CURVE('',#14235,#14236,#11627,.T.) ;
#17905 = EDGE_CURVE('',#14234,#14236,#7465,.T.) ;
#17906 = EDGE_CURVE('',#14233,#14235,#7466,.T.) ;
#17907 = EDGE_CURVE('',#14237,#14238,#11628,.T.) ;
#17908 = EDGE_CURVE('',#14238,#14236,#11629,.T.) ;
#17909 = EDGE_CURVE('',#14235,#14237,#11630,.T.) ;
#17910 = EDGE_CURVE('',#14239,#14240,#11631,.T.) ;
#17911 = EDGE_CURVE('',#14238,#14240,#7467,.T.) ;
#17912 = EDGE_CURVE('',#14237,#14239,#7468,.T.) ;
#17913 = EDGE_CURVE('',#14225,#14240,#11632,.T.) ;
#17914 = EDGE_CURVE('',#14226,#14239,#11633,.T.) ;
#17915 = EDGE_CURVE('',#14241,#14231,#7469,.T.) ;
#17916 = EDGE_CURVE('',#14242,#14241,#11634,.F.) ;
#17917 = EDGE_CURVE('',#14233,#14242,#7470,.T.) ;
#17918 = EDGE_CURVE('',#14229,#14243,#7471,.T.) ;
#17919 = EDGE_CURVE('',#14243,#14241,#7472,.T.) ;
#17920 = EDGE_CURVE('',#14244,#14227,#7473,.T.) ;
#17921 = EDGE_CURVE('',#14243,#14244,#11635,.F.) ;
#17922 = EDGE_CURVE('',#14226,#14245,#7474,.T.) ;
#17923 = EDGE_CURVE('',#14245,#14244,#7475,.T.) ;
#17924 = EDGE_CURVE('',#14246,#14247,#11636,.T.) ;
#17925 = EDGE_CURVE('',#14247,#14248,#7476,.T.) ;
#17926 = EDGE_CURVE('',#14248,#14249,#11637,.T.) ;
#17927 = EDGE_CURVE('',#14246,#14249,#7477,.T.) ;
#17928 = EDGE_CURVE('',#14250,#14251,#11638,.T.) ;
#17929 = EDGE_CURVE('',#14251,#14249,#11639,.T.) ;
#17930 = EDGE_CURVE('',#14248,#14250,#11640,.T.) ;
#17931 = EDGE_CURVE('',#14252,#14253,#11641,.T.) ;
#17932 = EDGE_CURVE('',#14251,#14253,#7478,.T.) ;
#17933 = EDGE_CURVE('',#14250,#14252,#7479,.T.) ;
#17934 = EDGE_CURVE('',#14254,#14255,#11642,.T.) ;
#17935 = EDGE_CURVE('',#14255,#14253,#11643,.T.) ;
#17936 = EDGE_CURVE('',#14254,#14252,#11644,.T.) ;
#17937 = EDGE_CURVE('',#14256,#14257,#11645,.T.) ;
#17938 = EDGE_CURVE('',#14255,#14257,#7480,.T.) ;
#17939 = EDGE_CURVE('',#14254,#14256,#7481,.T.) ;
#17940 = EDGE_CURVE('',#14258,#14259,#11646,.T.) ;
#17941 = EDGE_CURVE('',#14259,#14257,#11647,.T.) ;
#17942 = EDGE_CURVE('',#14256,#14258,#11648,.T.) ;
#17943 = EDGE_CURVE('',#14260,#14261,#11649,.T.) ;
#17944 = EDGE_CURVE('',#14259,#14261,#7482,.T.) ;
#17945 = EDGE_CURVE('',#14258,#14260,#7483,.T.) ;
#17946 = EDGE_CURVE('',#14246,#14261,#11650,.T.) ;
#17947 = EDGE_CURVE('',#14247,#14260,#11651,.T.) ;
#17948 = EDGE_CURVE('',#14262,#14252,#7484,.T.) ;
#17949 = EDGE_CURVE('',#14263,#14262,#11652,.F.) ;
#17950 = EDGE_CURVE('',#14254,#14263,#7485,.T.) ;
#17951 = EDGE_CURVE('',#14250,#14264,#7486,.T.) ;
#17952 = EDGE_CURVE('',#14264,#14262,#7487,.T.) ;
#17953 = EDGE_CURVE('',#14265,#14248,#7488,.T.) ;
#17954 = EDGE_CURVE('',#14264,#14265,#11653,.F.) ;
#17955 = EDGE_CURVE('',#14247,#14266,#7489,.T.) ;
#17956 = EDGE_CURVE('',#14266,#14265,#7490,.T.) ;
#17957 = EDGE_CURVE('',#14267,#14268,#11654,.T.) ;
#17958 = EDGE_CURVE('',#14268,#14269,#7491,.T.) ;
#17959 = EDGE_CURVE('',#14269,#14270,#11655,.T.) ;
#17960 = EDGE_CURVE('',#14267,#14270,#7492,.T.) ;
#17961 = EDGE_CURVE('',#14271,#14272,#11656,.T.) ;
#17962 = EDGE_CURVE('',#14272,#14270,#11657,.T.) ;
#17963 = EDGE_CURVE('',#14269,#14271,#11658,.T.) ;
#17964 = EDGE_CURVE('',#14273,#14274,#11659,.T.) ;
#17965 = EDGE_CURVE('',#14272,#14274,#7493,.T.) ;
#17966 = EDGE_CURVE('',#14271,#14273,#7494,.T.) ;
#17967 = EDGE_CURVE('',#14275,#14276,#11660,.T.) ;
#17968 = EDGE_CURVE('',#14276,#14274,#11661,.T.) ;
#17969 = EDGE_CURVE('',#14275,#14273,#11662,.T.) ;
#17970 = EDGE_CURVE('',#14277,#14278,#11663,.T.) ;
#17971 = EDGE_CURVE('',#14276,#14278,#7495,.T.) ;
#17972 = EDGE_CURVE('',#14275,#14277,#7496,.T.) ;
#17973 = EDGE_CURVE('',#14279,#14280,#11664,.T.) ;
#17974 = EDGE_CURVE('',#14280,#14278,#11665,.T.) ;
#17975 = EDGE_CURVE('',#14277,#14279,#11666,.T.) ;
#17976 = EDGE_CURVE('',#14281,#14282,#11667,.T.) ;
#17977 = EDGE_CURVE('',#14280,#14282,#7497,.T.) ;
#17978 = EDGE_CURVE('',#14279,#14281,#7498,.T.) ;
#17979 = EDGE_CURVE('',#14267,#14282,#11668,.T.) ;
#17980 = EDGE_CURVE('',#14268,#14281,#11669,.T.) ;
#17981 = EDGE_CURVE('',#14283,#14273,#7499,.T.) ;
#17982 = EDGE_CURVE('',#14284,#14283,#11670,.F.) ;
#17983 = EDGE_CURVE('',#14275,#14284,#7500,.T.) ;
#17984 = EDGE_CURVE('',#14271,#14285,#7501,.T.) ;
#17985 = EDGE_CURVE('',#14285,#14283,#7502,.T.) ;
#17986 = EDGE_CURVE('',#14286,#14269,#7503,.T.) ;
#17987 = EDGE_CURVE('',#14285,#14286,#11671,.F.) ;
#17988 = EDGE_CURVE('',#14268,#14287,#7504,.T.) ;
#17989 = EDGE_CURVE('',#14287,#14286,#7505,.T.) ;
#17990 = EDGE_CURVE('',#14288,#14289,#11672,.T.) ;
#17991 = EDGE_CURVE('',#14289,#14290,#7506,.T.) ;
#17992 = EDGE_CURVE('',#14290,#14291,#11673,.T.) ;
#17993 = EDGE_CURVE('',#14288,#14291,#7507,.T.) ;
#17994 = EDGE_CURVE('',#14292,#14293,#11674,.T.) ;
#17995 = EDGE_CURVE('',#14293,#14291,#11675,.T.) ;
#17996 = EDGE_CURVE('',#14290,#14292,#11676,.T.) ;
#17997 = EDGE_CURVE('',#14294,#14295,#11677,.T.) ;
#17998 = EDGE_CURVE('',#14293,#14295,#7508,.T.) ;
#17999 = EDGE_CURVE('',#14292,#14294,#7509,.T.) ;
#18000 = EDGE_CURVE('',#14296,#14297,#11678,.T.) ;
#18001 = EDGE_CURVE('',#14297,#14295,#11679,.T.) ;
#18002 = EDGE_CURVE('',#14296,#14294,#11680,.T.) ;
#18003 = EDGE_CURVE('',#14298,#14299,#11681,.T.) ;
#18004 = EDGE_CURVE('',#14297,#14299,#7510,.T.) ;
#18005 = EDGE_CURVE('',#14296,#14298,#7511,.T.) ;
#18006 = EDGE_CURVE('',#13963,#14300,#11682,.T.) ;
#18007 = EDGE_CURVE('',#14300,#14299,#11683,.T.) ;
#18008 = EDGE_CURVE('',#14298,#13963,#11684,.T.) ;
#18009 = EDGE_CURVE('',#13962,#14301,#11685,.T.) ;
#18010 = EDGE_CURVE('',#14300,#14301,#7512,.T.) ;
#18011 = EDGE_CURVE('',#14288,#14301,#11686,.T.) ;
#18012 = EDGE_CURVE('',#14289,#13962,#11687,.T.) ;
#18013 = EDGE_CURVE('',#14302,#14294,#7513,.T.) ;
#18014 = EDGE_CURVE('',#14302,#14303,#11688,.T.) ;
#18015 = EDGE_CURVE('',#14303,#14296,#7514,.T.) ;
#18016 = EDGE_CURVE('',#13955,#14304,#7515,.T.) ;
#18017 = EDGE_CURVE('',#14304,#14305,#11689,.T.) ;
#18018 = EDGE_CURVE('',#14305,#14302,#7516,.T.) ;
#18019 = EDGE_CURVE('',#14292,#14306,#7517,.T.) ;
#18020 = EDGE_CURVE('',#14306,#14307,#7518,.T.) ;
#18021 = EDGE_CURVE('',#14307,#14308,#11690,.T.) ;
#18022 = EDGE_CURVE('',#14308,#13956,#7519,.T.) ;
#18023 = EDGE_CURVE('',#14309,#14290,#7520,.T.) ;
#18024 = EDGE_CURVE('',#14309,#14306,#11691,.T.) ;
#18025 = EDGE_CURVE('',#14289,#14310,#7521,.T.) ;
#18026 = EDGE_CURVE('',#14310,#14309,#7522,.T.) ;
#18027 = EDGE_CURVE('',#14311,#14312,#11692,.T.) ;
#18028 = EDGE_CURVE('',#14312,#14313,#7523,.T.) ;
#18029 = EDGE_CURVE('',#14313,#14314,#11693,.T.) ;
#18030 = EDGE_CURVE('',#14311,#14314,#7524,.T.) ;
#18031 = EDGE_CURVE('',#14315,#14316,#11694,.T.) ;
#18032 = EDGE_CURVE('',#14316,#14314,#11695,.T.) ;
#18033 = EDGE_CURVE('',#14313,#14315,#11696,.T.) ;
#18034 = EDGE_CURVE('',#14317,#14318,#11697,.T.) ;
#18035 = EDGE_CURVE('',#14316,#14318,#7525,.T.) ;
#18036 = EDGE_CURVE('',#14315,#14317,#7526,.T.) ;
#18037 = EDGE_CURVE('',#14319,#14320,#11698,.T.) ;
#18038 = EDGE_CURVE('',#14320,#14318,#11699,.T.) ;
#18039 = EDGE_CURVE('',#14319,#14317,#11700,.T.) ;
#18040 = EDGE_CURVE('',#14321,#14322,#11701,.T.) ;
#18041 = EDGE_CURVE('',#14320,#14322,#7527,.T.) ;
#18042 = EDGE_CURVE('',#14319,#14321,#7528,.T.) ;
#18043 = EDGE_CURVE('',#13982,#14323,#11702,.T.) ;
#18044 = EDGE_CURVE('',#14323,#14322,#11703,.T.) ;
#18045 = EDGE_CURVE('',#14321,#13982,#11704,.T.) ;
#18046 = EDGE_CURVE('',#13981,#14324,#11705,.T.) ;
#18047 = EDGE_CURVE('',#14323,#14324,#7529,.T.) ;
#18048 = EDGE_CURVE('',#14311,#14324,#11706,.T.) ;
#18049 = EDGE_CURVE('',#14312,#13981,#11707,.T.) ;
#18050 = EDGE_CURVE('',#14325,#14317,#7530,.T.) ;
#18051 = EDGE_CURVE('',#14325,#14326,#11708,.T.) ;
#18052 = EDGE_CURVE('',#14326,#14319,#7531,.T.) ;
#18053 = EDGE_CURVE('',#13974,#14327,#7532,.T.) ;
#18054 = EDGE_CURVE('',#14327,#14328,#11709,.T.) ;
#18055 = EDGE_CURVE('',#14328,#14325,#7533,.T.) ;
#18056 = EDGE_CURVE('',#14315,#14329,#7534,.T.) ;
#18057 = EDGE_CURVE('',#14329,#14330,#7535,.T.) ;
#18058 = EDGE_CURVE('',#14330,#14331,#11710,.T.) ;
#18059 = EDGE_CURVE('',#14331,#13975,#7536,.T.) ;
#18060 = EDGE_CURVE('',#14332,#14313,#7537,.T.) ;
#18061 = EDGE_CURVE('',#14332,#14329,#11711,.T.) ;
#18062 = EDGE_CURVE('',#14312,#14333,#7538,.T.) ;
#18063 = EDGE_CURVE('',#14333,#14332,#7539,.T.) ;
#18064 = EDGE_CURVE('',#14334,#14335,#11712,.T.) ;
#18065 = EDGE_CURVE('',#14335,#14336,#7540,.T.) ;
#18066 = EDGE_CURVE('',#14336,#14337,#11713,.T.) ;
#18067 = EDGE_CURVE('',#14334,#14337,#7541,.T.) ;
#18068 = EDGE_CURVE('',#14338,#14339,#11714,.T.) ;
#18069 = EDGE_CURVE('',#14339,#14337,#11715,.T.) ;
#18070 = EDGE_CURVE('',#14336,#14338,#11716,.T.) ;
#18071 = EDGE_CURVE('',#14340,#14341,#11717,.T.) ;
#18072 = EDGE_CURVE('',#14339,#14341,#7542,.T.) ;
#18073 = EDGE_CURVE('',#14338,#14340,#7543,.T.) ;
#18074 = EDGE_CURVE('',#14342,#14343,#11718,.T.) ;
#18075 = EDGE_CURVE('',#14343,#14341,#11719,.T.) ;
#18076 = EDGE_CURVE('',#14342,#14340,#11720,.T.) ;
#18077 = EDGE_CURVE('',#14344,#14345,#11721,.T.) ;
#18078 = EDGE_CURVE('',#14343,#14345,#7544,.T.) ;
#18079 = EDGE_CURVE('',#14342,#14344,#7545,.T.) ;
#18080 = EDGE_CURVE('',#14001,#14346,#11722,.T.) ;
#18081 = EDGE_CURVE('',#14346,#14345,#11723,.T.) ;
#18082 = EDGE_CURVE('',#14344,#14001,#11724,.T.) ;
#18083 = EDGE_CURVE('',#14000,#14347,#11725,.T.) ;
#18084 = EDGE_CURVE('',#14346,#14347,#7546,.T.) ;
#18085 = EDGE_CURVE('',#14334,#14347,#11726,.T.) ;
#18086 = EDGE_CURVE('',#14335,#14000,#11727,.T.) ;
#18087 = EDGE_CURVE('',#14348,#14340,#7547,.T.) ;
#18088 = EDGE_CURVE('',#14348,#14349,#11728,.T.) ;
#18089 = EDGE_CURVE('',#14349,#14342,#7548,.T.) ;
#18090 = EDGE_CURVE('',#13993,#14350,#7549,.T.) ;
#18091 = EDGE_CURVE('',#14350,#14351,#11729,.T.) ;
#18092 = EDGE_CURVE('',#14351,#14348,#7550,.T.) ;
#18093 = EDGE_CURVE('',#14338,#14352,#7551,.T.) ;
#18094 = EDGE_CURVE('',#14352,#14353,#7552,.T.) ;
#18095 = EDGE_CURVE('',#14353,#14354,#11730,.T.) ;
#18096 = EDGE_CURVE('',#14354,#13994,#7553,.T.) ;
#18097 = EDGE_CURVE('',#14355,#14336,#7554,.T.) ;
#18098 = EDGE_CURVE('',#14355,#14352,#11731,.T.) ;
#18099 = EDGE_CURVE('',#14335,#14356,#7555,.T.) ;
#18100 = EDGE_CURVE('',#14356,#14355,#7556,.T.) ;
#18101 = EDGE_CURVE('',#14357,#14358,#11732,.T.) ;
#18102 = EDGE_CURVE('',#14358,#14359,#7557,.T.) ;
#18103 = EDGE_CURVE('',#14359,#14360,#11733,.T.) ;
#18104 = EDGE_CURVE('',#14357,#14360,#7558,.T.) ;
#18105 = EDGE_CURVE('',#14361,#14362,#11734,.T.) ;
#18106 = EDGE_CURVE('',#14362,#14360,#11735,.T.) ;
#18107 = EDGE_CURVE('',#14359,#14361,#11736,.T.) ;
#18108 = EDGE_CURVE('',#14363,#14364,#11737,.T.) ;
#18109 = EDGE_CURVE('',#14362,#14364,#7559,.T.) ;
#18110 = EDGE_CURVE('',#14361,#14363,#7560,.T.) ;
#18111 = EDGE_CURVE('',#14365,#14366,#11738,.T.) ;
#18112 = EDGE_CURVE('',#14366,#14364,#11739,.T.) ;
#18113 = EDGE_CURVE('',#14365,#14363,#11740,.T.) ;
#18114 = EDGE_CURVE('',#14367,#14368,#11741,.T.) ;
#18115 = EDGE_CURVE('',#14366,#14368,#7561,.T.) ;
#18116 = EDGE_CURVE('',#14365,#14367,#7562,.T.) ;
#18117 = EDGE_CURVE('',#14020,#14369,#11742,.T.) ;
#18118 = EDGE_CURVE('',#14369,#14368,#11743,.T.) ;
#18119 = EDGE_CURVE('',#14367,#14020,#11744,.T.) ;
#18120 = EDGE_CURVE('',#14019,#14370,#11745,.T.) ;
#18121 = EDGE_CURVE('',#14369,#14370,#7563,.T.) ;
#18122 = EDGE_CURVE('',#14357,#14370,#11746,.T.) ;
#18123 = EDGE_CURVE('',#14358,#14019,#11747,.T.) ;
#18124 = EDGE_CURVE('',#14371,#14363,#7564,.T.) ;
#18125 = EDGE_CURVE('',#14371,#14372,#11748,.T.) ;
#18126 = EDGE_CURVE('',#14372,#14365,#7565,.T.) ;
#18127 = EDGE_CURVE('',#14012,#14373,#7566,.T.) ;
#18128 = EDGE_CURVE('',#14373,#14374,#11749,.T.) ;
#18129 = EDGE_CURVE('',#14374,#14371,#7567,.T.) ;
#18130 = EDGE_CURVE('',#14361,#14375,#7568,.T.) ;
#18131 = EDGE_CURVE('',#14375,#14376,#7569,.T.) ;
#18132 = EDGE_CURVE('',#14376,#14377,#11750,.T.) ;
#18133 = EDGE_CURVE('',#14377,#14013,#7570,.T.) ;
#18134 = EDGE_CURVE('',#14378,#14359,#7571,.T.) ;
#18135 = EDGE_CURVE('',#14378,#14375,#11751,.T.) ;
#18136 = EDGE_CURVE('',#14358,#14379,#7572,.T.) ;
#18137 = EDGE_CURVE('',#14379,#14378,#7573,.T.) ;
#18138 = EDGE_CURVE('',#14380,#14381,#11752,.T.) ;
#18139 = EDGE_CURVE('',#14381,#14382,#7574,.T.) ;
#18140 = EDGE_CURVE('',#14382,#14383,#11753,.T.) ;
#18141 = EDGE_CURVE('',#14380,#14383,#7575,.T.) ;
#18142 = EDGE_CURVE('',#14384,#14385,#11754,.T.) ;
#18143 = EDGE_CURVE('',#14385,#14383,#11755,.T.) ;
#18144 = EDGE_CURVE('',#14382,#14384,#11756,.T.) ;
#18145 = EDGE_CURVE('',#14386,#14387,#11757,.T.) ;
#18146 = EDGE_CURVE('',#14385,#14387,#7576,.T.) ;
#18147 = EDGE_CURVE('',#14384,#14386,#7577,.T.) ;
#18148 = EDGE_CURVE('',#14388,#14389,#11758,.T.) ;
#18149 = EDGE_CURVE('',#14389,#14387,#11759,.T.) ;
#18150 = EDGE_CURVE('',#14388,#14386,#11760,.T.) ;
#18151 = EDGE_CURVE('',#14390,#14391,#11761,.T.) ;
#18152 = EDGE_CURVE('',#14389,#14391,#7578,.T.) ;
#18153 = EDGE_CURVE('',#14388,#14390,#7579,.T.) ;
#18154 = EDGE_CURVE('',#14039,#14392,#11762,.T.) ;
#18155 = EDGE_CURVE('',#14392,#14391,#11763,.T.) ;
#18156 = EDGE_CURVE('',#14390,#14039,#11764,.T.) ;
#18157 = EDGE_CURVE('',#14038,#14393,#11765,.T.) ;
#18158 = EDGE_CURVE('',#14392,#14393,#7580,.T.) ;
#18159 = EDGE_CURVE('',#14380,#14393,#11766,.T.) ;
#18160 = EDGE_CURVE('',#14381,#14038,#11767,.T.) ;
#18161 = EDGE_CURVE('',#14394,#14386,#7581,.T.) ;
#18162 = EDGE_CURVE('',#14394,#14395,#11768,.T.) ;
#18163 = EDGE_CURVE('',#14395,#14388,#7582,.T.) ;
#18164 = EDGE_CURVE('',#14031,#14396,#7583,.T.) ;
#18165 = EDGE_CURVE('',#14396,#14397,#11769,.T.) ;
#18166 = EDGE_CURVE('',#14397,#14394,#7584,.T.) ;
#18167 = EDGE_CURVE('',#14384,#14398,#7585,.T.) ;
#18168 = EDGE_CURVE('',#14398,#14399,#7586,.T.) ;
#18169 = EDGE_CURVE('',#14399,#14400,#11770,.T.) ;
#18170 = EDGE_CURVE('',#14400,#14032,#7587,.T.) ;
#18171 = EDGE_CURVE('',#14401,#14382,#7588,.T.) ;
#18172 = EDGE_CURVE('',#14401,#14398,#11771,.T.) ;
#18173 = EDGE_CURVE('',#14381,#14402,#7589,.T.) ;
#18174 = EDGE_CURVE('',#14402,#14401,#7590,.T.) ;
#18175 = EDGE_CURVE('',#14403,#14404,#11772,.T.) ;
#18176 = EDGE_CURVE('',#14404,#14405,#7591,.T.) ;
#18177 = EDGE_CURVE('',#14405,#14406,#11773,.T.) ;
#18178 = EDGE_CURVE('',#14403,#14406,#7592,.T.) ;
#18179 = EDGE_CURVE('',#14407,#14408,#11774,.T.) ;
#18180 = EDGE_CURVE('',#14408,#14406,#11775,.T.) ;
#18181 = EDGE_CURVE('',#14405,#14407,#11776,.T.) ;
#18182 = EDGE_CURVE('',#14409,#14410,#11777,.T.) ;
#18183 = EDGE_CURVE('',#14408,#14410,#7593,.T.) ;
#18184 = EDGE_CURVE('',#14407,#14409,#7594,.T.) ;
#18185 = EDGE_CURVE('',#14411,#14412,#11778,.T.) ;
#18186 = EDGE_CURVE('',#14412,#14410,#11779,.T.) ;
#18187 = EDGE_CURVE('',#14411,#14409,#11780,.T.) ;
#18188 = EDGE_CURVE('',#14413,#14414,#11781,.T.) ;
#18189 = EDGE_CURVE('',#14412,#14414,#7595,.T.) ;
#18190 = EDGE_CURVE('',#14411,#14413,#7596,.T.) ;
#18191 = EDGE_CURVE('',#14058,#14415,#11782,.T.) ;
#18192 = EDGE_CURVE('',#14415,#14414,#11783,.T.) ;
#18193 = EDGE_CURVE('',#14413,#14058,#11784,.T.) ;
#18194 = EDGE_CURVE('',#14057,#14416,#11785,.T.) ;
#18195 = EDGE_CURVE('',#14415,#14416,#7597,.T.) ;
#18196 = EDGE_CURVE('',#14403,#14416,#11786,.T.) ;
#18197 = EDGE_CURVE('',#14404,#14057,#11787,.T.) ;
#18198 = EDGE_CURVE('',#14417,#14409,#7598,.T.) ;
#18199 = EDGE_CURVE('',#14417,#14418,#11788,.T.) ;
#18200 = EDGE_CURVE('',#14418,#14411,#7599,.T.) ;
#18201 = EDGE_CURVE('',#14050,#14419,#7600,.T.) ;
#18202 = EDGE_CURVE('',#14419,#14420,#11789,.T.) ;
#18203 = EDGE_CURVE('',#14420,#14417,#7601,.T.) ;
#18204 = EDGE_CURVE('',#14407,#14421,#7602,.T.) ;
#18205 = EDGE_CURVE('',#14421,#14422,#7603,.T.) ;
#18206 = EDGE_CURVE('',#14422,#14423,#11790,.T.) ;
#18207 = EDGE_CURVE('',#14423,#14051,#7604,.T.) ;
#18208 = EDGE_CURVE('',#14424,#14405,#7605,.T.) ;
#18209 = EDGE_CURVE('',#14424,#14421,#11791,.T.) ;
#18210 = EDGE_CURVE('',#14404,#14425,#7606,.T.) ;
#18211 = EDGE_CURVE('',#14425,#14424,#7607,.T.) ;
#18212 = EDGE_CURVE('',#14426,#14427,#11792,.T.) ;
#18213 = EDGE_CURVE('',#14427,#14428,#7608,.T.) ;
#18214 = EDGE_CURVE('',#14428,#14429,#11793,.T.) ;
#18215 = EDGE_CURVE('',#14426,#14429,#7609,.T.) ;
#18216 = EDGE_CURVE('',#14430,#14431,#11794,.T.) ;
#18217 = EDGE_CURVE('',#14431,#14429,#11795,.T.) ;
#18218 = EDGE_CURVE('',#14428,#14430,#11796,.T.) ;
#18219 = EDGE_CURVE('',#14432,#14433,#11797,.T.) ;
#18220 = EDGE_CURVE('',#14431,#14433,#7610,.T.) ;
#18221 = EDGE_CURVE('',#14430,#14432,#7611,.T.) ;
#18222 = EDGE_CURVE('',#14434,#14435,#11798,.T.) ;
#18223 = EDGE_CURVE('',#14435,#14433,#11799,.T.) ;
#18224 = EDGE_CURVE('',#14434,#14432,#11800,.T.) ;
#18225 = EDGE_CURVE('',#14436,#14437,#11801,.T.) ;
#18226 = EDGE_CURVE('',#14435,#14437,#7612,.T.) ;
#18227 = EDGE_CURVE('',#14434,#14436,#7613,.T.) ;
#18228 = EDGE_CURVE('',#14077,#14438,#11802,.T.) ;
#18229 = EDGE_CURVE('',#14438,#14437,#11803,.T.) ;
#18230 = EDGE_CURVE('',#14436,#14077,#11804,.T.) ;
#18231 = EDGE_CURVE('',#14076,#14439,#11805,.T.) ;
#18232 = EDGE_CURVE('',#14438,#14439,#7614,.T.) ;
#18233 = EDGE_CURVE('',#14426,#14439,#11806,.T.) ;
#18234 = EDGE_CURVE('',#14427,#14076,#11807,.T.) ;
#18235 = EDGE_CURVE('',#14440,#14432,#7615,.T.) ;
#18236 = EDGE_CURVE('',#14440,#14441,#11808,.T.) ;
#18237 = EDGE_CURVE('',#14441,#14434,#7616,.T.) ;
#18238 = EDGE_CURVE('',#14069,#14442,#7617,.T.) ;
#18239 = EDGE_CURVE('',#14442,#14443,#11809,.T.) ;
#18240 = EDGE_CURVE('',#14443,#14440,#7618,.T.) ;
#18241 = EDGE_CURVE('',#14430,#14444,#7619,.T.) ;
#18242 = EDGE_CURVE('',#14444,#14445,#7620,.T.) ;
#18243 = EDGE_CURVE('',#14445,#14446,#11810,.T.) ;
#18244 = EDGE_CURVE('',#14446,#14070,#7621,.T.) ;
#18245 = EDGE_CURVE('',#14447,#14428,#7622,.T.) ;
#18246 = EDGE_CURVE('',#14447,#14444,#11811,.T.) ;
#18247 = EDGE_CURVE('',#14427,#14448,#7623,.T.) ;
#18248 = EDGE_CURVE('',#14448,#14447,#7624,.T.) ;
#18249 = EDGE_CURVE('',#14449,#14450,#11812,.T.) ;
#18250 = EDGE_CURVE('',#14450,#14451,#7625,.T.) ;
#18251 = EDGE_CURVE('',#14451,#14452,#11813,.T.) ;
#18252 = EDGE_CURVE('',#14449,#14452,#7626,.T.) ;
#18253 = EDGE_CURVE('',#14453,#14454,#11814,.T.) ;
#18254 = EDGE_CURVE('',#14454,#14452,#11815,.T.) ;
#18255 = EDGE_CURVE('',#14451,#14453,#11816,.T.) ;
#18256 = EDGE_CURVE('',#14455,#14456,#11817,.T.) ;
#18257 = EDGE_CURVE('',#14454,#14456,#7627,.T.) ;
#18258 = EDGE_CURVE('',#14453,#14455,#7628,.T.) ;
#18259 = EDGE_CURVE('',#14457,#14458,#11818,.T.) ;
#18260 = EDGE_CURVE('',#14458,#14456,#11819,.T.) ;
#18261 = EDGE_CURVE('',#14457,#14455,#11820,.T.) ;
#18262 = EDGE_CURVE('',#14459,#14460,#11821,.T.) ;
#18263 = EDGE_CURVE('',#14458,#14460,#7629,.T.) ;
#18264 = EDGE_CURVE('',#14457,#14459,#7630,.T.) ;
#18265 = EDGE_CURVE('',#14096,#14461,#11822,.T.) ;
#18266 = EDGE_CURVE('',#14461,#14460,#11823,.T.) ;
#18267 = EDGE_CURVE('',#14459,#14096,#11824,.T.) ;
#18268 = EDGE_CURVE('',#14095,#14462,#11825,.T.) ;
#18269 = EDGE_CURVE('',#14461,#14462,#7631,.T.) ;
#18270 = EDGE_CURVE('',#14449,#14462,#11826,.T.) ;
#18271 = EDGE_CURVE('',#14450,#14095,#11827,.T.) ;
#18272 = EDGE_CURVE('',#14463,#14455,#7632,.T.) ;
#18273 = EDGE_CURVE('',#14463,#14464,#11828,.T.) ;
#18274 = EDGE_CURVE('',#14464,#14457,#7633,.T.) ;
#18275 = EDGE_CURVE('',#14088,#14465,#7634,.T.) ;
#18276 = EDGE_CURVE('',#14465,#14466,#11829,.T.) ;
#18277 = EDGE_CURVE('',#14466,#14463,#7635,.T.) ;
#18278 = EDGE_CURVE('',#14453,#14467,#7636,.T.) ;
#18279 = EDGE_CURVE('',#14467,#14468,#7637,.T.) ;
#18280 = EDGE_CURVE('',#14468,#14469,#11830,.T.) ;
#18281 = EDGE_CURVE('',#14469,#14089,#7638,.T.) ;
#18282 = EDGE_CURVE('',#14470,#14451,#7639,.T.) ;
#18283 = EDGE_CURVE('',#14470,#14467,#11831,.T.) ;
#18284 = EDGE_CURVE('',#14450,#14471,#7640,.T.) ;
#18285 = EDGE_CURVE('',#14471,#14470,#7641,.T.) ;
#18286 = EDGE_CURVE('',#14472,#14473,#11832,.T.) ;
#18287 = EDGE_CURVE('',#14473,#14474,#7642,.T.) ;
#18288 = EDGE_CURVE('',#14474,#14475,#11833,.T.) ;
#18289 = EDGE_CURVE('',#14475,#14472,#7643,.T.) ;
#18290 = EDGE_CURVE('',#14476,#14477,#11834,.T.) ;
#18291 = EDGE_CURVE('',#14477,#14475,#11835,.T.) ;
#18292 = EDGE_CURVE('',#14474,#14476,#11836,.T.) ;
#18293 = EDGE_CURVE('',#14478,#14479,#11837,.T.) ;
#18294 = EDGE_CURVE('',#14479,#14477,#7644,.T.) ;
#18295 = EDGE_CURVE('',#14476,#14478,#7645,.T.) ;
#18296 = EDGE_CURVE('',#14480,#14481,#11838,.T.) ;
#18297 = EDGE_CURVE('',#14481,#14479,#11839,.T.) ;
#18298 = EDGE_CURVE('',#14478,#14480,#11840,.T.) ;
#18299 = EDGE_CURVE('',#14482,#14483,#11841,.T.) ;
#18300 = EDGE_CURVE('',#14483,#14481,#7646,.T.) ;
#18301 = EDGE_CURVE('',#14480,#14482,#7647,.T.) ;
#18302 = EDGE_CURVE('',#14484,#14485,#11842,.T.) ;
#18303 = EDGE_CURVE('',#14485,#14483,#11843,.T.) ;
#18304 = EDGE_CURVE('',#14482,#14484,#11844,.T.) ;
#18305 = EDGE_CURVE('',#14486,#14487,#11845,.T.) ;
#18306 = EDGE_CURVE('',#14487,#14485,#7648,.T.) ;
#18307 = EDGE_CURVE('',#14484,#14486,#7649,.T.) ;
#18308 = EDGE_CURVE('',#14472,#14487,#11846,.T.) ;
#18309 = EDGE_CURVE('',#14486,#14473,#11847,.T.) ;
#18310 = EDGE_CURVE('',#14488,#14478,#7650,.T.) ;
#18311 = EDGE_CURVE('',#14489,#14488,#11848,.F.) ;
#18312 = EDGE_CURVE('',#14480,#14489,#7651,.T.) ;
#18313 = EDGE_CURVE('',#14476,#14490,#7652,.T.) ;
#18314 = EDGE_CURVE('',#14490,#14488,#7653,.T.) ;
#18315 = EDGE_CURVE('',#14491,#14474,#7654,.T.) ;
#18316 = EDGE_CURVE('',#14490,#14491,#11849,.F.) ;
#18317 = EDGE_CURVE('',#14473,#14492,#7655,.T.) ;
#18318 = EDGE_CURVE('',#14492,#14491,#7656,.T.) ;
#18319 = EDGE_CURVE('',#14493,#14494,#7657,.T.) ;
#18320 = EDGE_CURVE('',#14495,#14494,#7658,.T.) ;
#18321 = EDGE_CURVE('',#14495,#14496,#7659,.T.) ;
#18322 = EDGE_CURVE('',#14493,#14496,#7660,.T.) ;
#18323 = EDGE_CURVE('',#14497,#14498,#7661,.T.) ;
#18324 = EDGE_CURVE('',#14499,#14497,#11850,.T.) ;
#18325 = EDGE_CURVE('',#14500,#14499,#7662,.T.) ;
#18326 = EDGE_CURVE('',#14501,#14500,#11851,.T.) ;
#18327 = EDGE_CURVE('',#14502,#14501,#7663,.T.) ;
#18328 = EDGE_CURVE('',#14503,#14502,#11852,.T.) ;
#18329 = EDGE_CURVE('',#14504,#14503,#7664,.T.) ;
#18330 = EDGE_CURVE('',#14498,#14504,#11853,.T.) ;
#18331 = EDGE_CURVE('',#14505,#14505,#11854,.T.) ;
#18332 = EDGE_CURVE('',#14498,#14506,#11855,.T.) ;
#18333 = EDGE_CURVE('',#14506,#14507,#7665,.T.) ;
#18334 = EDGE_CURVE('',#14507,#14497,#11856,.T.) ;
#18335 = EDGE_CURVE('',#14508,#14499,#11857,.T.) ;
#18336 = EDGE_CURVE('',#14507,#14508,#11858,.T.) ;
#18337 = EDGE_CURVE('',#14509,#14500,#11859,.T.) ;
#18338 = EDGE_CURVE('',#14508,#14509,#7666,.T.) ;
#18339 = EDGE_CURVE('',#14510,#14501,#11860,.T.) ;
#18340 = EDGE_CURVE('',#14509,#14510,#11861,.T.) ;
#18341 = EDGE_CURVE('',#14511,#14502,#11862,.T.) ;
#18342 = EDGE_CURVE('',#14510,#14511,#7667,.T.) ;
#18343 = EDGE_CURVE('',#14111,#14503,#11863,.T.) ;
#18344 = EDGE_CURVE('',#14511,#14111,#11864,.T.) ;
#18345 = EDGE_CURVE('',#14112,#14504,#11865,.T.) ;
#18346 = EDGE_CURVE('',#14112,#14506,#11866,.T.) ;
#18347 = EDGE_CURVE('',#14512,#14509,#7668,.T.) ;
#18348 = EDGE_CURVE('',#14512,#14513,#11867,.T.) ;
#18349 = EDGE_CURVE('',#14513,#14510,#7669,.T.) ;
#18350 = EDGE_CURVE('',#14508,#14514,#7670,.T.) ;
#18351 = EDGE_CURVE('',#14514,#14515,#7671,.T.) ;
#18352 = EDGE_CURVE('',#14515,#14516,#11868,.T.) ;
#18353 = EDGE_CURVE('',#14516,#14108,#7672,.T.) ;
#18354 = EDGE_CURVE('',#14107,#14517,#7673,.T.) ;
#18355 = EDGE_CURVE('',#14517,#14518,#11869,.T.) ;
#18356 = EDGE_CURVE('',#14518,#14512,#7674,.T.) ;
#18357 = EDGE_CURVE('',#14507,#14519,#7675,.T.) ;
#18358 = EDGE_CURVE('',#14519,#14514,#11870,.T.) ;
#18359 = EDGE_CURVE('',#14506,#14520,#7676,.T.) ;
#18360 = EDGE_CURVE('',#14520,#14519,#7677,.T.) ;
#18361 = EDGE_CURVE('',#14513,#14521,#7678,.T.) ;
#18362 = EDGE_CURVE('',#14521,#14511,#7679,.T.) ;
#18363 = EDGE_CURVE('',#14521,#14113,#11871,.T.) ;
#18364 = EDGE_CURVE('',#14117,#14520,#11872,.T.) ;
#18365 = EDGE_CURVE('',#14489,#14522,#7680,.T.) ;
#18366 = EDGE_CURVE('',#14522,#14482,#7681,.T.) ;
#18367 = EDGE_CURVE('',#14522,#14523,#11873,.T.) ;
#18368 = EDGE_CURVE('',#14484,#14523,#7682,.T.) ;
#18369 = EDGE_CURVE('',#14524,#14486,#7683,.T.) ;
#18370 = EDGE_CURVE('',#14524,#14492,#11874,.T.) ;
#18371 = EDGE_CURVE('',#14523,#14524,#7684,.T.) ;
#18372 = EDGE_CURVE('',#14525,#14525,#11875,.T.) ;
#18373 = EDGE_CURVE('',#14119,#14516,#11876,.T.) ;
#18374 = EDGE_CURVE('',#14521,#14526,#11877,.T.) ;
#18375 = EDGE_CURVE('',#14527,#14513,#11878,.T.) ;
#18376 = EDGE_CURVE('',#14526,#14527,#7685,.T.) ;
#18377 = EDGE_CURVE('',#14528,#14119,#11879,.F.) ;
#18378 = EDGE_CURVE('',#14515,#14528,#11880,.T.) ;
#18379 = EDGE_CURVE('',#14529,#14514,#11881,.T.) ;
#18380 = EDGE_CURVE('',#14528,#14529,#7686,.T.) ;
#18381 = EDGE_CURVE('',#14118,#14530,#11882,.F.) ;
#18382 = EDGE_CURVE('',#14530,#14116,#11883,.T.) ;
#18383 = EDGE_CURVE('',#14531,#14532,#11884,.F.) ;
#18384 = EDGE_CURVE('',#14532,#14518,#11885,.T.) ;
#18385 = EDGE_CURVE('',#14517,#14531,#11886,.T.) ;
#18386 = EDGE_CURVE('',#14531,#14106,#7687,.T.) ;
#18387 = EDGE_CURVE('',#14512,#14527,#11887,.T.) ;
#18388 = EDGE_CURVE('',#14527,#14532,#7688,.T.) ;
#18389 = EDGE_CURVE('',#14533,#14110,#11888,.F.) ;
#18390 = EDGE_CURVE('',#14114,#14533,#11889,.T.) ;
#18391 = EDGE_CURVE('',#14526,#14113,#11890,.T.) ;
#18392 = EDGE_CURVE('',#14533,#14526,#7689,.T.) ;
#18393 = EDGE_CURVE('',#14532,#14533,#7690,.T.) ;
#18394 = EDGE_CURVE('',#14110,#14531,#7691,.T.) ;
#18395 = EDGE_CURVE('',#14117,#14534,#11891,.T.) ;
#18396 = EDGE_CURVE('',#14534,#14530,#7692,.T.) ;
#18397 = EDGE_CURVE('',#14530,#14528,#7693,.T.) ;
#18398 = EDGE_CURVE('',#14534,#14520,#11892,.T.) ;
#18399 = EDGE_CURVE('',#14529,#14534,#7694,.T.) ;
#18400 = EDGE_CURVE('',#14519,#14529,#11893,.T.) ;
#18401 = EDGE_CURVE('',#14535,#14536,#7695,.T.) ;
#18402 = EDGE_CURVE('',#14536,#14537,#7696,.T.) ;
#18403 = EDGE_CURVE('',#14537,#14538,#7697,.T.) ;
#18404 = EDGE_CURVE('',#14538,#14535,#7698,.T.) ;
#18405 = EDGE_CURVE('',#14522,#14536,#11894,.T.) ;
#18406 = EDGE_CURVE('',#14536,#14523,#11895,.T.) ;
#18407 = EDGE_CURVE('',#14524,#14535,#11896,.T.) ;
#18408 = EDGE_CURVE('',#14535,#14492,#11897,.T.) ;
#18409 = EDGE_CURVE('',#14491,#14538,#11898,.F.) ;
#18410 = EDGE_CURVE('',#14537,#14489,#11899,.F.) ;
#18411 = EDGE_CURVE('',#14488,#14537,#11900,.F.) ;
#18412 = EDGE_CURVE('',#14538,#14490,#11901,.F.) ;
#18413 = EDGE_CURVE('',#14100,#14469,#11902,.T.) ;
#18414 = EDGE_CURVE('',#14539,#14540,#11903,.T.) ;
#18415 = EDGE_CURVE('',#14464,#14539,#7699,.T.) ;
#18416 = EDGE_CURVE('',#14541,#14464,#11904,.T.) ;
#18417 = EDGE_CURVE('',#14540,#14541,#7700,.T.) ;
#18418 = EDGE_CURVE('',#14542,#14100,#11905,.F.) ;
#18419 = EDGE_CURVE('',#14468,#14542,#11906,.T.) ;
#18420 = EDGE_CURVE('',#14543,#14467,#11907,.T.) ;
#18421 = EDGE_CURVE('',#14542,#14543,#7701,.T.) ;
#18422 = EDGE_CURVE('',#14099,#14544,#11908,.F.) ;
#18423 = EDGE_CURVE('',#14544,#14093,#11909,.T.) ;
#18424 = EDGE_CURVE('',#14545,#14546,#11910,.F.) ;
#18425 = EDGE_CURVE('',#14546,#14466,#11911,.T.) ;
#18426 = EDGE_CURVE('',#14465,#14545,#11912,.T.) ;
#18427 = EDGE_CURVE('',#14545,#14087,#7702,.T.) ;
#18428 = EDGE_CURVE('',#14463,#14541,#11913,.T.) ;
#18429 = EDGE_CURVE('',#14541,#14546,#7703,.T.) ;
#18430 = EDGE_CURVE('',#14547,#14091,#11914,.F.) ;
#18431 = EDGE_CURVE('',#14098,#14547,#11915,.T.) ;
#18432 = EDGE_CURVE('',#14540,#14097,#11916,.T.) ;
#18433 = EDGE_CURVE('',#14547,#14540,#7704,.T.) ;
#18434 = EDGE_CURVE('',#14546,#14547,#7705,.T.) ;
#18435 = EDGE_CURVE('',#14091,#14545,#7706,.T.) ;
#18436 = EDGE_CURVE('',#14094,#14548,#11917,.T.) ;
#18437 = EDGE_CURVE('',#14548,#14544,#7707,.T.) ;
#18438 = EDGE_CURVE('',#14544,#14542,#7708,.T.) ;
#18439 = EDGE_CURVE('',#14539,#14097,#11918,.T.) ;
#18440 = EDGE_CURVE('',#14548,#14471,#11919,.T.) ;
#18441 = EDGE_CURVE('',#14543,#14548,#7709,.T.) ;
#18442 = EDGE_CURVE('',#14470,#14543,#11920,.T.) ;
#18443 = EDGE_CURVE('',#14094,#14471,#11921,.T.) ;
#18444 = EDGE_CURVE('',#14549,#14550,#7710,.T.) ;
#18445 = EDGE_CURVE('',#14550,#14551,#7711,.T.) ;
#18446 = EDGE_CURVE('',#14551,#14552,#7712,.T.) ;
#18447 = EDGE_CURVE('',#14552,#14549,#7713,.T.) ;
#18448 = EDGE_CURVE('',#14553,#14550,#11922,.T.) ;
#18449 = EDGE_CURVE('',#14550,#14554,#11923,.T.) ;
#18450 = EDGE_CURVE('',#14553,#14554,#11924,.T.) ;
#18451 = EDGE_CURVE('',#14555,#14549,#11925,.T.) ;
#18452 = EDGE_CURVE('',#14549,#14287,#11926,.T.) ;
#18453 = EDGE_CURVE('',#14555,#14287,#11927,.T.) ;
#18454 = EDGE_CURVE('',#14554,#14555,#7714,.T.) ;
#18455 = EDGE_CURVE('',#14286,#14552,#11928,.F.) ;
#18456 = EDGE_CURVE('',#14284,#14553,#7715,.T.) ;
#18457 = EDGE_CURVE('',#14551,#14284,#11929,.F.) ;
#18458 = EDGE_CURVE('',#14283,#14551,#11930,.F.) ;
#18459 = EDGE_CURVE('',#14552,#14285,#11931,.F.) ;
#18460 = EDGE_CURVE('',#14081,#14446,#11932,.T.) ;
#18461 = EDGE_CURVE('',#14556,#14557,#11933,.T.) ;
#18462 = EDGE_CURVE('',#14441,#14556,#7716,.T.) ;
#18463 = EDGE_CURVE('',#14558,#14441,#11934,.T.) ;
#18464 = EDGE_CURVE('',#14557,#14558,#7717,.T.) ;
#18465 = EDGE_CURVE('',#14559,#14081,#11935,.F.) ;
#18466 = EDGE_CURVE('',#14445,#14559,#11936,.T.) ;
#18467 = EDGE_CURVE('',#14560,#14444,#11937,.T.) ;
#18468 = EDGE_CURVE('',#14559,#14560,#7718,.T.) ;
#18469 = EDGE_CURVE('',#14080,#14561,#11938,.F.) ;
#18470 = EDGE_CURVE('',#14561,#14074,#11939,.T.) ;
#18471 = EDGE_CURVE('',#14562,#14563,#11940,.F.) ;
#18472 = EDGE_CURVE('',#14563,#14443,#11941,.T.) ;
#18473 = EDGE_CURVE('',#14442,#14562,#11942,.T.) ;
#18474 = EDGE_CURVE('',#14562,#14068,#7719,.T.) ;
#18475 = EDGE_CURVE('',#14440,#14558,#11943,.T.) ;
#18476 = EDGE_CURVE('',#14558,#14563,#7720,.T.) ;
#18477 = EDGE_CURVE('',#14564,#14072,#11944,.F.) ;
#18478 = EDGE_CURVE('',#14079,#14564,#11945,.T.) ;
#18479 = EDGE_CURVE('',#14557,#14078,#11946,.T.) ;
#18480 = EDGE_CURVE('',#14564,#14557,#7721,.T.) ;
#18481 = EDGE_CURVE('',#14563,#14564,#7722,.T.) ;
#18482 = EDGE_CURVE('',#14072,#14562,#7723,.T.) ;
#18483 = EDGE_CURVE('',#14075,#14565,#11947,.T.) ;
#18484 = EDGE_CURVE('',#14565,#14561,#7724,.T.) ;
#18485 = EDGE_CURVE('',#14561,#14559,#7725,.T.) ;
#18486 = EDGE_CURVE('',#14556,#14078,#11948,.T.) ;
#18487 = EDGE_CURVE('',#14565,#14448,#11949,.T.) ;
#18488 = EDGE_CURVE('',#14560,#14565,#7726,.T.) ;
#18489 = EDGE_CURVE('',#14447,#14560,#11950,.T.) ;
#18490 = EDGE_CURVE('',#14075,#14448,#11951,.T.) ;
#18491 = EDGE_CURVE('',#14566,#14567,#7727,.T.) ;
#18492 = EDGE_CURVE('',#14567,#14568,#7728,.T.) ;
#18493 = EDGE_CURVE('',#14568,#14569,#7729,.T.) ;
#18494 = EDGE_CURVE('',#14569,#14566,#7730,.T.) ;
#18495 = EDGE_CURVE('',#14570,#14567,#11952,.T.) ;
#18496 = EDGE_CURVE('',#14567,#14571,#11953,.T.) ;
#18497 = EDGE_CURVE('',#14570,#14571,#11954,.T.) ;
#18498 = EDGE_CURVE('',#14572,#14566,#11955,.T.) ;
#18499 = EDGE_CURVE('',#14566,#14266,#11956,.T.) ;
#18500 = EDGE_CURVE('',#14572,#14266,#11957,.T.) ;
#18501 = EDGE_CURVE('',#14571,#14572,#7731,.T.) ;
#18502 = EDGE_CURVE('',#14265,#14569,#11958,.F.) ;
#18503 = EDGE_CURVE('',#14263,#14570,#7732,.T.) ;
#18504 = EDGE_CURVE('',#14568,#14263,#11959,.F.) ;
#18505 = EDGE_CURVE('',#14262,#14568,#11960,.F.) ;
#18506 = EDGE_CURVE('',#14569,#14264,#11961,.F.) ;
#18507 = EDGE_CURVE('',#14062,#14423,#11962,.T.) ;
#18508 = EDGE_CURVE('',#14573,#14574,#11963,.T.) ;
#18509 = EDGE_CURVE('',#14418,#14573,#7733,.T.) ;
#18510 = EDGE_CURVE('',#14575,#14418,#11964,.T.) ;
#18511 = EDGE_CURVE('',#14574,#14575,#7734,.T.) ;
#18512 = EDGE_CURVE('',#14576,#14062,#11965,.F.) ;
#18513 = EDGE_CURVE('',#14422,#14576,#11966,.T.) ;
#18514 = EDGE_CURVE('',#14577,#14421,#11967,.T.) ;
#18515 = EDGE_CURVE('',#14576,#14577,#7735,.T.) ;
#18516 = EDGE_CURVE('',#14061,#14578,#11968,.F.) ;
#18517 = EDGE_CURVE('',#14578,#14055,#11969,.T.) ;
#18518 = EDGE_CURVE('',#14579,#14580,#11970,.F.) ;
#18519 = EDGE_CURVE('',#14580,#14420,#11971,.T.) ;
#18520 = EDGE_CURVE('',#14419,#14579,#11972,.T.) ;
#18521 = EDGE_CURVE('',#14579,#14049,#7736,.T.) ;
#18522 = EDGE_CURVE('',#14417,#14575,#11973,.T.) ;
#18523 = EDGE_CURVE('',#14575,#14580,#7737,.T.) ;
#18524 = EDGE_CURVE('',#14581,#14053,#11974,.F.) ;
#18525 = EDGE_CURVE('',#14060,#14581,#11975,.T.) ;
#18526 = EDGE_CURVE('',#14574,#14059,#11976,.T.) ;
#18527 = EDGE_CURVE('',#14581,#14574,#7738,.T.) ;
#18528 = EDGE_CURVE('',#14580,#14581,#7739,.T.) ;
#18529 = EDGE_CURVE('',#14053,#14579,#7740,.T.) ;
#18530 = EDGE_CURVE('',#14056,#14582,#11977,.T.) ;
#18531 = EDGE_CURVE('',#14582,#14578,#7741,.T.) ;
#18532 = EDGE_CURVE('',#14578,#14576,#7742,.T.) ;
#18533 = EDGE_CURVE('',#14573,#14059,#11978,.T.) ;
#18534 = EDGE_CURVE('',#14582,#14425,#11979,.T.) ;
#18535 = EDGE_CURVE('',#14577,#14582,#7743,.T.) ;
#18536 = EDGE_CURVE('',#14424,#14577,#11980,.T.) ;
#18537 = EDGE_CURVE('',#14056,#14425,#11981,.T.) ;
#18538 = EDGE_CURVE('',#14583,#14584,#7744,.T.) ;
#18539 = EDGE_CURVE('',#14584,#14585,#7745,.T.) ;
#18540 = EDGE_CURVE('',#14585,#14586,#7746,.T.) ;
#18541 = EDGE_CURVE('',#14586,#14583,#7747,.T.) ;
#18542 = EDGE_CURVE('',#14587,#14584,#11982,.T.) ;
#18543 = EDGE_CURVE('',#14584,#14588,#11983,.T.) ;
#18544 = EDGE_CURVE('',#14587,#14588,#11984,.T.) ;
#18545 = EDGE_CURVE('',#14589,#14583,#11985,.T.) ;
#18546 = EDGE_CURVE('',#14583,#14245,#11986,.T.) ;
#18547 = EDGE_CURVE('',#14589,#14245,#11987,.T.) ;
#18548 = EDGE_CURVE('',#14588,#14589,#7748,.T.) ;
#18549 = EDGE_CURVE('',#14244,#14586,#11988,.F.) ;
#18550 = EDGE_CURVE('',#14242,#14587,#7749,.T.) ;
#18551 = EDGE_CURVE('',#14585,#14242,#11989,.F.) ;
#18552 = EDGE_CURVE('',#14241,#14585,#11990,.F.) ;
#18553 = EDGE_CURVE('',#14586,#14243,#11991,.F.) ;
#18554 = EDGE_CURVE('',#14043,#14400,#11992,.T.) ;
#18555 = EDGE_CURVE('',#14590,#14591,#11993,.T.) ;
#18556 = EDGE_CURVE('',#14395,#14590,#7750,.T.) ;
#18557 = EDGE_CURVE('',#14592,#14395,#11994,.T.) ;
#18558 = EDGE_CURVE('',#14591,#14592,#7751,.T.) ;
#18559 = EDGE_CURVE('',#14593,#14043,#11995,.F.) ;
#18560 = EDGE_CURVE('',#14399,#14593,#11996,.T.) ;
#18561 = EDGE_CURVE('',#14594,#14398,#11997,.T.) ;
#18562 = EDGE_CURVE('',#14593,#14594,#7752,.T.) ;
#18563 = EDGE_CURVE('',#14042,#14595,#11998,.F.) ;
#18564 = EDGE_CURVE('',#14595,#14036,#11999,.T.) ;
#18565 = EDGE_CURVE('',#14596,#14597,#12000,.F.) ;
#18566 = EDGE_CURVE('',#14597,#14397,#12001,.T.) ;
#18567 = EDGE_CURVE('',#14396,#14596,#12002,.T.) ;
#18568 = EDGE_CURVE('',#14596,#14030,#7753,.T.) ;
#18569 = EDGE_CURVE('',#14394,#14592,#12003,.T.) ;
#18570 = EDGE_CURVE('',#14592,#14597,#7754,.T.) ;
#18571 = EDGE_CURVE('',#14598,#14034,#12004,.F.) ;
#18572 = EDGE_CURVE('',#14041,#14598,#12005,.T.) ;
#18573 = EDGE_CURVE('',#14591,#14040,#12006,.T.) ;
#18574 = EDGE_CURVE('',#14598,#14591,#7755,.T.) ;
#18575 = EDGE_CURVE('',#14597,#14598,#7756,.T.) ;
#18576 = EDGE_CURVE('',#14034,#14596,#7757,.T.) ;
#18577 = EDGE_CURVE('',#14037,#14599,#12007,.T.) ;
#18578 = EDGE_CURVE('',#14599,#14595,#7758,.T.) ;
#18579 = EDGE_CURVE('',#14595,#14593,#7759,.T.) ;
#18580 = EDGE_CURVE('',#14590,#14040,#12008,.T.) ;
#18581 = EDGE_CURVE('',#14599,#14402,#12009,.T.) ;
#18582 = EDGE_CURVE('',#14594,#14599,#7760,.T.) ;
#18583 = EDGE_CURVE('',#14401,#14594,#12010,.T.) ;
#18584 = EDGE_CURVE('',#14037,#14402,#12011,.T.) ;
#18585 = EDGE_CURVE('',#14600,#14601,#7761,.T.) ;
#18586 = EDGE_CURVE('',#14601,#14602,#7762,.T.) ;
#18587 = EDGE_CURVE('',#14602,#14603,#7763,.T.) ;
#18588 = EDGE_CURVE('',#14603,#14600,#7764,.T.) ;
#18589 = EDGE_CURVE('',#14604,#14601,#12012,.T.) ;
#18590 = EDGE_CURVE('',#14601,#14605,#12013,.T.) ;
#18591 = EDGE_CURVE('',#14604,#14605,#12014,.T.) ;
#18592 = EDGE_CURVE('',#14606,#14600,#12015,.T.) ;
#18593 = EDGE_CURVE('',#14600,#14224,#12016,.T.) ;
#18594 = EDGE_CURVE('',#14606,#14224,#12017,.T.) ;
#18595 = EDGE_CURVE('',#14605,#14606,#7765,.T.) ;
#18596 = EDGE_CURVE('',#14223,#14603,#12018,.F.) ;
#18597 = EDGE_CURVE('',#14221,#14604,#7766,.T.) ;
#18598 = EDGE_CURVE('',#14602,#14221,#12019,.F.) ;
#18599 = EDGE_CURVE('',#14220,#14602,#12020,.F.) ;
#18600 = EDGE_CURVE('',#14603,#14222,#12021,.F.) ;
#18601 = EDGE_CURVE('',#14024,#14377,#12022,.T.) ;
#18602 = EDGE_CURVE('',#14607,#14608,#12023,.T.) ;
#18603 = EDGE_CURVE('',#14372,#14607,#7767,.T.) ;
#18604 = EDGE_CURVE('',#14609,#14372,#12024,.T.) ;
#18605 = EDGE_CURVE('',#14608,#14609,#7768,.T.) ;
#18606 = EDGE_CURVE('',#14610,#14024,#12025,.F.) ;
#18607 = EDGE_CURVE('',#14376,#14610,#12026,.T.) ;
#18608 = EDGE_CURVE('',#14611,#14375,#12027,.T.) ;
#18609 = EDGE_CURVE('',#14610,#14611,#7769,.T.) ;
#18610 = EDGE_CURVE('',#14023,#14612,#12028,.F.) ;
#18611 = EDGE_CURVE('',#14612,#14017,#12029,.T.) ;
#18612 = EDGE_CURVE('',#14613,#14614,#12030,.F.) ;
#18613 = EDGE_CURVE('',#14614,#14374,#12031,.T.) ;
#18614 = EDGE_CURVE('',#14373,#14613,#12032,.T.) ;
#18615 = EDGE_CURVE('',#14613,#14011,#7770,.T.) ;
#18616 = EDGE_CURVE('',#14371,#14609,#12033,.T.) ;
#18617 = EDGE_CURVE('',#14609,#14614,#7771,.T.) ;
#18618 = EDGE_CURVE('',#14615,#14015,#12034,.F.) ;
#18619 = EDGE_CURVE('',#14022,#14615,#12035,.T.) ;
#18620 = EDGE_CURVE('',#14608,#14021,#12036,.T.) ;
#18621 = EDGE_CURVE('',#14615,#14608,#7772,.T.) ;
#18622 = EDGE_CURVE('',#14614,#14615,#7773,.T.) ;
#18623 = EDGE_CURVE('',#14015,#14613,#7774,.T.) ;
#18624 = EDGE_CURVE('',#14018,#14616,#12037,.T.) ;
#18625 = EDGE_CURVE('',#14616,#14612,#7775,.T.) ;
#18626 = EDGE_CURVE('',#14612,#14610,#7776,.T.) ;
#18627 = EDGE_CURVE('',#14607,#14021,#12038,.T.) ;
#18628 = EDGE_CURVE('',#14616,#14379,#12039,.T.) ;
#18629 = EDGE_CURVE('',#14611,#14616,#7777,.T.) ;
#18630 = EDGE_CURVE('',#14378,#14611,#12040,.T.) ;
#18631 = EDGE_CURVE('',#14018,#14379,#12041,.T.) ;
#18632 = EDGE_CURVE('',#14617,#14618,#7778,.T.) ;
#18633 = EDGE_CURVE('',#14618,#14619,#7779,.T.) ;
#18634 = EDGE_CURVE('',#14619,#14620,#7780,.T.) ;
#18635 = EDGE_CURVE('',#14620,#14617,#7781,.T.) ;
#18636 = EDGE_CURVE('',#14621,#14618,#12042,.T.) ;
#18637 = EDGE_CURVE('',#14618,#14622,#12043,.T.) ;
#18638 = EDGE_CURVE('',#14621,#14622,#12044,.T.) ;
#18639 = EDGE_CURVE('',#14623,#14617,#12045,.T.) ;
#18640 = EDGE_CURVE('',#14617,#14203,#12046,.T.) ;
#18641 = EDGE_CURVE('',#14623,#14203,#12047,.T.) ;
#18642 = EDGE_CURVE('',#14622,#14623,#7782,.T.) ;
#18643 = EDGE_CURVE('',#14202,#14620,#12048,.F.) ;
#18644 = EDGE_CURVE('',#14200,#14621,#7783,.T.) ;
#18645 = EDGE_CURVE('',#14619,#14200,#12049,.F.) ;
#18646 = EDGE_CURVE('',#14199,#14619,#12050,.F.) ;
#18647 = EDGE_CURVE('',#14620,#14201,#12051,.F.) ;
#18648 = EDGE_CURVE('',#14005,#14354,#12052,.T.) ;
#18649 = EDGE_CURVE('',#14624,#14625,#12053,.T.) ;
#18650 = EDGE_CURVE('',#14349,#14624,#7784,.T.) ;
#18651 = EDGE_CURVE('',#14626,#14349,#12054,.T.) ;
#18652 = EDGE_CURVE('',#14625,#14626,#7785,.T.) ;
#18653 = EDGE_CURVE('',#14627,#14005,#12055,.F.) ;
#18654 = EDGE_CURVE('',#14353,#14627,#12056,.T.) ;
#18655 = EDGE_CURVE('',#14628,#14352,#12057,.T.) ;
#18656 = EDGE_CURVE('',#14627,#14628,#7786,.T.) ;
#18657 = EDGE_CURVE('',#14004,#14629,#12058,.F.) ;
#18658 = EDGE_CURVE('',#14629,#13998,#12059,.T.) ;
#18659 = EDGE_CURVE('',#14630,#14631,#12060,.F.) ;
#18660 = EDGE_CURVE('',#14631,#14351,#12061,.T.) ;
#18661 = EDGE_CURVE('',#14350,#14630,#12062,.T.) ;
#18662 = EDGE_CURVE('',#14630,#13992,#7787,.T.) ;
#18663 = EDGE_CURVE('',#14348,#14626,#12063,.T.) ;
#18664 = EDGE_CURVE('',#14626,#14631,#7788,.T.) ;
#18665 = EDGE_CURVE('',#14632,#13996,#12064,.F.) ;
#18666 = EDGE_CURVE('',#14003,#14632,#12065,.T.) ;
#18667 = EDGE_CURVE('',#14625,#14002,#12066,.T.) ;
#18668 = EDGE_CURVE('',#14632,#14625,#7789,.T.) ;
#18669 = EDGE_CURVE('',#14631,#14632,#7790,.T.) ;
#18670 = EDGE_CURVE('',#13996,#14630,#7791,.T.) ;
#18671 = EDGE_CURVE('',#13999,#14633,#12067,.T.) ;
#18672 = EDGE_CURVE('',#14633,#14629,#7792,.T.) ;
#18673 = EDGE_CURVE('',#14629,#14627,#7793,.T.) ;
#18674 = EDGE_CURVE('',#14624,#14002,#12068,.T.) ;
#18675 = EDGE_CURVE('',#14633,#14356,#12069,.T.) ;
#18676 = EDGE_CURVE('',#14628,#14633,#7794,.T.) ;
#18677 = EDGE_CURVE('',#14355,#14628,#12070,.T.) ;
#18678 = EDGE_CURVE('',#13999,#14356,#12071,.T.) ;
#18679 = EDGE_CURVE('',#14634,#14635,#7795,.T.) ;
#18680 = EDGE_CURVE('',#14635,#14636,#7796,.T.) ;
#18681 = EDGE_CURVE('',#14636,#14637,#7797,.T.) ;
#18682 = EDGE_CURVE('',#14637,#14634,#7798,.T.) ;
#18683 = EDGE_CURVE('',#14638,#14635,#12072,.T.) ;
#18684 = EDGE_CURVE('',#14635,#14639,#12073,.T.) ;
#18685 = EDGE_CURVE('',#14638,#14639,#12074,.T.) ;
#18686 = EDGE_CURVE('',#14640,#14634,#12075,.T.) ;
#18687 = EDGE_CURVE('',#14634,#14182,#12076,.T.) ;
#18688 = EDGE_CURVE('',#14640,#14182,#12077,.T.) ;
#18689 = EDGE_CURVE('',#14639,#14640,#7799,.T.) ;
#18690 = EDGE_CURVE('',#14181,#14637,#12078,.F.) ;
#18691 = EDGE_CURVE('',#14179,#14638,#7800,.T.) ;
#18692 = EDGE_CURVE('',#14636,#14179,#12079,.F.) ;
#18693 = EDGE_CURVE('',#14178,#14636,#12080,.F.) ;
#18694 = EDGE_CURVE('',#14637,#14180,#12081,.F.) ;
#18695 = EDGE_CURVE('',#13986,#14331,#12082,.T.) ;
#18696 = EDGE_CURVE('',#14641,#14642,#12083,.T.) ;
#18697 = EDGE_CURVE('',#14326,#14641,#7801,.T.) ;
#18698 = EDGE_CURVE('',#14643,#14326,#12084,.T.) ;
#18699 = EDGE_CURVE('',#14642,#14643,#7802,.T.) ;
#18700 = EDGE_CURVE('',#14644,#13986,#12085,.F.) ;
#18701 = EDGE_CURVE('',#14330,#14644,#12086,.T.) ;
#18702 = EDGE_CURVE('',#14645,#14329,#12087,.T.) ;
#18703 = EDGE_CURVE('',#14644,#14645,#7803,.T.) ;
#18704 = EDGE_CURVE('',#13985,#14646,#12088,.F.) ;
#18705 = EDGE_CURVE('',#14646,#13979,#12089,.T.) ;
#18706 = EDGE_CURVE('',#14647,#14648,#12090,.F.) ;
#18707 = EDGE_CURVE('',#14648,#14328,#12091,.T.) ;
#18708 = EDGE_CURVE('',#14327,#14647,#12092,.T.) ;
#18709 = EDGE_CURVE('',#14647,#13973,#7804,.T.) ;
#18710 = EDGE_CURVE('',#14325,#14643,#12093,.T.) ;
#18711 = EDGE_CURVE('',#14643,#14648,#7805,.T.) ;
#18712 = EDGE_CURVE('',#14649,#13977,#12094,.F.) ;
#18713 = EDGE_CURVE('',#13984,#14649,#12095,.T.) ;
#18714 = EDGE_CURVE('',#14642,#13983,#12096,.T.) ;
#18715 = EDGE_CURVE('',#14649,#14642,#7806,.T.) ;
#18716 = EDGE_CURVE('',#14648,#14649,#7807,.T.) ;
#18717 = EDGE_CURVE('',#13977,#14647,#7808,.T.) ;
#18718 = EDGE_CURVE('',#13980,#14650,#12097,.T.) ;
#18719 = EDGE_CURVE('',#14650,#14646,#7809,.T.) ;
#18720 = EDGE_CURVE('',#14646,#14644,#7810,.T.) ;
#18721 = EDGE_CURVE('',#14641,#13983,#12098,.T.) ;
#18722 = EDGE_CURVE('',#14650,#14333,#12099,.T.) ;
#18723 = EDGE_CURVE('',#14645,#14650,#7811,.T.) ;
#18724 = EDGE_CURVE('',#14332,#14645,#12100,.T.) ;
#18725 = EDGE_CURVE('',#13980,#14333,#12101,.T.) ;
#18726 = EDGE_CURVE('',#14651,#14652,#7812,.T.) ;
#18727 = EDGE_CURVE('',#14652,#14653,#7813,.T.) ;
#18728 = EDGE_CURVE('',#14653,#14654,#7814,.T.) ;
#18729 = EDGE_CURVE('',#14654,#14651,#7815,.T.) ;
#18730 = EDGE_CURVE('',#14655,#14652,#12102,.T.) ;
#18731 = EDGE_CURVE('',#14652,#14656,#12103,.T.) ;
#18732 = EDGE_CURVE('',#14655,#14656,#12104,.T.) ;
#18733 = EDGE_CURVE('',#14657,#14651,#12105,.T.) ;
#18734 = EDGE_CURVE('',#14651,#14161,#12106,.T.) ;
#18735 = EDGE_CURVE('',#14657,#14161,#12107,.T.) ;
#18736 = EDGE_CURVE('',#14656,#14657,#7816,.T.) ;
#18737 = EDGE_CURVE('',#14160,#14654,#12108,.F.) ;
#18738 = EDGE_CURVE('',#14158,#14655,#7817,.T.) ;
#18739 = EDGE_CURVE('',#14653,#14158,#12109,.F.) ;
#18740 = EDGE_CURVE('',#14157,#14653,#12110,.F.) ;
#18741 = EDGE_CURVE('',#14654,#14159,#12111,.F.) ;
#18742 = EDGE_CURVE('',#13967,#14308,#12112,.T.) ;
#18743 = EDGE_CURVE('',#14658,#14659,#12113,.T.) ;
#18744 = EDGE_CURVE('',#14303,#14658,#7818,.T.) ;
#18745 = EDGE_CURVE('',#14660,#14303,#12114,.T.) ;
#18746 = EDGE_CURVE('',#14659,#14660,#7819,.T.) ;
#18747 = EDGE_CURVE('',#14661,#13967,#12115,.F.) ;
#18748 = EDGE_CURVE('',#14307,#14661,#12116,.T.) ;
#18749 = EDGE_CURVE('',#14662,#14306,#12117,.T.) ;
#18750 = EDGE_CURVE('',#14661,#14662,#7820,.T.) ;
#18751 = EDGE_CURVE('',#13966,#14663,#12118,.F.) ;
#18752 = EDGE_CURVE('',#14663,#13960,#12119,.T.) ;
#18753 = EDGE_CURVE('',#14664,#14665,#12120,.F.) ;
#18754 = EDGE_CURVE('',#14665,#14305,#12121,.T.) ;
#18755 = EDGE_CURVE('',#14304,#14664,#12122,.T.) ;
#18756 = EDGE_CURVE('',#14664,#13954,#7821,.T.) ;
#18757 = EDGE_CURVE('',#14302,#14660,#12123,.T.) ;
#18758 = EDGE_CURVE('',#14660,#14665,#7822,.T.) ;
#18759 = EDGE_CURVE('',#14666,#13958,#12124,.F.) ;
#18760 = EDGE_CURVE('',#13965,#14666,#12125,.T.) ;
#18761 = EDGE_CURVE('',#14659,#13964,#12126,.T.) ;
#18762 = EDGE_CURVE('',#14666,#14659,#7823,.T.) ;
#18763 = EDGE_CURVE('',#14665,#14666,#7824,.T.) ;
#18764 = EDGE_CURVE('',#13958,#14664,#7825,.T.) ;
#18765 = EDGE_CURVE('',#13961,#14667,#12127,.T.) ;
#18766 = EDGE_CURVE('',#14667,#14663,#7826,.T.) ;
#18767 = EDGE_CURVE('',#14663,#14661,#7827,.T.) ;
#18768 = EDGE_CURVE('',#14658,#13964,#12128,.T.) ;
#18769 = EDGE_CURVE('',#14667,#14310,#12129,.T.) ;
#18770 = EDGE_CURVE('',#14662,#14667,#7828,.T.) ;
#18771 = EDGE_CURVE('',#14309,#14662,#12130,.T.) ;
#18772 = EDGE_CURVE('',#13961,#14310,#12131,.T.) ;
#18773 = EDGE_CURVE('',#14668,#14669,#7829,.T.) ;
#18774 = EDGE_CURVE('',#14669,#14670,#7830,.T.) ;
#18775 = EDGE_CURVE('',#14670,#14671,#7831,.T.) ;
#18776 = EDGE_CURVE('',#14671,#14668,#7832,.T.) ;
#18777 = EDGE_CURVE('',#14672,#14669,#12132,.T.) ;
#18778 = EDGE_CURVE('',#14669,#14673,#12133,.T.) ;
#18779 = EDGE_CURVE('',#14672,#14673,#12134,.T.) ;
#18780 = EDGE_CURVE('',#14674,#14668,#12135,.T.) ;
#18781 = EDGE_CURVE('',#14668,#14140,#12136,.T.) ;
#18782 = EDGE_CURVE('',#14674,#14140,#12137,.T.) ;
#18783 = EDGE_CURVE('',#14673,#14674,#7833,.T.) ;
#18784 = EDGE_CURVE('',#14139,#14671,#12138,.F.) ;
#18785 = EDGE_CURVE('',#14137,#14672,#7834,.T.) ;
#18786 = EDGE_CURVE('',#14670,#14137,#12139,.F.) ;
#18787 = EDGE_CURVE('',#14136,#14670,#12140,.F.) ;
#18788 = EDGE_CURVE('',#14671,#14138,#12141,.F.) ;
#18789 = EDGE_CURVE('',#13769,#13812,#7835,.T.) ;
#18790 = EDGE_CURVE('',#13811,#13770,#7836,.T.) ;
#18791 = EDGE_CURVE('',#13826,#13774,#7837,.T.) ;
#18792 = EDGE_CURVE('',#13773,#13827,#7838,.T.) ;
#18793 = EDGE_CURVE('',#13841,#13778,#7839,.T.) ;
#18794 = EDGE_CURVE('',#13777,#13842,#7840,.T.) ;
#18795 = EDGE_CURVE('',#13856,#13782,#7841,.T.) ;
#18796 = EDGE_CURVE('',#13781,#13857,#7842,.T.) ;
#18797 = EDGE_CURVE('',#13870,#13786,#7843,.T.) ;
#18798 = EDGE_CURVE('',#13785,#13869,#7844,.T.) ;
#18799 = EDGE_CURVE('',#13885,#13790,#7845,.T.) ;
#18800 = EDGE_CURVE('',#13789,#13884,#7846,.T.) ;
#18801 = EDGE_CURVE('',#13900,#13794,#7847,.T.) ;
#18802 = EDGE_CURVE('',#13793,#13899,#7848,.T.) ;
#18803 = EDGE_CURVE('',#13915,#13798,#7849,.T.) ;
#18804 = EDGE_CURVE('',#13797,#13914,#7850,.T.) ;
#18805 = EDGE_CURVE('',#13929,#13802,#7851,.T.) ;
#18806 = EDGE_CURVE('',#13801,#13928,#7852,.T.) ;
#18807 = EDGE_CURVE('',#13779,#13839,#7853,.T.) ;
#18808 = EDGE_CURVE('',#13840,#13776,#7854,.T.) ;
#18809 = EDGE_CURVE('',#13901,#13792,#7855,.T.) ;
#18810 = EDGE_CURVE('',#13795,#13902,#7856,.T.) ;
#18811 = EDGE_CURVE('',#13916,#13796,#7857,.T.) ;
#18812 = EDGE_CURVE('',#13799,#13917,#7858,.T.) ;
#18813 = EDGE_CURVE('',#13783,#13854,#7859,.T.) ;
#18814 = EDGE_CURVE('',#13855,#13780,#7860,.T.) ;
#18815 = EDGE_CURVE('',#13775,#13824,#7861,.T.) ;
#18816 = EDGE_CURVE('',#13825,#13772,#7862,.T.) ;
#18817 = EDGE_CURVE('',#13886,#13788,#7863,.T.) ;
#18818 = EDGE_CURVE('',#13791,#13887,#7864,.T.) ;
#18819 = EDGE_CURVE('',#13930,#13800,#7865,.T.) ;
#18820 = EDGE_CURVE('',#13803,#13931,#7866,.T.) ;
#18821 = EDGE_CURVE('',#13871,#13784,#7867,.T.) ;
#18822 = EDGE_CURVE('',#13787,#13872,#7868,.T.) ;
#18823 = EDGE_CURVE('',#13771,#13809,#7869,.T.) ;
#18824 = EDGE_CURVE('',#13810,#13768,#7870,.T.) ;
#18825 = EDGE_CURVE('',#14675,#14676,#7871,.T.) ;
#18826 = EDGE_CURVE('',#14677,#14676,#7872,.T.) ;
#18827 = EDGE_CURVE('',#14677,#14678,#7873,.T.) ;
#18828 = EDGE_CURVE('',#14679,#14678,#7874,.T.) ;
#18829 = EDGE_CURVE('',#14679,#14680,#7875,.T.) ;
#18830 = EDGE_CURVE('',#14681,#14680,#7876,.T.) ;
#18831 = EDGE_CURVE('',#14681,#14682,#7877,.T.) ;
#18832 = EDGE_CURVE('',#14683,#14682,#7878,.T.) ;
#18833 = EDGE_CURVE('',#14683,#14684,#7879,.T.) ;
#18834 = EDGE_CURVE('',#14685,#14684,#7880,.T.) ;
#18835 = EDGE_CURVE('',#14685,#14686,#7881,.T.) ;
#18836 = EDGE_CURVE('',#14687,#14686,#7882,.T.) ;
#18837 = EDGE_CURVE('',#14687,#14688,#7883,.T.) ;
#18838 = EDGE_CURVE('',#14689,#14688,#7884,.T.) ;
#18839 = EDGE_CURVE('',#14689,#14690,#7885,.T.) ;
#18840 = EDGE_CURVE('',#14691,#14690,#7886,.T.) ;
#18841 = EDGE_CURVE('',#14691,#14692,#7887,.T.) ;
#18842 = EDGE_CURVE('',#14693,#14692,#7888,.T.) ;
#18843 = EDGE_CURVE('',#14694,#14693,#7889,.T.) ;
#18844 = EDGE_CURVE('',#14695,#14694,#7890,.T.) ;
#18845 = EDGE_CURVE('',#14695,#14696,#7891,.T.) ;
#18846 = EDGE_CURVE('',#14697,#14696,#7892,.T.) ;
#18847 = EDGE_CURVE('',#14698,#14697,#7893,.T.) ;
#18848 = EDGE_CURVE('',#14699,#14698,#7894,.T.) ;
#18849 = EDGE_CURVE('',#14699,#14700,#7895,.T.) ;
#18850 = EDGE_CURVE('',#14701,#14700,#7896,.T.) ;
#18851 = EDGE_CURVE('',#14702,#14701,#7897,.T.) ;
#18852 = EDGE_CURVE('',#14703,#14702,#7898,.T.) ;
#18853 = EDGE_CURVE('',#14703,#14704,#7899,.T.) ;
#18854 = EDGE_CURVE('',#14705,#14704,#7900,.T.) ;
#18855 = EDGE_CURVE('',#14706,#14705,#7901,.T.) ;
#18856 = EDGE_CURVE('',#14707,#14706,#7902,.T.) ;
#18857 = EDGE_CURVE('',#14707,#14708,#7903,.T.) ;
#18858 = EDGE_CURVE('',#14709,#14708,#7904,.T.) ;
#18859 = EDGE_CURVE('',#14709,#14710,#7905,.T.) ;
#18860 = EDGE_CURVE('',#14711,#14710,#7906,.T.) ;
#18861 = EDGE_CURVE('',#14712,#14711,#7907,.T.) ;
#18862 = EDGE_CURVE('',#14713,#14712,#7908,.T.) ;
#18863 = EDGE_CURVE('',#14714,#14713,#7909,.T.) ;
#18864 = EDGE_CURVE('',#14675,#14714,#7910,.T.) ;
#18865 = EDGE_CURVE('',#14676,#14715,#130,.T.) ;
#18866 = EDGE_CURVE('',#14715,#14716,#7911,.T.) ;
#18867 = EDGE_CURVE('',#14716,#14677,#131,.T.) ;
#18868 = EDGE_CURVE('',#14494,#14675,#7912,.T.) ;
#18869 = EDGE_CURVE('',#14717,#14493,#7913,.F.) ;
#18870 = EDGE_CURVE('',#14715,#14717,#7914,.T.) ;
#18871 = EDGE_CURVE('',#14718,#14719,#7915,.T.) ;
#18872 = EDGE_CURVE('',#14719,#14681,#132,.T.) ;
#18873 = EDGE_CURVE('',#14680,#14718,#133,.T.) ;
#18874 = EDGE_CURVE('',#14684,#14720,#134,.T.) ;
#18875 = EDGE_CURVE('',#14720,#14721,#7916,.T.) ;
#18876 = EDGE_CURVE('',#14721,#14685,#135,.T.) ;
#18877 = EDGE_CURVE('',#14688,#14722,#136,.T.) ;
#18878 = EDGE_CURVE('',#14722,#14723,#7917,.T.) ;
#18879 = EDGE_CURVE('',#14723,#14689,#137,.T.) ;
#18880 = EDGE_CURVE('',#14724,#14725,#7918,.T.) ;
#18881 = EDGE_CURVE('',#14725,#14693,#138,.T.) ;
#18882 = EDGE_CURVE('',#14692,#14724,#139,.T.) ;
#18883 = EDGE_CURVE('',#14726,#14727,#7919,.T.) ;
#18884 = EDGE_CURVE('',#14727,#14697,#140,.T.) ;
#18885 = EDGE_CURVE('',#14696,#14726,#141,.T.) ;
#18886 = EDGE_CURVE('',#14728,#14729,#7920,.T.) ;
#18887 = EDGE_CURVE('',#14729,#14701,#142,.T.) ;
#18888 = EDGE_CURVE('',#14700,#14728,#143,.T.) ;
#18889 = EDGE_CURVE('',#14704,#14730,#144,.T.) ;
#18890 = EDGE_CURVE('',#14730,#14731,#7921,.T.) ;
#18891 = EDGE_CURVE('',#14731,#14705,#145,.T.) ;
#18892 = EDGE_CURVE('',#14732,#14733,#7922,.T.) ;
#18893 = EDGE_CURVE('',#14733,#14709,#146,.T.) ;
#18894 = EDGE_CURVE('',#14708,#14732,#147,.T.) ;
#18895 = EDGE_CURVE('',#14734,#14713,#148,.T.) ;
#18896 = EDGE_CURVE('',#14735,#14734,#7923,.T.) ;
#18897 = EDGE_CURVE('',#14496,#14735,#7924,.F.) ;
#18898 = EDGE_CURVE('',#14714,#14495,#7925,.T.) ;
#18899 = EDGE_CURVE('',#14736,#14734,#7926,.T.) ;
#18900 = EDGE_CURVE('',#14712,#14736,#149,.T.) ;
#18901 = EDGE_CURVE('',#14735,#14717,#7927,.T.) ;
#18902 = EDGE_CURVE('',#14737,#14738,#7928,.F.) ;
#18903 = EDGE_CURVE('',#14738,#14739,#7929,.T.) ;
#18904 = EDGE_CURVE('',#14739,#14740,#7930,.F.) ;
#18905 = EDGE_CURVE('',#14740,#14737,#7931,.T.) ;
#18906 = EDGE_CURVE('',#14741,#14742,#7932,.F.) ;
#18907 = EDGE_CURVE('',#14742,#14743,#7933,.T.) ;
#18908 = EDGE_CURVE('',#14743,#14744,#7934,.F.) ;
#18909 = EDGE_CURVE('',#14744,#14741,#7935,.T.) ;
#18910 = EDGE_CURVE('',#14745,#14746,#7936,.F.) ;
#18911 = EDGE_CURVE('',#14746,#14747,#7937,.T.) ;
#18912 = EDGE_CURVE('',#14747,#14748,#7938,.F.) ;
#18913 = EDGE_CURVE('',#14748,#14745,#7939,.T.) ;
#18914 = EDGE_CURVE('',#14749,#14750,#7940,.F.) ;
#18915 = EDGE_CURVE('',#14750,#14751,#7941,.T.) ;
#18916 = EDGE_CURVE('',#14751,#14752,#7942,.F.) ;
#18917 = EDGE_CURVE('',#14752,#14749,#7943,.T.) ;
#18918 = EDGE_CURVE('',#14753,#14754,#7944,.F.) ;
#18919 = EDGE_CURVE('',#14754,#14755,#7945,.T.) ;
#18920 = EDGE_CURVE('',#14755,#14756,#7946,.F.) ;
#18921 = EDGE_CURVE('',#14756,#14753,#7947,.T.) ;
#18922 = EDGE_CURVE('',#14757,#14758,#7948,.F.) ;
#18923 = EDGE_CURVE('',#14758,#14759,#7949,.T.) ;
#18924 = EDGE_CURVE('',#14759,#14760,#7950,.F.) ;
#18925 = EDGE_CURVE('',#14760,#14757,#7951,.T.) ;
#18926 = EDGE_CURVE('',#14761,#14762,#7952,.F.) ;
#18927 = EDGE_CURVE('',#14762,#14763,#7953,.T.) ;
#18928 = EDGE_CURVE('',#14763,#14764,#7954,.F.) ;
#18929 = EDGE_CURVE('',#14764,#14761,#7955,.T.) ;
#18930 = EDGE_CURVE('',#14765,#14766,#7956,.F.) ;
#18931 = EDGE_CURVE('',#14766,#14767,#7957,.T.) ;
#18932 = EDGE_CURVE('',#14767,#14768,#7958,.F.) ;
#18933 = EDGE_CURVE('',#14768,#14765,#7959,.T.) ;
#18934 = EDGE_CURVE('',#14736,#13804,#7960,.T.) ;
#18935 = EDGE_CURVE('',#13805,#14711,#7961,.T.) ;
#18936 = EDGE_CURVE('',#14738,#14716,#7962,.T.) ;
#18937 = EDGE_CURVE('',#14769,#14737,#7963,.T.) ;
#18938 = EDGE_CURVE('',#14678,#14769,#7964,.T.) ;
#18939 = EDGE_CURVE('',#14770,#14679,#7965,.T.) ;
#18940 = EDGE_CURVE('',#14740,#14770,#7966,.T.) ;
#18941 = EDGE_CURVE('',#14718,#14739,#7967,.T.) ;
#18942 = EDGE_CURVE('',#14742,#14719,#7968,.T.) ;
#18943 = EDGE_CURVE('',#14771,#14741,#7969,.T.) ;
#18944 = EDGE_CURVE('',#14682,#14771,#7970,.T.) ;
#18945 = EDGE_CURVE('',#14772,#14683,#7971,.T.) ;
#18946 = EDGE_CURVE('',#14744,#14772,#7972,.T.) ;
#18947 = EDGE_CURVE('',#14720,#14743,#7973,.T.) ;
#18948 = EDGE_CURVE('',#14746,#14721,#7974,.T.) ;
#18949 = EDGE_CURVE('',#14773,#14745,#7975,.T.) ;
#18950 = EDGE_CURVE('',#14686,#14773,#7976,.T.) ;
#18951 = EDGE_CURVE('',#14774,#14687,#7977,.T.) ;
#18952 = EDGE_CURVE('',#14748,#14774,#7978,.T.) ;
#18953 = EDGE_CURVE('',#14722,#14747,#7979,.T.) ;
#18954 = EDGE_CURVE('',#14750,#14723,#7980,.T.) ;
#18955 = EDGE_CURVE('',#14775,#14749,#7981,.T.) ;
#18956 = EDGE_CURVE('',#14690,#14775,#7982,.T.) ;
#18957 = EDGE_CURVE('',#14776,#14691,#7983,.T.) ;
#18958 = EDGE_CURVE('',#14752,#14776,#7984,.T.) ;
#18959 = EDGE_CURVE('',#14724,#14751,#7985,.T.) ;
#18960 = EDGE_CURVE('',#14754,#14725,#7986,.T.) ;
#18961 = EDGE_CURVE('',#14777,#14753,#7987,.T.) ;
#18962 = EDGE_CURVE('',#14694,#14777,#7988,.T.) ;
#18963 = EDGE_CURVE('',#14778,#14695,#7989,.T.) ;
#18964 = EDGE_CURVE('',#14756,#14778,#7990,.T.) ;
#18965 = EDGE_CURVE('',#14726,#14755,#7991,.T.) ;
#18966 = EDGE_CURVE('',#14758,#14727,#7992,.T.) ;
#18967 = EDGE_CURVE('',#14779,#14757,#7993,.T.) ;
#18968 = EDGE_CURVE('',#14698,#14779,#7994,.T.) ;
#18969 = EDGE_CURVE('',#14780,#14699,#7995,.T.) ;
#18970 = EDGE_CURVE('',#14760,#14780,#7996,.T.) ;
#18971 = EDGE_CURVE('',#14728,#14759,#7997,.T.) ;
#18972 = EDGE_CURVE('',#14762,#14729,#7998,.T.) ;
#18973 = EDGE_CURVE('',#14781,#14761,#7999,.T.) ;
#18974 = EDGE_CURVE('',#14702,#14781,#8000,.T.) ;
#18975 = EDGE_CURVE('',#14782,#14703,#8001,.T.) ;
#18976 = EDGE_CURVE('',#14764,#14782,#8002,.T.) ;
#18977 = EDGE_CURVE('',#14730,#14763,#8003,.T.) ;
#18978 = EDGE_CURVE('',#14766,#14731,#8004,.T.) ;
#18979 = EDGE_CURVE('',#14783,#14765,#8005,.T.) ;
#18980 = EDGE_CURVE('',#14706,#14783,#8006,.T.) ;
#18981 = EDGE_CURVE('',#14784,#14707,#8007,.T.) ;
#18982 = EDGE_CURVE('',#14768,#14784,#8008,.T.) ;
#18983 = EDGE_CURVE('',#14732,#14767,#8009,.T.) ;
#18984 = EDGE_CURVE('',#14710,#13766,#8010,.T.) ;
#18985 = EDGE_CURVE('',#14769,#14770,#8011,.T.) ;
#18986 = EDGE_CURVE('',#14771,#14772,#8012,.T.) ;
#18987 = EDGE_CURVE('',#14773,#14774,#8013,.T.) ;
#18988 = EDGE_CURVE('',#14775,#14776,#8014,.T.) ;
#18989 = EDGE_CURVE('',#14777,#14778,#8015,.T.) ;
#18990 = EDGE_CURVE('',#14779,#14780,#8016,.T.) ;
#18991 = EDGE_CURVE('',#14781,#14782,#8017,.T.) ;
#18992 = EDGE_CURVE('',#14783,#14784,#8018,.T.) ;
#18993 = EDGE_CURVE('',#14785,#14785,#12142,.T.) ;
#18994 = EDGE_CURVE('',#14786,#14787,#12143,.T.) ;
#18995 = EDGE_CURVE('',#14787,#14786,#12144,.T.) ;
#18996 = EDGE_CURVE('',#14787,#14785,#12145,.T.) ;
#18997 = EDGE_CURVE('',#14788,#14788,#12146,.T.) ;
#18998 = EDGE_CURVE('',#14788,#14786,#8019,.T.) ;
#18999 = EDGE_CURVE('',#14788,#13941,#12147,.T.) ;
#19000 = EDGE_CURVE('',#14658,#14298,#8020,.T.) ;
#19001 = EDGE_CURVE('',#14789,#14789,#12148,.T.) ;
#19002 = EDGE_CURVE('',#14790,#14791,#12149,.T.) ;
#19003 = EDGE_CURVE('',#14791,#14790,#12150,.T.) ;
#19004 = EDGE_CURVE('',#14791,#14789,#12151,.T.) ;
#19005 = EDGE_CURVE('',#14792,#14792,#12152,.T.) ;
#19006 = EDGE_CURVE('',#14792,#14790,#8021,.T.) ;
#19007 = EDGE_CURVE('',#14792,#13942,#12153,.T.) ;
#19008 = EDGE_CURVE('',#14641,#14321,#8022,.T.) ;
#19009 = EDGE_CURVE('',#14793,#14793,#12154,.T.) ;
#19010 = EDGE_CURVE('',#14794,#14795,#12155,.T.) ;
#19011 = EDGE_CURVE('',#14795,#14794,#12156,.T.) ;
#19012 = EDGE_CURVE('',#14795,#14793,#12157,.T.) ;
#19013 = EDGE_CURVE('',#14796,#14796,#12158,.T.) ;
#19014 = EDGE_CURVE('',#14796,#14794,#8023,.T.) ;
#19015 = EDGE_CURVE('',#14796,#13943,#12159,.T.) ;
#19016 = EDGE_CURVE('',#14624,#14344,#8024,.T.) ;
#19017 = EDGE_CURVE('',#14797,#14797,#12160,.T.) ;
#19018 = EDGE_CURVE('',#14798,#14799,#12161,.T.) ;
#19019 = EDGE_CURVE('',#14799,#14798,#12162,.T.) ;
#19020 = EDGE_CURVE('',#14799,#14797,#12163,.T.) ;
#19021 = EDGE_CURVE('',#14800,#14800,#12164,.T.) ;
#19022 = EDGE_CURVE('',#14800,#14798,#8025,.T.) ;
#19023 = EDGE_CURVE('',#14800,#13944,#12165,.T.) ;
#19024 = EDGE_CURVE('',#14607,#14367,#8026,.T.) ;
#19025 = EDGE_CURVE('',#14801,#14801,#12166,.T.) ;
#19026 = EDGE_CURVE('',#14802,#14803,#12167,.T.) ;
#19027 = EDGE_CURVE('',#14803,#14802,#12168,.T.) ;
#19028 = EDGE_CURVE('',#14803,#14801,#12169,.T.) ;
#19029 = EDGE_CURVE('',#14804,#14804,#12170,.T.) ;
#19030 = EDGE_CURVE('',#14804,#14802,#8027,.T.) ;
#19031 = EDGE_CURVE('',#14804,#13945,#12171,.T.) ;
#19032 = EDGE_CURVE('',#14590,#14390,#8028,.T.) ;
#19033 = EDGE_CURVE('',#14805,#14805,#12172,.T.) ;
#19034 = EDGE_CURVE('',#14806,#14807,#12173,.T.) ;
#19035 = EDGE_CURVE('',#14807,#14806,#12174,.T.) ;
#19036 = EDGE_CURVE('',#14807,#14805,#12175,.T.) ;
#19037 = EDGE_CURVE('',#14808,#14808,#12176,.T.) ;
#19038 = EDGE_CURVE('',#14808,#14806,#8029,.T.) ;
#19039 = EDGE_CURVE('',#14808,#13946,#12177,.T.) ;
#19040 = EDGE_CURVE('',#14573,#14413,#8030,.T.) ;
#19041 = EDGE_CURVE('',#14809,#14809,#12178,.T.) ;
#19042 = EDGE_CURVE('',#14810,#14811,#12179,.T.) ;
#19043 = EDGE_CURVE('',#14811,#14810,#12180,.T.) ;
#19044 = EDGE_CURVE('',#14811,#14809,#12181,.T.) ;
#19045 = EDGE_CURVE('',#14812,#14812,#12182,.T.) ;
#19046 = EDGE_CURVE('',#14812,#14810,#8031,.T.) ;
#19047 = EDGE_CURVE('',#14812,#13947,#12183,.T.) ;
#19048 = EDGE_CURVE('',#14556,#14436,#8032,.T.) ;
#19049 = EDGE_CURVE('',#14813,#14813,#12184,.T.) ;
#19050 = EDGE_CURVE('',#14814,#14815,#12185,.T.) ;
#19051 = EDGE_CURVE('',#14815,#14814,#12186,.T.) ;
#19052 = EDGE_CURVE('',#14815,#14813,#12187,.T.) ;
#19053 = EDGE_CURVE('',#14816,#14816,#12188,.T.) ;
#19054 = EDGE_CURVE('',#14816,#14814,#8033,.T.) ;
#19055 = EDGE_CURVE('',#14816,#13948,#12189,.T.) ;
#19056 = EDGE_CURVE('',#14539,#14459,#8034,.T.) ;
#19057 = EDGE_CURVE('',#14817,#14818,#12190,.T.) ;
#19058 = EDGE_CURVE('',#14818,#14817,#12191,.T.) ;
#19059 = EDGE_CURVE('',#14818,#14505,#12192,.T.) ;
#19060 = EDGE_CURVE('',#14819,#14819,#12193,.T.) ;
#19061 = EDGE_CURVE('',#14819,#14817,#8035,.T.) ;
#19062 = EDGE_CURVE('',#14819,#14525,#12194,.T.) ;
#19063 = EDGE_CURVE('',#13767,#14733,#8036,.T.) ;
#19064 = EDGE_CURVE('',#14674,#14134,#8037,.T.) ;
#19065 = EDGE_CURVE('',#14132,#14673,#8038,.T.) ;
#19066 = EDGE_CURVE('',#14672,#14130,#8039,.T.) ;
#19067 = EDGE_CURVE('',#14657,#14155,#8040,.T.) ;
#19068 = EDGE_CURVE('',#14153,#14656,#8041,.T.) ;
#19069 = EDGE_CURVE('',#14655,#14151,#8042,.T.) ;
#19070 = EDGE_CURVE('',#14640,#14176,#8043,.T.) ;
#19071 = EDGE_CURVE('',#14174,#14639,#8044,.T.) ;
#19072 = EDGE_CURVE('',#14638,#14172,#8045,.T.) ;
#19073 = EDGE_CURVE('',#14623,#14197,#8046,.T.) ;
#19074 = EDGE_CURVE('',#14195,#14622,#8047,.T.) ;
#19075 = EDGE_CURVE('',#14621,#14193,#8048,.T.) ;
#19076 = EDGE_CURVE('',#14606,#14218,#8049,.T.) ;
#19077 = EDGE_CURVE('',#14216,#14605,#8050,.T.) ;
#19078 = EDGE_CURVE('',#14604,#14214,#8051,.T.) ;
#19079 = EDGE_CURVE('',#14589,#14239,#8052,.T.) ;
#19080 = EDGE_CURVE('',#14237,#14588,#8053,.T.) ;
#19081 = EDGE_CURVE('',#14587,#14235,#8054,.T.) ;
#19082 = EDGE_CURVE('',#14572,#14260,#8055,.T.) ;
#19083 = EDGE_CURVE('',#14258,#14571,#8056,.T.) ;
#19084 = EDGE_CURVE('',#14570,#14256,#8057,.T.) ;
#19085 = EDGE_CURVE('',#14555,#14281,#8058,.T.) ;
#19086 = EDGE_CURVE('',#14279,#14554,#8059,.T.) ;
#19087 = EDGE_CURVE('',#14553,#14277,#8060,.T.) ;
#19088 = EDGE_CURVE('',#14820,#14821,#8061,.T.) ;
#19089 = EDGE_CURVE('',#14820,#14822,#1465,.T.) ;
#19090 = EDGE_CURVE('',#14822,#14823,#1466,.T.) ;
#19091 = EDGE_CURVE('',#14821,#14823,#804,.T.) ;
#19092 = EDGE_CURVE('',#14824,#14825,#8062,.T.) ;
#19093 = EDGE_CURVE('',#14824,#14820,#1467,.T.) ;
#19094 = EDGE_CURVE('',#14825,#14821,#1468,.F.) ;
#19095 = EDGE_CURVE('',#14826,#14827,#8063,.T.) ;
#19096 = EDGE_CURVE('',#14826,#14824,#1469,.T.) ;
#19097 = EDGE_CURVE('',#14827,#14825,#1470,.F.) ;
#19098 = EDGE_CURVE('',#14828,#14829,#8064,.T.) ;
#19099 = EDGE_CURVE('',#14828,#14826,#1471,.T.) ;
#19100 = EDGE_CURVE('',#14829,#14827,#1472,.F.) ;
#19101 = EDGE_CURVE('',#14830,#14831,#8065,.T.) ;
#19102 = EDGE_CURVE('',#14830,#14828,#1473,.T.) ;
#19103 = EDGE_CURVE('',#14831,#14829,#1474,.F.) ;
#19104 = EDGE_CURVE('',#14832,#14833,#8066,.T.) ;
#19105 = EDGE_CURVE('',#14832,#14830,#1475,.T.) ;
#19106 = EDGE_CURVE('',#14833,#14831,#1476,.F.) ;
#19107 = EDGE_CURVE('',#14834,#14835,#8067,.T.) ;
#19108 = EDGE_CURVE('',#14834,#14832,#1477,.T.) ;
#19109 = EDGE_CURVE('',#14835,#14833,#1478,.F.) ;
#19110 = EDGE_CURVE('',#14836,#14837,#8068,.T.) ;
#19111 = EDGE_CURVE('',#14838,#14836,#12195,.T.) ;
#19112 = EDGE_CURVE('',#14838,#14834,#1479,.T.) ;
#19113 = EDGE_CURVE('',#14837,#14835,#1480,.F.) ;
#19114 = EDGE_CURVE('',#14839,#14840,#8069,.T.) ;
#19115 = EDGE_CURVE('',#14841,#14839,#1481,.F.) ;
#19116 = EDGE_CURVE('',#14841,#14842,#12196,.T.) ;
#19117 = EDGE_CURVE('',#14842,#14840,#1482,.T.) ;
#19118 = EDGE_CURVE('',#14843,#14844,#8070,.T.) ;
#19119 = EDGE_CURVE('',#14839,#14843,#1483,.F.) ;
#19120 = EDGE_CURVE('',#14840,#14844,#1484,.T.) ;
#19121 = EDGE_CURVE('',#14845,#14846,#8071,.T.) ;
#19122 = EDGE_CURVE('',#14843,#14845,#1485,.F.) ;
#19123 = EDGE_CURVE('',#14844,#14846,#1486,.T.) ;
#19124 = EDGE_CURVE('',#14847,#14848,#8072,.T.) ;
#19125 = EDGE_CURVE('',#14845,#14847,#1487,.F.) ;
#19126 = EDGE_CURVE('',#14846,#14848,#1488,.T.) ;
#19127 = EDGE_CURVE('',#14849,#14850,#8073,.T.) ;
#19128 = EDGE_CURVE('',#14847,#14849,#1489,.F.) ;
#19129 = EDGE_CURVE('',#14848,#14850,#1490,.T.) ;
#19130 = EDGE_CURVE('',#14851,#14852,#8074,.T.) ;
#19131 = EDGE_CURVE('',#14849,#14851,#1491,.F.) ;
#19132 = EDGE_CURVE('',#14850,#14852,#1492,.T.) ;
#19133 = EDGE_CURVE('',#14853,#14854,#8075,.T.) ;
#19134 = EDGE_CURVE('',#14851,#14853,#1493,.F.) ;
#19135 = EDGE_CURVE('',#14852,#14854,#1494,.T.) ;
#19136 = EDGE_CURVE('',#14854,#14855,#1495,.T.) ;
#19137 = EDGE_CURVE('',#14856,#14855,#12197,.T.) ;
#19138 = EDGE_CURVE('',#14857,#14856,#1496,.T.) ;
#19139 = EDGE_CURVE('',#14853,#14857,#1497,.F.) ;
#19140 = EDGE_CURVE('',#14858,#14837,#1498,.F.) ;
#19141 = EDGE_CURVE('',#14836,#14858,#12198,.T.) ;
#19142 = EDGE_CURVE('',#14859,#14860,#12199,.T.) ;
#19143 = EDGE_CURVE('',#14860,#14861,#1499,.T.) ;
#19144 = EDGE_CURVE('',#14861,#14859,#1500,.T.) ;
#19145 = EDGE_CURVE('',#14859,#14862,#1501,.T.) ;
#19146 = EDGE_CURVE('',#14862,#14863,#12200,.T.) ;
#19147 = EDGE_CURVE('',#14863,#14860,#1502,.T.) ;
#19148 = EDGE_CURVE('',#14864,#14865,#12201,.T.) ;
#19149 = EDGE_CURVE('',#14865,#14863,#1503,.T.) ;
#19150 = EDGE_CURVE('',#14862,#14864,#1504,.T.) ;
#19151 = EDGE_CURVE('',#14866,#14867,#12202,.T.) ;
#19152 = EDGE_CURVE('',#14867,#14865,#150,.T.) ;
#19153 = EDGE_CURVE('',#14864,#14866,#151,.T.) ;
#19154 = EDGE_CURVE('',#14868,#14869,#12203,.T.) ;
#19155 = EDGE_CURVE('',#14869,#14870,#8076,.T.) ;
#19156 = EDGE_CURVE('',#14870,#14868,#1505,.T.) ;
#19157 = EDGE_CURVE('',#14871,#14872,#12204,.T.) ;
#19158 = EDGE_CURVE('',#14872,#14869,#8077,.T.) ;
#19159 = EDGE_CURVE('',#14868,#14871,#1506,.T.) ;
#19160 = EDGE_CURVE('',#14871,#14867,#1507,.T.) ;
#19161 = EDGE_CURVE('',#14866,#14872,#8078,.T.) ;
#19162 = EDGE_CURVE('',#14873,#14863,#12205,.T.) ;
#19163 = EDGE_CURVE('',#14873,#14860,#152,.T.) ;
#19164 = EDGE_CURVE('',#14874,#14875,#12206,.T.) ;
#19165 = EDGE_CURVE('',#14876,#14874,#1508,.T.) ;
#19166 = EDGE_CURVE('',#14877,#14876,#153,.T.) ;
#19167 = EDGE_CURVE('',#14878,#14877,#12207,.T.) ;
#19168 = EDGE_CURVE('',#14879,#14878,#154,.T.) ;
#19169 = EDGE_CURVE('',#14880,#14879,#1509,.T.) ;
#19170 = EDGE_CURVE('',#14861,#14880,#12208,.T.) ;
#19171 = EDGE_CURVE('',#14881,#14873,#12209,.T.) ;
#19172 = EDGE_CURVE('',#14882,#14881,#155,.T.) ;
#19173 = EDGE_CURVE('',#14883,#14882,#1510,.T.) ;
#19174 = EDGE_CURVE('',#14875,#14883,#12210,.T.) ;
#19175 = EDGE_CURVE('',#14875,#14884,#12211,.T.) ;
#19176 = EDGE_CURVE('',#14884,#14884,#12212,.T.) ;
#19177 = EDGE_CURVE('',#14867,#14885,#12213,.T.) ;
#19178 = EDGE_CURVE('',#14886,#14885,#156,.T.) ;
#19179 = EDGE_CURVE('',#14887,#14886,#1511,.T.) ;
#19180 = EDGE_CURVE('',#14881,#14887,#12214,.T.) ;
#19181 = EDGE_CURVE('',#14882,#14888,#12215,.T.) ;
#19182 = EDGE_CURVE('',#14888,#14883,#1512,.T.) ;
#19183 = EDGE_CURVE('',#14887,#14889,#12216,.T.) ;
#19184 = EDGE_CURVE('',#14889,#14888,#1513,.T.) ;
#19185 = EDGE_CURVE('',#14882,#14887,#1514,.T.) ;
#19186 = EDGE_CURVE('',#14886,#14890,#12217,.T.) ;
#19187 = EDGE_CURVE('',#14890,#14889,#1515,.T.) ;
#19188 = EDGE_CURVE('',#14885,#14891,#12218,.T.) ;
#19189 = EDGE_CURVE('',#14891,#14890,#157,.T.) ;
#19190 = EDGE_CURVE('',#14892,#14893,#1516,.T.) ;
#19191 = EDGE_CURVE('',#14893,#14894,#8079,.T.) ;
#19192 = EDGE_CURVE('',#14894,#14892,#12219,.T.) ;
#19193 = EDGE_CURVE('',#14894,#14895,#8080,.T.) ;
#19194 = EDGE_CURVE('',#14895,#14896,#12220,.T.) ;
#19195 = EDGE_CURVE('',#14896,#14892,#1517,.T.) ;
#19196 = EDGE_CURVE('',#14895,#14891,#8081,.T.) ;
#19197 = EDGE_CURVE('',#14885,#14896,#1518,.T.) ;
#19198 = EDGE_CURVE('',#14890,#14897,#8082,.T.) ;
#19199 = EDGE_CURVE('',#14897,#14898,#12221,.T.) ;
#19200 = EDGE_CURVE('',#14898,#14883,#8083,.T.) ;
#19201 = EDGE_CURVE('',#14899,#14893,#8084,.T.) ;
#19202 = EDGE_CURVE('',#14900,#14899,#8085,.T.) ;
#19203 = EDGE_CURVE('',#14901,#14900,#12222,.T.) ;
#19204 = EDGE_CURVE('',#14897,#14901,#1519,.T.) ;
#19205 = EDGE_CURVE('',#14902,#14876,#12223,.T.) ;
#19206 = EDGE_CURVE('',#14874,#14902,#1520,.T.) ;
#19207 = EDGE_CURVE('',#14902,#14903,#1521,.T.) ;
#19208 = EDGE_CURVE('',#14903,#14904,#12224,.T.) ;
#19209 = EDGE_CURVE('',#14904,#14876,#1522,.T.) ;
#19210 = EDGE_CURVE('',#14905,#14906,#12225,.T.) ;
#19211 = EDGE_CURVE('',#14906,#14904,#1523,.T.) ;
#19212 = EDGE_CURVE('',#14903,#14905,#1524,.T.) ;
#19213 = EDGE_CURVE('',#14907,#14908,#12226,.T.) ;
#19214 = EDGE_CURVE('',#14908,#14906,#158,.T.) ;
#19215 = EDGE_CURVE('',#14905,#14907,#159,.T.) ;
#19216 = EDGE_CURVE('',#14909,#14910,#12227,.T.) ;
#19217 = EDGE_CURVE('',#14910,#14911,#8086,.T.) ;
#19218 = EDGE_CURVE('',#14911,#14909,#1525,.T.) ;
#19219 = EDGE_CURVE('',#14912,#14913,#12228,.T.) ;
#19220 = EDGE_CURVE('',#14913,#14910,#8087,.T.) ;
#19221 = EDGE_CURVE('',#14909,#14912,#1526,.T.) ;
#19222 = EDGE_CURVE('',#14912,#14908,#1527,.T.) ;
#19223 = EDGE_CURVE('',#14907,#14913,#8088,.T.) ;
#19224 = EDGE_CURVE('',#14877,#14904,#12229,.T.) ;
#19225 = EDGE_CURVE('',#14908,#14914,#12230,.T.) ;
#19226 = EDGE_CURVE('',#14915,#14914,#160,.T.) ;
#19227 = EDGE_CURVE('',#14916,#14915,#1528,.T.) ;
#19228 = EDGE_CURVE('',#14878,#14916,#12231,.T.) ;
#19229 = EDGE_CURVE('',#14879,#14917,#12232,.T.) ;
#19230 = EDGE_CURVE('',#14917,#14880,#1529,.T.) ;
#19231 = EDGE_CURVE('',#14916,#14918,#12233,.T.) ;
#19232 = EDGE_CURVE('',#14918,#14917,#1530,.T.) ;
#19233 = EDGE_CURVE('',#14879,#14916,#1531,.T.) ;
#19234 = EDGE_CURVE('',#14915,#14919,#12234,.T.) ;
#19235 = EDGE_CURVE('',#14919,#14918,#1532,.T.) ;
#19236 = EDGE_CURVE('',#14914,#14920,#12235,.T.) ;
#19237 = EDGE_CURVE('',#14920,#14919,#161,.T.) ;
#19238 = EDGE_CURVE('',#14921,#14922,#1533,.T.) ;
#19239 = EDGE_CURVE('',#14922,#14923,#8089,.T.) ;
#19240 = EDGE_CURVE('',#14923,#14921,#12236,.T.) ;
#19241 = EDGE_CURVE('',#14923,#14924,#8090,.T.) ;
#19242 = EDGE_CURVE('',#14924,#14925,#12237,.T.) ;
#19243 = EDGE_CURVE('',#14925,#14921,#1534,.T.) ;
#19244 = EDGE_CURVE('',#14924,#14920,#8091,.T.) ;
#19245 = EDGE_CURVE('',#14914,#14925,#1535,.T.) ;
#19246 = EDGE_CURVE('',#14919,#14926,#8092,.T.) ;
#19247 = EDGE_CURVE('',#14927,#14926,#12238,.T.) ;
#19248 = EDGE_CURVE('',#14927,#14880,#8093,.T.) ;
#19249 = EDGE_CURVE('',#14928,#14922,#8094,.T.) ;
#19250 = EDGE_CURVE('',#14929,#14928,#8095,.T.) ;
#19251 = EDGE_CURVE('',#14930,#14929,#12239,.T.) ;
#19252 = EDGE_CURVE('',#14926,#14930,#162,.T.) ;
#19253 = EDGE_CURVE('',#14931,#14932,#12240,.T.) ;
#19254 = EDGE_CURVE('',#14932,#14933,#163,.T.) ;
#19255 = EDGE_CURVE('',#14933,#14931,#164,.T.) ;
#19256 = EDGE_CURVE('',#14931,#14934,#8096,.T.) ;
#19257 = EDGE_CURVE('',#14934,#14935,#12241,.T.) ;
#19258 = EDGE_CURVE('',#14935,#14932,#8097,.T.) ;
#19259 = EDGE_CURVE('',#14934,#14936,#12242,.T.) ;
#19260 = EDGE_CURVE('',#14936,#14935,#12243,.T.) ;
#19261 = EDGE_CURVE('',#14934,#14937,#12244,.T.) ;
#19262 = EDGE_CURVE('',#14938,#14937,#1536,.T.) ;
#19263 = EDGE_CURVE('',#14938,#14936,#12245,.T.) ;
#19264 = EDGE_CURVE('',#14939,#14931,#8098,.T.) ;
#19265 = EDGE_CURVE('',#14940,#14939,#1537,.T.) ;
#19266 = EDGE_CURVE('',#14937,#14940,#165,.T.) ;
#19267 = EDGE_CURVE('',#14933,#14941,#8099,.T.) ;
#19268 = EDGE_CURVE('',#14939,#14941,#12246,.T.) ;
#19269 = EDGE_CURVE('',#14942,#14938,#1538,.T.) ;
#19270 = EDGE_CURVE('',#14937,#14942,#12247,.T.) ;
#19271 = EDGE_CURVE('',#14940,#14943,#12248,.T.) ;
#19272 = EDGE_CURVE('',#14943,#14942,#166,.T.) ;
#19273 = EDGE_CURVE('',#14939,#14944,#12249,.T.) ;
#19274 = EDGE_CURVE('',#14944,#14943,#1539,.T.) ;
#19275 = EDGE_CURVE('',#14941,#14944,#12250,.T.) ;
#19276 = EDGE_CURVE('',#14945,#14946,#12251,.T.) ;
#19277 = EDGE_CURVE('',#14946,#14947,#12252,.T.) ;
#19278 = EDGE_CURVE('',#14947,#14945,#12253,.T.) ;
#19279 = EDGE_CURVE('',#14948,#14949,#12254,.T.) ;
#19280 = EDGE_CURVE('',#14949,#14946,#1540,.T.) ;
#19281 = EDGE_CURVE('',#14945,#14948,#1541,.T.) ;
#19282 = EDGE_CURVE('',#14950,#14951,#12255,.T.) ;
#19283 = EDGE_CURVE('',#14951,#14949,#167,.T.) ;
#19284 = EDGE_CURVE('',#14948,#14950,#168,.T.) ;
#19285 = EDGE_CURVE('',#14950,#14952,#1542,.T.) ;
#19286 = EDGE_CURVE('',#14952,#14951,#1543,.T.) ;
#19287 = EDGE_CURVE('',#14950,#14953,#12256,.T.) ;
#19288 = EDGE_CURVE('',#14954,#14953,#12257,.T.) ;
#19289 = EDGE_CURVE('',#14954,#14952,#12258,.T.) ;
#19290 = EDGE_CURVE('',#14955,#14945,#8100,.T.) ;
#19291 = EDGE_CURVE('',#14953,#14955,#8101,.T.) ;
#19292 = EDGE_CURVE('',#14947,#14956,#8102,.T.) ;
#19293 = EDGE_CURVE('',#14955,#14956,#169,.T.) ;
#19294 = EDGE_CURVE('',#14957,#14955,#12259,.T.) ;
#19295 = EDGE_CURVE('',#14956,#14957,#170,.T.) ;
#19296 = EDGE_CURVE('',#14957,#14958,#8103,.T.) ;
#19297 = EDGE_CURVE('',#14958,#14953,#12260,.T.) ;
#19298 = EDGE_CURVE('',#14958,#14954,#12261,.T.) ;
#19299 = EDGE_CURVE('',#14959,#14957,#8104,.T.) ;
#19300 = EDGE_CURVE('',#14960,#14959,#8105,.T.) ;
#19301 = EDGE_CURVE('',#14961,#14960,#171,.T.) ;
#19302 = EDGE_CURVE('',#14962,#14961,#8106,.T.) ;
#19303 = EDGE_CURVE('',#14958,#14962,#12262,.T.) ;
#19304 = EDGE_CURVE('',#14956,#14963,#8107,.T.) ;
#19305 = EDGE_CURVE('',#14959,#14963,#172,.T.) ;
#19306 = EDGE_CURVE('',#14964,#14965,#12263,.T.) ;
#19307 = EDGE_CURVE('',#14965,#14966,#12264,.T.) ;
#19308 = EDGE_CURVE('',#14966,#14964,#12265,.T.) ;
#19309 = EDGE_CURVE('',#14967,#14968,#12266,.T.) ;
#19310 = EDGE_CURVE('',#14968,#14965,#1544,.T.) ;
#19311 = EDGE_CURVE('',#14964,#14967,#1545,.T.) ;
#19312 = EDGE_CURVE('',#14967,#14969,#173,.T.) ;
#19313 = EDGE_CURVE('',#14969,#14970,#12267,.T.) ;
#19314 = EDGE_CURVE('',#14970,#14968,#174,.T.) ;
#19315 = EDGE_CURVE('',#14969,#14971,#1546,.T.) ;
#19316 = EDGE_CURVE('',#14971,#14970,#1547,.T.) ;
#19317 = EDGE_CURVE('',#14967,#14972,#12268,.T.) ;
#19318 = EDGE_CURVE('',#14973,#14972,#175,.T.) ;
#19319 = EDGE_CURVE('',#14974,#14973,#1548,.T.) ;
#19320 = EDGE_CURVE('',#14974,#14971,#12269,.T.) ;
#19321 = EDGE_CURVE('',#14975,#14964,#12270,.T.) ;
#19322 = EDGE_CURVE('',#14972,#14975,#1549,.T.) ;
#19323 = EDGE_CURVE('',#14966,#14976,#12271,.T.) ;
#19324 = EDGE_CURVE('',#14975,#14976,#12272,.T.) ;
#19325 = EDGE_CURVE('',#14965,#14977,#8108,.T.) ;
#19326 = EDGE_CURVE('',#14978,#14977,#176,.T.) ;
#19327 = EDGE_CURVE('',#14978,#14966,#8109,.T.) ;
#19328 = EDGE_CURVE('',#14979,#14975,#12273,.T.) ;
#19329 = EDGE_CURVE('',#14976,#14979,#12274,.T.) ;
#19330 = EDGE_CURVE('',#14980,#14972,#12275,.T.) ;
#19331 = EDGE_CURVE('',#14979,#14980,#1550,.T.) ;
#19332 = EDGE_CURVE('',#14981,#14973,#12276,.T.) ;
#19333 = EDGE_CURVE('',#14980,#14981,#177,.T.) ;
#19334 = EDGE_CURVE('',#14981,#14974,#1551,.T.) ;
#19335 = EDGE_CURVE('',#14981,#14982,#12277,.T.) ;
#19336 = EDGE_CURVE('',#14983,#14982,#12278,.T.) ;
#19337 = EDGE_CURVE('',#14983,#14974,#12279,.T.) ;
#19338 = EDGE_CURVE('',#14984,#14979,#8110,.T.) ;
#19339 = EDGE_CURVE('',#14982,#14984,#8111,.T.) ;
#19340 = EDGE_CURVE('',#14976,#14985,#8112,.T.) ;
#19341 = EDGE_CURVE('',#14984,#14985,#178,.T.) ;
#19342 = EDGE_CURVE('',#14986,#14984,#12280,.T.) ;
#19343 = EDGE_CURVE('',#14985,#14986,#179,.T.) ;
#19344 = EDGE_CURVE('',#14986,#14987,#8113,.T.) ;
#19345 = EDGE_CURVE('',#14987,#14982,#12281,.T.) ;
#19346 = EDGE_CURVE('',#14987,#14983,#12282,.T.) ;
#19347 = EDGE_CURVE('',#14988,#14986,#8114,.T.) ;
#19348 = EDGE_CURVE('',#14989,#14988,#8115,.T.) ;
#19349 = EDGE_CURVE('',#14990,#14989,#180,.T.) ;
#19350 = EDGE_CURVE('',#14991,#14990,#8116,.T.) ;
#19351 = EDGE_CURVE('',#14987,#14991,#12283,.T.) ;
#19352 = EDGE_CURVE('',#14985,#14992,#8117,.T.) ;
#19353 = EDGE_CURVE('',#14988,#14992,#181,.T.) ;
#19354 = EDGE_CURVE('',#14977,#14993,#12284,.T.) ;
#19355 = EDGE_CURVE('',#14993,#14978,#182,.T.) ;
#19356 = EDGE_CURVE('',#14977,#14994,#8118,.T.) ;
#19357 = EDGE_CURVE('',#14994,#14995,#12285,.T.) ;
#19358 = EDGE_CURVE('',#14995,#14993,#8119,.T.) ;
#19359 = EDGE_CURVE('',#14994,#14996,#12286,.T.) ;
#19360 = EDGE_CURVE('',#14996,#14995,#12287,.T.) ;
#19361 = EDGE_CURVE('',#14994,#14970,#12288,.T.) ;
#19362 = EDGE_CURVE('',#14993,#14997,#8120,.T.) ;
#19363 = EDGE_CURVE('',#14998,#14997,#183,.T.) ;
#19364 = EDGE_CURVE('',#14998,#14978,#8121,.T.) ;
#19365 = EDGE_CURVE('',#14999,#15000,#1552,.T.) ;
#19366 = EDGE_CURVE('',#14999,#15001,#1553,.T.) ;
#19367 = EDGE_CURVE('',#15001,#15002,#1554,.T.) ;
#19368 = EDGE_CURVE('',#15002,#15003,#184,.T.) ;
#19369 = EDGE_CURVE('',#15003,#15004,#12289,.T.) ;
#19370 = EDGE_CURVE('',#15004,#15005,#1555,.T.) ;
#19371 = EDGE_CURVE('',#15005,#15006,#1556,.T.) ;
#19372 = EDGE_CURVE('',#15006,#15000,#1557,.T.) ;
#19373 = EDGE_CURVE('',#14855,#15002,#1558,.T.) ;
#19374 = EDGE_CURVE('',#15001,#15007,#12290,.T.) ;
#19375 = EDGE_CURVE('',#15007,#14856,#1559,.T.) ;
#19376 = EDGE_CURVE('',#14823,#15000,#1560,.T.) ;
#19377 = EDGE_CURVE('',#14822,#15008,#1561,.T.) ;
#19378 = EDGE_CURVE('',#15008,#15009,#1562,.T.) ;
#19379 = EDGE_CURVE('',#15009,#15010,#185,.T.) ;
#19380 = EDGE_CURVE('',#15010,#14857,#12291,.T.) ;
#19381 = EDGE_CURVE('',#15007,#14999,#1563,.T.) ;
#19382 = EDGE_CURVE('',#14858,#14842,#1564,.T.) ;
#19383 = EDGE_CURVE('',#15011,#15012,#12292,.T.) ;
#19384 = EDGE_CURVE('',#15012,#15013,#186,.T.) ;
#19385 = EDGE_CURVE('',#15013,#15014,#187,.T.) ;
#19386 = EDGE_CURVE('',#15014,#15015,#188,.T.) ;
#19387 = EDGE_CURVE('',#15015,#15016,#8122,.T.) ;
#19388 = EDGE_CURVE('',#15016,#15017,#8123,.T.) ;
#19389 = EDGE_CURVE('',#15017,#15018,#189,.T.) ;
#19390 = EDGE_CURVE('',#15018,#15019,#190,.T.) ;
#19391 = EDGE_CURVE('',#15019,#15011,#191,.T.) ;
#19392 = EDGE_CURVE('',#15020,#15021,#12293,.T.) ;
#19393 = EDGE_CURVE('',#15021,#15012,#192,.T.) ;
#19394 = EDGE_CURVE('',#15011,#15020,#193,.T.) ;
#19395 = EDGE_CURVE('',#15020,#15022,#8124,.T.) ;
#19396 = EDGE_CURVE('',#15022,#15023,#12294,.T.) ;
#19397 = EDGE_CURVE('',#15023,#15021,#8125,.T.) ;
#19398 = EDGE_CURVE('',#15022,#15024,#12295,.T.) ;
#19399 = EDGE_CURVE('',#15024,#15023,#12296,.T.) ;
#19400 = EDGE_CURVE('',#15025,#15020,#8126,.T.) ;
#19401 = EDGE_CURVE('',#15026,#15025,#8127,.T.) ;
#19402 = EDGE_CURVE('',#15022,#15026,#8128,.T.) ;
#19403 = EDGE_CURVE('',#15016,#15027,#8129,.T.) ;
#19404 = EDGE_CURVE('',#15027,#15025,#12297,.F.) ;
#19405 = EDGE_CURVE('',#15012,#15028,#12298,.T.) ;
#19406 = EDGE_CURVE('',#15029,#15028,#1565,.T.) ;
#19407 = EDGE_CURVE('',#15030,#15029,#1566,.T.) ;
#19408 = EDGE_CURVE('',#15030,#15016,#12299,.T.) ;
#19409 = EDGE_CURVE('',#15031,#15032,#12300,.T.) ;
#19410 = EDGE_CURVE('',#15032,#15033,#12301,.T.) ;
#19411 = EDGE_CURVE('',#15033,#15031,#12302,.T.) ;
#19412 = EDGE_CURVE('',#15034,#15035,#12303,.T.) ;
#19413 = EDGE_CURVE('',#15035,#15032,#8130,.T.) ;
#19414 = EDGE_CURVE('',#15031,#15034,#8131,.T.) ;
#19415 = EDGE_CURVE('',#15034,#15036,#194,.T.) ;
#19416 = EDGE_CURVE('',#15036,#15028,#12304,.T.) ;
#19417 = EDGE_CURVE('',#15028,#15035,#195,.T.) ;
#19418 = EDGE_CURVE('',#15036,#15037,#1567,.T.) ;
#19419 = EDGE_CURVE('',#15037,#15030,#1568,.T.) ;
#19420 = EDGE_CURVE('',#15034,#15038,#8132,.T.) ;
#19421 = EDGE_CURVE('',#15038,#15039,#12305,.F.) ;
#19422 = EDGE_CURVE('',#15039,#15030,#8133,.T.) ;
#19423 = EDGE_CURVE('',#15040,#15031,#8134,.T.) ;
#19424 = EDGE_CURVE('',#15038,#15040,#8135,.T.) ;
#19425 = EDGE_CURVE('',#15033,#15041,#8136,.T.) ;
#19426 = EDGE_CURVE('',#15040,#15041,#196,.T.) ;
#19427 = EDGE_CURVE('',#15042,#15039,#8137,.T.) ;
#19428 = EDGE_CURVE('',#14885,#15042,#8138,.T.) ;
#19429 = EDGE_CURVE('',#15043,#14867,#8139,.T.) ;
#19430 = EDGE_CURVE('',#15027,#15043,#8140,.T.) ;
#19431 = EDGE_CURVE('',#14997,#15044,#12306,.T.) ;
#19432 = EDGE_CURVE('',#15044,#14998,#197,.T.) ;
#19433 = EDGE_CURVE('',#15045,#15046,#12307,.T.) ;
#19434 = EDGE_CURVE('',#15046,#15044,#8141,.T.) ;
#19435 = EDGE_CURVE('',#14997,#15045,#8142,.T.) ;
#19436 = EDGE_CURVE('',#15042,#15045,#12308,.T.) ;
#19437 = EDGE_CURVE('',#15045,#15047,#198,.T.) ;
#19438 = EDGE_CURVE('',#15047,#14899,#12309,.T.) ;
#19439 = EDGE_CURVE('',#14899,#15042,#199,.T.) ;
#19440 = EDGE_CURVE('',#15048,#14900,#12310,.T.) ;
#19441 = EDGE_CURVE('',#15047,#15048,#8143,.T.) ;
#19442 = EDGE_CURVE('',#15048,#15049,#12311,.T.) ;
#19443 = EDGE_CURVE('',#15049,#14900,#12312,.T.) ;
#19444 = EDGE_CURVE('',#15042,#15046,#12313,.T.) ;
#19445 = EDGE_CURVE('',#15044,#15050,#8144,.T.) ;
#19446 = EDGE_CURVE('',#15041,#15050,#200,.T.) ;
#19447 = EDGE_CURVE('',#15041,#14998,#8145,.T.) ;
#19448 = EDGE_CURVE('',#15051,#15046,#8146,.T.) ;
#19449 = EDGE_CURVE('',#15050,#15051,#8147,.T.) ;
#19450 = EDGE_CURVE('',#15051,#15038,#12314,.F.) ;
#19451 = EDGE_CURVE('',#15039,#15051,#12315,.F.) ;
#19452 = EDGE_CURVE('',#15040,#15050,#12316,.T.) ;
#19453 = EDGE_CURVE('',#15052,#14961,#12317,.T.) ;
#19454 = EDGE_CURVE('',#14960,#15043,#12318,.T.) ;
#19455 = EDGE_CURVE('',#15043,#15052,#201,.T.) ;
#19456 = EDGE_CURVE('',#15053,#14962,#12319,.T.) ;
#19457 = EDGE_CURVE('',#15052,#15053,#8148,.T.) ;
#19458 = EDGE_CURVE('',#15053,#15054,#12320,.T.) ;
#19459 = EDGE_CURVE('',#15054,#14962,#12321,.T.) ;
#19460 = EDGE_CURVE('',#15055,#14960,#12322,.T.) ;
#19461 = EDGE_CURVE('',#14959,#15056,#12323,.T.) ;
#19462 = EDGE_CURVE('',#15056,#15055,#8149,.T.) ;
#19463 = EDGE_CURVE('',#14963,#15056,#202,.T.) ;
#19464 = EDGE_CURVE('',#15055,#15043,#12324,.T.) ;
#19465 = EDGE_CURVE('',#15054,#14954,#12325,.T.) ;
#19466 = EDGE_CURVE('',#15053,#15057,#12326,.T.) ;
#19467 = EDGE_CURVE('',#15058,#15057,#12327,.T.) ;
#19468 = EDGE_CURVE('',#15058,#15054,#12328,.T.) ;
#19469 = EDGE_CURVE('',#15059,#14864,#8150,.T.) ;
#19470 = EDGE_CURVE('',#15057,#15059,#203,.T.) ;
#19471 = EDGE_CURVE('',#14870,#15052,#8151,.T.) ;
#19472 = EDGE_CURVE('',#15060,#15056,#8152,.T.) ;
#19473 = EDGE_CURVE('',#15061,#15060,#8153,.T.) ;
#19474 = EDGE_CURVE('',#15055,#15061,#8154,.T.) ;
#19475 = EDGE_CURVE('',#15025,#15061,#12329,.F.) ;
#19476 = EDGE_CURVE('',#15061,#15027,#12330,.F.) ;
#19477 = EDGE_CURVE('',#15060,#15026,#12331,.T.) ;
#19478 = EDGE_CURVE('',#15060,#15062,#204,.T.) ;
#19479 = EDGE_CURVE('',#15062,#15026,#205,.T.) ;
#19480 = EDGE_CURVE('',#15062,#15024,#8155,.T.) ;
#19481 = EDGE_CURVE('',#14963,#15062,#8156,.T.) ;
#19482 = EDGE_CURVE('',#15063,#14908,#8157,.T.) ;
#19483 = EDGE_CURVE('',#14911,#15064,#8158,.T.) ;
#19484 = EDGE_CURVE('',#15063,#15064,#206,.T.) ;
#19485 = EDGE_CURVE('',#15065,#15066,#12332,.T.) ;
#19486 = EDGE_CURVE('',#15066,#15067,#207,.T.) ;
#19487 = EDGE_CURVE('',#15067,#15068,#208,.T.) ;
#19488 = EDGE_CURVE('',#15068,#15069,#209,.T.) ;
#19489 = EDGE_CURVE('',#15069,#15070,#8159,.T.) ;
#19490 = EDGE_CURVE('',#15070,#15071,#8160,.T.) ;
#19491 = EDGE_CURVE('',#15071,#15072,#210,.T.) ;
#19492 = EDGE_CURVE('',#15072,#15073,#211,.T.) ;
#19493 = EDGE_CURVE('',#15073,#15065,#212,.T.) ;
#19494 = EDGE_CURVE('',#15074,#15075,#12333,.T.) ;
#19495 = EDGE_CURVE('',#15075,#15066,#213,.T.) ;
#19496 = EDGE_CURVE('',#15065,#15074,#214,.T.) ;
#19497 = EDGE_CURVE('',#15074,#15076,#8161,.T.) ;
#19498 = EDGE_CURVE('',#15076,#15077,#12334,.T.) ;
#19499 = EDGE_CURVE('',#15077,#15075,#8162,.T.) ;
#19500 = EDGE_CURVE('',#15076,#15078,#12335,.T.) ;
#19501 = EDGE_CURVE('',#15078,#15077,#12336,.T.) ;
#19502 = EDGE_CURVE('',#15079,#15074,#8163,.T.) ;
#19503 = EDGE_CURVE('',#15080,#15079,#8164,.T.) ;
#19504 = EDGE_CURVE('',#15076,#15080,#8165,.T.) ;
#19505 = EDGE_CURVE('',#15070,#15081,#8166,.T.) ;
#19506 = EDGE_CURVE('',#15081,#15079,#12337,.F.) ;
#19507 = EDGE_CURVE('',#15066,#15082,#12338,.T.) ;
#19508 = EDGE_CURVE('',#15083,#15082,#1569,.T.) ;
#19509 = EDGE_CURVE('',#15084,#15083,#1570,.T.) ;
#19510 = EDGE_CURVE('',#15084,#15070,#12339,.T.) ;
#19511 = EDGE_CURVE('',#15085,#15086,#12340,.T.) ;
#19512 = EDGE_CURVE('',#15086,#15087,#12341,.T.) ;
#19513 = EDGE_CURVE('',#15087,#15085,#12342,.T.) ;
#19514 = EDGE_CURVE('',#15088,#15089,#12343,.T.) ;
#19515 = EDGE_CURVE('',#15089,#15086,#8167,.T.) ;
#19516 = EDGE_CURVE('',#15085,#15088,#8168,.T.) ;
#19517 = EDGE_CURVE('',#15088,#15090,#215,.T.) ;
#19518 = EDGE_CURVE('',#15090,#15082,#12344,.T.) ;
#19519 = EDGE_CURVE('',#15082,#15089,#216,.T.) ;
#19520 = EDGE_CURVE('',#15090,#15091,#1571,.T.) ;
#19521 = EDGE_CURVE('',#15091,#15084,#1572,.T.) ;
#19522 = EDGE_CURVE('',#15088,#15092,#8169,.T.) ;
#19523 = EDGE_CURVE('',#15092,#15093,#12345,.F.) ;
#19524 = EDGE_CURVE('',#15093,#15084,#8170,.T.) ;
#19525 = EDGE_CURVE('',#15094,#15085,#8171,.T.) ;
#19526 = EDGE_CURVE('',#15092,#15094,#8172,.T.) ;
#19527 = EDGE_CURVE('',#15087,#15095,#8173,.T.) ;
#19528 = EDGE_CURVE('',#15094,#15095,#217,.T.) ;
#19529 = EDGE_CURVE('',#15081,#15063,#8174,.T.) ;
#19530 = EDGE_CURVE('',#15096,#15093,#8175,.T.) ;
#19531 = EDGE_CURVE('',#14914,#15096,#8176,.T.) ;
#19532 = EDGE_CURVE('',#15097,#15098,#12346,.T.) ;
#19533 = EDGE_CURVE('',#15098,#15099,#8177,.T.) ;
#19534 = EDGE_CURVE('',#15099,#15100,#12347,.T.) ;
#19535 = EDGE_CURVE('',#15100,#15097,#8178,.T.) ;
#19536 = EDGE_CURVE('',#15099,#15101,#218,.T.) ;
#19537 = EDGE_CURVE('',#15101,#15100,#219,.T.) ;
#19538 = EDGE_CURVE('',#15096,#15097,#12348,.T.) ;
#19539 = EDGE_CURVE('',#15097,#15102,#220,.T.) ;
#19540 = EDGE_CURVE('',#15102,#14928,#12349,.T.) ;
#19541 = EDGE_CURVE('',#14928,#15096,#221,.T.) ;
#19542 = EDGE_CURVE('',#15103,#14929,#12350,.T.) ;
#19543 = EDGE_CURVE('',#15102,#15103,#8179,.T.) ;
#19544 = EDGE_CURVE('',#15103,#15104,#12351,.T.) ;
#19545 = EDGE_CURVE('',#15104,#14929,#12352,.T.) ;
#19546 = EDGE_CURVE('',#15096,#15098,#12353,.T.) ;
#19547 = EDGE_CURVE('',#14932,#15100,#8180,.T.) ;
#19548 = EDGE_CURVE('',#15101,#14933,#8181,.T.) ;
#19549 = EDGE_CURVE('',#15099,#15105,#8182,.T.) ;
#19550 = EDGE_CURVE('',#15095,#15105,#222,.T.) ;
#19551 = EDGE_CURVE('',#15095,#15101,#8183,.T.) ;
#19552 = EDGE_CURVE('',#15106,#15098,#8184,.T.) ;
#19553 = EDGE_CURVE('',#15105,#15106,#8185,.T.) ;
#19554 = EDGE_CURVE('',#15106,#15092,#12354,.F.) ;
#19555 = EDGE_CURVE('',#15093,#15106,#12355,.F.) ;
#19556 = EDGE_CURVE('',#15105,#15094,#12356,.T.) ;
#19557 = EDGE_CURVE('',#15103,#14935,#12357,.T.) ;
#19558 = EDGE_CURVE('',#15064,#14990,#12358,.T.) ;
#19559 = EDGE_CURVE('',#14989,#15063,#12359,.T.) ;
#19560 = EDGE_CURVE('',#15107,#14991,#12360,.T.) ;
#19561 = EDGE_CURVE('',#15064,#15107,#8186,.T.) ;
#19562 = EDGE_CURVE('',#15107,#15108,#12361,.T.) ;
#19563 = EDGE_CURVE('',#15108,#14991,#12362,.T.) ;
#19564 = EDGE_CURVE('',#15109,#14989,#12363,.T.) ;
#19565 = EDGE_CURVE('',#14988,#15110,#12364,.T.) ;
#19566 = EDGE_CURVE('',#15110,#15109,#8187,.T.) ;
#19567 = EDGE_CURVE('',#14992,#15110,#223,.T.) ;
#19568 = EDGE_CURVE('',#15109,#15063,#12365,.T.) ;
#19569 = EDGE_CURVE('',#15108,#14983,#12366,.T.) ;
#19570 = EDGE_CURVE('',#15107,#15111,#12367,.T.) ;
#19571 = EDGE_CURVE('',#15111,#15112,#12368,.T.) ;
#19572 = EDGE_CURVE('',#15112,#15108,#12369,.T.) ;
#19573 = EDGE_CURVE('',#15113,#14905,#8188,.T.) ;
#19574 = EDGE_CURVE('',#15111,#15113,#1573,.T.) ;
#19575 = EDGE_CURVE('',#15114,#15110,#8189,.T.) ;
#19576 = EDGE_CURVE('',#15115,#15114,#8190,.T.) ;
#19577 = EDGE_CURVE('',#15109,#15115,#8191,.T.) ;
#19578 = EDGE_CURVE('',#15079,#15115,#12370,.F.) ;
#19579 = EDGE_CURVE('',#15115,#15081,#12371,.F.) ;
#19580 = EDGE_CURVE('',#15114,#15080,#12372,.T.) ;
#19581 = EDGE_CURVE('',#15114,#15116,#224,.T.) ;
#19582 = EDGE_CURVE('',#15116,#15080,#225,.T.) ;
#19583 = EDGE_CURVE('',#15116,#15078,#8192,.T.) ;
#19584 = EDGE_CURVE('',#14992,#15116,#8193,.T.) ;
#19585 = EDGE_CURVE('',#15024,#15033,#12373,.T.) ;
#19586 = EDGE_CURVE('',#15032,#15023,#12374,.T.) ;
#19587 = EDGE_CURVE('',#14941,#14947,#12375,.T.) ;
#19588 = EDGE_CURVE('',#14946,#14944,#12376,.T.) ;
#19589 = EDGE_CURVE('',#15078,#15087,#12377,.T.) ;
#19590 = EDGE_CURVE('',#15086,#15077,#12378,.T.) ;
#19591 = EDGE_CURVE('',#15048,#14995,#12379,.T.) ;
#19592 = EDGE_CURVE('',#15104,#15117,#12380,.T.) ;
#19593 = EDGE_CURVE('',#15117,#14930,#12381,.T.) ;
#19594 = EDGE_CURVE('',#15117,#14927,#1574,.T.) ;
#19595 = EDGE_CURVE('',#14936,#15104,#12382,.T.) ;
#19596 = EDGE_CURVE('',#14943,#14949,#12383,.T.) ;
#19597 = EDGE_CURVE('',#14952,#14938,#12384,.T.) ;
#19598 = EDGE_CURVE('',#14861,#15118,#8194,.T.) ;
#19599 = EDGE_CURVE('',#15118,#15059,#12385,.T.) ;
#19600 = EDGE_CURVE('',#15118,#15058,#1575,.T.) ;
#19601 = EDGE_CURVE('',#15058,#15117,#12386,.T.) ;
#19602 = EDGE_CURVE('',#15118,#14927,#12387,.T.) ;
#19603 = EDGE_CURVE('',#14901,#15119,#12388,.T.) ;
#19604 = EDGE_CURVE('',#15119,#14898,#1576,.T.) ;
#19605 = EDGE_CURVE('',#15049,#15119,#12389,.T.) ;
#19606 = EDGE_CURVE('',#14996,#15049,#12390,.T.) ;
#19607 = EDGE_CURVE('',#14971,#14996,#12391,.T.) ;
#19608 = EDGE_CURVE('',#15113,#15120,#12392,.T.) ;
#19609 = EDGE_CURVE('',#15120,#15112,#1577,.T.) ;
#19610 = EDGE_CURVE('',#14874,#15120,#8195,.T.) ;
#19611 = EDGE_CURVE('',#15112,#15119,#12393,.T.) ;
#19612 = EDGE_CURVE('',#15120,#14898,#12394,.T.) ;
#19613 = EDGE_CURVE('',#14841,#15121,#1578,.F.) ;
#19614 = EDGE_CURVE('',#15121,#15122,#8196,.T.) ;
#19615 = EDGE_CURVE('',#15122,#15122,#12395,.T.) ;
#19616 = EDGE_CURVE('',#15121,#14838,#1579,.F.) ;
#19617 = EDGE_CURVE('',#15123,#15124,#8197,.T.) ;
#19618 = EDGE_CURVE('',#15124,#15125,#1580,.T.) ;
#19619 = EDGE_CURVE('',#15126,#15125,#12396,.T.) ;
#19620 = EDGE_CURVE('',#15123,#15126,#1581,.F.) ;
#19621 = EDGE_CURVE('',#15127,#15128,#8198,.T.) ;
#19622 = EDGE_CURVE('',#15128,#15124,#1582,.T.) ;
#19623 = EDGE_CURVE('',#15127,#15123,#1583,.F.) ;
#19624 = EDGE_CURVE('',#15129,#15130,#8199,.T.) ;
#19625 = EDGE_CURVE('',#15130,#15128,#1584,.T.) ;
#19626 = EDGE_CURVE('',#15129,#15127,#1585,.F.) ;
#19627 = EDGE_CURVE('',#15131,#15132,#8200,.T.) ;
#19628 = EDGE_CURVE('',#15133,#15131,#1586,.F.) ;
#19629 = EDGE_CURVE('',#15134,#15133,#12397,.T.) ;
#19630 = EDGE_CURVE('',#15134,#15132,#1587,.T.) ;
#19631 = EDGE_CURVE('',#15135,#15136,#8201,.T.) ;
#19632 = EDGE_CURVE('',#15136,#15137,#1588,.T.) ;
#19633 = EDGE_CURVE('',#15138,#15137,#12398,.F.) ;
#19634 = EDGE_CURVE('',#15138,#15135,#1589,.T.) ;
#19635 = EDGE_CURVE('',#15139,#15140,#8202,.T.) ;
#19636 = EDGE_CURVE('',#15140,#15136,#1590,.T.) ;
#19637 = EDGE_CURVE('',#15135,#15139,#1591,.T.) ;
#19638 = EDGE_CURVE('',#15141,#15142,#8203,.T.) ;
#19639 = EDGE_CURVE('',#15142,#15140,#1592,.T.) ;
#19640 = EDGE_CURVE('',#15139,#15141,#1593,.T.) ;
#19641 = EDGE_CURVE('',#15143,#15144,#8204,.T.) ;
#19642 = EDGE_CURVE('',#15143,#15145,#1594,.T.) ;
#19643 = EDGE_CURVE('',#15146,#15145,#12399,.F.) ;
#19644 = EDGE_CURVE('',#15146,#15144,#1595,.T.) ;
#19645 = EDGE_CURVE('',#15144,#15142,#1596,.T.) ;
#19646 = EDGE_CURVE('',#15141,#15143,#1597,.T.) ;
#19647 = EDGE_CURVE('',#15132,#15130,#1598,.T.) ;
#19648 = EDGE_CURVE('',#15131,#15129,#1599,.F.) ;
#19649 = EDGE_CURVE('',#15147,#15148,#12400,.T.) ;
#19650 = EDGE_CURVE('',#15148,#15149,#8205,.T.) ;
#19651 = EDGE_CURVE('',#15149,#15150,#12401,.T.) ;
#19652 = EDGE_CURVE('',#15150,#15147,#8206,.T.) ;
#19653 = EDGE_CURVE('',#15151,#15152,#12402,.F.) ;
#19654 = EDGE_CURVE('',#15153,#15151,#12403,.T.) ;
#19655 = EDGE_CURVE('',#15153,#15154,#12404,.T.) ;
#19656 = EDGE_CURVE('',#15152,#15154,#12405,.T.) ;
#19657 = EDGE_CURVE('',#15155,#15156,#12406,.T.) ;
#19658 = EDGE_CURVE('',#15156,#15153,#8207,.T.) ;
#19659 = EDGE_CURVE('',#15151,#15155,#8208,.T.) ;
#19660 = EDGE_CURVE('',#15157,#15158,#12407,.F.) ;
#19661 = EDGE_CURVE('',#15159,#15157,#12408,.T.) ;
#19662 = EDGE_CURVE('',#15159,#15160,#12409,.T.) ;
#19663 = EDGE_CURVE('',#15158,#15160,#12410,.T.) ;
#19664 = EDGE_CURVE('',#15161,#15162,#12411,.F.) ;
#19665 = EDGE_CURVE('',#15163,#15161,#12412,.T.) ;
#19666 = EDGE_CURVE('',#15163,#15164,#12413,.T.) ;
#19667 = EDGE_CURVE('',#15162,#15164,#12414,.T.) ;
#19668 = EDGE_CURVE('',#15165,#15166,#12415,.T.) ;
#19669 = EDGE_CURVE('',#15166,#15163,#8209,.T.) ;
#19670 = EDGE_CURVE('',#15161,#15165,#8210,.T.) ;
#19671 = EDGE_CURVE('',#15167,#15168,#12416,.T.) ;
#19672 = EDGE_CURVE('',#15168,#15166,#12417,.T.) ;
#19673 = EDGE_CURVE('',#15165,#15167,#12418,.T.) ;
#19674 = EDGE_CURVE('',#15154,#15168,#8211,.T.) ;
#19675 = EDGE_CURVE('',#15167,#15152,#8212,.T.) ;
#19676 = EDGE_CURVE('',#15169,#15149,#12419,.T.) ;
#19677 = EDGE_CURVE('',#15149,#15162,#8213,.T.) ;
#19678 = EDGE_CURVE('',#15164,#15169,#8214,.T.) ;
#19679 = EDGE_CURVE('',#15170,#15171,#12420,.F.) ;
#19680 = EDGE_CURVE('',#15172,#15170,#12421,.T.) ;
#19681 = EDGE_CURVE('',#15172,#15173,#12422,.T.) ;
#19682 = EDGE_CURVE('',#15171,#15173,#12423,.T.) ;
#19683 = EDGE_CURVE('',#15148,#15174,#12424,.T.) ;
#19684 = EDGE_CURVE('',#15174,#15172,#8215,.T.) ;
#19685 = EDGE_CURVE('',#15170,#15148,#8216,.T.) ;
#19686 = EDGE_CURVE('',#15175,#15176,#12425,.T.) ;
#19687 = EDGE_CURVE('',#15176,#15159,#8217,.T.) ;
#19688 = EDGE_CURVE('',#15157,#15175,#8218,.T.) ;
#19689 = EDGE_CURVE('',#15177,#15178,#12426,.T.) ;
#19690 = EDGE_CURVE('',#15178,#15176,#12427,.T.) ;
#19691 = EDGE_CURVE('',#15175,#15177,#12428,.T.) ;
#19692 = EDGE_CURVE('',#15173,#15178,#8219,.T.) ;
#19693 = EDGE_CURVE('',#15177,#15171,#8220,.T.) ;
#19694 = EDGE_CURVE('',#15171,#15161,#8221,.T.) ;
#19695 = EDGE_CURVE('',#15162,#15170,#8222,.T.) ;
#19696 = EDGE_CURVE('',#15179,#15180,#12429,.T.) ;
#19697 = EDGE_CURVE('',#15180,#15158,#8223,.T.) ;
#19698 = EDGE_CURVE('',#15160,#15179,#8224,.T.) ;
#19699 = EDGE_CURVE('',#15152,#15157,#8225,.T.) ;
#19700 = EDGE_CURVE('',#15158,#15151,#8226,.T.) ;
#19701 = EDGE_CURVE('',#15147,#15174,#12430,.T.) ;
#19702 = EDGE_CURVE('',#15169,#15150,#12431,.T.) ;
#19703 = EDGE_CURVE('',#15180,#15181,#12432,.T.) ;
#19704 = EDGE_CURVE('',#15181,#15182,#8227,.T.) ;
#19705 = EDGE_CURVE('',#15182,#15155,#12433,.T.) ;
#19706 = EDGE_CURVE('',#15155,#15180,#8228,.T.) ;
#19707 = EDGE_CURVE('',#15179,#15181,#12434,.T.) ;
#19708 = EDGE_CURVE('',#15182,#15156,#12435,.T.) ;
#19709 = EDGE_CURVE('',#15177,#15165,#8229,.T.) ;
#19710 = EDGE_CURVE('',#15169,#15183,#8230,.T.) ;
#19711 = EDGE_CURVE('',#15184,#15183,#12436,.T.) ;
#19712 = EDGE_CURVE('',#15150,#15184,#8231,.T.) ;
#19713 = EDGE_CURVE('',#15185,#15156,#8232,.T.) ;
#19714 = EDGE_CURVE('',#15185,#15186,#1600,.T.) ;
#19715 = EDGE_CURVE('',#15187,#15186,#8233,.T.) ;
#19716 = EDGE_CURVE('',#15187,#15183,#1601,.T.) ;
#19717 = EDGE_CURVE('',#15182,#15188,#8234,.T.) ;
#19718 = EDGE_CURVE('',#15185,#15188,#12437,.T.) ;
#19719 = EDGE_CURVE('',#15189,#15181,#8235,.T.) ;
#19720 = EDGE_CURVE('',#15188,#15189,#8236,.T.) ;
#19721 = EDGE_CURVE('',#15175,#15167,#8237,.T.) ;
#19722 = EDGE_CURVE('',#15179,#15190,#8238,.T.) ;
#19723 = EDGE_CURVE('',#15190,#15189,#12438,.T.) ;
#19724 = EDGE_CURVE('',#15147,#15191,#8239,.T.) ;
#19725 = EDGE_CURVE('',#15191,#15192,#12439,.T.) ;
#19726 = EDGE_CURVE('',#15192,#15174,#8240,.T.) ;
#19727 = EDGE_CURVE('',#15193,#15192,#12440,.T.) ;
#19728 = EDGE_CURVE('',#15194,#15193,#8241,.T.) ;
#19729 = EDGE_CURVE('',#15195,#15194,#8242,.T.) ;
#19730 = EDGE_CURVE('',#15195,#15196,#8243,.T.) ;
#19731 = EDGE_CURVE('',#15197,#15196,#8244,.T.) ;
#19732 = EDGE_CURVE('',#15198,#15197,#8245,.T.) ;
#19733 = EDGE_CURVE('',#15190,#15198,#12441,.T.) ;
#19734 = EDGE_CURVE('',#15191,#15184,#8246,.T.) ;
#19735 = EDGE_CURVE('',#15199,#15200,#8247,.T.) ;
#19736 = EDGE_CURVE('',#15201,#15199,#8248,.T.) ;
#19737 = EDGE_CURVE('',#15201,#15202,#1602,.T.) ;
#19738 = EDGE_CURVE('',#15202,#15203,#8249,.T.) ;
#19739 = EDGE_CURVE('',#15203,#15204,#1603,.T.) ;
#19740 = EDGE_CURVE('',#15200,#15204,#8250,.T.) ;
#19741 = EDGE_CURVE('',#15205,#15206,#8251,.T.) ;
#19742 = EDGE_CURVE('',#15207,#15205,#8252,.T.) ;
#19743 = EDGE_CURVE('',#15208,#15207,#8253,.T.) ;
#19744 = EDGE_CURVE('',#15206,#15208,#8254,.T.) ;
#19745 = EDGE_CURVE('',#15209,#15210,#8255,.T.) ;
#19746 = EDGE_CURVE('',#15211,#15209,#8256,.T.) ;
#19747 = EDGE_CURVE('',#15212,#15211,#12442,.T.) ;
#19748 = EDGE_CURVE('',#15213,#15212,#8257,.T.) ;
#19749 = EDGE_CURVE('',#15214,#15213,#8258,.T.) ;
#19750 = EDGE_CURVE('',#15215,#15214,#8259,.T.) ;
#19751 = EDGE_CURVE('',#15216,#15215,#8260,.T.) ;
#19752 = EDGE_CURVE('',#15217,#15216,#8261,.T.) ;
#19753 = EDGE_CURVE('',#15218,#15217,#12443,.T.) ;
#19754 = EDGE_CURVE('',#15210,#15218,#8262,.T.) ;
#19755 = EDGE_CURVE('',#15219,#15220,#8263,.T.) ;
#19756 = EDGE_CURVE('',#15219,#15221,#8264,.T.) ;
#19757 = EDGE_CURVE('',#15222,#15221,#8265,.T.) ;
#19758 = EDGE_CURVE('',#15220,#15222,#8266,.T.) ;
#19759 = EDGE_CURVE('',#15125,#15138,#1604,.T.) ;
#19760 = EDGE_CURVE('',#15137,#15126,#1605,.T.) ;
#19761 = EDGE_CURVE('',#15215,#15219,#12444,.T.) ;
#19762 = EDGE_CURVE('',#15221,#15214,#12445,.T.) ;
#19763 = EDGE_CURVE('',#15220,#15195,#12446,.T.) ;
#19764 = EDGE_CURVE('',#15196,#15222,#12447,.T.) ;
#19765 = EDGE_CURVE('',#15223,#15203,#1606,.T.) ;
#19766 = EDGE_CURVE('',#15202,#15224,#1607,.T.) ;
#19767 = EDGE_CURVE('',#15223,#15224,#8267,.T.) ;
#19768 = EDGE_CURVE('',#15186,#15225,#1608,.T.) ;
#19769 = EDGE_CURVE('',#15225,#15226,#8268,.T.) ;
#19770 = EDGE_CURVE('',#15226,#15187,#1609,.T.) ;
#19771 = EDGE_CURVE('',#15227,#15228,#8269,.T.) ;
#19772 = EDGE_CURVE('',#15229,#15227,#8270,.T.) ;
#19773 = EDGE_CURVE('',#15230,#15229,#8271,.T.) ;
#19774 = EDGE_CURVE('',#15228,#15230,#8272,.T.) ;
#19775 = EDGE_CURVE('',#15200,#15227,#12448,.T.) ;
#19776 = EDGE_CURVE('',#15229,#15204,#12449,.T.) ;
#19777 = EDGE_CURVE('',#15231,#15232,#8273,.T.) ;
#19778 = EDGE_CURVE('',#15233,#15231,#8274,.T.) ;
#19779 = EDGE_CURVE('',#15234,#15233,#12450,.T.) ;
#19780 = EDGE_CURVE('',#15235,#15234,#8275,.T.) ;
#19781 = EDGE_CURVE('',#15236,#15235,#12451,.T.) ;
#19782 = EDGE_CURVE('',#15232,#15236,#8276,.T.) ;
#19783 = EDGE_CURVE('',#15237,#15238,#8277,.T.) ;
#19784 = EDGE_CURVE('',#15239,#15237,#12452,.T.) ;
#19785 = EDGE_CURVE('',#15240,#15239,#8278,.T.) ;
#19786 = EDGE_CURVE('',#15241,#15240,#12453,.T.) ;
#19787 = EDGE_CURVE('',#15242,#15241,#8279,.T.) ;
#19788 = EDGE_CURVE('',#15238,#15242,#8280,.T.) ;
#19789 = EDGE_CURVE('',#15243,#15199,#12454,.T.) ;
#19790 = EDGE_CURVE('',#15243,#15244,#8281,.T.) ;
#19791 = EDGE_CURVE('',#15201,#15244,#12455,.T.) ;
#19792 = EDGE_CURVE('',#15245,#15243,#8282,.T.) ;
#19793 = EDGE_CURVE('',#15246,#15245,#8283,.T.) ;
#19794 = EDGE_CURVE('',#15244,#15246,#8284,.T.) ;
#19795 = EDGE_CURVE('',#15247,#15188,#12456,.T.) ;
#19796 = EDGE_CURVE('',#15247,#15225,#12457,.T.) ;
#19797 = EDGE_CURVE('',#15226,#15248,#12458,.T.) ;
#19798 = EDGE_CURVE('',#15184,#15248,#12459,.T.) ;
#19799 = EDGE_CURVE('',#15223,#15249,#12460,.T.) ;
#19800 = EDGE_CURVE('',#15229,#15249,#12461,.T.) ;
#19801 = EDGE_CURVE('',#15243,#15206,#12462,.T.) ;
#19802 = EDGE_CURVE('',#15206,#15199,#12463,.T.) ;
#19803 = EDGE_CURVE('',#15250,#15244,#12464,.T.) ;
#19804 = EDGE_CURVE('',#15250,#15224,#12465,.T.) ;
#19805 = EDGE_CURVE('',#15200,#15205,#12466,.T.) ;
#19806 = EDGE_CURVE('',#15205,#15227,#12467,.T.) ;
#19807 = EDGE_CURVE('',#15189,#15251,#12468,.F.) ;
#19808 = EDGE_CURVE('',#15251,#15247,#8285,.T.) ;
#19809 = EDGE_CURVE('',#15248,#15252,#8286,.T.) ;
#19810 = EDGE_CURVE('',#15252,#15191,#12469,.F.) ;
#19811 = EDGE_CURVE('',#15197,#15253,#12470,.F.) ;
#19812 = EDGE_CURVE('',#15253,#15251,#8287,.T.) ;
#19813 = EDGE_CURVE('',#15251,#15198,#12471,.T.) ;
#19814 = EDGE_CURVE('',#15193,#15252,#12472,.T.) ;
#19815 = EDGE_CURVE('',#15252,#15254,#8288,.T.) ;
#19816 = EDGE_CURVE('',#15254,#15194,#12473,.F.) ;
#19817 = EDGE_CURVE('',#15213,#15232,#12474,.F.) ;
#19818 = EDGE_CURVE('',#15214,#15236,#12475,.T.) ;
#19819 = EDGE_CURVE('',#15221,#15235,#12476,.T.) ;
#19820 = EDGE_CURVE('',#15222,#15234,#12477,.T.) ;
#19821 = EDGE_CURVE('',#15196,#15233,#12478,.T.) ;
#19822 = EDGE_CURVE('',#15231,#15197,#12479,.F.) ;
#19823 = EDGE_CURVE('',#15232,#15255,#12480,.F.) ;
#19824 = EDGE_CURVE('',#15255,#15253,#8289,.T.) ;
#19825 = EDGE_CURVE('',#15253,#15231,#12481,.F.) ;
#19826 = EDGE_CURVE('',#15242,#15254,#12482,.F.) ;
#19827 = EDGE_CURVE('',#15254,#15256,#8290,.T.) ;
#19828 = EDGE_CURVE('',#15256,#15238,#12483,.F.) ;
#19829 = EDGE_CURVE('',#15194,#15242,#12484,.F.) ;
#19830 = EDGE_CURVE('',#15195,#15241,#12485,.T.) ;
#19831 = EDGE_CURVE('',#15220,#15240,#12486,.T.) ;
#19832 = EDGE_CURVE('',#15219,#15239,#12487,.T.) ;
#19833 = EDGE_CURVE('',#15215,#15237,#12488,.T.) ;
#19834 = EDGE_CURVE('',#15238,#15216,#12489,.F.) ;
#19835 = EDGE_CURVE('',#15249,#15257,#8291,.T.) ;
#19836 = EDGE_CURVE('',#15257,#15230,#12490,.F.) ;
#19837 = EDGE_CURVE('',#15209,#15228,#12491,.F.) ;
#19838 = EDGE_CURVE('',#15230,#15211,#12492,.T.) ;
#19839 = EDGE_CURVE('',#15228,#15207,#12493,.F.) ;
#19840 = EDGE_CURVE('',#15208,#15245,#12494,.F.) ;
#19841 = EDGE_CURVE('',#15218,#15246,#12495,.T.) ;
#19842 = EDGE_CURVE('',#15245,#15210,#12496,.F.) ;
#19843 = EDGE_CURVE('',#15207,#15209,#12497,.F.) ;
#19844 = EDGE_CURVE('',#15210,#15208,#12498,.F.) ;
#19845 = EDGE_CURVE('',#15246,#15258,#12499,.F.) ;
#19846 = EDGE_CURVE('',#15258,#15250,#8292,.T.) ;
#19847 = EDGE_CURVE('',#15216,#15256,#12500,.F.) ;
#19848 = EDGE_CURVE('',#15256,#15258,#8293,.T.) ;
#19849 = EDGE_CURVE('',#15258,#15217,#12501,.T.) ;
#19850 = EDGE_CURVE('',#15212,#15257,#12502,.T.) ;
#19851 = EDGE_CURVE('',#15257,#15255,#8294,.T.) ;
#19852 = EDGE_CURVE('',#15255,#15213,#12503,.F.) ;
#19853 = EDGE_CURVE('',#15259,#15259,#12504,.T.) ;
#19854 = EDGE_CURVE('',#15259,#15260,#12505,.T.) ;
#19855 = EDGE_CURVE('',#15260,#15260,#12506,.T.) ;
#19856 = EDGE_CURVE('',#15261,#15261,#12507,.T.) ;
#19857 = EDGE_CURVE('',#15262,#15263,#12508,.T.) ;
#19858 = EDGE_CURVE('',#15263,#15262,#12509,.T.) ;
#19859 = EDGE_CURVE('',#15263,#15260,#8295,.T.) ;
#19860 = EDGE_CURVE('',#15261,#15262,#12510,.T.) ;
#19861 = EDGE_CURVE('',#15145,#15134,#1610,.T.) ;
#19862 = EDGE_CURVE('',#15133,#15146,#1611,.T.) ;
#19863 = EDGE_CURVE('',#15264,#15265,#1612,.T.) ;
#19864 = EDGE_CURVE('',#15266,#15264,#12511,.T.) ;
#19865 = EDGE_CURVE('',#15267,#15266,#1613,.T.) ;
#19866 = EDGE_CURVE('',#15265,#15267,#12512,.T.) ;
#19867 = EDGE_CURVE('',#15268,#15269,#1614,.T.) ;
#19868 = EDGE_CURVE('',#15270,#15268,#12513,.T.) ;
#19869 = EDGE_CURVE('',#15271,#15270,#1615,.T.) ;
#19870 = EDGE_CURVE('',#15269,#15271,#12514,.T.) ;
#19871 = EDGE_CURVE('',#15272,#15266,#12515,.T.) ;
#19872 = EDGE_CURVE('',#15273,#15272,#1616,.T.) ;
#19873 = EDGE_CURVE('',#15267,#15273,#12516,.T.) ;
#19874 = EDGE_CURVE('',#15274,#15275,#1617,.T.) ;
#19875 = EDGE_CURVE('',#15276,#15274,#12517,.T.) ;
#19876 = EDGE_CURVE('',#15277,#15276,#1618,.T.) ;
#19877 = EDGE_CURVE('',#15275,#15277,#12518,.T.) ;
#19878 = EDGE_CURVE('',#15278,#15279,#1619,.T.) ;
#19879 = EDGE_CURVE('',#15280,#15278,#12519,.T.) ;
#19880 = EDGE_CURVE('',#15281,#15280,#1620,.T.) ;
#19881 = EDGE_CURVE('',#15279,#15281,#12520,.T.) ;
#19882 = EDGE_CURVE('',#15282,#15282,#12521,.T.) ;
#19883 = EDGE_CURVE('',#15282,#15283,#8296,.T.) ;
#19884 = EDGE_CURVE('',#15283,#15283,#12522,.T.) ;
#19885 = EDGE_CURVE('',#15284,#15268,#8297,.T.) ;
#19886 = EDGE_CURVE('',#15284,#15285,#8298,.T.) ;
#19887 = EDGE_CURVE('',#15286,#15285,#12523,.T.) ;
#19888 = EDGE_CURVE('',#15286,#15287,#8299,.T.) ;
#19889 = EDGE_CURVE('',#15276,#15287,#8300,.T.) ;
#19890 = EDGE_CURVE('',#15288,#15274,#8301,.T.) ;
#19891 = EDGE_CURVE('',#15288,#15289,#8302,.T.) ;
#19892 = EDGE_CURVE('',#15290,#15289,#12524,.T.) ;
#19893 = EDGE_CURVE('',#15290,#15291,#8303,.T.) ;
#19894 = EDGE_CURVE('',#15272,#15291,#8304,.T.) ;
#19895 = EDGE_CURVE('',#15292,#15264,#8305,.T.) ;
#19896 = EDGE_CURVE('',#15292,#15293,#8306,.T.) ;
#19897 = EDGE_CURVE('',#15294,#15293,#12525,.T.) ;
#19898 = EDGE_CURVE('',#15294,#15295,#8307,.T.) ;
#19899 = EDGE_CURVE('',#15280,#15295,#8308,.T.) ;
#19900 = EDGE_CURVE('',#15296,#15278,#8309,.T.) ;
#19901 = EDGE_CURVE('',#15296,#15297,#8310,.T.) ;
#19902 = EDGE_CURVE('',#15298,#15297,#12526,.T.) ;
#19903 = EDGE_CURVE('',#15298,#15299,#8311,.T.) ;
#19904 = EDGE_CURVE('',#15270,#15299,#8312,.T.) ;
#19905 = EDGE_CURVE('',#15300,#15301,#8313,.T.) ;
#19906 = EDGE_CURVE('',#15302,#15300,#8314,.T.) ;
#19907 = EDGE_CURVE('',#15303,#15302,#8315,.T.) ;
#19908 = EDGE_CURVE('',#15301,#15303,#12527,.T.) ;
#19909 = EDGE_CURVE('',#15304,#15305,#8316,.T.) ;
#19910 = EDGE_CURVE('',#15306,#15304,#8317,.T.) ;
#19911 = EDGE_CURVE('',#15307,#15306,#12528,.T.) ;
#19912 = EDGE_CURVE('',#15305,#15307,#8318,.T.) ;
#19913 = EDGE_CURVE('',#15308,#15309,#8319,.T.) ;
#19914 = EDGE_CURVE('',#15310,#15308,#8320,.T.) ;
#19915 = EDGE_CURVE('',#15311,#15310,#8321,.T.) ;
#19916 = EDGE_CURVE('',#15309,#15311,#12529,.T.) ;
#19917 = EDGE_CURVE('',#15312,#15313,#8322,.T.) ;
#19918 = EDGE_CURVE('',#15314,#15312,#8323,.T.) ;
#19919 = EDGE_CURVE('',#15315,#15314,#12530,.T.) ;
#19920 = EDGE_CURVE('',#15313,#15315,#8324,.T.) ;
#19921 = EDGE_CURVE('',#15294,#15316,#12531,.T.) ;
#19922 = EDGE_CURVE('',#15293,#15317,#12532,.T.) ;
#19923 = EDGE_CURVE('',#15316,#15317,#12533,.T.) ;
#19924 = EDGE_CURVE('',#15316,#15318,#8325,.T.) ;
#19925 = EDGE_CURVE('',#15295,#15318,#12534,.T.) ;
#19926 = EDGE_CURVE('',#15319,#15292,#12535,.T.) ;
#19927 = EDGE_CURVE('',#15319,#15317,#8326,.T.) ;
#19928 = EDGE_CURVE('',#15320,#15298,#12536,.T.) ;
#19929 = EDGE_CURVE('',#15297,#15321,#12537,.T.) ;
#19930 = EDGE_CURVE('',#15320,#15321,#12538,.T.) ;
#19931 = EDGE_CURVE('',#15320,#15322,#8327,.T.) ;
#19932 = EDGE_CURVE('',#15299,#15322,#12539,.T.) ;
#19933 = EDGE_CURVE('',#15323,#15296,#12540,.T.) ;
#19934 = EDGE_CURVE('',#15323,#15321,#8328,.T.) ;
#19935 = EDGE_CURVE('',#15286,#15324,#12541,.T.) ;
#19936 = EDGE_CURVE('',#15285,#15325,#12542,.T.) ;
#19937 = EDGE_CURVE('',#15324,#15325,#12543,.T.) ;
#19938 = EDGE_CURVE('',#15324,#15326,#8329,.T.) ;
#19939 = EDGE_CURVE('',#15287,#15326,#12544,.T.) ;
#19940 = EDGE_CURVE('',#15327,#15284,#12545,.T.) ;
#19941 = EDGE_CURVE('',#15327,#15325,#8330,.T.) ;
#19942 = EDGE_CURVE('',#15328,#15329,#8331,.T.) ;
#19943 = EDGE_CURVE('',#15326,#15329,#8332,.T.) ;
#19944 = EDGE_CURVE('',#15324,#15328,#8333,.T.) ;
#19945 = EDGE_CURVE('',#15330,#15331,#8334,.T.) ;
#19946 = EDGE_CURVE('',#15325,#15331,#8335,.T.) ;
#19947 = EDGE_CURVE('',#15327,#15330,#8336,.T.) ;
#19948 = EDGE_CURVE('',#15331,#15328,#12546,.T.) ;
#19949 = EDGE_CURVE('',#15311,#15328,#12547,.T.) ;
#19950 = EDGE_CURVE('',#15329,#15310,#12548,.T.) ;
#19951 = EDGE_CURVE('',#15308,#15330,#12549,.T.) ;
#19952 = EDGE_CURVE('',#15309,#15331,#12550,.T.) ;
#19953 = EDGE_CURVE('',#15332,#15333,#8337,.T.) ;
#19954 = EDGE_CURVE('',#15333,#15334,#8338,.T.) ;
#19955 = EDGE_CURVE('',#15335,#15334,#8339,.T.) ;
#19956 = EDGE_CURVE('',#15332,#15335,#8340,.T.) ;
#19957 = EDGE_CURVE('',#15336,#15337,#8341,.T.) ;
#19958 = EDGE_CURVE('',#15337,#15338,#8342,.T.) ;
#19959 = EDGE_CURVE('',#15339,#15338,#8343,.T.) ;
#19960 = EDGE_CURVE('',#15336,#15339,#8344,.T.) ;
#19961 = EDGE_CURVE('',#15338,#15307,#12551,.T.) ;
#19962 = EDGE_CURVE('',#15306,#15333,#12552,.T.) ;
#19963 = EDGE_CURVE('',#15338,#15333,#12553,.T.) ;
#19964 = EDGE_CURVE('',#15334,#15304,#12554,.T.) ;
#19965 = EDGE_CURVE('',#15305,#15337,#12555,.T.) ;
#19966 = EDGE_CURVE('',#15340,#15341,#8345,.T.) ;
#19967 = EDGE_CURVE('',#15318,#15341,#8346,.T.) ;
#19968 = EDGE_CURVE('',#15316,#15340,#8347,.T.) ;
#19969 = EDGE_CURVE('',#15342,#15343,#8348,.T.) ;
#19970 = EDGE_CURVE('',#15317,#15343,#8349,.T.) ;
#19971 = EDGE_CURVE('',#15319,#15342,#8350,.T.) ;
#19972 = EDGE_CURVE('',#15343,#15340,#12556,.T.) ;
#19973 = EDGE_CURVE('',#15343,#15315,#12557,.T.) ;
#19974 = EDGE_CURVE('',#15314,#15340,#12558,.T.) ;
#19975 = EDGE_CURVE('',#15341,#15312,#12559,.T.) ;
#19976 = EDGE_CURVE('',#15313,#15342,#12560,.T.) ;
#19977 = EDGE_CURVE('',#15344,#15345,#8351,.T.) ;
#19978 = EDGE_CURVE('',#15322,#15345,#8352,.T.) ;
#19979 = EDGE_CURVE('',#15320,#15344,#8353,.T.) ;
#19980 = EDGE_CURVE('',#15346,#15347,#8354,.T.) ;
#19981 = EDGE_CURVE('',#15321,#15347,#8355,.T.) ;
#19982 = EDGE_CURVE('',#15323,#15346,#8356,.T.) ;
#19983 = EDGE_CURVE('',#15347,#15344,#12561,.T.) ;
#19984 = EDGE_CURVE('',#15303,#15344,#12562,.T.) ;
#19985 = EDGE_CURVE('',#15345,#15302,#12563,.T.) ;
#19986 = EDGE_CURVE('',#15300,#15346,#12564,.T.) ;
#19987 = EDGE_CURVE('',#15301,#15347,#12565,.T.) ;
#19988 = EDGE_CURVE('',#15332,#15339,#12566,.T.) ;
#19989 = EDGE_CURVE('',#15332,#15290,#12567,.T.) ;
#19990 = EDGE_CURVE('',#15289,#15339,#12568,.T.) ;
#19991 = EDGE_CURVE('',#15291,#15335,#12569,.T.) ;
#19992 = EDGE_CURVE('',#15336,#15288,#12570,.T.) ;
#19993 = EDGE_CURVE('',#15348,#15349,#12571,.T.) ;
#19994 = EDGE_CURVE('',#15349,#15350,#8357,.T.) ;
#19995 = EDGE_CURVE('',#15350,#15351,#8358,.T.) ;
#19996 = EDGE_CURVE('',#15351,#15348,#8359,.T.) ;
#19997 = EDGE_CURVE('',#15352,#15353,#8360,.T.) ;
#19998 = EDGE_CURVE('',#15353,#15354,#8361,.T.) ;
#19999 = EDGE_CURVE('',#15352,#15354,#8362,.T.) ;
#20000 = EDGE_CURVE('',#15355,#15356,#8363,.T.) ;
#20001 = EDGE_CURVE('',#15355,#15357,#8364,.T.) ;
#20002 = EDGE_CURVE('',#15357,#15358,#8365,.T.) ;
#20003 = EDGE_CURVE('',#15356,#15358,#8366,.T.) ;
#20004 = EDGE_CURVE('',#15357,#15352,#12572,.T.) ;
#20005 = EDGE_CURVE('',#15358,#15352,#12573,.T.) ;
#20006 = EDGE_CURVE('',#15350,#15354,#12574,.T.) ;
#20007 = EDGE_CURVE('',#15352,#15349,#12575,.T.) ;
#20008 = EDGE_CURVE('',#15358,#15348,#12576,.T.) ;
#20009 = EDGE_CURVE('',#15356,#15351,#12577,.T.) ;
#20010 = EDGE_CURVE('',#15359,#15360,#12578,.T.) ;
#20011 = EDGE_CURVE('',#15360,#15361,#8367,.T.) ;
#20012 = EDGE_CURVE('',#15361,#15362,#8368,.T.) ;
#20013 = EDGE_CURVE('',#15362,#15359,#8369,.T.) ;
#20014 = EDGE_CURVE('',#15363,#15364,#8370,.T.) ;
#20015 = EDGE_CURVE('',#15364,#15365,#8371,.T.) ;
#20016 = EDGE_CURVE('',#15363,#15365,#8372,.T.) ;
#20017 = EDGE_CURVE('',#15366,#15367,#8373,.T.) ;
#20018 = EDGE_CURVE('',#15366,#15368,#8374,.T.) ;
#20019 = EDGE_CURVE('',#15368,#15369,#8375,.T.) ;
#20020 = EDGE_CURVE('',#15367,#15369,#8376,.T.) ;
#20021 = EDGE_CURVE('',#15368,#15363,#12579,.T.) ;
#20022 = EDGE_CURVE('',#15369,#15363,#12580,.T.) ;
#20023 = EDGE_CURVE('',#15361,#15365,#12581,.T.) ;
#20024 = EDGE_CURVE('',#15363,#15360,#12582,.T.) ;
#20025 = EDGE_CURVE('',#15369,#15359,#12583,.T.) ;
#20026 = EDGE_CURVE('',#15367,#15362,#12584,.T.) ;
#20027 = EDGE_CURVE('',#15370,#15371,#8377,.T.) ;
#20028 = EDGE_CURVE('',#15372,#15370,#8378,.T.) ;
#20029 = EDGE_CURVE('',#15373,#15372,#8379,.T.) ;
#20030 = EDGE_CURVE('',#15371,#15373,#12585,.T.) ;
#20031 = EDGE_CURVE('',#15374,#15375,#8380,.T.) ;
#20032 = EDGE_CURVE('',#15376,#15375,#8381,.T.) ;
#20033 = EDGE_CURVE('',#15376,#15374,#8382,.T.) ;
#20034 = EDGE_CURVE('',#15377,#15378,#8383,.T.) ;
#20035 = EDGE_CURVE('',#15379,#15378,#8384,.T.) ;
#20036 = EDGE_CURVE('',#15379,#15380,#8385,.T.) ;
#20037 = EDGE_CURVE('',#15380,#15377,#8386,.T.) ;
#20038 = EDGE_CURVE('',#15378,#15374,#12586,.T.) ;
#20039 = EDGE_CURVE('',#15374,#15379,#12587,.T.) ;
#20040 = EDGE_CURVE('',#15374,#15373,#12588,.T.) ;
#20041 = EDGE_CURVE('',#15372,#15375,#12589,.T.) ;
#20042 = EDGE_CURVE('',#15377,#15370,#12590,.T.) ;
#20043 = EDGE_CURVE('',#15378,#15371,#12591,.T.) ;
#20044 = EDGE_CURVE('',#15381,#15382,#8387,.T.) ;
#20045 = EDGE_CURVE('',#15383,#15381,#8388,.T.) ;
#20046 = EDGE_CURVE('',#15384,#15383,#8389,.T.) ;
#20047 = EDGE_CURVE('',#15382,#15384,#12592,.T.) ;
#20048 = EDGE_CURVE('',#15385,#15386,#8390,.T.) ;
#20049 = EDGE_CURVE('',#15387,#15386,#8391,.T.) ;
#20050 = EDGE_CURVE('',#15387,#15385,#8392,.T.) ;
#20051 = EDGE_CURVE('',#15388,#15389,#8393,.T.) ;
#20052 = EDGE_CURVE('',#15390,#15389,#8394,.T.) ;
#20053 = EDGE_CURVE('',#15390,#15391,#8395,.T.) ;
#20054 = EDGE_CURVE('',#15391,#15388,#8396,.T.) ;
#20055 = EDGE_CURVE('',#15389,#15385,#12593,.T.) ;
#20056 = EDGE_CURVE('',#15385,#15390,#12594,.T.) ;
#20057 = EDGE_CURVE('',#15385,#15384,#12595,.T.) ;
#20058 = EDGE_CURVE('',#15383,#15386,#12596,.T.) ;
#20059 = EDGE_CURVE('',#15388,#15381,#12597,.T.) ;
#20060 = EDGE_CURVE('',#15389,#15382,#12598,.T.) ;
#20061 = EDGE_CURVE('',#15392,#15271,#8397,.T.) ;
#20062 = EDGE_CURVE('',#15279,#15393,#8398,.T.) ;
#20063 = EDGE_CURVE('',#15394,#15393,#8399,.T.) ;
#20064 = EDGE_CURVE('',#15355,#15394,#8400,.T.) ;
#20065 = EDGE_CURVE('',#15395,#15353,#8401,.T.) ;
#20066 = EDGE_CURVE('',#15392,#15395,#8402,.T.) ;
#20067 = EDGE_CURVE('',#15396,#15273,#8403,.T.) ;
#20068 = EDGE_CURVE('',#15275,#15397,#8404,.T.) ;
#20069 = EDGE_CURVE('',#15398,#15397,#8405,.T.) ;
#20070 = EDGE_CURVE('',#15387,#15398,#8406,.T.) ;
#20071 = EDGE_CURVE('',#15399,#15391,#8407,.T.) ;
#20072 = EDGE_CURVE('',#15396,#15399,#8408,.T.) ;
#20073 = EDGE_CURVE('',#15400,#15277,#8409,.T.) ;
#20074 = EDGE_CURVE('',#15269,#15401,#8410,.T.) ;
#20075 = EDGE_CURVE('',#15402,#15401,#8411,.T.) ;
#20076 = EDGE_CURVE('',#15366,#15402,#8412,.T.) ;
#20077 = EDGE_CURVE('',#15403,#15364,#8413,.T.) ;
#20078 = EDGE_CURVE('',#15400,#15403,#8414,.T.) ;
#20079 = EDGE_CURVE('',#15404,#15281,#8415,.T.) ;
#20080 = EDGE_CURVE('',#15265,#15405,#8416,.T.) ;
#20081 = EDGE_CURVE('',#15406,#15405,#8417,.T.) ;
#20082 = EDGE_CURVE('',#15376,#15406,#8418,.T.) ;
#20083 = EDGE_CURVE('',#15407,#15380,#8419,.T.) ;
#20084 = EDGE_CURVE('',#15404,#15407,#8420,.T.) ;
#20085 = EDGE_CURVE('',#15407,#15394,#12599,.T.) ;
#20086 = EDGE_CURVE('',#15408,#15406,#12600,.T.) ;
#20087 = EDGE_CURVE('',#15399,#15408,#12601,.T.) ;
#20088 = EDGE_CURVE('',#15403,#15398,#12602,.T.) ;
#20089 = EDGE_CURVE('',#15395,#15402,#12603,.T.) ;
#20090 = EDGE_CURVE('',#15409,#15410,#12604,.T.) ;
#20091 = EDGE_CURVE('',#15410,#15395,#1621,.T.) ;
#20092 = EDGE_CURVE('',#15402,#15409,#1622,.T.) ;
#20093 = EDGE_CURVE('',#15410,#15392,#8421,.T.) ;
#20094 = EDGE_CURVE('',#15401,#15409,#8422,.T.) ;
#20095 = EDGE_CURVE('',#15411,#15412,#12605,.T.) ;
#20096 = EDGE_CURVE('',#15412,#15403,#1623,.T.) ;
#20097 = EDGE_CURVE('',#15398,#15411,#1624,.T.) ;
#20098 = EDGE_CURVE('',#15397,#15411,#8423,.T.) ;
#20099 = EDGE_CURVE('',#15412,#15400,#8424,.T.) ;
#20100 = EDGE_CURVE('',#15413,#15414,#12606,.T.) ;
#20101 = EDGE_CURVE('',#15414,#15399,#1625,.T.) ;
#20102 = EDGE_CURVE('',#15413,#15408,#1626,.T.) ;
#20103 = EDGE_CURVE('',#15415,#15413,#12607,.T.) ;
#20104 = EDGE_CURVE('',#15406,#15415,#1627,.T.) ;
#20105 = EDGE_CURVE('',#15414,#15396,#8425,.T.) ;
#20106 = EDGE_CURVE('',#15405,#15415,#8426,.T.) ;
#20107 = EDGE_CURVE('',#15416,#15417,#12608,.T.) ;
#20108 = EDGE_CURVE('',#15417,#15407,#1628,.T.) ;
#20109 = EDGE_CURVE('',#15394,#15416,#1629,.T.) ;
#20110 = EDGE_CURVE('',#15393,#15416,#8427,.T.) ;
#20111 = EDGE_CURVE('',#15417,#15404,#8428,.T.) ;
#20112 = EDGE_CURVE('',#15418,#15419,#8429,.T.) ;
#20113 = EDGE_CURVE('',#15419,#15420,#8430,.T.) ;
#20114 = EDGE_CURVE('',#15420,#15421,#8431,.T.) ;
#20115 = EDGE_CURVE('',#15421,#15422,#8432,.T.) ;
#20116 = EDGE_CURVE('',#15422,#15423,#8433,.T.) ;
#20117 = EDGE_CURVE('',#15423,#15418,#8434,.T.) ;
#20118 = EDGE_CURVE('',#15424,#15421,#8435,.T.) ;
#20119 = EDGE_CURVE('',#15424,#15425,#8436,.T.) ;
#20120 = EDGE_CURVE('',#15426,#15425,#8437,.T.) ;
#20121 = EDGE_CURVE('',#15427,#15426,#8438,.T.) ;
#20122 = EDGE_CURVE('',#15427,#15422,#8439,.T.) ;
#20123 = EDGE_CURVE('',#15420,#15428,#8440,.T.) ;
#20124 = EDGE_CURVE('',#15429,#15428,#8441,.T.) ;
#20125 = EDGE_CURVE('',#15429,#15430,#8442,.T.) ;
#20126 = EDGE_CURVE('',#15430,#15424,#8443,.T.) ;
#20127 = EDGE_CURVE('',#15431,#15419,#8444,.T.) ;
#20128 = EDGE_CURVE('',#15428,#15431,#8445,.T.) ;
#20129 = EDGE_CURVE('',#15432,#15433,#8446,.T.) ;
#20130 = EDGE_CURVE('',#15433,#15434,#8447,.T.) ;
#20131 = EDGE_CURVE('',#15434,#15429,#8448,.T.) ;
#20132 = EDGE_CURVE('',#15431,#15432,#8449,.T.) ;
#20133 = EDGE_CURVE('',#15434,#15435,#8450,.T.) ;
#20134 = EDGE_CURVE('',#15436,#15435,#8451,.T.) ;
#20135 = EDGE_CURVE('',#15437,#15436,#8452,.T.) ;
#20136 = EDGE_CURVE('',#15437,#15430,#8453,.T.) ;
#20137 = EDGE_CURVE('',#15438,#15439,#8454,.T.) ;
#20138 = EDGE_CURVE('',#15439,#15440,#8455,.T.) ;
#20139 = EDGE_CURVE('',#15440,#15436,#8456,.T.) ;
#20140 = EDGE_CURVE('',#15435,#15441,#8457,.T.) ;
#20141 = EDGE_CURVE('',#15441,#15438,#8458,.T.) ;
#20142 = EDGE_CURVE('',#15440,#15442,#8459,.T.) ;
#20143 = EDGE_CURVE('',#15426,#15442,#8460,.T.) ;
#20144 = EDGE_CURVE('',#15425,#15437,#8461,.T.) ;
#20145 = EDGE_CURVE('',#15443,#15439,#8462,.T.) ;
#20146 = EDGE_CURVE('',#15442,#15443,#8463,.T.) ;
#20147 = EDGE_CURVE('',#15444,#15438,#8464,.T.) ;
#20148 = EDGE_CURVE('',#15444,#15445,#8465,.T.) ;
#20149 = EDGE_CURVE('',#15446,#15445,#8466,.T.) ;
#20150 = EDGE_CURVE('',#15443,#15446,#8467,.T.) ;
#20151 = EDGE_CURVE('',#15446,#15447,#8468,.T.) ;
#20152 = EDGE_CURVE('',#15447,#15427,#8469,.T.) ;
#20153 = EDGE_CURVE('',#15441,#15433,#8470,.T.) ;
#20154 = EDGE_CURVE('',#15448,#15448,#12609,.T.) ;
#20155 = EDGE_CURVE('',#15449,#15449,#12610,.T.) ;
#20156 = EDGE_CURVE('',#15450,#15450,#12611,.T.) ;
#20157 = EDGE_CURVE('',#15451,#15451,#12612,.T.) ;
#20158 = EDGE_CURVE('',#15452,#15452,#12613,.T.) ;
#20159 = EDGE_CURVE('',#15423,#15447,#8471,.T.) ;
#20160 = EDGE_CURVE('',#15453,#15453,#12614,.T.) ;
#20161 = EDGE_CURVE('',#15454,#15454,#12615,.T.) ;
#20162 = EDGE_CURVE('',#15455,#15455,#12616,.T.) ;
#20163 = EDGE_CURVE('',#15456,#15456,#12617,.T.) ;
#20164 = EDGE_CURVE('',#15457,#15457,#12618,.T.) ;
#20165 = EDGE_CURVE('',#15432,#15458,#8472,.T.) ;
#20166 = EDGE_CURVE('',#15458,#15444,#8473,.T.) ;
#20167 = EDGE_CURVE('',#15459,#15458,#8474,.T.) ;
#20168 = EDGE_CURVE('',#15445,#15459,#8475,.T.) ;
#20169 = EDGE_CURVE('',#15459,#15418,#8476,.T.) ;
#20170 = EDGE_CURVE('',#15452,#15457,#8477,.T.) ;
#20171 = EDGE_CURVE('',#15451,#15456,#8478,.T.) ;
#20172 = EDGE_CURVE('',#15450,#15455,#8479,.T.) ;
#20173 = EDGE_CURVE('',#15449,#15454,#8480,.T.) ;
#20174 = EDGE_CURVE('',#15448,#15453,#8481,.T.) ;
#20175 = EDGE_CURVE('',#15460,#15461,#8482,.T.) ;
#20176 = EDGE_CURVE('',#15462,#15460,#1630,.F.) ;
#20177 = EDGE_CURVE('',#15463,#15462,#12619,.T.) ;
#20178 = EDGE_CURVE('',#15463,#15461,#1631,.T.) ;
#20179 = EDGE_CURVE('',#15464,#15465,#8483,.T.) ;
#20180 = EDGE_CURVE('',#15460,#15464,#1632,.F.) ;
#20181 = EDGE_CURVE('',#15461,#15465,#1633,.T.) ;
#20182 = EDGE_CURVE('',#15466,#15467,#8484,.T.) ;
#20183 = EDGE_CURVE('',#15464,#15466,#1634,.F.) ;
#20184 = EDGE_CURVE('',#15465,#15467,#1635,.T.) ;
#20185 = EDGE_CURVE('',#15468,#15469,#8485,.T.) ;
#20186 = EDGE_CURVE('',#15466,#15468,#1636,.F.) ;
#20187 = EDGE_CURVE('',#15467,#15469,#1637,.T.) ;
#20188 = EDGE_CURVE('',#15470,#15471,#8486,.T.) ;
#20189 = EDGE_CURVE('',#15468,#15470,#1638,.F.) ;
#20190 = EDGE_CURVE('',#15469,#15471,#1639,.T.) ;
#20191 = EDGE_CURVE('',#15472,#15473,#8487,.T.) ;
#20192 = EDGE_CURVE('',#15470,#15472,#1640,.F.) ;
#20193 = EDGE_CURVE('',#15471,#15473,#1641,.T.) ;
#20194 = EDGE_CURVE('',#15474,#15475,#8488,.T.) ;
#20195 = EDGE_CURVE('',#15472,#15474,#1642,.F.) ;
#20196 = EDGE_CURVE('',#15473,#15475,#1643,.T.) ;
#20197 = EDGE_CURVE('',#15476,#15477,#8489,.T.) ;
#20198 = EDGE_CURVE('',#15474,#15476,#1644,.F.) ;
#20199 = EDGE_CURVE('',#15475,#15477,#1645,.T.) ;
#20200 = EDGE_CURVE('',#15478,#15479,#8490,.T.) ;
#20201 = EDGE_CURVE('',#15476,#15478,#1646,.F.) ;
#20202 = EDGE_CURVE('',#15477,#15479,#1647,.T.) ;
#20203 = EDGE_CURVE('',#15480,#15481,#8491,.T.) ;
#20204 = EDGE_CURVE('',#15478,#15480,#1648,.F.) ;
#20205 = EDGE_CURVE('',#15479,#15481,#1649,.T.) ;
#20206 = EDGE_CURVE('',#15482,#15483,#8492,.T.) ;
#20207 = EDGE_CURVE('',#15480,#15482,#1650,.F.) ;
#20208 = EDGE_CURVE('',#15481,#15483,#1651,.T.) ;
#20209 = EDGE_CURVE('',#15484,#15485,#8493,.T.) ;
#20210 = EDGE_CURVE('',#15482,#15484,#1652,.F.) ;
#20211 = EDGE_CURVE('',#15483,#15485,#1653,.T.) ;
#20212 = EDGE_CURVE('',#15486,#15487,#8494,.T.) ;
#20213 = EDGE_CURVE('',#15484,#15486,#1654,.F.) ;
#20214 = EDGE_CURVE('',#15485,#15487,#1655,.T.) ;
#20215 = EDGE_CURVE('',#15488,#15489,#8495,.T.) ;
#20216 = EDGE_CURVE('',#15486,#15488,#1656,.F.) ;
#20217 = EDGE_CURVE('',#15487,#15489,#1657,.T.) ;
#20218 = EDGE_CURVE('',#15490,#15491,#8496,.T.) ;
#20219 = EDGE_CURVE('',#15488,#15490,#1658,.F.) ;
#20220 = EDGE_CURVE('',#15489,#15491,#1659,.T.) ;
#20221 = EDGE_CURVE('',#15492,#15493,#8497,.T.) ;
#20222 = EDGE_CURVE('',#15494,#15492,#1660,.F.) ;
#20223 = EDGE_CURVE('',#15494,#15495,#12620,.T.) ;
#20224 = EDGE_CURVE('',#15496,#15495,#1661,.F.) ;
#20225 = EDGE_CURVE('',#15496,#15493,#1662,.T.) ;
#20226 = EDGE_CURVE('',#15497,#15498,#8498,.T.) ;
#20227 = EDGE_CURVE('',#15492,#15497,#1663,.F.) ;
#20228 = EDGE_CURVE('',#15493,#15498,#1664,.T.) ;
#20229 = EDGE_CURVE('',#15499,#15500,#8499,.T.) ;
#20230 = EDGE_CURVE('',#15497,#15499,#1665,.F.) ;
#20231 = EDGE_CURVE('',#15498,#15500,#1666,.T.) ;
#20232 = EDGE_CURVE('',#15501,#15502,#8500,.T.) ;
#20233 = EDGE_CURVE('',#15499,#15501,#1667,.F.) ;
#20234 = EDGE_CURVE('',#15500,#15502,#1668,.T.) ;
#20235 = EDGE_CURVE('',#15503,#15504,#8501,.T.) ;
#20236 = EDGE_CURVE('',#15501,#15503,#1669,.F.) ;
#20237 = EDGE_CURVE('',#15502,#15504,#1670,.T.) ;
#20238 = EDGE_CURVE('',#15505,#15506,#8502,.T.) ;
#20239 = EDGE_CURVE('',#15503,#15505,#1671,.F.) ;
#20240 = EDGE_CURVE('',#15504,#15506,#1672,.T.) ;
#20241 = EDGE_CURVE('',#15507,#15508,#8503,.T.) ;
#20242 = EDGE_CURVE('',#15505,#15507,#1673,.F.) ;
#20243 = EDGE_CURVE('',#15506,#15508,#1674,.T.) ;
#20244 = EDGE_CURVE('',#15509,#15510,#8504,.T.) ;
#20245 = EDGE_CURVE('',#15507,#15509,#1675,.F.) ;
#20246 = EDGE_CURVE('',#15508,#15510,#1676,.T.) ;
#20247 = EDGE_CURVE('',#15511,#15512,#8505,.T.) ;
#20248 = EDGE_CURVE('',#15509,#15511,#1677,.F.) ;
#20249 = EDGE_CURVE('',#15510,#15512,#1678,.T.) ;
#20250 = EDGE_CURVE('',#15513,#15514,#8506,.T.) ;
#20251 = EDGE_CURVE('',#15511,#15513,#1679,.F.) ;
#20252 = EDGE_CURVE('',#15512,#15514,#1680,.T.) ;
#20253 = EDGE_CURVE('',#15515,#15516,#8507,.T.) ;
#20254 = EDGE_CURVE('',#15513,#15515,#1681,.F.) ;
#20255 = EDGE_CURVE('',#15514,#15516,#1682,.T.) ;
#20256 = EDGE_CURVE('',#15517,#15518,#8508,.T.) ;
#20257 = EDGE_CURVE('',#15515,#15517,#1683,.F.) ;
#20258 = EDGE_CURVE('',#15516,#15518,#1684,.T.) ;
#20259 = EDGE_CURVE('',#15519,#15520,#8509,.T.) ;
#20260 = EDGE_CURVE('',#15517,#15519,#1685,.F.) ;
#20261 = EDGE_CURVE('',#15518,#15520,#1686,.T.) ;
#20262 = EDGE_CURVE('',#15521,#15522,#8510,.T.) ;
#20263 = EDGE_CURVE('',#15519,#15521,#1687,.F.) ;
#20264 = EDGE_CURVE('',#15520,#15522,#1688,.T.) ;
#20265 = EDGE_CURVE('',#15523,#15524,#8511,.T.) ;
#20266 = EDGE_CURVE('',#15521,#15523,#1689,.F.) ;
#20267 = EDGE_CURVE('',#15522,#15524,#1690,.T.) ;
#20268 = EDGE_CURVE('',#15525,#15526,#8512,.T.) ;
#20269 = EDGE_CURVE('',#15523,#15525,#1691,.F.) ;
#20270 = EDGE_CURVE('',#15524,#15526,#1692,.T.) ;
#20271 = EDGE_CURVE('',#15527,#15528,#8513,.T.) ;
#20272 = EDGE_CURVE('',#15527,#15529,#1693,.F.) ;
#20273 = EDGE_CURVE('',#15495,#15529,#1694,.F.) ;
#20274 = EDGE_CURVE('',#15495,#15528,#12621,.T.) ;
#20275 = EDGE_CURVE('',#15528,#15494,#12622,.T.) ;
#20276 = EDGE_CURVE('',#15494,#15463,#1695,.T.) ;
#20277 = EDGE_CURVE('',#15462,#15527,#1696,.F.) ;
#20278 = EDGE_CURVE('',#15526,#15530,#1697,.T.) ;
#20279 = EDGE_CURVE('',#15531,#15530,#12623,.T.) ;
#20280 = EDGE_CURVE('',#15525,#15531,#1698,.F.) ;
#20281 = EDGE_CURVE('',#15491,#15532,#1699,.T.) ;
#20282 = EDGE_CURVE('',#15533,#15532,#12624,.T.) ;
#20283 = EDGE_CURVE('',#15490,#15533,#1700,.F.) ;
#20284 = EDGE_CURVE('',#15534,#15535,#12625,.T.) ;
#20285 = EDGE_CURVE('',#15534,#15536,#805,.T.) ;
#20286 = EDGE_CURVE('',#15536,#15537,#12626,.T.) ;
#20287 = EDGE_CURVE('',#15535,#15537,#806,.T.) ;
#20288 = EDGE_CURVE('',#15538,#15539,#12627,.T.) ;
#20289 = EDGE_CURVE('',#15538,#15540,#807,.T.) ;
#20290 = EDGE_CURVE('',#15540,#15541,#12628,.T.) ;
#20291 = EDGE_CURVE('',#15539,#15541,#808,.T.) ;
#20292 = EDGE_CURVE('',#15542,#15542,#12629,.T.) ;
#20293 = EDGE_CURVE('',#15542,#15543,#12630,.T.) ;
#20294 = EDGE_CURVE('',#15543,#15544,#12631,.T.) ;
#20295 = EDGE_CURVE('',#15544,#15543,#12632,.T.) ;
#20296 = EDGE_CURVE('',#15545,#15546,#12633,.T.) ;
#20297 = EDGE_CURVE('',#15547,#15545,#12634,.T.) ;
#20298 = EDGE_CURVE('',#15548,#15547,#12635,.T.) ;
#20299 = EDGE_CURVE('',#15549,#15548,#12636,.T.) ;
#20300 = EDGE_CURVE('',#15541,#15549,#12637,.T.) ;
#20301 = EDGE_CURVE('',#15550,#15540,#12638,.T.) ;
#20302 = EDGE_CURVE('',#15551,#15550,#12639,.T.) ;
#20303 = EDGE_CURVE('',#15552,#15551,#12640,.T.) ;
#20304 = EDGE_CURVE('',#15537,#15552,#12641,.T.) ;
#20305 = EDGE_CURVE('',#15553,#15536,#12642,.T.) ;
#20306 = EDGE_CURVE('',#15554,#15553,#12643,.T.) ;
#20307 = EDGE_CURVE('',#15555,#15554,#12644,.T.) ;
#20308 = EDGE_CURVE('',#15556,#15555,#12645,.T.) ;
#20309 = EDGE_CURVE('',#15557,#15556,#12646,.T.) ;
#20310 = EDGE_CURVE('',#15558,#15557,#12647,.T.) ;
#20311 = EDGE_CURVE('',#15559,#15558,#12648,.T.) ;
#20312 = EDGE_CURVE('',#15560,#15559,#12649,.T.) ;
#20313 = EDGE_CURVE('',#15546,#15560,#12650,.T.) ;
#20314 = EDGE_CURVE('',#15561,#15562,#12651,.T.) ;
#20315 = EDGE_CURVE('',#15562,#15544,#8514,.T.) ;
#20316 = EDGE_CURVE('',#15562,#15561,#12652,.T.) ;
#20317 = EDGE_CURVE('',#15561,#15563,#12653,.T.) ;
#20318 = EDGE_CURVE('',#15563,#15563,#12654,.T.) ;
#20319 = EDGE_CURVE('',#15532,#15531,#1701,.T.) ;
#20320 = EDGE_CURVE('',#15530,#15533,#1702,.T.) ;
#20321 = EDGE_CURVE('',#15529,#15496,#8515,.T.) ;
#20322 = EDGE_CURVE('',#15564,#15546,#809,.T.) ;
#20323 = EDGE_CURVE('',#15565,#15564,#12655,.T.) ;
#20324 = EDGE_CURVE('',#15565,#15545,#810,.T.) ;
#20325 = EDGE_CURVE('',#15566,#15565,#8516,.T.) ;
#20326 = EDGE_CURVE('',#15566,#15547,#8517,.T.) ;
#20327 = EDGE_CURVE('',#15567,#15566,#8518,.T.) ;
#20328 = EDGE_CURVE('',#15567,#15548,#8519,.T.) ;
#20329 = EDGE_CURVE('',#15568,#15567,#8520,.T.) ;
#20330 = EDGE_CURVE('',#15568,#15549,#8521,.T.) ;
#20331 = EDGE_CURVE('',#15539,#15568,#8522,.T.) ;
#20332 = EDGE_CURVE('',#15569,#15538,#8523,.T.) ;
#20333 = EDGE_CURVE('',#15564,#15570,#8524,.T.) ;
#20334 = EDGE_CURVE('',#15570,#15571,#8525,.T.) ;
#20335 = EDGE_CURVE('',#15571,#15572,#8526,.T.) ;
#20336 = EDGE_CURVE('',#15572,#15573,#8527,.T.) ;
#20337 = EDGE_CURVE('',#15573,#15574,#12656,.T.) ;
#20338 = EDGE_CURVE('',#15574,#15575,#8528,.T.) ;
#20339 = EDGE_CURVE('',#15575,#15576,#8529,.T.) ;
#20340 = EDGE_CURVE('',#15576,#15577,#8530,.T.) ;
#20341 = EDGE_CURVE('',#15577,#15534,#8531,.T.) ;
#20342 = EDGE_CURVE('',#15535,#15578,#8532,.T.) ;
#20343 = EDGE_CURVE('',#15578,#15579,#8533,.T.) ;
#20344 = EDGE_CURVE('',#15579,#15569,#8534,.T.) ;
#20345 = EDGE_CURVE('',#15569,#15550,#8535,.T.) ;
#20346 = EDGE_CURVE('',#15579,#15551,#8536,.T.) ;
#20347 = EDGE_CURVE('',#15578,#15552,#8537,.T.) ;
#20348 = EDGE_CURVE('',#15577,#15553,#8538,.T.) ;
#20349 = EDGE_CURVE('',#15576,#15554,#8539,.T.) ;
#20350 = EDGE_CURVE('',#15575,#15555,#8540,.T.) ;
#20351 = EDGE_CURVE('',#15574,#15556,#811,.T.) ;
#20352 = EDGE_CURVE('',#15573,#15557,#812,.T.) ;
#20353 = EDGE_CURVE('',#15572,#15558,#8541,.T.) ;
#20354 = EDGE_CURVE('',#15571,#15559,#8542,.T.) ;
#20355 = EDGE_CURVE('',#15570,#15560,#8543,.T.) ;
#20356 = EDGE_CURVE('',#15580,#15581,#8544,.T.) ;
#20357 = EDGE_CURVE('',#15581,#15582,#8545,.T.) ;
#20358 = EDGE_CURVE('',#15582,#15583,#8546,.T.) ;
#20359 = EDGE_CURVE('',#15583,#15580,#8547,.T.) ;
#20360 = EDGE_CURVE('',#15584,#15585,#8548,.T.) ;
#20361 = EDGE_CURVE('',#15585,#15586,#8549,.T.) ;
#20362 = EDGE_CURVE('',#15586,#15587,#8550,.T.) ;
#20363 = EDGE_CURVE('',#15587,#15584,#8551,.T.) ;
#20364 = EDGE_CURVE('',#15580,#15585,#1703,.T.) ;
#20365 = EDGE_CURVE('',#15581,#15584,#1704,.T.) ;
#20366 = EDGE_CURVE('',#15583,#15586,#1705,.T.) ;
#20367 = EDGE_CURVE('',#15582,#15587,#813,.T.) ;
#20368 = EDGE_CURVE('',#15588,#15588,#12657,.T.) ;
#20369 = EDGE_CURVE('',#15588,#15589,#12658,.T.) ;
#20370 = EDGE_CURVE('',#15589,#15590,#12659,.T.) ;
#20371 = EDGE_CURVE('',#15590,#15589,#12660,.T.) ;
#20372 = EDGE_CURVE('',#15591,#15592,#12661,.T.) ;
#20373 = EDGE_CURVE('',#15592,#15591,#12662,.T.) ;
#20374 = EDGE_CURVE('',#15592,#15590,#8552,.T.) ;
#20375 = EDGE_CURVE('',#15593,#15593,#12663,.T.) ;
#20376 = EDGE_CURVE('',#15591,#15594,#12664,.T.) ;
#20377 = EDGE_CURVE('',#15594,#15594,#12665,.T.) ;
#20378 = EDGE_CURVE('',#15595,#15595,#12666,.T.) ;
#20379 = EDGE_CURVE('',#15593,#15595,#8553,.T.) ;
#20380 = ORIENTED_EDGE('',*,*,#15596,.T.) ;
#20381 = ORIENTED_EDGE('',*,*,#15597,.T.) ;
#20382 = ORIENTED_EDGE('',*,*,#15598,.T.) ;
#20383 = ORIENTED_EDGE('',*,*,#15599,.T.) ;
#20384 = ORIENTED_EDGE('',*,*,#15597,.F.) ;
#20385 = ORIENTED_EDGE('',*,*,#15600,.F.) ;
#20386 = ORIENTED_EDGE('',*,*,#15601,.F.) ;
#20387 = ORIENTED_EDGE('',*,*,#15602,.T.) ;
#20388 = ORIENTED_EDGE('',*,*,#15603,.F.) ;
#20389 = ORIENTED_EDGE('',*,*,#15604,.T.) ;
#20390 = ORIENTED_EDGE('',*,*,#15605,.T.) ;
#20391 = ORIENTED_EDGE('',*,*,#15606,.F.) ;
#20392 = ORIENTED_EDGE('',*,*,#15607,.T.) ;
#20393 = ORIENTED_EDGE('',*,*,#15608,.F.) ;
#20394 = ORIENTED_EDGE('',*,*,#15609,.F.) ;
#20395 = ORIENTED_EDGE('',*,*,#15610,.T.) ;
#20396 = ORIENTED_EDGE('',*,*,#15611,.F.) ;
#20397 = ORIENTED_EDGE('',*,*,#15612,.T.) ;
#20398 = ORIENTED_EDGE('',*,*,#15613,.F.) ;
#20399 = ORIENTED_EDGE('',*,*,#15614,.T.) ;
#20400 = ORIENTED_EDGE('',*,*,#15615,.F.) ;
#20401 = ORIENTED_EDGE('',*,*,#15616,.T.) ;
#20402 = ORIENTED_EDGE('',*,*,#15617,.T.) ;
#20403 = ORIENTED_EDGE('',*,*,#15618,.F.) ;
#20404 = ORIENTED_EDGE('',*,*,#15619,.T.) ;
#20405 = ORIENTED_EDGE('',*,*,#15620,.F.) ;
#20406 = ORIENTED_EDGE('',*,*,#15621,.F.) ;
#20407 = ORIENTED_EDGE('',*,*,#15622,.T.) ;
#20408 = ORIENTED_EDGE('',*,*,#15623,.F.) ;
#20409 = ORIENTED_EDGE('',*,*,#15624,.T.) ;
#20410 = ORIENTED_EDGE('',*,*,#15625,.F.) ;
#20411 = ORIENTED_EDGE('',*,*,#15626,.T.) ;
#20412 = ORIENTED_EDGE('',*,*,#15627,.F.) ;
#20413 = ORIENTED_EDGE('',*,*,#15628,.T.) ;
#20414 = ORIENTED_EDGE('',*,*,#15629,.F.) ;
#20415 = ORIENTED_EDGE('',*,*,#15630,.T.) ;
#20416 = ORIENTED_EDGE('',*,*,#15631,.F.) ;
#20417 = ORIENTED_EDGE('',*,*,#15632,.T.) ;
#20418 = ORIENTED_EDGE('',*,*,#15633,.F.) ;
#20419 = ORIENTED_EDGE('',*,*,#15634,.T.) ;
#20420 = ORIENTED_EDGE('',*,*,#15635,.F.) ;
#20421 = ORIENTED_EDGE('',*,*,#15636,.T.) ;
#20422 = ORIENTED_EDGE('',*,*,#15637,.F.) ;
#20423 = ORIENTED_EDGE('',*,*,#15638,.T.) ;
#20424 = ORIENTED_EDGE('',*,*,#15639,.F.) ;
#20425 = ORIENTED_EDGE('',*,*,#15640,.T.) ;
#20426 = ORIENTED_EDGE('',*,*,#15641,.F.) ;
#20427 = ORIENTED_EDGE('',*,*,#15642,.T.) ;
#20428 = ORIENTED_EDGE('',*,*,#15643,.F.) ;
#20429 = ORIENTED_EDGE('',*,*,#15644,.T.) ;
#20430 = ORIENTED_EDGE('',*,*,#15645,.T.) ;
#20431 = ORIENTED_EDGE('',*,*,#15646,.T.) ;
#20432 = ORIENTED_EDGE('',*,*,#15647,.T.) ;
#20433 = ORIENTED_EDGE('',*,*,#15648,.T.) ;
#20434 = ORIENTED_EDGE('',*,*,#15649,.T.) ;
#20435 = ORIENTED_EDGE('',*,*,#15650,.T.) ;
#20436 = ORIENTED_EDGE('',*,*,#15651,.F.) ;
#20437 = ORIENTED_EDGE('',*,*,#15652,.T.) ;
#20438 = ORIENTED_EDGE('',*,*,#15653,.F.) ;
#20439 = ORIENTED_EDGE('',*,*,#15654,.T.) ;
#20440 = ORIENTED_EDGE('',*,*,#15655,.F.) ;
#20441 = ORIENTED_EDGE('',*,*,#15656,.T.) ;
#20442 = ORIENTED_EDGE('',*,*,#15657,.F.) ;
#20443 = ORIENTED_EDGE('',*,*,#15658,.T.) ;
#20444 = ORIENTED_EDGE('',*,*,#15659,.F.) ;
#20445 = ORIENTED_EDGE('',*,*,#15660,.T.) ;
#20446 = ORIENTED_EDGE('',*,*,#15661,.F.) ;
#20447 = ORIENTED_EDGE('',*,*,#15662,.T.) ;
#20448 = ORIENTED_EDGE('',*,*,#15663,.T.) ;
#20449 = ORIENTED_EDGE('',*,*,#15664,.F.) ;
#20450 = ORIENTED_EDGE('',*,*,#15665,.T.) ;
#20451 = ORIENTED_EDGE('',*,*,#15666,.F.) ;
#20452 = ORIENTED_EDGE('',*,*,#15667,.T.) ;
#20453 = ORIENTED_EDGE('',*,*,#15603,.T.) ;
#20454 = ORIENTED_EDGE('',*,*,#15668,.T.) ;
#20455 = ORIENTED_EDGE('',*,*,#15669,.T.) ;
#20456 = ORIENTED_EDGE('',*,*,#15670,.T.) ;
#20457 = ORIENTED_EDGE('',*,*,#15671,.T.) ;
#20458 = ORIENTED_EDGE('',*,*,#15672,.T.) ;
#20459 = ORIENTED_EDGE('',*,*,#15601,.T.) ;
#20460 = ORIENTED_EDGE('',*,*,#15671,.F.) ;
#20461 = ORIENTED_EDGE('',*,*,#15673,.T.) ;
#20462 = ORIENTED_EDGE('',*,*,#15674,.F.) ;
#20463 = ORIENTED_EDGE('',*,*,#15675,.T.) ;
#20464 = ORIENTED_EDGE('',*,*,#15676,.F.) ;
#20465 = ORIENTED_EDGE('',*,*,#15677,.T.) ;
#20466 = ORIENTED_EDGE('',*,*,#15678,.F.) ;
#20467 = ORIENTED_EDGE('',*,*,#15679,.F.) ;
#20468 = ORIENTED_EDGE('',*,*,#15680,.F.) ;
#20469 = ORIENTED_EDGE('',*,*,#15681,.T.) ;
#20470 = ORIENTED_EDGE('',*,*,#15682,.F.) ;
#20471 = ORIENTED_EDGE('',*,*,#15683,.T.) ;
#20472 = ORIENTED_EDGE('',*,*,#15684,.F.) ;
#20473 = ORIENTED_EDGE('',*,*,#15685,.T.) ;
#20474 = ORIENTED_EDGE('',*,*,#15686,.F.) ;
#20475 = ORIENTED_EDGE('',*,*,#15687,.F.) ;
#20476 = ORIENTED_EDGE('',*,*,#15688,.F.) ;
#20477 = ORIENTED_EDGE('',*,*,#15689,.T.) ;
#20478 = ORIENTED_EDGE('',*,*,#15690,.T.) ;
#20479 = ORIENTED_EDGE('',*,*,#15691,.T.) ;
#20480 = ORIENTED_EDGE('',*,*,#15692,.T.) ;
#20481 = ORIENTED_EDGE('',*,*,#15693,.T.) ;
#20482 = ORIENTED_EDGE('',*,*,#15694,.T.) ;
#20483 = ORIENTED_EDGE('',*,*,#15695,.T.) ;
#20484 = ORIENTED_EDGE('',*,*,#15692,.F.) ;
#20485 = ORIENTED_EDGE('',*,*,#15696,.F.) ;
#20486 = ORIENTED_EDGE('',*,*,#15697,.F.) ;
#20487 = ORIENTED_EDGE('',*,*,#15698,.F.) ;
#20488 = ORIENTED_EDGE('',*,*,#15598,.F.) ;
#20489 = ORIENTED_EDGE('',*,*,#15604,.F.) ;
#20490 = ORIENTED_EDGE('',*,*,#15699,.F.) ;
#20491 = ORIENTED_EDGE('',*,*,#15700,.F.) ;
#20492 = ORIENTED_EDGE('',*,*,#15695,.F.) ;
#20493 = ORIENTED_EDGE('',*,*,#15701,.T.) ;
#20494 = ORIENTED_EDGE('',*,*,#15702,.F.) ;
#20495 = ORIENTED_EDGE('',*,*,#15703,.F.) ;
#20496 = ORIENTED_EDGE('',*,*,#15704,.F.) ;
#20497 = ORIENTED_EDGE('',*,*,#15705,.F.) ;
#20498 = ORIENTED_EDGE('',*,*,#15706,.F.) ;
#20499 = ORIENTED_EDGE('',*,*,#15707,.F.) ;
#20500 = ORIENTED_EDGE('',*,*,#15708,.F.) ;
#20501 = ORIENTED_EDGE('',*,*,#15709,.F.) ;
#20502 = ORIENTED_EDGE('',*,*,#15710,.F.) ;
#20503 = ORIENTED_EDGE('',*,*,#15711,.F.) ;
#20504 = ORIENTED_EDGE('',*,*,#15712,.F.) ;
#20505 = ORIENTED_EDGE('',*,*,#15713,.T.) ;
#20506 = ORIENTED_EDGE('',*,*,#15714,.F.) ;
#20507 = ORIENTED_EDGE('',*,*,#15715,.F.) ;
#20508 = ORIENTED_EDGE('',*,*,#15716,.F.) ;
#20509 = ORIENTED_EDGE('',*,*,#15696,.T.) ;
#20510 = ORIENTED_EDGE('',*,*,#15717,.F.) ;
#20511 = ORIENTED_EDGE('',*,*,#15718,.T.) ;
#20512 = ORIENTED_EDGE('',*,*,#15719,.T.) ;
#20513 = ORIENTED_EDGE('',*,*,#15720,.T.) ;
#20514 = ORIENTED_EDGE('',*,*,#15721,.T.) ;
#20515 = ORIENTED_EDGE('',*,*,#15722,.T.) ;
#20516 = ORIENTED_EDGE('',*,*,#15719,.F.) ;
#20517 = ORIENTED_EDGE('',*,*,#15723,.F.) ;
#20518 = ORIENTED_EDGE('',*,*,#15724,.F.) ;
#20519 = ORIENTED_EDGE('',*,*,#15673,.F.) ;
#20520 = ORIENTED_EDGE('',*,*,#15670,.F.) ;
#20521 = ORIENTED_EDGE('',*,*,#15725,.F.) ;
#20522 = ORIENTED_EDGE('',*,*,#15726,.F.) ;
#20523 = ORIENTED_EDGE('',*,*,#15722,.F.) ;
#20524 = ORIENTED_EDGE('',*,*,#15727,.F.) ;
#20525 = ORIENTED_EDGE('',*,*,#15728,.F.) ;
#20526 = ORIENTED_EDGE('',*,*,#15729,.F.) ;
#20527 = ORIENTED_EDGE('',*,*,#15730,.F.) ;
#20528 = ORIENTED_EDGE('',*,*,#15731,.T.) ;
#20529 = ORIENTED_EDGE('',*,*,#15732,.F.) ;
#20530 = ORIENTED_EDGE('',*,*,#15733,.T.) ;
#20531 = ORIENTED_EDGE('',*,*,#15734,.F.) ;
#20532 = ORIENTED_EDGE('',*,*,#15735,.T.) ;
#20533 = ORIENTED_EDGE('',*,*,#15736,.F.) ;
#20534 = ORIENTED_EDGE('',*,*,#15737,.F.) ;
#20535 = ORIENTED_EDGE('',*,*,#15738,.F.) ;
#20536 = ORIENTED_EDGE('',*,*,#15739,.T.) ;
#20537 = ORIENTED_EDGE('',*,*,#15740,.F.) ;
#20538 = ORIENTED_EDGE('',*,*,#15741,.T.) ;
#20539 = ORIENTED_EDGE('',*,*,#15742,.F.) ;
#20540 = ORIENTED_EDGE('',*,*,#15723,.T.) ;
#20541 = ORIENTED_EDGE('',*,*,#15743,.T.) ;
#20542 = ORIENTED_EDGE('',*,*,#15744,.T.) ;
#20543 = ORIENTED_EDGE('',*,*,#15704,.T.) ;
#20544 = ORIENTED_EDGE('',*,*,#15745,.T.) ;
#20545 = ORIENTED_EDGE('',*,*,#15746,.T.) ;
#20546 = ORIENTED_EDGE('',*,*,#15747,.T.) ;
#20547 = ORIENTED_EDGE('',*,*,#15745,.F.) ;
#20548 = ORIENTED_EDGE('',*,*,#15703,.T.) ;
#20549 = ORIENTED_EDGE('',*,*,#15748,.F.) ;
#20550 = ORIENTED_EDGE('',*,*,#15749,.F.) ;
#20551 = ORIENTED_EDGE('',*,*,#15676,.T.) ;
#20552 = ORIENTED_EDGE('',*,*,#15750,.T.) ;
#20553 = ORIENTED_EDGE('',*,*,#15740,.T.) ;
#20554 = ORIENTED_EDGE('',*,*,#15751,.T.) ;
#20555 = ORIENTED_EDGE('',*,*,#15750,.F.) ;
#20556 = ORIENTED_EDGE('',*,*,#15675,.F.) ;
#20557 = ORIENTED_EDGE('',*,*,#15752,.F.) ;
#20558 = ORIENTED_EDGE('',*,*,#15741,.F.) ;
#20559 = ORIENTED_EDGE('',*,*,#15753,.T.) ;
#20560 = ORIENTED_EDGE('',*,*,#15754,.T.) ;
#20561 = ORIENTED_EDGE('',*,*,#15755,.T.) ;
#20562 = ORIENTED_EDGE('',*,*,#15756,.T.) ;
#20563 = ORIENTED_EDGE('',*,*,#15755,.F.) ;
#20564 = ORIENTED_EDGE('',*,*,#15757,.T.) ;
#20565 = ORIENTED_EDGE('',*,*,#15699,.T.) ;
#20566 = ORIENTED_EDGE('',*,*,#15667,.F.) ;
#20567 = ORIENTED_EDGE('',*,*,#15758,.F.) ;
#20568 = ORIENTED_EDGE('',*,*,#15759,.F.) ;
#20569 = ORIENTED_EDGE('',*,*,#15760,.F.) ;
#20570 = ORIENTED_EDGE('',*,*,#15693,.F.) ;
#20571 = ORIENTED_EDGE('',*,*,#15700,.T.) ;
#20572 = ORIENTED_EDGE('',*,*,#15757,.F.) ;
#20573 = ORIENTED_EDGE('',*,*,#15754,.F.) ;
#20574 = ORIENTED_EDGE('',*,*,#15761,.F.) ;
#20575 = ORIENTED_EDGE('',*,*,#15762,.F.) ;
#20576 = ORIENTED_EDGE('',*,*,#15720,.F.) ;
#20577 = ORIENTED_EDGE('',*,*,#15726,.T.) ;
#20578 = ORIENTED_EDGE('',*,*,#15763,.F.) ;
#20579 = ORIENTED_EDGE('',*,*,#15764,.F.) ;
#20580 = ORIENTED_EDGE('',*,*,#15765,.F.) ;
#20581 = ORIENTED_EDGE('',*,*,#15766,.F.) ;
#20582 = ORIENTED_EDGE('',*,*,#15767,.T.) ;
#20583 = ORIENTED_EDGE('',*,*,#15768,.F.) ;
#20584 = ORIENTED_EDGE('',*,*,#15769,.F.) ;
#20585 = ORIENTED_EDGE('',*,*,#15770,.F.) ;
#20586 = ORIENTED_EDGE('',*,*,#15771,.T.) ;
#20587 = ORIENTED_EDGE('',*,*,#15772,.T.) ;
#20588 = ORIENTED_EDGE('',*,*,#15773,.T.) ;
#20589 = ORIENTED_EDGE('',*,*,#15774,.F.) ;
#20590 = ORIENTED_EDGE('',*,*,#15775,.T.) ;
#20591 = ORIENTED_EDGE('',*,*,#15776,.F.) ;
#20592 = ORIENTED_EDGE('',*,*,#15777,.T.) ;
#20593 = ORIENTED_EDGE('',*,*,#15778,.F.) ;
#20594 = ORIENTED_EDGE('',*,*,#15779,.T.) ;
#20595 = ORIENTED_EDGE('',*,*,#15780,.F.) ;
#20596 = ORIENTED_EDGE('',*,*,#15781,.T.) ;
#20597 = ORIENTED_EDGE('',*,*,#15782,.F.) ;
#20598 = ORIENTED_EDGE('',*,*,#15783,.T.) ;
#20599 = ORIENTED_EDGE('',*,*,#15784,.F.) ;
#20600 = ORIENTED_EDGE('',*,*,#15785,.T.) ;
#20601 = ORIENTED_EDGE('',*,*,#15786,.F.) ;
#20602 = ORIENTED_EDGE('',*,*,#15787,.T.) ;
#20603 = ORIENTED_EDGE('',*,*,#15788,.F.) ;
#20604 = ORIENTED_EDGE('',*,*,#15789,.T.) ;
#20605 = ORIENTED_EDGE('',*,*,#15790,.F.) ;
#20606 = ORIENTED_EDGE('',*,*,#15791,.T.) ;
#20607 = ORIENTED_EDGE('',*,*,#15792,.F.) ;
#20608 = ORIENTED_EDGE('',*,*,#15793,.T.) ;
#20609 = ORIENTED_EDGE('',*,*,#15794,.F.) ;
#20610 = ORIENTED_EDGE('',*,*,#15795,.T.) ;
#20611 = ORIENTED_EDGE('',*,*,#15796,.F.) ;
#20612 = ORIENTED_EDGE('',*,*,#15797,.T.) ;
#20613 = ORIENTED_EDGE('',*,*,#15798,.T.) ;
#20614 = ORIENTED_EDGE('',*,*,#15799,.T.) ;
#20615 = ORIENTED_EDGE('',*,*,#15800,.T.) ;
#20616 = ORIENTED_EDGE('',*,*,#15801,.T.) ;
#20617 = ORIENTED_EDGE('',*,*,#15802,.F.) ;
#20618 = ORIENTED_EDGE('',*,*,#15803,.T.) ;
#20619 = ORIENTED_EDGE('',*,*,#15804,.F.) ;
#20620 = ORIENTED_EDGE('',*,*,#15805,.F.) ;
#20621 = ORIENTED_EDGE('',*,*,#15806,.T.) ;
#20622 = ORIENTED_EDGE('',*,*,#15807,.F.) ;
#20623 = ORIENTED_EDGE('',*,*,#15808,.T.) ;
#20624 = ORIENTED_EDGE('',*,*,#15809,.F.) ;
#20625 = ORIENTED_EDGE('',*,*,#15810,.T.) ;
#20626 = ORIENTED_EDGE('',*,*,#15811,.F.) ;
#20627 = ORIENTED_EDGE('',*,*,#15812,.T.) ;
#20628 = ORIENTED_EDGE('',*,*,#15813,.F.) ;
#20629 = ORIENTED_EDGE('',*,*,#15814,.T.) ;
#20630 = ORIENTED_EDGE('',*,*,#15815,.F.) ;
#20631 = ORIENTED_EDGE('',*,*,#15816,.T.) ;
#20632 = ORIENTED_EDGE('',*,*,#15817,.T.) ;
#20633 = ORIENTED_EDGE('',*,*,#15818,.F.) ;
#20634 = ORIENTED_EDGE('',*,*,#15819,.F.) ;
#20635 = ORIENTED_EDGE('',*,*,#15820,.F.) ;
#20636 = ORIENTED_EDGE('',*,*,#15821,.T.) ;
#20637 = ORIENTED_EDGE('',*,*,#15822,.F.) ;
#20638 = ORIENTED_EDGE('',*,*,#15823,.F.) ;
#20639 = ORIENTED_EDGE('',*,*,#15824,.F.) ;
#20640 = ORIENTED_EDGE('',*,*,#15825,.T.) ;
#20641 = ORIENTED_EDGE('',*,*,#15826,.F.) ;
#20642 = ORIENTED_EDGE('',*,*,#15827,.F.) ;
#20643 = ORIENTED_EDGE('',*,*,#15828,.F.) ;
#20644 = ORIENTED_EDGE('',*,*,#15599,.F.) ;
#20645 = ORIENTED_EDGE('',*,*,#15698,.T.) ;
#20646 = ORIENTED_EDGE('',*,*,#15829,.F.) ;
#20647 = ORIENTED_EDGE('',*,*,#15830,.F.) ;
#20648 = ORIENTED_EDGE('',*,*,#15831,.F.) ;
#20649 = ORIENTED_EDGE('',*,*,#15832,.T.) ;
#20650 = ORIENTED_EDGE('',*,*,#15833,.F.) ;
#20651 = ORIENTED_EDGE('',*,*,#15834,.T.) ;
#20652 = ORIENTED_EDGE('',*,*,#15835,.F.) ;
#20653 = ORIENTED_EDGE('',*,*,#15836,.T.) ;
#20654 = ORIENTED_EDGE('',*,*,#15837,.F.) ;
#20655 = ORIENTED_EDGE('',*,*,#15838,.T.) ;
#20656 = ORIENTED_EDGE('',*,*,#15839,.F.) ;
#20657 = ORIENTED_EDGE('',*,*,#15840,.T.) ;
#20658 = ORIENTED_EDGE('',*,*,#15746,.F.) ;
#20659 = ORIENTED_EDGE('',*,*,#15749,.T.) ;
#20660 = ORIENTED_EDGE('',*,*,#15841,.F.) ;
#20661 = ORIENTED_EDGE('',*,*,#15842,.T.) ;
#20662 = ORIENTED_EDGE('',*,*,#15843,.F.) ;
#20663 = ORIENTED_EDGE('',*,*,#15844,.T.) ;
#20664 = ORIENTED_EDGE('',*,*,#15669,.F.) ;
#20665 = ORIENTED_EDGE('',*,*,#15845,.T.) ;
#20666 = ORIENTED_EDGE('',*,*,#15846,.F.) ;
#20667 = ORIENTED_EDGE('',*,*,#15847,.T.) ;
#20668 = ORIENTED_EDGE('',*,*,#15848,.F.) ;
#20669 = ORIENTED_EDGE('',*,*,#15758,.T.) ;
#20670 = ORIENTED_EDGE('',*,*,#15666,.T.) ;
#20671 = ORIENTED_EDGE('',*,*,#15849,.T.) ;
#20672 = ORIENTED_EDGE('',*,*,#15768,.T.) ;
#20673 = ORIENTED_EDGE('',*,*,#15850,.F.) ;
#20674 = ORIENTED_EDGE('',*,*,#15849,.F.) ;
#20675 = ORIENTED_EDGE('',*,*,#15665,.F.) ;
#20676 = ORIENTED_EDGE('',*,*,#15851,.F.) ;
#20677 = ORIENTED_EDGE('',*,*,#15769,.T.) ;
#20678 = ORIENTED_EDGE('',*,*,#15820,.T.) ;
#20679 = ORIENTED_EDGE('',*,*,#15852,.T.) ;
#20680 = ORIENTED_EDGE('',*,*,#15613,.T.) ;
#20681 = ORIENTED_EDGE('',*,*,#15853,.T.) ;
#20682 = ORIENTED_EDGE('',*,*,#15852,.F.) ;
#20683 = ORIENTED_EDGE('',*,*,#15819,.T.) ;
#20684 = ORIENTED_EDGE('',*,*,#15854,.F.) ;
#20685 = ORIENTED_EDGE('',*,*,#15614,.F.) ;
#20686 = ORIENTED_EDGE('',*,*,#15615,.T.) ;
#20687 = ORIENTED_EDGE('',*,*,#15854,.T.) ;
#20688 = ORIENTED_EDGE('',*,*,#15818,.T.) ;
#20689 = ORIENTED_EDGE('',*,*,#15855,.F.) ;
#20690 = ORIENTED_EDGE('',*,*,#15824,.T.) ;
#20691 = ORIENTED_EDGE('',*,*,#15856,.T.) ;
#20692 = ORIENTED_EDGE('',*,*,#15609,.T.) ;
#20693 = ORIENTED_EDGE('',*,*,#15857,.T.) ;
#20694 = ORIENTED_EDGE('',*,*,#15856,.F.) ;
#20695 = ORIENTED_EDGE('',*,*,#15823,.T.) ;
#20696 = ORIENTED_EDGE('',*,*,#15858,.F.) ;
#20697 = ORIENTED_EDGE('',*,*,#15610,.F.) ;
#20698 = ORIENTED_EDGE('',*,*,#15611,.T.) ;
#20699 = ORIENTED_EDGE('',*,*,#15858,.T.) ;
#20700 = ORIENTED_EDGE('',*,*,#15822,.T.) ;
#20701 = ORIENTED_EDGE('',*,*,#15859,.F.) ;
#20702 = ORIENTED_EDGE('',*,*,#15828,.T.) ;
#20703 = ORIENTED_EDGE('',*,*,#15860,.T.) ;
#20704 = ORIENTED_EDGE('',*,*,#15606,.T.) ;
#20705 = ORIENTED_EDGE('',*,*,#15861,.T.) ;
#20706 = ORIENTED_EDGE('',*,*,#15860,.F.) ;
#20707 = ORIENTED_EDGE('',*,*,#15827,.T.) ;
#20708 = ORIENTED_EDGE('',*,*,#15862,.F.) ;
#20709 = ORIENTED_EDGE('',*,*,#15607,.F.) ;
#20710 = ORIENTED_EDGE('',*,*,#15608,.T.) ;
#20711 = ORIENTED_EDGE('',*,*,#15862,.T.) ;
#20712 = ORIENTED_EDGE('',*,*,#15826,.T.) ;
#20713 = ORIENTED_EDGE('',*,*,#15863,.F.) ;
#20714 = ORIENTED_EDGE('',*,*,#15770,.T.) ;
#20715 = ORIENTED_EDGE('',*,*,#15851,.T.) ;
#20716 = ORIENTED_EDGE('',*,*,#15664,.T.) ;
#20717 = ORIENTED_EDGE('',*,*,#15864,.T.) ;
#20718 = ORIENTED_EDGE('',*,*,#15848,.T.) ;
#20719 = ORIENTED_EDGE('',*,*,#15865,.T.) ;
#20720 = ORIENTED_EDGE('',*,*,#15866,.T.) ;
#20721 = ORIENTED_EDGE('',*,*,#15759,.T.) ;
#20722 = ORIENTED_EDGE('',*,*,#15865,.F.) ;
#20723 = ORIENTED_EDGE('',*,*,#15847,.F.) ;
#20724 = ORIENTED_EDGE('',*,*,#15867,.F.) ;
#20725 = ORIENTED_EDGE('',*,*,#15868,.F.) ;
#20726 = ORIENTED_EDGE('',*,*,#15846,.T.) ;
#20727 = ORIENTED_EDGE('',*,*,#15869,.T.) ;
#20728 = ORIENTED_EDGE('',*,*,#15870,.T.) ;
#20729 = ORIENTED_EDGE('',*,*,#15867,.T.) ;
#20730 = ORIENTED_EDGE('',*,*,#15753,.F.) ;
#20731 = ORIENTED_EDGE('',*,*,#15871,.T.) ;
#20732 = ORIENTED_EDGE('',*,*,#15869,.F.) ;
#20733 = ORIENTED_EDGE('',*,*,#15845,.F.) ;
#20734 = ORIENTED_EDGE('',*,*,#15668,.F.) ;
#20735 = ORIENTED_EDGE('',*,*,#15872,.F.) ;
#20736 = ORIENTED_EDGE('',*,*,#15761,.T.) ;
#20737 = ORIENTED_EDGE('',*,*,#15674,.T.) ;
#20738 = ORIENTED_EDGE('',*,*,#15724,.T.) ;
#20739 = ORIENTED_EDGE('',*,*,#15742,.T.) ;
#20740 = ORIENTED_EDGE('',*,*,#15752,.T.) ;
#20741 = ORIENTED_EDGE('',*,*,#15873,.T.) ;
#20742 = ORIENTED_EDGE('',*,*,#15874,.T.) ;
#20743 = ORIENTED_EDGE('',*,*,#15875,.T.) ;
#20744 = ORIENTED_EDGE('',*,*,#15876,.T.) ;
#20745 = ORIENTED_EDGE('',*,*,#15874,.F.) ;
#20746 = ORIENTED_EDGE('',*,*,#15877,.T.) ;
#20747 = ORIENTED_EDGE('',*,*,#15878,.F.) ;
#20748 = ORIENTED_EDGE('',*,*,#15879,.T.) ;
#20749 = ORIENTED_EDGE('',*,*,#15873,.F.) ;
#20750 = ORIENTED_EDGE('',*,*,#15880,.T.) ;
#20751 = ORIENTED_EDGE('',*,*,#15881,.F.) ;
#20752 = ORIENTED_EDGE('',*,*,#15882,.T.) ;
#20753 = ORIENTED_EDGE('',*,*,#15883,.F.) ;
#20754 = ORIENTED_EDGE('',*,*,#15877,.F.) ;
#20755 = ORIENTED_EDGE('',*,*,#15884,.T.) ;
#20756 = ORIENTED_EDGE('',*,*,#15878,.T.) ;
#20757 = ORIENTED_EDGE('',*,*,#15883,.T.) ;
#20758 = ORIENTED_EDGE('',*,*,#15885,.T.) ;
#20759 = ORIENTED_EDGE('',*,*,#15886,.T.) ;
#20760 = ORIENTED_EDGE('',*,*,#15887,.T.) ;
#20761 = ORIENTED_EDGE('',*,*,#15885,.F.) ;
#20762 = ORIENTED_EDGE('',*,*,#15882,.F.) ;
#20763 = ORIENTED_EDGE('',*,*,#15888,.F.) ;
#20764 = ORIENTED_EDGE('',*,*,#15889,.F.) ;
#20765 = ORIENTED_EDGE('',*,*,#15765,.T.) ;
#20766 = ORIENTED_EDGE('',*,*,#15841,.T.) ;
#20767 = ORIENTED_EDGE('',*,*,#15748,.T.) ;
#20768 = ORIENTED_EDGE('',*,*,#15702,.T.) ;
#20769 = ORIENTED_EDGE('',*,*,#15890,.T.) ;
#20770 = ORIENTED_EDGE('',*,*,#15694,.F.) ;
#20771 = ORIENTED_EDGE('',*,*,#15766,.T.) ;
#20772 = ORIENTED_EDGE('',*,*,#15889,.T.) ;
#20773 = ORIENTED_EDGE('',*,*,#15596,.F.) ;
#20774 = ORIENTED_EDGE('',*,*,#15842,.F.) ;
#20775 = ORIENTED_EDGE('',*,*,#15890,.F.) ;
#20776 = ORIENTED_EDGE('',*,*,#15701,.F.) ;
#20777 = ORIENTED_EDGE('',*,*,#15738,.T.) ;
#20778 = ORIENTED_EDGE('',*,*,#15891,.T.) ;
#20779 = ORIENTED_EDGE('',*,*,#15678,.T.) ;
#20780 = ORIENTED_EDGE('',*,*,#15892,.T.) ;
#20781 = ORIENTED_EDGE('',*,*,#15891,.F.) ;
#20782 = ORIENTED_EDGE('',*,*,#15737,.T.) ;
#20783 = ORIENTED_EDGE('',*,*,#15893,.F.) ;
#20784 = ORIENTED_EDGE('',*,*,#15679,.T.) ;
#20785 = ORIENTED_EDGE('',*,*,#15682,.T.) ;
#20786 = ORIENTED_EDGE('',*,*,#15894,.T.) ;
#20787 = ORIENTED_EDGE('',*,*,#15734,.T.) ;
#20788 = ORIENTED_EDGE('',*,*,#15895,.T.) ;
#20789 = ORIENTED_EDGE('',*,*,#15894,.F.) ;
#20790 = ORIENTED_EDGE('',*,*,#15681,.F.) ;
#20791 = ORIENTED_EDGE('',*,*,#15896,.F.) ;
#20792 = ORIENTED_EDGE('',*,*,#15735,.F.) ;
#20793 = ORIENTED_EDGE('',*,*,#15680,.T.) ;
#20794 = ORIENTED_EDGE('',*,*,#15893,.T.) ;
#20795 = ORIENTED_EDGE('',*,*,#15736,.T.) ;
#20796 = ORIENTED_EDGE('',*,*,#15896,.T.) ;
#20797 = ORIENTED_EDGE('',*,*,#15730,.T.) ;
#20798 = ORIENTED_EDGE('',*,*,#15897,.T.) ;
#20799 = ORIENTED_EDGE('',*,*,#15686,.T.) ;
#20800 = ORIENTED_EDGE('',*,*,#15898,.T.) ;
#20801 = ORIENTED_EDGE('',*,*,#15897,.F.) ;
#20802 = ORIENTED_EDGE('',*,*,#15729,.T.) ;
#20803 = ORIENTED_EDGE('',*,*,#15899,.F.) ;
#20804 = ORIENTED_EDGE('',*,*,#15687,.T.) ;
#20805 = ORIENTED_EDGE('',*,*,#15684,.T.) ;
#20806 = ORIENTED_EDGE('',*,*,#15900,.T.) ;
#20807 = ORIENTED_EDGE('',*,*,#15732,.T.) ;
#20808 = ORIENTED_EDGE('',*,*,#15901,.T.) ;
#20809 = ORIENTED_EDGE('',*,*,#15895,.F.) ;
#20810 = ORIENTED_EDGE('',*,*,#15733,.F.) ;
#20811 = ORIENTED_EDGE('',*,*,#15900,.F.) ;
#20812 = ORIENTED_EDGE('',*,*,#15683,.F.) ;
#20813 = ORIENTED_EDGE('',*,*,#15688,.T.) ;
#20814 = ORIENTED_EDGE('',*,*,#15899,.T.) ;
#20815 = ORIENTED_EDGE('',*,*,#15728,.T.) ;
#20816 = ORIENTED_EDGE('',*,*,#15902,.T.) ;
#20817 = ORIENTED_EDGE('',*,*,#15833,.T.) ;
#20818 = ORIENTED_EDGE('',*,*,#15903,.T.) ;
#20819 = ORIENTED_EDGE('',*,*,#15712,.T.) ;
#20820 = ORIENTED_EDGE('',*,*,#15904,.T.) ;
#20821 = ORIENTED_EDGE('',*,*,#15903,.F.) ;
#20822 = ORIENTED_EDGE('',*,*,#15832,.F.) ;
#20823 = ORIENTED_EDGE('',*,*,#15905,.F.) ;
#20824 = ORIENTED_EDGE('',*,*,#15713,.F.) ;
#20825 = ORIENTED_EDGE('',*,*,#15831,.T.) ;
#20826 = ORIENTED_EDGE('',*,*,#15906,.T.) ;
#20827 = ORIENTED_EDGE('',*,*,#15714,.T.) ;
#20828 = ORIENTED_EDGE('',*,*,#15905,.T.) ;
#20829 = ORIENTED_EDGE('',*,*,#15906,.F.) ;
#20830 = ORIENTED_EDGE('',*,*,#15830,.T.) ;
#20831 = ORIENTED_EDGE('',*,*,#15907,.F.) ;
#20832 = ORIENTED_EDGE('',*,*,#15715,.T.) ;
#20833 = ORIENTED_EDGE('',*,*,#15716,.T.) ;
#20834 = ORIENTED_EDGE('',*,*,#15907,.T.) ;
#20835 = ORIENTED_EDGE('',*,*,#15829,.T.) ;
#20836 = ORIENTED_EDGE('',*,*,#15697,.T.) ;
#20837 = ORIENTED_EDGE('',*,*,#15710,.T.) ;
#20838 = ORIENTED_EDGE('',*,*,#15908,.T.) ;
#20839 = ORIENTED_EDGE('',*,*,#15835,.T.) ;
#20840 = ORIENTED_EDGE('',*,*,#15909,.T.) ;
#20841 = ORIENTED_EDGE('',*,*,#15908,.F.) ;
#20842 = ORIENTED_EDGE('',*,*,#15709,.T.) ;
#20843 = ORIENTED_EDGE('',*,*,#15910,.F.) ;
#20844 = ORIENTED_EDGE('',*,*,#15836,.F.) ;
#20845 = ORIENTED_EDGE('',*,*,#15837,.T.) ;
#20846 = ORIENTED_EDGE('',*,*,#15910,.T.) ;
#20847 = ORIENTED_EDGE('',*,*,#15708,.T.) ;
#20848 = ORIENTED_EDGE('',*,*,#15911,.T.) ;
#20849 = ORIENTED_EDGE('',*,*,#15747,.F.) ;
#20850 = ORIENTED_EDGE('',*,*,#15840,.F.) ;
#20851 = ORIENTED_EDGE('',*,*,#15912,.F.) ;
#20852 = ORIENTED_EDGE('',*,*,#15705,.T.) ;
#20853 = ORIENTED_EDGE('',*,*,#15839,.T.) ;
#20854 = ORIENTED_EDGE('',*,*,#15913,.T.) ;
#20855 = ORIENTED_EDGE('',*,*,#15706,.T.) ;
#20856 = ORIENTED_EDGE('',*,*,#15912,.T.) ;
#20857 = ORIENTED_EDGE('',*,*,#15911,.F.) ;
#20858 = ORIENTED_EDGE('',*,*,#15707,.T.) ;
#20859 = ORIENTED_EDGE('',*,*,#15913,.F.) ;
#20860 = ORIENTED_EDGE('',*,*,#15838,.F.) ;
#20861 = ORIENTED_EDGE('',*,*,#15888,.T.) ;
#20862 = ORIENTED_EDGE('',*,*,#15881,.T.) ;
#20863 = ORIENTED_EDGE('',*,*,#15914,.T.) ;
#20864 = ORIENTED_EDGE('',*,*,#15600,.T.) ;
#20865 = ORIENTED_EDGE('',*,*,#15914,.F.) ;
#20866 = ORIENTED_EDGE('',*,*,#15880,.F.) ;
#20867 = ORIENTED_EDGE('',*,*,#15876,.F.) ;
#20868 = ORIENTED_EDGE('',*,*,#15915,.F.) ;
#20869 = ORIENTED_EDGE('',*,*,#15916,.T.) ;
#20870 = ORIENTED_EDGE('',*,*,#15763,.T.) ;
#20871 = ORIENTED_EDGE('',*,*,#15725,.T.) ;
#20872 = ORIENTED_EDGE('',*,*,#15721,.F.) ;
#20873 = ORIENTED_EDGE('',*,*,#15762,.T.) ;
#20874 = ORIENTED_EDGE('',*,*,#15872,.T.) ;
#20875 = ORIENTED_EDGE('',*,*,#15602,.F.) ;
#20876 = ORIENTED_EDGE('',*,*,#15672,.F.) ;
#20877 = ORIENTED_EDGE('',*,*,#15689,.F.) ;
#20878 = ORIENTED_EDGE('',*,*,#15902,.F.) ;
#20879 = ORIENTED_EDGE('',*,*,#15727,.T.) ;
#20880 = ORIENTED_EDGE('',*,*,#15751,.F.) ;
#20881 = ORIENTED_EDGE('',*,*,#15739,.F.) ;
#20882 = ORIENTED_EDGE('',*,*,#15892,.F.) ;
#20883 = ORIENTED_EDGE('',*,*,#15677,.F.) ;
#20884 = ORIENTED_EDGE('',*,*,#15691,.F.) ;
#20885 = ORIENTED_EDGE('',*,*,#15917,.T.) ;
#20886 = ORIENTED_EDGE('',*,*,#15744,.F.) ;
#20887 = ORIENTED_EDGE('',*,*,#15917,.F.) ;
#20888 = ORIENTED_EDGE('',*,*,#15690,.F.) ;
#20889 = ORIENTED_EDGE('',*,*,#15918,.T.) ;
#20890 = ORIENTED_EDGE('',*,*,#15743,.F.) ;
#20891 = ORIENTED_EDGE('',*,*,#15918,.F.) ;
#20892 = ORIENTED_EDGE('',*,*,#15898,.F.) ;
#20893 = ORIENTED_EDGE('',*,*,#15685,.F.) ;
#20894 = ORIENTED_EDGE('',*,*,#15901,.F.) ;
#20895 = ORIENTED_EDGE('',*,*,#15731,.F.) ;
#20896 = ORIENTED_EDGE('',*,*,#15718,.F.) ;
#20897 = ORIENTED_EDGE('',*,*,#15919,.T.) ;
#20898 = ORIENTED_EDGE('',*,*,#15844,.F.) ;
#20899 = ORIENTED_EDGE('',*,*,#15919,.F.) ;
#20900 = ORIENTED_EDGE('',*,*,#15618,.T.) ;
#20901 = ORIENTED_EDGE('',*,*,#15920,.F.) ;
#20902 = ORIENTED_EDGE('',*,*,#15804,.T.) ;
#20903 = ORIENTED_EDGE('',*,*,#15921,.T.) ;
#20904 = ORIENTED_EDGE('',*,*,#15620,.T.) ;
#20905 = ORIENTED_EDGE('',*,*,#15922,.F.) ;
#20906 = ORIENTED_EDGE('',*,*,#15802,.T.) ;
#20907 = ORIENTED_EDGE('',*,*,#15923,.F.) ;
#20908 = ORIENTED_EDGE('',*,*,#15801,.F.) ;
#20909 = ORIENTED_EDGE('',*,*,#15920,.T.) ;
#20910 = ORIENTED_EDGE('',*,*,#15617,.F.) ;
#20911 = ORIENTED_EDGE('',*,*,#15923,.T.) ;
#20912 = ORIENTED_EDGE('',*,*,#15803,.F.) ;
#20913 = ORIENTED_EDGE('',*,*,#15922,.T.) ;
#20914 = ORIENTED_EDGE('',*,*,#15619,.F.) ;
#20915 = ORIENTED_EDGE('',*,*,#15921,.F.) ;
#20916 = ORIENTED_EDGE('',*,*,#15821,.F.) ;
#20917 = ORIENTED_EDGE('',*,*,#15857,.F.) ;
#20918 = ORIENTED_EDGE('',*,*,#15612,.F.) ;
#20919 = ORIENTED_EDGE('',*,*,#15859,.T.) ;
#20920 = ORIENTED_EDGE('',*,*,#15646,.F.) ;
#20921 = ORIENTED_EDGE('',*,*,#15924,.T.) ;
#20922 = ORIENTED_EDGE('',*,*,#15771,.F.) ;
#20923 = ORIENTED_EDGE('',*,*,#15924,.F.) ;
#20924 = ORIENTED_EDGE('',*,*,#15645,.F.) ;
#20925 = ORIENTED_EDGE('',*,*,#15925,.T.) ;
#20926 = ORIENTED_EDGE('',*,*,#15772,.F.) ;
#20927 = ORIENTED_EDGE('',*,*,#15925,.F.) ;
#20928 = ORIENTED_EDGE('',*,*,#15904,.F.) ;
#20929 = ORIENTED_EDGE('',*,*,#15711,.T.) ;
#20930 = ORIENTED_EDGE('',*,*,#15909,.F.) ;
#20931 = ORIENTED_EDGE('',*,*,#15834,.F.) ;
#20932 = ORIENTED_EDGE('',*,*,#15756,.F.) ;
#20933 = ORIENTED_EDGE('',*,*,#15760,.T.) ;
#20934 = ORIENTED_EDGE('',*,*,#15866,.F.) ;
#20935 = ORIENTED_EDGE('',*,*,#15868,.T.) ;
#20936 = ORIENTED_EDGE('',*,*,#15870,.F.) ;
#20937 = ORIENTED_EDGE('',*,*,#15871,.F.) ;
#20938 = ORIENTED_EDGE('',*,*,#15647,.F.) ;
#20939 = ORIENTED_EDGE('',*,*,#15926,.T.) ;
#20940 = ORIENTED_EDGE('',*,*,#15800,.F.) ;
#20941 = ORIENTED_EDGE('',*,*,#15926,.F.) ;
#20942 = ORIENTED_EDGE('',*,*,#15648,.F.) ;
#20943 = ORIENTED_EDGE('',*,*,#15927,.T.) ;
#20944 = ORIENTED_EDGE('',*,*,#15799,.F.) ;
#20945 = ORIENTED_EDGE('',*,*,#15927,.F.) ;
#20946 = ORIENTED_EDGE('',*,*,#15649,.F.) ;
#20947 = ORIENTED_EDGE('',*,*,#15928,.T.) ;
#20948 = ORIENTED_EDGE('',*,*,#15798,.F.) ;
#20949 = ORIENTED_EDGE('',*,*,#15928,.F.) ;
#20950 = ORIENTED_EDGE('',*,*,#15650,.F.) ;
#20951 = ORIENTED_EDGE('',*,*,#15929,.T.) ;
#20952 = ORIENTED_EDGE('',*,*,#15797,.F.) ;
#20953 = ORIENTED_EDGE('',*,*,#15929,.F.) ;
#20954 = ORIENTED_EDGE('',*,*,#15795,.F.) ;
#20955 = ORIENTED_EDGE('',*,*,#15930,.T.) ;
#20956 = ORIENTED_EDGE('',*,*,#15642,.F.) ;
#20957 = ORIENTED_EDGE('',*,*,#15931,.T.) ;
#20958 = ORIENTED_EDGE('',*,*,#15794,.T.) ;
#20959 = ORIENTED_EDGE('',*,*,#15932,.F.) ;
#20960 = ORIENTED_EDGE('',*,*,#15643,.T.) ;
#20961 = ORIENTED_EDGE('',*,*,#15930,.F.) ;
#20962 = ORIENTED_EDGE('',*,*,#15793,.F.) ;
#20963 = ORIENTED_EDGE('',*,*,#15933,.T.) ;
#20964 = ORIENTED_EDGE('',*,*,#15644,.F.) ;
#20965 = ORIENTED_EDGE('',*,*,#15932,.T.) ;
#20966 = ORIENTED_EDGE('',*,*,#15796,.T.) ;
#20967 = ORIENTED_EDGE('',*,*,#15931,.F.) ;
#20968 = ORIENTED_EDGE('',*,*,#15641,.T.) ;
#20969 = ORIENTED_EDGE('',*,*,#15933,.F.) ;
#20970 = ORIENTED_EDGE('',*,*,#15791,.F.) ;
#20971 = ORIENTED_EDGE('',*,*,#15934,.T.) ;
#20972 = ORIENTED_EDGE('',*,*,#15638,.F.) ;
#20973 = ORIENTED_EDGE('',*,*,#15935,.T.) ;
#20974 = ORIENTED_EDGE('',*,*,#15790,.T.) ;
#20975 = ORIENTED_EDGE('',*,*,#15936,.F.) ;
#20976 = ORIENTED_EDGE('',*,*,#15639,.T.) ;
#20977 = ORIENTED_EDGE('',*,*,#15934,.F.) ;
#20978 = ORIENTED_EDGE('',*,*,#15789,.F.) ;
#20979 = ORIENTED_EDGE('',*,*,#15937,.T.) ;
#20980 = ORIENTED_EDGE('',*,*,#15640,.F.) ;
#20981 = ORIENTED_EDGE('',*,*,#15936,.T.) ;
#20982 = ORIENTED_EDGE('',*,*,#15792,.T.) ;
#20983 = ORIENTED_EDGE('',*,*,#15935,.F.) ;
#20984 = ORIENTED_EDGE('',*,*,#15637,.T.) ;
#20985 = ORIENTED_EDGE('',*,*,#15937,.F.) ;
#20986 = ORIENTED_EDGE('',*,*,#15787,.F.) ;
#20987 = ORIENTED_EDGE('',*,*,#15938,.T.) ;
#20988 = ORIENTED_EDGE('',*,*,#15634,.F.) ;
#20989 = ORIENTED_EDGE('',*,*,#15939,.T.) ;
#20990 = ORIENTED_EDGE('',*,*,#15786,.T.) ;
#20991 = ORIENTED_EDGE('',*,*,#15940,.F.) ;
#20992 = ORIENTED_EDGE('',*,*,#15635,.T.) ;
#20993 = ORIENTED_EDGE('',*,*,#15938,.F.) ;
#20994 = ORIENTED_EDGE('',*,*,#15785,.F.) ;
#20995 = ORIENTED_EDGE('',*,*,#15941,.T.) ;
#20996 = ORIENTED_EDGE('',*,*,#15636,.F.) ;
#20997 = ORIENTED_EDGE('',*,*,#15940,.T.) ;
#20998 = ORIENTED_EDGE('',*,*,#15788,.T.) ;
#20999 = ORIENTED_EDGE('',*,*,#15939,.F.) ;
#21000 = ORIENTED_EDGE('',*,*,#15633,.T.) ;
#21001 = ORIENTED_EDGE('',*,*,#15941,.F.) ;
#21002 = ORIENTED_EDGE('',*,*,#15783,.F.) ;
#21003 = ORIENTED_EDGE('',*,*,#15942,.T.) ;
#21004 = ORIENTED_EDGE('',*,*,#15630,.F.) ;
#21005 = ORIENTED_EDGE('',*,*,#15943,.T.) ;
#21006 = ORIENTED_EDGE('',*,*,#15782,.T.) ;
#21007 = ORIENTED_EDGE('',*,*,#15944,.F.) ;
#21008 = ORIENTED_EDGE('',*,*,#15631,.T.) ;
#21009 = ORIENTED_EDGE('',*,*,#15942,.F.) ;
#21010 = ORIENTED_EDGE('',*,*,#15781,.F.) ;
#21011 = ORIENTED_EDGE('',*,*,#15945,.T.) ;
#21012 = ORIENTED_EDGE('',*,*,#15632,.F.) ;
#21013 = ORIENTED_EDGE('',*,*,#15944,.T.) ;
#21014 = ORIENTED_EDGE('',*,*,#15784,.T.) ;
#21015 = ORIENTED_EDGE('',*,*,#15943,.F.) ;
#21016 = ORIENTED_EDGE('',*,*,#15629,.T.) ;
#21017 = ORIENTED_EDGE('',*,*,#15945,.F.) ;
#21018 = ORIENTED_EDGE('',*,*,#15779,.F.) ;
#21019 = ORIENTED_EDGE('',*,*,#15946,.T.) ;
#21020 = ORIENTED_EDGE('',*,*,#15626,.F.) ;
#21021 = ORIENTED_EDGE('',*,*,#15947,.T.) ;
#21022 = ORIENTED_EDGE('',*,*,#15778,.T.) ;
#21023 = ORIENTED_EDGE('',*,*,#15948,.F.) ;
#21024 = ORIENTED_EDGE('',*,*,#15627,.T.) ;
#21025 = ORIENTED_EDGE('',*,*,#15946,.F.) ;
#21026 = ORIENTED_EDGE('',*,*,#15777,.F.) ;
#21027 = ORIENTED_EDGE('',*,*,#15949,.T.) ;
#21028 = ORIENTED_EDGE('',*,*,#15628,.F.) ;
#21029 = ORIENTED_EDGE('',*,*,#15948,.T.) ;
#21030 = ORIENTED_EDGE('',*,*,#15780,.T.) ;
#21031 = ORIENTED_EDGE('',*,*,#15947,.F.) ;
#21032 = ORIENTED_EDGE('',*,*,#15625,.T.) ;
#21033 = ORIENTED_EDGE('',*,*,#15949,.F.) ;
#21034 = ORIENTED_EDGE('',*,*,#15775,.F.) ;
#21035 = ORIENTED_EDGE('',*,*,#15950,.T.) ;
#21036 = ORIENTED_EDGE('',*,*,#15622,.F.) ;
#21037 = ORIENTED_EDGE('',*,*,#15951,.T.) ;
#21038 = ORIENTED_EDGE('',*,*,#15774,.T.) ;
#21039 = ORIENTED_EDGE('',*,*,#15952,.F.) ;
#21040 = ORIENTED_EDGE('',*,*,#15623,.T.) ;
#21041 = ORIENTED_EDGE('',*,*,#15950,.F.) ;
#21042 = ORIENTED_EDGE('',*,*,#15773,.F.) ;
#21043 = ORIENTED_EDGE('',*,*,#15953,.T.) ;
#21044 = ORIENTED_EDGE('',*,*,#15624,.F.) ;
#21045 = ORIENTED_EDGE('',*,*,#15952,.T.) ;
#21046 = ORIENTED_EDGE('',*,*,#15776,.T.) ;
#21047 = ORIENTED_EDGE('',*,*,#15951,.F.) ;
#21048 = ORIENTED_EDGE('',*,*,#15621,.T.) ;
#21049 = ORIENTED_EDGE('',*,*,#15953,.F.) ;
#21050 = ORIENTED_EDGE('',*,*,#15764,.T.) ;
#21051 = ORIENTED_EDGE('',*,*,#15916,.F.) ;
#21052 = ORIENTED_EDGE('',*,*,#15954,.T.) ;
#21053 = ORIENTED_EDGE('',*,*,#15886,.F.) ;
#21054 = ORIENTED_EDGE('',*,*,#15875,.F.) ;
#21055 = ORIENTED_EDGE('',*,*,#15879,.F.) ;
#21056 = ORIENTED_EDGE('',*,*,#15884,.F.) ;
#21057 = ORIENTED_EDGE('',*,*,#15887,.F.) ;
#21058 = ORIENTED_EDGE('',*,*,#15954,.F.) ;
#21059 = ORIENTED_EDGE('',*,*,#15915,.T.) ;
#21060 = ORIENTED_EDGE('',*,*,#15717,.T.) ;
#21061 = ORIENTED_EDGE('',*,*,#15955,.T.) ;
#21062 = ORIENTED_EDGE('',*,*,#15843,.T.) ;
#21063 = ORIENTED_EDGE('',*,*,#15955,.F.) ;
#21064 = ORIENTED_EDGE('',*,*,#15825,.F.) ;
#21065 = ORIENTED_EDGE('',*,*,#15861,.F.) ;
#21066 = ORIENTED_EDGE('',*,*,#15605,.F.) ;
#21067 = ORIENTED_EDGE('',*,*,#15863,.T.) ;
#21068 = ORIENTED_EDGE('',*,*,#15767,.F.) ;
#21069 = ORIENTED_EDGE('',*,*,#15864,.F.) ;
#21070 = ORIENTED_EDGE('',*,*,#15663,.F.) ;
#21071 = ORIENTED_EDGE('',*,*,#15850,.T.) ;
#21072 = ORIENTED_EDGE('',*,*,#15817,.F.) ;
#21073 = ORIENTED_EDGE('',*,*,#15853,.F.) ;
#21074 = ORIENTED_EDGE('',*,*,#15616,.F.) ;
#21075 = ORIENTED_EDGE('',*,*,#15855,.T.) ;
#21076 = ORIENTED_EDGE('',*,*,#15651,.T.) ;
#21077 = ORIENTED_EDGE('',*,*,#15956,.F.) ;
#21078 = ORIENTED_EDGE('',*,*,#15805,.T.) ;
#21079 = ORIENTED_EDGE('',*,*,#15957,.T.) ;
#21080 = ORIENTED_EDGE('',*,*,#15653,.T.) ;
#21081 = ORIENTED_EDGE('',*,*,#15958,.F.) ;
#21082 = ORIENTED_EDGE('',*,*,#15807,.T.) ;
#21083 = ORIENTED_EDGE('',*,*,#15959,.F.) ;
#21084 = ORIENTED_EDGE('',*,*,#15806,.F.) ;
#21085 = ORIENTED_EDGE('',*,*,#15956,.T.) ;
#21086 = ORIENTED_EDGE('',*,*,#15654,.F.) ;
#21087 = ORIENTED_EDGE('',*,*,#15959,.T.) ;
#21088 = ORIENTED_EDGE('',*,*,#15808,.F.) ;
#21089 = ORIENTED_EDGE('',*,*,#15958,.T.) ;
#21090 = ORIENTED_EDGE('',*,*,#15652,.F.) ;
#21091 = ORIENTED_EDGE('',*,*,#15957,.F.) ;
#21092 = ORIENTED_EDGE('',*,*,#15655,.T.) ;
#21093 = ORIENTED_EDGE('',*,*,#15960,.F.) ;
#21094 = ORIENTED_EDGE('',*,*,#15809,.T.) ;
#21095 = ORIENTED_EDGE('',*,*,#15961,.T.) ;
#21096 = ORIENTED_EDGE('',*,*,#15657,.T.) ;
#21097 = ORIENTED_EDGE('',*,*,#15962,.F.) ;
#21098 = ORIENTED_EDGE('',*,*,#15811,.T.) ;
#21099 = ORIENTED_EDGE('',*,*,#15963,.F.) ;
#21100 = ORIENTED_EDGE('',*,*,#15810,.F.) ;
#21101 = ORIENTED_EDGE('',*,*,#15960,.T.) ;
#21102 = ORIENTED_EDGE('',*,*,#15658,.F.) ;
#21103 = ORIENTED_EDGE('',*,*,#15963,.T.) ;
#21104 = ORIENTED_EDGE('',*,*,#15812,.F.) ;
#21105 = ORIENTED_EDGE('',*,*,#15962,.T.) ;
#21106 = ORIENTED_EDGE('',*,*,#15656,.F.) ;
#21107 = ORIENTED_EDGE('',*,*,#15961,.F.) ;
#21108 = ORIENTED_EDGE('',*,*,#15659,.T.) ;
#21109 = ORIENTED_EDGE('',*,*,#15964,.F.) ;
#21110 = ORIENTED_EDGE('',*,*,#15813,.T.) ;
#21111 = ORIENTED_EDGE('',*,*,#15965,.T.) ;
#21112 = ORIENTED_EDGE('',*,*,#15661,.T.) ;
#21113 = ORIENTED_EDGE('',*,*,#15966,.F.) ;
#21114 = ORIENTED_EDGE('',*,*,#15815,.T.) ;
#21115 = ORIENTED_EDGE('',*,*,#15967,.F.) ;
#21116 = ORIENTED_EDGE('',*,*,#15814,.F.) ;
#21117 = ORIENTED_EDGE('',*,*,#15964,.T.) ;
#21118 = ORIENTED_EDGE('',*,*,#15662,.F.) ;
#21119 = ORIENTED_EDGE('',*,*,#15967,.T.) ;
#21120 = ORIENTED_EDGE('',*,*,#15816,.F.) ;
#21121 = ORIENTED_EDGE('',*,*,#15966,.T.) ;
#21122 = ORIENTED_EDGE('',*,*,#15660,.F.) ;
#21123 = ORIENTED_EDGE('',*,*,#15965,.F.) ;
#21124 = ORIENTED_EDGE('',*,*,#15968,.T.) ;
#21125 = ORIENTED_EDGE('',*,*,#15969,.T.) ;
#21126 = ORIENTED_EDGE('',*,*,#15970,.T.) ;
#21127 = ORIENTED_EDGE('',*,*,#15971,.F.) ;
#21128 = ORIENTED_EDGE('',*,*,#15972,.T.) ;
#21129 = ORIENTED_EDGE('',*,*,#15973,.T.) ;
#21130 = ORIENTED_EDGE('',*,*,#15968,.F.) ;
#21131 = ORIENTED_EDGE('',*,*,#15974,.F.) ;
#21132 = ORIENTED_EDGE('',*,*,#15975,.T.) ;
#21133 = ORIENTED_EDGE('',*,*,#15976,.T.) ;
#21134 = ORIENTED_EDGE('',*,*,#15972,.F.) ;
#21135 = ORIENTED_EDGE('',*,*,#15977,.F.) ;
#21136 = ORIENTED_EDGE('',*,*,#15978,.T.) ;
#21137 = ORIENTED_EDGE('',*,*,#15979,.T.) ;
#21138 = ORIENTED_EDGE('',*,*,#15975,.F.) ;
#21139 = ORIENTED_EDGE('',*,*,#15980,.F.) ;
#21140 = ORIENTED_EDGE('',*,*,#15981,.F.) ;
#21141 = ORIENTED_EDGE('',*,*,#15982,.F.) ;
#21142 = ORIENTED_EDGE('',*,*,#15983,.F.) ;
#21143 = ORIENTED_EDGE('',*,*,#15984,.T.) ;
#21144 = ORIENTED_EDGE('',*,*,#15985,.T.) ;
#21145 = ORIENTED_EDGE('',*,*,#15986,.F.) ;
#21146 = ORIENTED_EDGE('',*,*,#15987,.F.) ;
#21147 = ORIENTED_EDGE('',*,*,#15988,.F.) ;
#21148 = ORIENTED_EDGE('',*,*,#15989,.T.) ;
#21149 = ORIENTED_EDGE('',*,*,#15990,.F.) ;
#21150 = ORIENTED_EDGE('',*,*,#15985,.F.) ;
#21151 = ORIENTED_EDGE('',*,*,#15991,.F.) ;
#21152 = ORIENTED_EDGE('',*,*,#15992,.T.) ;
#21153 = ORIENTED_EDGE('',*,*,#15993,.F.) ;
#21154 = ORIENTED_EDGE('',*,*,#15989,.F.) ;
#21155 = ORIENTED_EDGE('',*,*,#15994,.F.) ;
#21156 = ORIENTED_EDGE('',*,*,#15995,.T.) ;
#21157 = ORIENTED_EDGE('',*,*,#15996,.F.) ;
#21158 = ORIENTED_EDGE('',*,*,#15992,.F.) ;
#21159 = ORIENTED_EDGE('',*,*,#15997,.F.) ;
#21160 = ORIENTED_EDGE('',*,*,#15998,.T.) ;
#21161 = ORIENTED_EDGE('',*,*,#15999,.F.) ;
#21162 = ORIENTED_EDGE('',*,*,#15995,.F.) ;
#21163 = ORIENTED_EDGE('',*,*,#16000,.F.) ;
#21164 = ORIENTED_EDGE('',*,*,#16001,.F.) ;
#21165 = ORIENTED_EDGE('',*,*,#16002,.F.) ;
#21166 = ORIENTED_EDGE('',*,*,#16003,.T.) ;
#21167 = ORIENTED_EDGE('',*,*,#16004,.F.) ;
#21168 = ORIENTED_EDGE('',*,*,#16005,.F.) ;
#21169 = ORIENTED_EDGE('',*,*,#16006,.T.) ;
#21170 = ORIENTED_EDGE('',*,*,#15983,.T.) ;
#21171 = ORIENTED_EDGE('',*,*,#16007,.T.) ;
#21172 = ORIENTED_EDGE('',*,*,#16008,.F.) ;
#21173 = ORIENTED_EDGE('',*,*,#16009,.F.) ;
#21174 = ORIENTED_EDGE('',*,*,#15970,.F.) ;
#21175 = ORIENTED_EDGE('',*,*,#16010,.F.) ;
#21176 = ORIENTED_EDGE('',*,*,#16008,.T.) ;
#21177 = ORIENTED_EDGE('',*,*,#16011,.F.) ;
#21178 = ORIENTED_EDGE('',*,*,#16012,.F.) ;
#21179 = ORIENTED_EDGE('',*,*,#16005,.T.) ;
#21180 = ORIENTED_EDGE('',*,*,#16013,.T.) ;
#21181 = ORIENTED_EDGE('',*,*,#16014,.T.) ;
#21182 = ORIENTED_EDGE('',*,*,#16015,.T.) ;
#21183 = ORIENTED_EDGE('',*,*,#16001,.T.) ;
#21184 = ORIENTED_EDGE('',*,*,#16016,.F.) ;
#21185 = ORIENTED_EDGE('',*,*,#15998,.F.) ;
#21186 = ORIENTED_EDGE('',*,*,#16017,.F.) ;
#21187 = ORIENTED_EDGE('',*,*,#15981,.T.) ;
#21188 = ORIENTED_EDGE('',*,*,#16018,.T.) ;
#21189 = ORIENTED_EDGE('',*,*,#15978,.F.) ;
#21190 = ORIENTED_EDGE('',*,*,#16019,.F.) ;
#21191 = ORIENTED_EDGE('',*,*,#16020,.F.) ;
#21192 = ORIENTED_EDGE('',*,*,#16021,.F.) ;
#21193 = ORIENTED_EDGE('',*,*,#16022,.F.) ;
#21194 = ORIENTED_EDGE('',*,*,#16023,.F.) ;
#21195 = ORIENTED_EDGE('',*,*,#16024,.T.) ;
#21196 = ORIENTED_EDGE('',*,*,#16025,.T.) ;
#21197 = ORIENTED_EDGE('',*,*,#16002,.T.) ;
#21198 = ORIENTED_EDGE('',*,*,#16017,.T.) ;
#21199 = ORIENTED_EDGE('',*,*,#16000,.T.) ;
#21200 = ORIENTED_EDGE('',*,*,#15997,.T.) ;
#21201 = ORIENTED_EDGE('',*,*,#15994,.T.) ;
#21202 = ORIENTED_EDGE('',*,*,#15991,.T.) ;
#21203 = ORIENTED_EDGE('',*,*,#15988,.T.) ;
#21204 = ORIENTED_EDGE('',*,*,#16010,.T.) ;
#21205 = ORIENTED_EDGE('',*,*,#15969,.F.) ;
#21206 = ORIENTED_EDGE('',*,*,#15973,.F.) ;
#21207 = ORIENTED_EDGE('',*,*,#15976,.F.) ;
#21208 = ORIENTED_EDGE('',*,*,#15979,.F.) ;
#21209 = ORIENTED_EDGE('',*,*,#16018,.F.) ;
#21210 = ORIENTED_EDGE('',*,*,#15984,.F.) ;
#21211 = ORIENTED_EDGE('',*,*,#16006,.F.) ;
#21212 = ORIENTED_EDGE('',*,*,#16015,.F.) ;
#21213 = ORIENTED_EDGE('',*,*,#15982,.T.) ;
#21214 = ORIENTED_EDGE('',*,*,#16019,.T.) ;
#21215 = ORIENTED_EDGE('',*,*,#15980,.T.) ;
#21216 = ORIENTED_EDGE('',*,*,#15977,.T.) ;
#21217 = ORIENTED_EDGE('',*,*,#15974,.T.) ;
#21218 = ORIENTED_EDGE('',*,*,#15971,.T.) ;
#21219 = ORIENTED_EDGE('',*,*,#16009,.T.) ;
#21220 = ORIENTED_EDGE('',*,*,#16012,.T.) ;
#21221 = ORIENTED_EDGE('',*,*,#15986,.T.) ;
#21222 = ORIENTED_EDGE('',*,*,#15990,.T.) ;
#21223 = ORIENTED_EDGE('',*,*,#15993,.T.) ;
#21224 = ORIENTED_EDGE('',*,*,#15996,.T.) ;
#21225 = ORIENTED_EDGE('',*,*,#15999,.T.) ;
#21226 = ORIENTED_EDGE('',*,*,#16016,.T.) ;
#21227 = ORIENTED_EDGE('',*,*,#16004,.T.) ;
#21228 = ORIENTED_EDGE('',*,*,#16013,.F.) ;
#21229 = ORIENTED_EDGE('',*,*,#16007,.F.) ;
#21230 = ORIENTED_EDGE('',*,*,#16023,.T.) ;
#21231 = ORIENTED_EDGE('',*,*,#16026,.T.) ;
#21232 = ORIENTED_EDGE('',*,*,#16027,.T.) ;
#21233 = ORIENTED_EDGE('',*,*,#16028,.T.) ;
#21234 = ORIENTED_EDGE('',*,*,#16029,.T.) ;
#21235 = ORIENTED_EDGE('',*,*,#16030,.T.) ;
#21236 = ORIENTED_EDGE('',*,*,#16014,.F.) ;
#21237 = ORIENTED_EDGE('',*,*,#16003,.F.) ;
#21238 = ORIENTED_EDGE('',*,*,#16031,.T.) ;
#21239 = ORIENTED_EDGE('',*,*,#16032,.T.) ;
#21240 = ORIENTED_EDGE('',*,*,#16033,.T.) ;
#21241 = ORIENTED_EDGE('',*,*,#16034,.F.) ;
#21242 = ORIENTED_EDGE('',*,*,#16035,.F.) ;
#21243 = ORIENTED_EDGE('',*,*,#16036,.F.) ;
#21244 = ORIENTED_EDGE('',*,*,#16034,.T.) ;
#21245 = ORIENTED_EDGE('',*,*,#16037,.T.) ;
#21246 = ORIENTED_EDGE('',*,*,#16038,.T.) ;
#21247 = ORIENTED_EDGE('',*,*,#16039,.F.) ;
#21248 = ORIENTED_EDGE('',*,*,#16040,.F.) ;
#21249 = ORIENTED_EDGE('',*,*,#16041,.F.) ;
#21250 = ORIENTED_EDGE('',*,*,#16039,.T.) ;
#21251 = ORIENTED_EDGE('',*,*,#16042,.T.) ;
#21252 = ORIENTED_EDGE('',*,*,#16022,.T.) ;
#21253 = ORIENTED_EDGE('',*,*,#16043,.F.) ;
#21254 = ORIENTED_EDGE('',*,*,#16024,.F.) ;
#21255 = ORIENTED_EDGE('',*,*,#16044,.F.) ;
#21256 = ORIENTED_EDGE('',*,*,#16043,.T.) ;
#21257 = ORIENTED_EDGE('',*,*,#16021,.T.) ;
#21258 = ORIENTED_EDGE('',*,*,#16045,.T.) ;
#21259 = ORIENTED_EDGE('',*,*,#16046,.F.) ;
#21260 = ORIENTED_EDGE('',*,*,#16047,.F.) ;
#21261 = ORIENTED_EDGE('',*,*,#16025,.F.) ;
#21262 = ORIENTED_EDGE('',*,*,#16046,.T.) ;
#21263 = ORIENTED_EDGE('',*,*,#16048,.T.) ;
#21264 = ORIENTED_EDGE('',*,*,#16049,.T.) ;
#21265 = ORIENTED_EDGE('',*,*,#16050,.F.) ;
#21266 = ORIENTED_EDGE('',*,*,#16051,.F.) ;
#21267 = ORIENTED_EDGE('',*,*,#16052,.F.) ;
#21268 = ORIENTED_EDGE('',*,*,#16050,.T.) ;
#21269 = ORIENTED_EDGE('',*,*,#16053,.T.) ;
#21270 = ORIENTED_EDGE('',*,*,#16054,.T.) ;
#21271 = ORIENTED_EDGE('',*,*,#16031,.F.) ;
#21272 = ORIENTED_EDGE('',*,*,#16055,.F.) ;
#21273 = ORIENTED_EDGE('',*,*,#16056,.F.) ;
#21274 = ORIENTED_EDGE('',*,*,#16020,.T.) ;
#21275 = ORIENTED_EDGE('',*,*,#16057,.T.) ;
#21276 = ORIENTED_EDGE('',*,*,#16058,.T.) ;
#21277 = ORIENTED_EDGE('',*,*,#16059,.T.) ;
#21278 = ORIENTED_EDGE('',*,*,#16060,.T.) ;
#21279 = ORIENTED_EDGE('',*,*,#16061,.F.) ;
#21280 = ORIENTED_EDGE('',*,*,#15987,.T.) ;
#21281 = ORIENTED_EDGE('',*,*,#16011,.T.) ;
#21282 = ORIENTED_EDGE('',*,*,#16036,.T.) ;
#21283 = ORIENTED_EDGE('',*,*,#16028,.F.) ;
#21284 = ORIENTED_EDGE('',*,*,#16055,.T.) ;
#21285 = ORIENTED_EDGE('',*,*,#16051,.T.) ;
#21286 = ORIENTED_EDGE('',*,*,#16056,.T.) ;
#21287 = ORIENTED_EDGE('',*,*,#16027,.F.) ;
#21288 = ORIENTED_EDGE('',*,*,#16047,.T.) ;
#21289 = ORIENTED_EDGE('',*,*,#16052,.T.) ;
#21290 = ORIENTED_EDGE('',*,*,#16026,.F.) ;
#21291 = ORIENTED_EDGE('',*,*,#16040,.T.) ;
#21292 = ORIENTED_EDGE('',*,*,#16044,.T.) ;
#21293 = ORIENTED_EDGE('',*,*,#16030,.F.) ;
#21294 = ORIENTED_EDGE('',*,*,#16035,.T.) ;
#21295 = ORIENTED_EDGE('',*,*,#16041,.T.) ;
#21296 = ORIENTED_EDGE('',*,*,#16029,.F.) ;
#21297 = ORIENTED_EDGE('',*,*,#16061,.T.) ;
#21298 = ORIENTED_EDGE('',*,*,#16048,.F.) ;
#21299 = ORIENTED_EDGE('',*,*,#16045,.F.) ;
#21300 = ORIENTED_EDGE('',*,*,#16060,.F.) ;
#21301 = ORIENTED_EDGE('',*,*,#16053,.F.) ;
#21302 = ORIENTED_EDGE('',*,*,#16049,.F.) ;
#21303 = ORIENTED_EDGE('',*,*,#16054,.F.) ;
#21304 = ORIENTED_EDGE('',*,*,#16059,.F.) ;
#21305 = ORIENTED_EDGE('',*,*,#16032,.F.) ;
#21306 = ORIENTED_EDGE('',*,*,#16058,.F.) ;
#21307 = ORIENTED_EDGE('',*,*,#16037,.F.) ;
#21308 = ORIENTED_EDGE('',*,*,#16033,.F.) ;
#21309 = ORIENTED_EDGE('',*,*,#16057,.F.) ;
#21310 = ORIENTED_EDGE('',*,*,#16042,.F.) ;
#21311 = ORIENTED_EDGE('',*,*,#16038,.F.) ;
#21312 = ORIENTED_EDGE('',*,*,#16062,.F.) ;
#21313 = ORIENTED_EDGE('',*,*,#16063,.T.) ;
#21314 = ORIENTED_EDGE('',*,*,#16064,.T.) ;
#21315 = ORIENTED_EDGE('',*,*,#16065,.F.) ;
#21316 = ORIENTED_EDGE('',*,*,#16066,.T.) ;
#21317 = ORIENTED_EDGE('',*,*,#16062,.T.) ;
#21318 = ORIENTED_EDGE('',*,*,#16067,.T.) ;
#21319 = ORIENTED_EDGE('',*,*,#16068,.F.) ;
#21320 = ORIENTED_EDGE('',*,*,#16069,.F.) ;
#21321 = ORIENTED_EDGE('',*,*,#16070,.T.) ;
#21322 = ORIENTED_EDGE('',*,*,#16065,.T.) ;
#21323 = ORIENTED_EDGE('',*,*,#16071,.F.) ;
#21324 = ORIENTED_EDGE('',*,*,#16072,.F.) ;
#21325 = ORIENTED_EDGE('',*,*,#16073,.T.) ;
#21326 = ORIENTED_EDGE('',*,*,#16069,.T.) ;
#21327 = ORIENTED_EDGE('',*,*,#16074,.F.) ;
#21328 = ORIENTED_EDGE('',*,*,#16075,.F.) ;
#21329 = ORIENTED_EDGE('',*,*,#16076,.T.) ;
#21330 = ORIENTED_EDGE('',*,*,#16072,.T.) ;
#21331 = ORIENTED_EDGE('',*,*,#16077,.F.) ;
#21332 = ORIENTED_EDGE('',*,*,#16078,.F.) ;
#21333 = ORIENTED_EDGE('',*,*,#16079,.T.) ;
#21334 = ORIENTED_EDGE('',*,*,#16075,.T.) ;
#21335 = ORIENTED_EDGE('',*,*,#16080,.F.) ;
#21336 = ORIENTED_EDGE('',*,*,#16081,.F.) ;
#21337 = ORIENTED_EDGE('',*,*,#16082,.F.) ;
#21338 = ORIENTED_EDGE('',*,*,#16083,.T.) ;
#21339 = ORIENTED_EDGE('',*,*,#16084,.T.) ;
#21340 = ORIENTED_EDGE('',*,*,#16085,.T.) ;
#21341 = ORIENTED_EDGE('',*,*,#16086,.T.) ;
#21342 = ORIENTED_EDGE('',*,*,#16084,.F.) ;
#21343 = ORIENTED_EDGE('',*,*,#16087,.T.) ;
#21344 = ORIENTED_EDGE('',*,*,#16088,.F.) ;
#21345 = ORIENTED_EDGE('',*,*,#16089,.F.) ;
#21346 = ORIENTED_EDGE('',*,*,#16090,.F.) ;
#21347 = ORIENTED_EDGE('',*,*,#16081,.T.) ;
#21348 = ORIENTED_EDGE('',*,*,#16091,.F.) ;
#21349 = ORIENTED_EDGE('',*,*,#16092,.F.) ;
#21350 = ORIENTED_EDGE('',*,*,#16093,.F.) ;
#21351 = ORIENTED_EDGE('',*,*,#16089,.T.) ;
#21352 = ORIENTED_EDGE('',*,*,#16094,.F.) ;
#21353 = ORIENTED_EDGE('',*,*,#16095,.F.) ;
#21354 = ORIENTED_EDGE('',*,*,#16096,.F.) ;
#21355 = ORIENTED_EDGE('',*,*,#16092,.T.) ;
#21356 = ORIENTED_EDGE('',*,*,#16097,.F.) ;
#21357 = ORIENTED_EDGE('',*,*,#16098,.F.) ;
#21358 = ORIENTED_EDGE('',*,*,#16099,.F.) ;
#21359 = ORIENTED_EDGE('',*,*,#16095,.T.) ;
#21360 = ORIENTED_EDGE('',*,*,#16100,.F.) ;
#21361 = ORIENTED_EDGE('',*,*,#16098,.T.) ;
#21362 = ORIENTED_EDGE('',*,*,#16101,.F.) ;
#21363 = ORIENTED_EDGE('',*,*,#16102,.F.) ;
#21364 = ORIENTED_EDGE('',*,*,#16103,.F.) ;
#21365 = ORIENTED_EDGE('',*,*,#16078,.T.) ;
#21366 = ORIENTED_EDGE('',*,*,#16104,.F.) ;
#21367 = ORIENTED_EDGE('',*,*,#16105,.F.) ;
#21368 = ORIENTED_EDGE('',*,*,#16106,.T.) ;
#21369 = ORIENTED_EDGE('',*,*,#16107,.T.) ;
#21370 = ORIENTED_EDGE('',*,*,#16108,.T.) ;
#21371 = ORIENTED_EDGE('',*,*,#16109,.T.) ;
#21372 = ORIENTED_EDGE('',*,*,#16110,.T.) ;
#21373 = ORIENTED_EDGE('',*,*,#16108,.F.) ;
#21374 = ORIENTED_EDGE('',*,*,#16110,.F.) ;
#21375 = ORIENTED_EDGE('',*,*,#16111,.T.) ;
#21376 = ORIENTED_EDGE('',*,*,#16085,.F.) ;
#21377 = ORIENTED_EDGE('',*,*,#16086,.F.) ;
#21378 = ORIENTED_EDGE('',*,*,#16111,.F.) ;
#21379 = ORIENTED_EDGE('',*,*,#16109,.F.) ;
#21380 = ORIENTED_EDGE('',*,*,#16107,.F.) ;
#21381 = ORIENTED_EDGE('',*,*,#16112,.F.) ;
#21382 = ORIENTED_EDGE('',*,*,#16113,.T.) ;
#21383 = ORIENTED_EDGE('',*,*,#16114,.T.) ;
#21384 = ORIENTED_EDGE('',*,*,#16115,.T.) ;
#21385 = ORIENTED_EDGE('',*,*,#16116,.F.) ;
#21386 = ORIENTED_EDGE('',*,*,#16117,.F.) ;
#21387 = ORIENTED_EDGE('',*,*,#16118,.T.) ;
#21388 = ORIENTED_EDGE('',*,*,#16119,.T.) ;
#21389 = ORIENTED_EDGE('',*,*,#16120,.T.) ;
#21390 = ORIENTED_EDGE('',*,*,#16121,.F.) ;
#21391 = ORIENTED_EDGE('',*,*,#16122,.F.) ;
#21392 = ORIENTED_EDGE('',*,*,#16123,.T.) ;
#21393 = ORIENTED_EDGE('',*,*,#16124,.T.) ;
#21394 = ORIENTED_EDGE('',*,*,#16125,.T.) ;
#21395 = ORIENTED_EDGE('',*,*,#16126,.F.) ;
#21396 = ORIENTED_EDGE('',*,*,#16127,.T.) ;
#21397 = ORIENTED_EDGE('',*,*,#16128,.T.) ;
#21398 = ORIENTED_EDGE('',*,*,#16129,.T.) ;
#21399 = ORIENTED_EDGE('',*,*,#16130,.T.) ;
#21400 = ORIENTED_EDGE('',*,*,#16131,.F.) ;
#21401 = ORIENTED_EDGE('',*,*,#16132,.T.) ;
#21402 = ORIENTED_EDGE('',*,*,#16133,.T.) ;
#21403 = ORIENTED_EDGE('',*,*,#16134,.F.) ;
#21404 = ORIENTED_EDGE('',*,*,#16133,.F.) ;
#21405 = ORIENTED_EDGE('',*,*,#16135,.T.) ;
#21406 = ORIENTED_EDGE('',*,*,#16105,.T.) ;
#21407 = ORIENTED_EDGE('',*,*,#16136,.T.) ;
#21408 = ORIENTED_EDGE('',*,*,#16102,.T.) ;
#21409 = ORIENTED_EDGE('',*,*,#16137,.T.) ;
#21410 = ORIENTED_EDGE('',*,*,#16138,.T.) ;
#21411 = ORIENTED_EDGE('',*,*,#16139,.F.) ;
#21412 = ORIENTED_EDGE('',*,*,#16140,.T.) ;
#21413 = ORIENTED_EDGE('',*,*,#16141,.T.) ;
#21414 = ORIENTED_EDGE('',*,*,#16142,.T.) ;
#21415 = ORIENTED_EDGE('',*,*,#16143,.F.) ;
#21416 = ORIENTED_EDGE('',*,*,#16144,.F.) ;
#21417 = ORIENTED_EDGE('',*,*,#16145,.T.) ;
#21418 = ORIENTED_EDGE('',*,*,#16146,.T.) ;
#21419 = ORIENTED_EDGE('',*,*,#16147,.T.) ;
#21420 = ORIENTED_EDGE('',*,*,#16148,.F.) ;
#21421 = ORIENTED_EDGE('',*,*,#16149,.F.) ;
#21422 = ORIENTED_EDGE('',*,*,#16150,.T.) ;
#21423 = ORIENTED_EDGE('',*,*,#16151,.T.) ;
#21424 = ORIENTED_EDGE('',*,*,#16152,.T.) ;
#21425 = ORIENTED_EDGE('',*,*,#16153,.F.) ;
#21426 = ORIENTED_EDGE('',*,*,#16154,.F.) ;
#21427 = ORIENTED_EDGE('',*,*,#16155,.T.) ;
#21428 = ORIENTED_EDGE('',*,*,#16156,.T.) ;
#21429 = ORIENTED_EDGE('',*,*,#16157,.T.) ;
#21430 = ORIENTED_EDGE('',*,*,#16158,.T.) ;
#21431 = ORIENTED_EDGE('',*,*,#16137,.F.) ;
#21432 = ORIENTED_EDGE('',*,*,#16153,.T.) ;
#21433 = ORIENTED_EDGE('',*,*,#16159,.T.) ;
#21434 = ORIENTED_EDGE('',*,*,#16112,.T.) ;
#21435 = ORIENTED_EDGE('',*,*,#16160,.F.) ;
#21436 = ORIENTED_EDGE('',*,*,#16143,.T.) ;
#21437 = ORIENTED_EDGE('',*,*,#16161,.T.) ;
#21438 = ORIENTED_EDGE('',*,*,#16122,.T.) ;
#21439 = ORIENTED_EDGE('',*,*,#16162,.F.) ;
#21440 = ORIENTED_EDGE('',*,*,#16148,.T.) ;
#21441 = ORIENTED_EDGE('',*,*,#16163,.T.) ;
#21442 = ORIENTED_EDGE('',*,*,#16117,.T.) ;
#21443 = ORIENTED_EDGE('',*,*,#16164,.F.) ;
#21444 = ORIENTED_EDGE('',*,*,#16165,.T.) ;
#21445 = ORIENTED_EDGE('',*,*,#16114,.F.) ;
#21446 = ORIENTED_EDGE('',*,*,#16166,.F.) ;
#21447 = ORIENTED_EDGE('',*,*,#16151,.F.) ;
#21448 = ORIENTED_EDGE('',*,*,#16167,.T.) ;
#21449 = ORIENTED_EDGE('',*,*,#16115,.F.) ;
#21450 = ORIENTED_EDGE('',*,*,#16165,.F.) ;
#21451 = ORIENTED_EDGE('',*,*,#16150,.F.) ;
#21452 = ORIENTED_EDGE('',*,*,#16149,.T.) ;
#21453 = ORIENTED_EDGE('',*,*,#16164,.T.) ;
#21454 = ORIENTED_EDGE('',*,*,#16116,.T.) ;
#21455 = ORIENTED_EDGE('',*,*,#16167,.F.) ;
#21456 = ORIENTED_EDGE('',*,*,#16168,.T.) ;
#21457 = ORIENTED_EDGE('',*,*,#16118,.F.) ;
#21458 = ORIENTED_EDGE('',*,*,#16163,.F.) ;
#21459 = ORIENTED_EDGE('',*,*,#16147,.F.) ;
#21460 = ORIENTED_EDGE('',*,*,#16169,.T.) ;
#21461 = ORIENTED_EDGE('',*,*,#16119,.F.) ;
#21462 = ORIENTED_EDGE('',*,*,#16168,.F.) ;
#21463 = ORIENTED_EDGE('',*,*,#16146,.F.) ;
#21464 = ORIENTED_EDGE('',*,*,#16170,.T.) ;
#21465 = ORIENTED_EDGE('',*,*,#16120,.F.) ;
#21466 = ORIENTED_EDGE('',*,*,#16169,.F.) ;
#21467 = ORIENTED_EDGE('',*,*,#16145,.F.) ;
#21468 = ORIENTED_EDGE('',*,*,#16144,.T.) ;
#21469 = ORIENTED_EDGE('',*,*,#16162,.T.) ;
#21470 = ORIENTED_EDGE('',*,*,#16121,.T.) ;
#21471 = ORIENTED_EDGE('',*,*,#16170,.F.) ;
#21472 = ORIENTED_EDGE('',*,*,#16171,.T.) ;
#21473 = ORIENTED_EDGE('',*,*,#16123,.F.) ;
#21474 = ORIENTED_EDGE('',*,*,#16161,.F.) ;
#21475 = ORIENTED_EDGE('',*,*,#16142,.F.) ;
#21476 = ORIENTED_EDGE('',*,*,#16172,.T.) ;
#21477 = ORIENTED_EDGE('',*,*,#16124,.F.) ;
#21478 = ORIENTED_EDGE('',*,*,#16171,.F.) ;
#21479 = ORIENTED_EDGE('',*,*,#16141,.F.) ;
#21480 = ORIENTED_EDGE('',*,*,#16173,.T.) ;
#21481 = ORIENTED_EDGE('',*,*,#16125,.F.) ;
#21482 = ORIENTED_EDGE('',*,*,#16172,.F.) ;
#21483 = ORIENTED_EDGE('',*,*,#16140,.F.) ;
#21484 = ORIENTED_EDGE('',*,*,#16139,.T.) ;
#21485 = ORIENTED_EDGE('',*,*,#16174,.T.) ;
#21486 = ORIENTED_EDGE('',*,*,#16126,.T.) ;
#21487 = ORIENTED_EDGE('',*,*,#16173,.F.) ;
#21488 = ORIENTED_EDGE('',*,*,#16175,.T.) ;
#21489 = ORIENTED_EDGE('',*,*,#16127,.F.) ;
#21490 = ORIENTED_EDGE('',*,*,#16174,.F.) ;
#21491 = ORIENTED_EDGE('',*,*,#16138,.F.) ;
#21492 = ORIENTED_EDGE('',*,*,#16158,.F.) ;
#21493 = ORIENTED_EDGE('',*,*,#16176,.T.) ;
#21494 = ORIENTED_EDGE('',*,*,#16128,.F.) ;
#21495 = ORIENTED_EDGE('',*,*,#16175,.F.) ;
#21496 = ORIENTED_EDGE('',*,*,#16157,.F.) ;
#21497 = ORIENTED_EDGE('',*,*,#16177,.T.) ;
#21498 = ORIENTED_EDGE('',*,*,#16129,.F.) ;
#21499 = ORIENTED_EDGE('',*,*,#16176,.F.) ;
#21500 = ORIENTED_EDGE('',*,*,#16156,.F.) ;
#21501 = ORIENTED_EDGE('',*,*,#16178,.T.) ;
#21502 = ORIENTED_EDGE('',*,*,#16130,.F.) ;
#21503 = ORIENTED_EDGE('',*,*,#16177,.F.) ;
#21504 = ORIENTED_EDGE('',*,*,#16155,.F.) ;
#21505 = ORIENTED_EDGE('',*,*,#16154,.T.) ;
#21506 = ORIENTED_EDGE('',*,*,#16160,.T.) ;
#21507 = ORIENTED_EDGE('',*,*,#16131,.T.) ;
#21508 = ORIENTED_EDGE('',*,*,#16178,.F.) ;
#21509 = ORIENTED_EDGE('',*,*,#16166,.T.) ;
#21510 = ORIENTED_EDGE('',*,*,#16113,.F.) ;
#21511 = ORIENTED_EDGE('',*,*,#16159,.F.) ;
#21512 = ORIENTED_EDGE('',*,*,#16152,.F.) ;
#21513 = ORIENTED_EDGE('',*,*,#16179,.F.) ;
#21514 = ORIENTED_EDGE('',*,*,#16087,.F.) ;
#21515 = ORIENTED_EDGE('',*,*,#16083,.F.) ;
#21516 = ORIENTED_EDGE('',*,*,#16180,.F.) ;
#21517 = ORIENTED_EDGE('',*,*,#16067,.F.) ;
#21518 = ORIENTED_EDGE('',*,*,#16064,.F.) ;
#21519 = ORIENTED_EDGE('',*,*,#16134,.T.) ;
#21520 = ORIENTED_EDGE('',*,*,#16179,.T.) ;
#21521 = ORIENTED_EDGE('',*,*,#16063,.F.) ;
#21522 = ORIENTED_EDGE('',*,*,#16066,.F.) ;
#21523 = ORIENTED_EDGE('',*,*,#16070,.F.) ;
#21524 = ORIENTED_EDGE('',*,*,#16073,.F.) ;
#21525 = ORIENTED_EDGE('',*,*,#16076,.F.) ;
#21526 = ORIENTED_EDGE('',*,*,#16079,.F.) ;
#21527 = ORIENTED_EDGE('',*,*,#16106,.F.) ;
#21528 = ORIENTED_EDGE('',*,*,#16135,.F.) ;
#21529 = ORIENTED_EDGE('',*,*,#16132,.F.) ;
#21530 = ORIENTED_EDGE('',*,*,#16101,.T.) ;
#21531 = ORIENTED_EDGE('',*,*,#16100,.T.) ;
#21532 = ORIENTED_EDGE('',*,*,#16097,.T.) ;
#21533 = ORIENTED_EDGE('',*,*,#16094,.T.) ;
#21534 = ORIENTED_EDGE('',*,*,#16091,.T.) ;
#21535 = ORIENTED_EDGE('',*,*,#16088,.T.) ;
#21536 = ORIENTED_EDGE('',*,*,#16180,.T.) ;
#21537 = ORIENTED_EDGE('',*,*,#16082,.T.) ;
#21538 = ORIENTED_EDGE('',*,*,#16090,.T.) ;
#21539 = ORIENTED_EDGE('',*,*,#16093,.T.) ;
#21540 = ORIENTED_EDGE('',*,*,#16096,.T.) ;
#21541 = ORIENTED_EDGE('',*,*,#16099,.T.) ;
#21542 = ORIENTED_EDGE('',*,*,#16103,.T.) ;
#21543 = ORIENTED_EDGE('',*,*,#16136,.F.) ;
#21544 = ORIENTED_EDGE('',*,*,#16104,.T.) ;
#21545 = ORIENTED_EDGE('',*,*,#16080,.T.) ;
#21546 = ORIENTED_EDGE('',*,*,#16077,.T.) ;
#21547 = ORIENTED_EDGE('',*,*,#16074,.T.) ;
#21548 = ORIENTED_EDGE('',*,*,#16071,.T.) ;
#21549 = ORIENTED_EDGE('',*,*,#16068,.T.) ;
#21550 = ORIENTED_EDGE('',*,*,#16181,.T.) ;
#21551 = ORIENTED_EDGE('',*,*,#16182,.T.) ;
#21552 = ORIENTED_EDGE('',*,*,#16183,.F.) ;
#21553 = ORIENTED_EDGE('',*,*,#16184,.F.) ;
#21554 = ORIENTED_EDGE('',*,*,#16185,.T.) ;
#21555 = ORIENTED_EDGE('',*,*,#16186,.T.) ;
#21556 = ORIENTED_EDGE('',*,*,#16187,.T.) ;
#21557 = ORIENTED_EDGE('',*,*,#16181,.F.) ;
#21558 = ORIENTED_EDGE('',*,*,#16188,.F.) ;
#21559 = ORIENTED_EDGE('',*,*,#16189,.F.) ;
#21560 = ORIENTED_EDGE('',*,*,#16190,.F.) ;
#21561 = ORIENTED_EDGE('',*,*,#16191,.F.) ;
#21562 = ORIENTED_EDGE('',*,*,#16192,.F.) ;
#21563 = ORIENTED_EDGE('',*,*,#16193,.T.) ;
#21564 = ORIENTED_EDGE('',*,*,#16194,.T.) ;
#21565 = ORIENTED_EDGE('',*,*,#16195,.T.) ;
#21566 = ORIENTED_EDGE('',*,*,#16196,.F.) ;
#21567 = ORIENTED_EDGE('',*,*,#16197,.F.) ;
#21568 = ORIENTED_EDGE('',*,*,#16198,.T.) ;
#21569 = ORIENTED_EDGE('',*,*,#16199,.T.) ;
#21570 = ORIENTED_EDGE('',*,*,#16200,.T.) ;
#21571 = ORIENTED_EDGE('',*,*,#16194,.F.) ;
#21572 = ORIENTED_EDGE('',*,*,#16201,.F.) ;
#21573 = ORIENTED_EDGE('',*,*,#16202,.F.) ;
#21574 = ORIENTED_EDGE('',*,*,#16203,.F.) ;
#21575 = ORIENTED_EDGE('',*,*,#16204,.F.) ;
#21576 = ORIENTED_EDGE('',*,*,#16205,.F.) ;
#21577 = ORIENTED_EDGE('',*,*,#16206,.F.) ;
#21578 = ORIENTED_EDGE('',*,*,#16207,.F.) ;
#21579 = ORIENTED_EDGE('',*,*,#16208,.T.) ;
#21580 = ORIENTED_EDGE('',*,*,#16209,.T.) ;
#21581 = ORIENTED_EDGE('',*,*,#16210,.T.) ;
#21582 = ORIENTED_EDGE('',*,*,#16211,.T.) ;
#21583 = ORIENTED_EDGE('',*,*,#16212,.F.) ;
#21584 = ORIENTED_EDGE('',*,*,#16213,.F.) ;
#21585 = ORIENTED_EDGE('',*,*,#16214,.T.) ;
#21586 = ORIENTED_EDGE('',*,*,#16215,.T.) ;
#21587 = ORIENTED_EDGE('',*,*,#16216,.T.) ;
#21588 = ORIENTED_EDGE('',*,*,#16210,.F.) ;
#21589 = ORIENTED_EDGE('',*,*,#16217,.F.) ;
#21590 = ORIENTED_EDGE('',*,*,#16218,.F.) ;
#21591 = ORIENTED_EDGE('',*,*,#16219,.F.) ;
#21592 = ORIENTED_EDGE('',*,*,#16220,.F.) ;
#21593 = ORIENTED_EDGE('',*,*,#16221,.F.) ;
#21594 = ORIENTED_EDGE('',*,*,#16222,.T.) ;
#21595 = ORIENTED_EDGE('',*,*,#16223,.T.) ;
#21596 = ORIENTED_EDGE('',*,*,#16224,.T.) ;
#21597 = ORIENTED_EDGE('',*,*,#16225,.T.) ;
#21598 = ORIENTED_EDGE('',*,*,#16226,.F.) ;
#21599 = ORIENTED_EDGE('',*,*,#16227,.F.) ;
#21600 = ORIENTED_EDGE('',*,*,#16228,.T.) ;
#21601 = ORIENTED_EDGE('',*,*,#16229,.T.) ;
#21602 = ORIENTED_EDGE('',*,*,#16230,.T.) ;
#21603 = ORIENTED_EDGE('',*,*,#16224,.F.) ;
#21604 = ORIENTED_EDGE('',*,*,#16231,.F.) ;
#21605 = ORIENTED_EDGE('',*,*,#16232,.F.) ;
#21606 = ORIENTED_EDGE('',*,*,#16233,.F.) ;
#21607 = ORIENTED_EDGE('',*,*,#16234,.F.) ;
#21608 = ORIENTED_EDGE('',*,*,#16235,.F.) ;
#21609 = ORIENTED_EDGE('',*,*,#16236,.T.) ;
#21610 = ORIENTED_EDGE('',*,*,#16237,.T.) ;
#21611 = ORIENTED_EDGE('',*,*,#16238,.F.) ;
#21612 = ORIENTED_EDGE('',*,*,#16239,.T.) ;
#21613 = ORIENTED_EDGE('',*,*,#16240,.T.) ;
#21614 = ORIENTED_EDGE('',*,*,#16241,.T.) ;
#21615 = ORIENTED_EDGE('',*,*,#16242,.F.) ;
#21616 = ORIENTED_EDGE('',*,*,#16237,.F.) ;
#21617 = ORIENTED_EDGE('',*,*,#16243,.T.) ;
#21618 = ORIENTED_EDGE('',*,*,#16244,.F.) ;
#21619 = ORIENTED_EDGE('',*,*,#16245,.T.) ;
#21620 = ORIENTED_EDGE('',*,*,#16246,.T.) ;
#21621 = ORIENTED_EDGE('',*,*,#16247,.F.) ;
#21622 = ORIENTED_EDGE('',*,*,#16248,.T.) ;
#21623 = ORIENTED_EDGE('',*,*,#16249,.T.) ;
#21624 = ORIENTED_EDGE('',*,*,#16250,.T.) ;
#21625 = ORIENTED_EDGE('',*,*,#16251,.F.) ;
#21626 = ORIENTED_EDGE('',*,*,#16252,.T.) ;
#21627 = ORIENTED_EDGE('',*,*,#16253,.T.) ;
#21628 = ORIENTED_EDGE('',*,*,#16254,.T.) ;
#21629 = ORIENTED_EDGE('',*,*,#16255,.F.) ;
#21630 = ORIENTED_EDGE('',*,*,#16250,.F.) ;
#21631 = ORIENTED_EDGE('',*,*,#16256,.T.) ;
#21632 = ORIENTED_EDGE('',*,*,#16257,.F.) ;
#21633 = ORIENTED_EDGE('',*,*,#16258,.T.) ;
#21634 = ORIENTED_EDGE('',*,*,#16259,.T.) ;
#21635 = ORIENTED_EDGE('',*,*,#16260,.F.) ;
#21636 = ORIENTED_EDGE('',*,*,#16261,.T.) ;
#21637 = ORIENTED_EDGE('',*,*,#16262,.T.) ;
#21638 = ORIENTED_EDGE('',*,*,#16263,.T.) ;
#21639 = ORIENTED_EDGE('',*,*,#16264,.F.) ;
#21640 = ORIENTED_EDGE('',*,*,#16265,.T.) ;
#21641 = ORIENTED_EDGE('',*,*,#16266,.T.) ;
#21642 = ORIENTED_EDGE('',*,*,#16267,.T.) ;
#21643 = ORIENTED_EDGE('',*,*,#16268,.F.) ;
#21644 = ORIENTED_EDGE('',*,*,#16263,.F.) ;
#21645 = ORIENTED_EDGE('',*,*,#16269,.T.) ;
#21646 = ORIENTED_EDGE('',*,*,#16270,.F.) ;
#21647 = ORIENTED_EDGE('',*,*,#16271,.T.) ;
#21648 = ORIENTED_EDGE('',*,*,#16272,.T.) ;
#21649 = ORIENTED_EDGE('',*,*,#16273,.F.) ;
#21650 = ORIENTED_EDGE('',*,*,#16274,.T.) ;
#21651 = ORIENTED_EDGE('',*,*,#16275,.T.) ;
#21652 = ORIENTED_EDGE('',*,*,#16276,.T.) ;
#21653 = ORIENTED_EDGE('',*,*,#16277,.F.) ;
#21654 = ORIENTED_EDGE('',*,*,#16278,.T.) ;
#21655 = ORIENTED_EDGE('',*,*,#16279,.T.) ;
#21656 = ORIENTED_EDGE('',*,*,#16280,.T.) ;
#21657 = ORIENTED_EDGE('',*,*,#16281,.F.) ;
#21658 = ORIENTED_EDGE('',*,*,#16276,.F.) ;
#21659 = ORIENTED_EDGE('',*,*,#16282,.T.) ;
#21660 = ORIENTED_EDGE('',*,*,#16283,.F.) ;
#21661 = ORIENTED_EDGE('',*,*,#16284,.T.) ;
#21662 = ORIENTED_EDGE('',*,*,#16285,.T.) ;
#21663 = ORIENTED_EDGE('',*,*,#16286,.F.) ;
#21664 = ORIENTED_EDGE('',*,*,#16287,.T.) ;
#21665 = ORIENTED_EDGE('',*,*,#16288,.T.) ;
#21666 = ORIENTED_EDGE('',*,*,#16289,.T.) ;
#21667 = ORIENTED_EDGE('',*,*,#16290,.T.) ;
#21668 = ORIENTED_EDGE('',*,*,#16291,.F.) ;
#21669 = ORIENTED_EDGE('',*,*,#16292,.F.) ;
#21670 = ORIENTED_EDGE('',*,*,#16293,.T.) ;
#21671 = ORIENTED_EDGE('',*,*,#16294,.T.) ;
#21672 = ORIENTED_EDGE('',*,*,#16295,.T.) ;
#21673 = ORIENTED_EDGE('',*,*,#16289,.F.) ;
#21674 = ORIENTED_EDGE('',*,*,#16296,.F.) ;
#21675 = ORIENTED_EDGE('',*,*,#16297,.F.) ;
#21676 = ORIENTED_EDGE('',*,*,#16298,.F.) ;
#21677 = ORIENTED_EDGE('',*,*,#16299,.F.) ;
#21678 = ORIENTED_EDGE('',*,*,#16300,.F.) ;
#21679 = ORIENTED_EDGE('',*,*,#16301,.T.) ;
#21680 = ORIENTED_EDGE('',*,*,#16302,.T.) ;
#21681 = ORIENTED_EDGE('',*,*,#16303,.T.) ;
#21682 = ORIENTED_EDGE('',*,*,#16304,.F.) ;
#21683 = ORIENTED_EDGE('',*,*,#16305,.F.) ;
#21684 = ORIENTED_EDGE('',*,*,#16306,.T.) ;
#21685 = ORIENTED_EDGE('',*,*,#16307,.T.) ;
#21686 = ORIENTED_EDGE('',*,*,#16308,.T.) ;
#21687 = ORIENTED_EDGE('',*,*,#16302,.F.) ;
#21688 = ORIENTED_EDGE('',*,*,#16309,.F.) ;
#21689 = ORIENTED_EDGE('',*,*,#16310,.F.) ;
#21690 = ORIENTED_EDGE('',*,*,#16311,.F.) ;
#21691 = ORIENTED_EDGE('',*,*,#16312,.F.) ;
#21692 = ORIENTED_EDGE('',*,*,#16313,.F.) ;
#21693 = ORIENTED_EDGE('',*,*,#16314,.T.) ;
#21694 = ORIENTED_EDGE('',*,*,#16315,.T.) ;
#21695 = ORIENTED_EDGE('',*,*,#16316,.T.) ;
#21696 = ORIENTED_EDGE('',*,*,#16317,.F.) ;
#21697 = ORIENTED_EDGE('',*,*,#16318,.T.) ;
#21698 = ORIENTED_EDGE('',*,*,#16319,.T.) ;
#21699 = ORIENTED_EDGE('',*,*,#16320,.T.) ;
#21700 = ORIENTED_EDGE('',*,*,#16321,.F.) ;
#21701 = ORIENTED_EDGE('',*,*,#16316,.F.) ;
#21702 = ORIENTED_EDGE('',*,*,#16322,.T.) ;
#21703 = ORIENTED_EDGE('',*,*,#16323,.F.) ;
#21704 = ORIENTED_EDGE('',*,*,#16324,.T.) ;
#21705 = ORIENTED_EDGE('',*,*,#16325,.T.) ;
#21706 = ORIENTED_EDGE('',*,*,#16326,.F.) ;
#21707 = ORIENTED_EDGE('',*,*,#16327,.T.) ;
#21708 = ORIENTED_EDGE('',*,*,#16328,.T.) ;
#21709 = ORIENTED_EDGE('',*,*,#16329,.T.) ;
#21710 = ORIENTED_EDGE('',*,*,#16330,.F.) ;
#21711 = ORIENTED_EDGE('',*,*,#16331,.T.) ;
#21712 = ORIENTED_EDGE('',*,*,#16332,.T.) ;
#21713 = ORIENTED_EDGE('',*,*,#16333,.T.) ;
#21714 = ORIENTED_EDGE('',*,*,#16334,.F.) ;
#21715 = ORIENTED_EDGE('',*,*,#16329,.F.) ;
#21716 = ORIENTED_EDGE('',*,*,#16335,.T.) ;
#21717 = ORIENTED_EDGE('',*,*,#16336,.F.) ;
#21718 = ORIENTED_EDGE('',*,*,#16337,.T.) ;
#21719 = ORIENTED_EDGE('',*,*,#16338,.T.) ;
#21720 = ORIENTED_EDGE('',*,*,#16339,.F.) ;
#21721 = ORIENTED_EDGE('',*,*,#16340,.T.) ;
#21722 = ORIENTED_EDGE('',*,*,#16341,.T.) ;
#21723 = ORIENTED_EDGE('',*,*,#16342,.T.) ;
#21724 = ORIENTED_EDGE('',*,*,#16343,.T.) ;
#21725 = ORIENTED_EDGE('',*,*,#16344,.F.) ;
#21726 = ORIENTED_EDGE('',*,*,#16345,.F.) ;
#21727 = ORIENTED_EDGE('',*,*,#16346,.T.) ;
#21728 = ORIENTED_EDGE('',*,*,#16347,.T.) ;
#21729 = ORIENTED_EDGE('',*,*,#16348,.T.) ;
#21730 = ORIENTED_EDGE('',*,*,#16342,.F.) ;
#21731 = ORIENTED_EDGE('',*,*,#16349,.F.) ;
#21732 = ORIENTED_EDGE('',*,*,#16350,.F.) ;
#21733 = ORIENTED_EDGE('',*,*,#16351,.F.) ;
#21734 = ORIENTED_EDGE('',*,*,#16352,.F.) ;
#21735 = ORIENTED_EDGE('',*,*,#16353,.F.) ;
#21736 = ORIENTED_EDGE('',*,*,#16354,.T.) ;
#21737 = ORIENTED_EDGE('',*,*,#16355,.T.) ;
#21738 = ORIENTED_EDGE('',*,*,#16356,.T.) ;
#21739 = ORIENTED_EDGE('',*,*,#16357,.F.) ;
#21740 = ORIENTED_EDGE('',*,*,#16358,.F.) ;
#21741 = ORIENTED_EDGE('',*,*,#16359,.T.) ;
#21742 = ORIENTED_EDGE('',*,*,#16360,.T.) ;
#21743 = ORIENTED_EDGE('',*,*,#16361,.T.) ;
#21744 = ORIENTED_EDGE('',*,*,#16355,.F.) ;
#21745 = ORIENTED_EDGE('',*,*,#16362,.F.) ;
#21746 = ORIENTED_EDGE('',*,*,#16363,.F.) ;
#21747 = ORIENTED_EDGE('',*,*,#16364,.F.) ;
#21748 = ORIENTED_EDGE('',*,*,#16365,.F.) ;
#21749 = ORIENTED_EDGE('',*,*,#16366,.F.) ;
#21750 = ORIENTED_EDGE('',*,*,#16367,.T.) ;
#21751 = ORIENTED_EDGE('',*,*,#16368,.T.) ;
#21752 = ORIENTED_EDGE('',*,*,#16369,.F.) ;
#21753 = ORIENTED_EDGE('',*,*,#16370,.T.) ;
#21754 = ORIENTED_EDGE('',*,*,#16371,.T.) ;
#21755 = ORIENTED_EDGE('',*,*,#16372,.T.) ;
#21756 = ORIENTED_EDGE('',*,*,#16373,.F.) ;
#21757 = ORIENTED_EDGE('',*,*,#16368,.F.) ;
#21758 = ORIENTED_EDGE('',*,*,#16374,.T.) ;
#21759 = ORIENTED_EDGE('',*,*,#16375,.F.) ;
#21760 = ORIENTED_EDGE('',*,*,#16376,.T.) ;
#21761 = ORIENTED_EDGE('',*,*,#16377,.T.) ;
#21762 = ORIENTED_EDGE('',*,*,#16378,.F.) ;
#21763 = ORIENTED_EDGE('',*,*,#16379,.T.) ;
#21764 = ORIENTED_EDGE('',*,*,#16380,.T.) ;
#21765 = ORIENTED_EDGE('',*,*,#16381,.T.) ;
#21766 = ORIENTED_EDGE('',*,*,#16382,.F.) ;
#21767 = ORIENTED_EDGE('',*,*,#16383,.T.) ;
#21768 = ORIENTED_EDGE('',*,*,#16384,.T.) ;
#21769 = ORIENTED_EDGE('',*,*,#16385,.T.) ;
#21770 = ORIENTED_EDGE('',*,*,#16386,.F.) ;
#21771 = ORIENTED_EDGE('',*,*,#16381,.F.) ;
#21772 = ORIENTED_EDGE('',*,*,#16387,.T.) ;
#21773 = ORIENTED_EDGE('',*,*,#16388,.F.) ;
#21774 = ORIENTED_EDGE('',*,*,#16389,.T.) ;
#21775 = ORIENTED_EDGE('',*,*,#16390,.T.) ;
#21776 = ORIENTED_EDGE('',*,*,#16391,.F.) ;
#21777 = ORIENTED_EDGE('',*,*,#16392,.T.) ;
#21778 = ORIENTED_EDGE('',*,*,#16393,.T.) ;
#21779 = ORIENTED_EDGE('',*,*,#16388,.T.) ;
#21780 = ORIENTED_EDGE('',*,*,#16394,.T.) ;
#21781 = ORIENTED_EDGE('',*,*,#16384,.F.) ;
#21782 = ORIENTED_EDGE('',*,*,#16395,.T.) ;
#21783 = ORIENTED_EDGE('',*,*,#16375,.T.) ;
#21784 = ORIENTED_EDGE('',*,*,#16396,.T.) ;
#21785 = ORIENTED_EDGE('',*,*,#16371,.F.) ;
#21786 = ORIENTED_EDGE('',*,*,#16397,.T.) ;
#21787 = ORIENTED_EDGE('',*,*,#16363,.T.) ;
#21788 = ORIENTED_EDGE('',*,*,#16398,.T.) ;
#21789 = ORIENTED_EDGE('',*,*,#16359,.F.) ;
#21790 = ORIENTED_EDGE('',*,*,#16399,.F.) ;
#21791 = ORIENTED_EDGE('',*,*,#16350,.T.) ;
#21792 = ORIENTED_EDGE('',*,*,#16400,.T.) ;
#21793 = ORIENTED_EDGE('',*,*,#16346,.F.) ;
#21794 = ORIENTED_EDGE('',*,*,#16401,.F.) ;
#21795 = ORIENTED_EDGE('',*,*,#16336,.T.) ;
#21796 = ORIENTED_EDGE('',*,*,#16402,.T.) ;
#21797 = ORIENTED_EDGE('',*,*,#16332,.F.) ;
#21798 = ORIENTED_EDGE('',*,*,#16403,.T.) ;
#21799 = ORIENTED_EDGE('',*,*,#16323,.T.) ;
#21800 = ORIENTED_EDGE('',*,*,#16404,.T.) ;
#21801 = ORIENTED_EDGE('',*,*,#16319,.F.) ;
#21802 = ORIENTED_EDGE('',*,*,#16405,.T.) ;
#21803 = ORIENTED_EDGE('',*,*,#16310,.T.) ;
#21804 = ORIENTED_EDGE('',*,*,#16406,.T.) ;
#21805 = ORIENTED_EDGE('',*,*,#16407,.T.) ;
#21806 = ORIENTED_EDGE('',*,*,#16306,.F.) ;
#21807 = ORIENTED_EDGE('',*,*,#16408,.F.) ;
#21808 = ORIENTED_EDGE('',*,*,#16297,.T.) ;
#21809 = ORIENTED_EDGE('',*,*,#16409,.T.) ;
#21810 = ORIENTED_EDGE('',*,*,#16293,.F.) ;
#21811 = ORIENTED_EDGE('',*,*,#16410,.F.) ;
#21812 = ORIENTED_EDGE('',*,*,#16283,.T.) ;
#21813 = ORIENTED_EDGE('',*,*,#16411,.T.) ;
#21814 = ORIENTED_EDGE('',*,*,#16279,.F.) ;
#21815 = ORIENTED_EDGE('',*,*,#16412,.T.) ;
#21816 = ORIENTED_EDGE('',*,*,#16270,.T.) ;
#21817 = ORIENTED_EDGE('',*,*,#16413,.T.) ;
#21818 = ORIENTED_EDGE('',*,*,#16266,.F.) ;
#21819 = ORIENTED_EDGE('',*,*,#16414,.T.) ;
#21820 = ORIENTED_EDGE('',*,*,#16257,.T.) ;
#21821 = ORIENTED_EDGE('',*,*,#16415,.T.) ;
#21822 = ORIENTED_EDGE('',*,*,#16253,.F.) ;
#21823 = ORIENTED_EDGE('',*,*,#16416,.T.) ;
#21824 = ORIENTED_EDGE('',*,*,#16244,.T.) ;
#21825 = ORIENTED_EDGE('',*,*,#16417,.T.) ;
#21826 = ORIENTED_EDGE('',*,*,#16240,.F.) ;
#21827 = ORIENTED_EDGE('',*,*,#16418,.T.) ;
#21828 = ORIENTED_EDGE('',*,*,#16232,.T.) ;
#21829 = ORIENTED_EDGE('',*,*,#16419,.T.) ;
#21830 = ORIENTED_EDGE('',*,*,#16228,.F.) ;
#21831 = ORIENTED_EDGE('',*,*,#16420,.F.) ;
#21832 = ORIENTED_EDGE('',*,*,#16218,.T.) ;
#21833 = ORIENTED_EDGE('',*,*,#16421,.T.) ;
#21834 = ORIENTED_EDGE('',*,*,#16422,.T.) ;
#21835 = ORIENTED_EDGE('',*,*,#16214,.F.) ;
#21836 = ORIENTED_EDGE('',*,*,#16423,.F.) ;
#21837 = ORIENTED_EDGE('',*,*,#16203,.T.) ;
#21838 = ORIENTED_EDGE('',*,*,#16424,.T.) ;
#21839 = ORIENTED_EDGE('',*,*,#16198,.F.) ;
#21840 = ORIENTED_EDGE('',*,*,#16425,.F.) ;
#21841 = ORIENTED_EDGE('',*,*,#16189,.T.) ;
#21842 = ORIENTED_EDGE('',*,*,#16426,.T.) ;
#21843 = ORIENTED_EDGE('',*,*,#16185,.F.) ;
#21844 = ORIENTED_EDGE('',*,*,#16427,.F.) ;
#21845 = ORIENTED_EDGE('',*,*,#16428,.F.) ;
#21846 = ORIENTED_EDGE('',*,*,#16429,.T.) ;
#21847 = ORIENTED_EDGE('',*,*,#16430,.T.) ;
#21848 = ORIENTED_EDGE('',*,*,#16431,.T.) ;
#21849 = ORIENTED_EDGE('',*,*,#16432,.F.) ;
#21850 = ORIENTED_EDGE('',*,*,#16433,.T.) ;
#21851 = ORIENTED_EDGE('',*,*,#16434,.F.) ;
#21852 = ORIENTED_EDGE('',*,*,#16435,.T.) ;
#21853 = ORIENTED_EDGE('',*,*,#16436,.F.) ;
#21854 = ORIENTED_EDGE('',*,*,#16437,.T.) ;
#21855 = ORIENTED_EDGE('',*,*,#16438,.F.) ;
#21856 = ORIENTED_EDGE('',*,*,#16439,.T.) ;
#21857 = ORIENTED_EDGE('',*,*,#16440,.F.) ;
#21858 = ORIENTED_EDGE('',*,*,#16441,.T.) ;
#21859 = ORIENTED_EDGE('',*,*,#16442,.F.) ;
#21860 = ORIENTED_EDGE('',*,*,#16443,.T.) ;
#21861 = ORIENTED_EDGE('',*,*,#16444,.F.) ;
#21862 = ORIENTED_EDGE('',*,*,#16445,.T.) ;
#21863 = ORIENTED_EDGE('',*,*,#16446,.F.) ;
#21864 = ORIENTED_EDGE('',*,*,#16447,.T.) ;
#21865 = ORIENTED_EDGE('',*,*,#16428,.T.) ;
#21866 = ORIENTED_EDGE('',*,*,#16448,.F.) ;
#21867 = ORIENTED_EDGE('',*,*,#16449,.F.) ;
#21868 = ORIENTED_EDGE('',*,*,#16450,.F.) ;
#21869 = ORIENTED_EDGE('',*,*,#16439,.F.) ;
#21870 = ORIENTED_EDGE('',*,*,#16451,.F.) ;
#21871 = ORIENTED_EDGE('',*,*,#16452,.F.) ;
#21872 = ORIENTED_EDGE('',*,*,#16453,.F.) ;
#21873 = ORIENTED_EDGE('',*,*,#16454,.F.) ;
#21874 = ORIENTED_EDGE('',*,*,#16455,.F.) ;
#21875 = ORIENTED_EDGE('',*,*,#16441,.F.) ;
#21876 = ORIENTED_EDGE('',*,*,#16456,.F.) ;
#21877 = ORIENTED_EDGE('',*,*,#16457,.F.) ;
#21878 = ORIENTED_EDGE('',*,*,#16458,.T.) ;
#21879 = ORIENTED_EDGE('',*,*,#16459,.F.) ;
#21880 = ORIENTED_EDGE('',*,*,#16460,.F.) ;
#21881 = ORIENTED_EDGE('',*,*,#16461,.T.) ;
#21882 = ORIENTED_EDGE('',*,*,#16462,.T.) ;
#21883 = ORIENTED_EDGE('',*,*,#16463,.F.) ;
#21884 = ORIENTED_EDGE('',*,*,#16464,.T.) ;
#21885 = ORIENTED_EDGE('',*,*,#16432,.T.) ;
#21886 = ORIENTED_EDGE('',*,*,#16465,.F.) ;
#21887 = ORIENTED_EDGE('',*,*,#16436,.T.) ;
#21888 = ORIENTED_EDGE('',*,*,#16450,.T.) ;
#21889 = ORIENTED_EDGE('',*,*,#16466,.F.) ;
#21890 = ORIENTED_EDGE('',*,*,#16467,.T.) ;
#21891 = ORIENTED_EDGE('',*,*,#16468,.T.) ;
#21892 = ORIENTED_EDGE('',*,*,#16469,.T.) ;
#21893 = ORIENTED_EDGE('',*,*,#16470,.F.) ;
#21894 = ORIENTED_EDGE('',*,*,#16471,.T.) ;
#21895 = ORIENTED_EDGE('',*,*,#16472,.T.) ;
#21896 = ORIENTED_EDGE('',*,*,#16473,.T.) ;
#21897 = ORIENTED_EDGE('',*,*,#16474,.F.) ;
#21898 = ORIENTED_EDGE('',*,*,#16475,.F.) ;
#21899 = ORIENTED_EDGE('',*,*,#16476,.F.) ;
#21900 = ORIENTED_EDGE('',*,*,#16477,.F.) ;
#21901 = ORIENTED_EDGE('',*,*,#16478,.T.) ;
#21902 = ORIENTED_EDGE('',*,*,#16479,.F.) ;
#21903 = ORIENTED_EDGE('',*,*,#16480,.T.) ;
#21904 = ORIENTED_EDGE('',*,*,#16481,.F.) ;
#21905 = ORIENTED_EDGE('',*,*,#16482,.T.) ;
#21906 = ORIENTED_EDGE('',*,*,#16483,.F.) ;
#21907 = ORIENTED_EDGE('',*,*,#16484,.F.) ;
#21908 = ORIENTED_EDGE('',*,*,#16485,.F.) ;
#21909 = ORIENTED_EDGE('',*,*,#16486,.F.) ;
#21910 = ORIENTED_EDGE('',*,*,#16487,.F.) ;
#21911 = ORIENTED_EDGE('',*,*,#16488,.T.) ;
#21912 = ORIENTED_EDGE('',*,*,#16489,.F.) ;
#21913 = ORIENTED_EDGE('',*,*,#16490,.T.) ;
#21914 = ORIENTED_EDGE('',*,*,#16491,.F.) ;
#21915 = ORIENTED_EDGE('',*,*,#16492,.T.) ;
#21916 = ORIENTED_EDGE('',*,*,#16493,.T.) ;
#21917 = ORIENTED_EDGE('',*,*,#16330,.T.) ;
#21918 = ORIENTED_EDGE('',*,*,#16334,.T.) ;
#21919 = ORIENTED_EDGE('',*,*,#16494,.T.) ;
#21920 = ORIENTED_EDGE('',*,*,#16291,.T.) ;
#21921 = ORIENTED_EDGE('',*,*,#16495,.T.) ;
#21922 = ORIENTED_EDGE('',*,*,#16496,.T.) ;
#21923 = ORIENTED_EDGE('',*,*,#16317,.T.) ;
#21924 = ORIENTED_EDGE('',*,*,#16321,.T.) ;
#21925 = ORIENTED_EDGE('',*,*,#16497,.T.) ;
#21926 = ORIENTED_EDGE('',*,*,#16304,.T.) ;
#21927 = ORIENTED_EDGE('',*,*,#16498,.F.) ;
#21928 = ORIENTED_EDGE('',*,*,#16499,.F.) ;
#21929 = ORIENTED_EDGE('',*,*,#16500,.F.) ;
#21930 = ORIENTED_EDGE('',*,*,#16501,.F.) ;
#21931 = ORIENTED_EDGE('',*,*,#16502,.F.) ;
#21932 = ORIENTED_EDGE('',*,*,#16503,.F.) ;
#21933 = ORIENTED_EDGE('',*,*,#16504,.F.) ;
#21934 = ORIENTED_EDGE('',*,*,#16505,.F.) ;
#21935 = ORIENTED_EDGE('',*,*,#16506,.F.) ;
#21936 = ORIENTED_EDGE('',*,*,#16507,.F.) ;
#21937 = ORIENTED_EDGE('',*,*,#16508,.F.) ;
#21938 = ORIENTED_EDGE('',*,*,#16509,.F.) ;
#21939 = ORIENTED_EDGE('',*,*,#16510,.F.) ;
#21940 = ORIENTED_EDGE('',*,*,#16511,.F.) ;
#21941 = ORIENTED_EDGE('',*,*,#16512,.F.) ;
#21942 = ORIENTED_EDGE('',*,*,#16513,.T.) ;
#21943 = ORIENTED_EDGE('',*,*,#16514,.T.) ;
#21944 = ORIENTED_EDGE('',*,*,#16515,.T.) ;
#21945 = ORIENTED_EDGE('',*,*,#16456,.T.) ;
#21946 = ORIENTED_EDGE('',*,*,#16440,.T.) ;
#21947 = ORIENTED_EDGE('',*,*,#16516,.F.) ;
#21948 = ORIENTED_EDGE('',*,*,#16444,.T.) ;
#21949 = ORIENTED_EDGE('',*,*,#16517,.F.) ;
#21950 = ORIENTED_EDGE('',*,*,#16518,.F.) ;
#21951 = ORIENTED_EDGE('',*,*,#16519,.F.) ;
#21952 = ORIENTED_EDGE('',*,*,#16515,.F.) ;
#21953 = ORIENTED_EDGE('',*,*,#16520,.T.) ;
#21954 = ORIENTED_EDGE('',*,*,#16521,.T.) ;
#21955 = ORIENTED_EDGE('',*,*,#16522,.T.) ;
#21956 = ORIENTED_EDGE('',*,*,#16523,.F.) ;
#21957 = ORIENTED_EDGE('',*,*,#16524,.T.) ;
#21958 = ORIENTED_EDGE('',*,*,#16525,.T.) ;
#21959 = ORIENTED_EDGE('',*,*,#16526,.T.) ;
#21960 = ORIENTED_EDGE('',*,*,#16527,.F.) ;
#21961 = ORIENTED_EDGE('',*,*,#16528,.T.) ;
#21962 = ORIENTED_EDGE('',*,*,#16529,.T.) ;
#21963 = ORIENTED_EDGE('',*,*,#16530,.T.) ;
#21964 = ORIENTED_EDGE('',*,*,#16531,.F.) ;
#21965 = ORIENTED_EDGE('',*,*,#16532,.T.) ;
#21966 = ORIENTED_EDGE('',*,*,#16533,.T.) ;
#21967 = ORIENTED_EDGE('',*,*,#16534,.T.) ;
#21968 = ORIENTED_EDGE('',*,*,#16429,.F.) ;
#21969 = ORIENTED_EDGE('',*,*,#16535,.F.) ;
#21970 = ORIENTED_EDGE('',*,*,#16536,.F.) ;
#21971 = ORIENTED_EDGE('',*,*,#16537,.F.) ;
#21972 = ORIENTED_EDGE('',*,*,#16538,.F.) ;
#21973 = ORIENTED_EDGE('',*,*,#16539,.F.) ;
#21974 = ORIENTED_EDGE('',*,*,#16540,.F.) ;
#21975 = ORIENTED_EDGE('',*,*,#16541,.F.) ;
#21976 = ORIENTED_EDGE('',*,*,#16542,.F.) ;
#21977 = ORIENTED_EDGE('',*,*,#16543,.F.) ;
#21978 = ORIENTED_EDGE('',*,*,#16544,.F.) ;
#21979 = ORIENTED_EDGE('',*,*,#16545,.F.) ;
#21980 = ORIENTED_EDGE('',*,*,#16546,.F.) ;
#21981 = ORIENTED_EDGE('',*,*,#16547,.F.) ;
#21982 = ORIENTED_EDGE('',*,*,#16548,.F.) ;
#21983 = ORIENTED_EDGE('',*,*,#16549,.F.) ;
#21984 = ORIENTED_EDGE('',*,*,#16550,.F.) ;
#21985 = ORIENTED_EDGE('',*,*,#16551,.F.) ;
#21986 = ORIENTED_EDGE('',*,*,#16552,.F.) ;
#21987 = ORIENTED_EDGE('',*,*,#16553,.T.) ;
#21988 = ORIENTED_EDGE('',*,*,#16554,.T.) ;
#21989 = ORIENTED_EDGE('',*,*,#16369,.T.) ;
#21990 = ORIENTED_EDGE('',*,*,#16373,.T.) ;
#21991 = ORIENTED_EDGE('',*,*,#16555,.T.) ;
#21992 = ORIENTED_EDGE('',*,*,#16357,.T.) ;
#21993 = ORIENTED_EDGE('',*,*,#16556,.T.) ;
#21994 = ORIENTED_EDGE('',*,*,#16557,.T.) ;
#21995 = ORIENTED_EDGE('',*,*,#16382,.T.) ;
#21996 = ORIENTED_EDGE('',*,*,#16386,.T.) ;
#21997 = ORIENTED_EDGE('',*,*,#16558,.T.) ;
#21998 = ORIENTED_EDGE('',*,*,#16344,.T.) ;
#21999 = ORIENTED_EDGE('',*,*,#16559,.T.) ;
#22000 = ORIENTED_EDGE('',*,*,#16560,.F.) ;
#22001 = ORIENTED_EDGE('',*,*,#16561,.T.) ;
#22002 = ORIENTED_EDGE('',*,*,#16562,.F.) ;
#22003 = ORIENTED_EDGE('',*,*,#16563,.T.) ;
#22004 = ORIENTED_EDGE('',*,*,#16564,.F.) ;
#22005 = ORIENTED_EDGE('',*,*,#16565,.T.) ;
#22006 = ORIENTED_EDGE('',*,*,#16566,.F.) ;
#22007 = ORIENTED_EDGE('',*,*,#16567,.T.) ;
#22008 = ORIENTED_EDGE('',*,*,#16568,.F.) ;
#22009 = ORIENTED_EDGE('',*,*,#16569,.T.) ;
#22010 = ORIENTED_EDGE('',*,*,#16570,.F.) ;
#22011 = ORIENTED_EDGE('',*,*,#16571,.T.) ;
#22012 = ORIENTED_EDGE('',*,*,#16572,.F.) ;
#22013 = ORIENTED_EDGE('',*,*,#16573,.F.) ;
#22014 = ORIENTED_EDGE('',*,*,#16574,.F.) ;
#22015 = ORIENTED_EDGE('',*,*,#16575,.F.) ;
#22016 = ORIENTED_EDGE('',*,*,#16576,.F.) ;
#22017 = ORIENTED_EDGE('',*,*,#16434,.T.) ;
#22018 = ORIENTED_EDGE('',*,*,#16577,.F.) ;
#22019 = ORIENTED_EDGE('',*,*,#16578,.F.) ;
#22020 = ORIENTED_EDGE('',*,*,#16579,.F.) ;
#22021 = ORIENTED_EDGE('',*,*,#16580,.T.) ;
#22022 = ORIENTED_EDGE('',*,*,#16581,.T.) ;
#22023 = ORIENTED_EDGE('',*,*,#16582,.T.) ;
#22024 = ORIENTED_EDGE('',*,*,#16583,.F.) ;
#22025 = ORIENTED_EDGE('',*,*,#16584,.F.) ;
#22026 = ORIENTED_EDGE('',*,*,#16585,.T.) ;
#22027 = ORIENTED_EDGE('',*,*,#16586,.T.) ;
#22028 = ORIENTED_EDGE('',*,*,#16587,.T.) ;
#22029 = ORIENTED_EDGE('',*,*,#16588,.T.) ;
#22030 = ORIENTED_EDGE('',*,*,#16451,.T.) ;
#22031 = ORIENTED_EDGE('',*,*,#16438,.T.) ;
#22032 = ORIENTED_EDGE('',*,*,#16589,.F.) ;
#22033 = ORIENTED_EDGE('',*,*,#16590,.F.) ;
#22034 = ORIENTED_EDGE('',*,*,#16591,.F.) ;
#22035 = ORIENTED_EDGE('',*,*,#16592,.F.) ;
#22036 = ORIENTED_EDGE('',*,*,#16593,.F.) ;
#22037 = ORIENTED_EDGE('',*,*,#16594,.F.) ;
#22038 = ORIENTED_EDGE('',*,*,#16595,.F.) ;
#22039 = ORIENTED_EDGE('',*,*,#16596,.F.) ;
#22040 = ORIENTED_EDGE('',*,*,#16597,.F.) ;
#22041 = ORIENTED_EDGE('',*,*,#16598,.F.) ;
#22042 = ORIENTED_EDGE('',*,*,#16599,.F.) ;
#22043 = ORIENTED_EDGE('',*,*,#16600,.F.) ;
#22044 = ORIENTED_EDGE('',*,*,#16601,.F.) ;
#22045 = ORIENTED_EDGE('',*,*,#16602,.F.) ;
#22046 = ORIENTED_EDGE('',*,*,#16603,.T.) ;
#22047 = ORIENTED_EDGE('',*,*,#16604,.F.) ;
#22048 = ORIENTED_EDGE('',*,*,#16605,.T.) ;
#22049 = ORIENTED_EDGE('',*,*,#16606,.F.) ;
#22050 = ORIENTED_EDGE('',*,*,#16607,.F.) ;
#22051 = ORIENTED_EDGE('',*,*,#16608,.F.) ;
#22052 = ORIENTED_EDGE('',*,*,#16609,.F.) ;
#22053 = ORIENTED_EDGE('',*,*,#16610,.T.) ;
#22054 = ORIENTED_EDGE('',*,*,#16300,.T.) ;
#22055 = ORIENTED_EDGE('',*,*,#16611,.T.) ;
#22056 = ORIENTED_EDGE('',*,*,#16612,.T.) ;
#22057 = ORIENTED_EDGE('',*,*,#16339,.T.) ;
#22058 = ORIENTED_EDGE('',*,*,#16613,.T.) ;
#22059 = ORIENTED_EDGE('',*,*,#16313,.T.) ;
#22060 = ORIENTED_EDGE('',*,*,#16614,.T.) ;
#22061 = ORIENTED_EDGE('',*,*,#16615,.T.) ;
#22062 = ORIENTED_EDGE('',*,*,#16326,.T.) ;
#22063 = ORIENTED_EDGE('',*,*,#16455,.T.) ;
#22064 = ORIENTED_EDGE('',*,*,#16616,.F.) ;
#22065 = ORIENTED_EDGE('',*,*,#16617,.T.) ;
#22066 = ORIENTED_EDGE('',*,*,#16618,.T.) ;
#22067 = ORIENTED_EDGE('',*,*,#16619,.T.) ;
#22068 = ORIENTED_EDGE('',*,*,#16620,.T.) ;
#22069 = ORIENTED_EDGE('',*,*,#16621,.T.) ;
#22070 = ORIENTED_EDGE('',*,*,#16622,.T.) ;
#22071 = ORIENTED_EDGE('',*,*,#16623,.F.) ;
#22072 = ORIENTED_EDGE('',*,*,#16624,.F.) ;
#22073 = ORIENTED_EDGE('',*,*,#16625,.T.) ;
#22074 = ORIENTED_EDGE('',*,*,#16626,.T.) ;
#22075 = ORIENTED_EDGE('',*,*,#16627,.T.) ;
#22076 = ORIENTED_EDGE('',*,*,#16628,.F.) ;
#22077 = ORIENTED_EDGE('',*,*,#16629,.T.) ;
#22078 = ORIENTED_EDGE('',*,*,#16630,.T.) ;
#22079 = ORIENTED_EDGE('',*,*,#16631,.T.) ;
#22080 = ORIENTED_EDGE('',*,*,#16632,.F.) ;
#22081 = ORIENTED_EDGE('',*,*,#16633,.F.) ;
#22082 = ORIENTED_EDGE('',*,*,#16634,.F.) ;
#22083 = ORIENTED_EDGE('',*,*,#16635,.F.) ;
#22084 = ORIENTED_EDGE('',*,*,#16446,.T.) ;
#22085 = ORIENTED_EDGE('',*,*,#16636,.F.) ;
#22086 = ORIENTED_EDGE('',*,*,#16442,.T.) ;
#22087 = ORIENTED_EDGE('',*,*,#16637,.F.) ;
#22088 = ORIENTED_EDGE('',*,*,#16638,.F.) ;
#22089 = ORIENTED_EDGE('',*,*,#16639,.F.) ;
#22090 = ORIENTED_EDGE('',*,*,#16640,.F.) ;
#22091 = ORIENTED_EDGE('',*,*,#16641,.F.) ;
#22092 = ORIENTED_EDGE('',*,*,#16642,.F.) ;
#22093 = ORIENTED_EDGE('',*,*,#16643,.F.) ;
#22094 = ORIENTED_EDGE('',*,*,#16644,.F.) ;
#22095 = ORIENTED_EDGE('',*,*,#16645,.T.) ;
#22096 = ORIENTED_EDGE('',*,*,#16366,.T.) ;
#22097 = ORIENTED_EDGE('',*,*,#16646,.T.) ;
#22098 = ORIENTED_EDGE('',*,*,#16647,.T.) ;
#22099 = ORIENTED_EDGE('',*,*,#16378,.T.) ;
#22100 = ORIENTED_EDGE('',*,*,#16648,.T.) ;
#22101 = ORIENTED_EDGE('',*,*,#16353,.T.) ;
#22102 = ORIENTED_EDGE('',*,*,#16649,.T.) ;
#22103 = ORIENTED_EDGE('',*,*,#16650,.T.) ;
#22104 = ORIENTED_EDGE('',*,*,#16391,.T.) ;
#22105 = ORIENTED_EDGE('',*,*,#16651,.T.) ;
#22106 = ORIENTED_EDGE('',*,*,#16652,.F.) ;
#22107 = ORIENTED_EDGE('',*,*,#16653,.T.) ;
#22108 = ORIENTED_EDGE('',*,*,#16654,.F.) ;
#22109 = ORIENTED_EDGE('',*,*,#16655,.F.) ;
#22110 = ORIENTED_EDGE('',*,*,#16656,.F.) ;
#22111 = ORIENTED_EDGE('',*,*,#16657,.F.) ;
#22112 = ORIENTED_EDGE('',*,*,#16658,.F.) ;
#22113 = ORIENTED_EDGE('',*,*,#16659,.F.) ;
#22114 = ORIENTED_EDGE('',*,*,#16660,.F.) ;
#22115 = ORIENTED_EDGE('',*,*,#16661,.F.) ;
#22116 = ORIENTED_EDGE('',*,*,#16662,.F.) ;
#22117 = ORIENTED_EDGE('',*,*,#16663,.F.) ;
#22118 = ORIENTED_EDGE('',*,*,#16664,.F.) ;
#22119 = ORIENTED_EDGE('',*,*,#16665,.F.) ;
#22120 = ORIENTED_EDGE('',*,*,#16666,.F.) ;
#22121 = ORIENTED_EDGE('',*,*,#16667,.F.) ;
#22122 = ORIENTED_EDGE('',*,*,#16668,.F.) ;
#22123 = ORIENTED_EDGE('',*,*,#16669,.F.) ;
#22124 = ORIENTED_EDGE('',*,*,#16670,.F.) ;
#22125 = ORIENTED_EDGE('',*,*,#16671,.F.) ;
#22126 = ORIENTED_EDGE('',*,*,#16672,.F.) ;
#22127 = ORIENTED_EDGE('',*,*,#16673,.F.) ;
#22128 = ORIENTED_EDGE('',*,*,#16674,.F.) ;
#22129 = ORIENTED_EDGE('',*,*,#16675,.T.) ;
#22130 = ORIENTED_EDGE('',*,*,#16676,.F.) ;
#22131 = ORIENTED_EDGE('',*,*,#16677,.F.) ;
#22132 = ORIENTED_EDGE('',*,*,#16678,.T.) ;
#22133 = ORIENTED_EDGE('',*,*,#16512,.T.) ;
#22134 = ORIENTED_EDGE('',*,*,#16519,.T.) ;
#22135 = ORIENTED_EDGE('',*,*,#16679,.T.) ;
#22136 = ORIENTED_EDGE('',*,*,#16633,.T.) ;
#22137 = ORIENTED_EDGE('',*,*,#16680,.T.) ;
#22138 = ORIENTED_EDGE('',*,*,#16464,.F.) ;
#22139 = ORIENTED_EDGE('',*,*,#16681,.T.) ;
#22140 = ORIENTED_EDGE('',*,*,#16682,.T.) ;
#22141 = ORIENTED_EDGE('',*,*,#16683,.T.) ;
#22142 = ORIENTED_EDGE('',*,*,#16684,.F.) ;
#22143 = ORIENTED_EDGE('',*,*,#16685,.T.) ;
#22144 = ORIENTED_EDGE('',*,*,#16686,.T.) ;
#22145 = ORIENTED_EDGE('',*,*,#16632,.T.) ;
#22146 = ORIENTED_EDGE('',*,*,#16687,.F.) ;
#22147 = ORIENTED_EDGE('',*,*,#16688,.F.) ;
#22148 = ORIENTED_EDGE('',*,*,#16675,.F.) ;
#22149 = ORIENTED_EDGE('',*,*,#16689,.F.) ;
#22150 = ORIENTED_EDGE('',*,*,#16690,.F.) ;
#22151 = ORIENTED_EDGE('',*,*,#16616,.T.) ;
#22152 = ORIENTED_EDGE('',*,*,#16454,.T.) ;
#22153 = ORIENTED_EDGE('',*,*,#16588,.F.) ;
#22154 = ORIENTED_EDGE('',*,*,#16691,.F.) ;
#22155 = ORIENTED_EDGE('',*,*,#16692,.T.) ;
#22156 = ORIENTED_EDGE('',*,*,#16452,.T.) ;
#22157 = ORIENTED_EDGE('',*,*,#16474,.T.) ;
#22158 = ORIENTED_EDGE('',*,*,#16693,.T.) ;
#22159 = ORIENTED_EDGE('',*,*,#16694,.F.) ;
#22160 = ORIENTED_EDGE('',*,*,#16695,.F.) ;
#22161 = ORIENTED_EDGE('',*,*,#16447,.F.) ;
#22162 = ORIENTED_EDGE('',*,*,#16635,.T.) ;
#22163 = ORIENTED_EDGE('',*,*,#16696,.T.) ;
#22164 = ORIENTED_EDGE('',*,*,#16517,.T.) ;
#22165 = ORIENTED_EDGE('',*,*,#16697,.T.) ;
#22166 = ORIENTED_EDGE('',*,*,#16698,.T.) ;
#22167 = ORIENTED_EDGE('',*,*,#16699,.T.) ;
#22168 = ORIENTED_EDGE('',*,*,#16684,.T.) ;
#22169 = ORIENTED_EDGE('',*,*,#16700,.T.) ;
#22170 = ORIENTED_EDGE('',*,*,#16685,.F.) ;
#22171 = ORIENTED_EDGE('',*,*,#16699,.F.) ;
#22172 = ORIENTED_EDGE('',*,*,#16701,.F.) ;
#22173 = ORIENTED_EDGE('',*,*,#16702,.T.) ;
#22174 = ORIENTED_EDGE('',*,*,#16703,.F.) ;
#22175 = ORIENTED_EDGE('',*,*,#16697,.F.) ;
#22176 = ORIENTED_EDGE('',*,*,#16683,.F.) ;
#22177 = ORIENTED_EDGE('',*,*,#16704,.F.) ;
#22178 = ORIENTED_EDGE('',*,*,#16686,.F.) ;
#22179 = ORIENTED_EDGE('',*,*,#16700,.F.) ;
#22180 = ORIENTED_EDGE('',*,*,#16705,.F.) ;
#22181 = ORIENTED_EDGE('',*,*,#16457,.T.) ;
#22182 = ORIENTED_EDGE('',*,*,#16706,.F.) ;
#22183 = ORIENTED_EDGE('',*,*,#16707,.T.) ;
#22184 = ORIENTED_EDGE('',*,*,#16461,.F.) ;
#22185 = ORIENTED_EDGE('',*,*,#16680,.F.) ;
#22186 = ORIENTED_EDGE('',*,*,#16704,.T.) ;
#22187 = ORIENTED_EDGE('',*,*,#16708,.F.) ;
#22188 = ORIENTED_EDGE('',*,*,#16709,.T.) ;
#22189 = ORIENTED_EDGE('',*,*,#16707,.F.) ;
#22190 = ORIENTED_EDGE('',*,*,#16710,.F.) ;
#22191 = ORIENTED_EDGE('',*,*,#16711,.T.) ;
#22192 = ORIENTED_EDGE('',*,*,#16579,.T.) ;
#22193 = ORIENTED_EDGE('',*,*,#16712,.T.) ;
#22194 = ORIENTED_EDGE('',*,*,#16475,.T.) ;
#22195 = ORIENTED_EDGE('',*,*,#16695,.T.) ;
#22196 = ORIENTED_EDGE('',*,*,#16634,.T.) ;
#22197 = ORIENTED_EDGE('',*,*,#16679,.F.) ;
#22198 = ORIENTED_EDGE('',*,*,#16518,.T.) ;
#22199 = ORIENTED_EDGE('',*,*,#16696,.F.) ;
#22200 = ORIENTED_EDGE('',*,*,#16476,.T.) ;
#22201 = ORIENTED_EDGE('',*,*,#16712,.F.) ;
#22202 = ORIENTED_EDGE('',*,*,#16578,.T.) ;
#22203 = ORIENTED_EDGE('',*,*,#16713,.F.) ;
#22204 = ORIENTED_EDGE('',*,*,#16677,.T.) ;
#22205 = ORIENTED_EDGE('',*,*,#16714,.F.) ;
#22206 = ORIENTED_EDGE('',*,*,#16459,.T.) ;
#22207 = ORIENTED_EDGE('',*,*,#16715,.F.) ;
#22208 = ORIENTED_EDGE('',*,*,#16716,.T.) ;
#22209 = ORIENTED_EDGE('',*,*,#16681,.F.) ;
#22210 = ORIENTED_EDGE('',*,*,#16463,.T.) ;
#22211 = ORIENTED_EDGE('',*,*,#16716,.F.) ;
#22212 = ORIENTED_EDGE('',*,*,#16717,.F.) ;
#22213 = ORIENTED_EDGE('',*,*,#16702,.F.) ;
#22214 = ORIENTED_EDGE('',*,*,#16682,.F.) ;
#22215 = ORIENTED_EDGE('',*,*,#16718,.T.) ;
#22216 = ORIENTED_EDGE('',*,*,#16719,.T.) ;
#22217 = ORIENTED_EDGE('',*,*,#16720,.T.) ;
#22218 = ORIENTED_EDGE('',*,*,#16491,.T.) ;
#22219 = ORIENTED_EDGE('',*,*,#16719,.F.) ;
#22220 = ORIENTED_EDGE('',*,*,#16721,.T.) ;
#22221 = ORIENTED_EDGE('',*,*,#16722,.F.) ;
#22222 = ORIENTED_EDGE('',*,*,#16723,.F.) ;
#22223 = ORIENTED_EDGE('',*,*,#16724,.T.) ;
#22224 = ORIENTED_EDGE('',*,*,#16483,.T.) ;
#22225 = ORIENTED_EDGE('',*,*,#16725,.T.) ;
#22226 = ORIENTED_EDGE('',*,*,#16726,.T.) ;
#22227 = ORIENTED_EDGE('',*,*,#16727,.T.) ;
#22228 = ORIENTED_EDGE('',*,*,#16484,.T.) ;
#22229 = ORIENTED_EDGE('',*,*,#16724,.F.) ;
#22230 = ORIENTED_EDGE('',*,*,#16728,.T.) ;
#22231 = ORIENTED_EDGE('',*,*,#16729,.T.) ;
#22232 = ORIENTED_EDGE('',*,*,#16485,.T.) ;
#22233 = ORIENTED_EDGE('',*,*,#16727,.F.) ;
#22234 = ORIENTED_EDGE('',*,*,#16730,.T.) ;
#22235 = ORIENTED_EDGE('',*,*,#16731,.T.) ;
#22236 = ORIENTED_EDGE('',*,*,#16486,.T.) ;
#22237 = ORIENTED_EDGE('',*,*,#16729,.F.) ;
#22238 = ORIENTED_EDGE('',*,*,#16732,.T.) ;
#22239 = ORIENTED_EDGE('',*,*,#16733,.F.) ;
#22240 = ORIENTED_EDGE('',*,*,#16487,.T.) ;
#22241 = ORIENTED_EDGE('',*,*,#16731,.F.) ;
#22242 = ORIENTED_EDGE('',*,*,#16734,.T.) ;
#22243 = ORIENTED_EDGE('',*,*,#16734,.F.) ;
#22244 = ORIENTED_EDGE('',*,*,#16735,.F.) ;
#22245 = ORIENTED_EDGE('',*,*,#16736,.F.) ;
#22246 = ORIENTED_EDGE('',*,*,#16737,.T.) ;
#22247 = ORIENTED_EDGE('',*,*,#16732,.F.) ;
#22248 = ORIENTED_EDGE('',*,*,#16738,.T.) ;
#22249 = ORIENTED_EDGE('',*,*,#16739,.F.) ;
#22250 = ORIENTED_EDGE('',*,*,#16735,.T.) ;
#22251 = ORIENTED_EDGE('',*,*,#16730,.F.) ;
#22252 = ORIENTED_EDGE('',*,*,#16740,.F.) ;
#22253 = ORIENTED_EDGE('',*,*,#16741,.F.) ;
#22254 = ORIENTED_EDGE('',*,*,#16738,.F.) ;
#22255 = ORIENTED_EDGE('',*,*,#16728,.F.) ;
#22256 = ORIENTED_EDGE('',*,*,#16742,.T.) ;
#22257 = ORIENTED_EDGE('',*,*,#16743,.F.) ;
#22258 = ORIENTED_EDGE('',*,*,#16740,.T.) ;
#22259 = ORIENTED_EDGE('',*,*,#16726,.F.) ;
#22260 = ORIENTED_EDGE('',*,*,#16744,.T.) ;
#22261 = ORIENTED_EDGE('',*,*,#16745,.F.) ;
#22262 = ORIENTED_EDGE('',*,*,#16742,.F.) ;
#22263 = ORIENTED_EDGE('',*,*,#16746,.T.) ;
#22264 = ORIENTED_EDGE('',*,*,#16572,.T.) ;
#22265 = ORIENTED_EDGE('',*,*,#16747,.T.) ;
#22266 = ORIENTED_EDGE('',*,*,#16748,.T.) ;
#22267 = ORIENTED_EDGE('',*,*,#16749,.T.) ;
#22268 = ORIENTED_EDGE('',*,*,#16573,.T.) ;
#22269 = ORIENTED_EDGE('',*,*,#16746,.F.) ;
#22270 = ORIENTED_EDGE('',*,*,#16750,.T.) ;
#22271 = ORIENTED_EDGE('',*,*,#16751,.T.) ;
#22272 = ORIENTED_EDGE('',*,*,#16574,.T.) ;
#22273 = ORIENTED_EDGE('',*,*,#16749,.F.) ;
#22274 = ORIENTED_EDGE('',*,*,#16752,.T.) ;
#22275 = ORIENTED_EDGE('',*,*,#16753,.T.) ;
#22276 = ORIENTED_EDGE('',*,*,#16575,.T.) ;
#22277 = ORIENTED_EDGE('',*,*,#16751,.F.) ;
#22278 = ORIENTED_EDGE('',*,*,#16754,.T.) ;
#22279 = ORIENTED_EDGE('',*,*,#16755,.T.) ;
#22280 = ORIENTED_EDGE('',*,*,#16576,.T.) ;
#22281 = ORIENTED_EDGE('',*,*,#16753,.F.) ;
#22282 = ORIENTED_EDGE('',*,*,#16756,.T.) ;
#22283 = ORIENTED_EDGE('',*,*,#16756,.F.) ;
#22284 = ORIENTED_EDGE('',*,*,#16757,.F.) ;
#22285 = ORIENTED_EDGE('',*,*,#16758,.F.) ;
#22286 = ORIENTED_EDGE('',*,*,#16759,.T.) ;
#22287 = ORIENTED_EDGE('',*,*,#16754,.F.) ;
#22288 = ORIENTED_EDGE('',*,*,#16760,.T.) ;
#22289 = ORIENTED_EDGE('',*,*,#16761,.F.) ;
#22290 = ORIENTED_EDGE('',*,*,#16757,.T.) ;
#22291 = ORIENTED_EDGE('',*,*,#16752,.F.) ;
#22292 = ORIENTED_EDGE('',*,*,#16762,.F.) ;
#22293 = ORIENTED_EDGE('',*,*,#16763,.F.) ;
#22294 = ORIENTED_EDGE('',*,*,#16760,.F.) ;
#22295 = ORIENTED_EDGE('',*,*,#16750,.F.) ;
#22296 = ORIENTED_EDGE('',*,*,#16764,.T.) ;
#22297 = ORIENTED_EDGE('',*,*,#16765,.F.) ;
#22298 = ORIENTED_EDGE('',*,*,#16762,.T.) ;
#22299 = ORIENTED_EDGE('',*,*,#16748,.F.) ;
#22300 = ORIENTED_EDGE('',*,*,#16766,.T.) ;
#22301 = ORIENTED_EDGE('',*,*,#16767,.F.) ;
#22302 = ORIENTED_EDGE('',*,*,#16764,.F.) ;
#22303 = ORIENTED_EDGE('',*,*,#16768,.F.) ;
#22304 = ORIENTED_EDGE('',*,*,#16769,.T.) ;
#22305 = ORIENTED_EDGE('',*,*,#16770,.F.) ;
#22306 = ORIENTED_EDGE('',*,*,#16771,.F.) ;
#22307 = ORIENTED_EDGE('',*,*,#16772,.F.) ;
#22308 = ORIENTED_EDGE('',*,*,#16771,.T.) ;
#22309 = ORIENTED_EDGE('',*,*,#16773,.F.) ;
#22310 = ORIENTED_EDGE('',*,*,#16774,.F.) ;
#22311 = ORIENTED_EDGE('',*,*,#16775,.F.) ;
#22312 = ORIENTED_EDGE('',*,*,#16774,.T.) ;
#22313 = ORIENTED_EDGE('',*,*,#16776,.F.) ;
#22314 = ORIENTED_EDGE('',*,*,#16777,.F.) ;
#22315 = ORIENTED_EDGE('',*,*,#16778,.F.) ;
#22316 = ORIENTED_EDGE('',*,*,#16777,.T.) ;
#22317 = ORIENTED_EDGE('',*,*,#16779,.F.) ;
#22318 = ORIENTED_EDGE('',*,*,#16780,.F.) ;
#22319 = ORIENTED_EDGE('',*,*,#16781,.F.) ;
#22320 = ORIENTED_EDGE('',*,*,#16782,.T.) ;
#22321 = ORIENTED_EDGE('',*,*,#16783,.F.) ;
#22322 = ORIENTED_EDGE('',*,*,#16769,.F.) ;
#22323 = ORIENTED_EDGE('',*,*,#16784,.F.) ;
#22324 = ORIENTED_EDGE('',*,*,#16780,.T.) ;
#22325 = ORIENTED_EDGE('',*,*,#16785,.F.) ;
#22326 = ORIENTED_EDGE('',*,*,#16782,.F.) ;
#22327 = ORIENTED_EDGE('',*,*,#16786,.F.) ;
#22328 = ORIENTED_EDGE('',*,*,#16787,.T.) ;
#22329 = ORIENTED_EDGE('',*,*,#16788,.F.) ;
#22330 = ORIENTED_EDGE('',*,*,#16789,.F.) ;
#22331 = ORIENTED_EDGE('',*,*,#16790,.F.) ;
#22332 = ORIENTED_EDGE('',*,*,#16789,.T.) ;
#22333 = ORIENTED_EDGE('',*,*,#16791,.F.) ;
#22334 = ORIENTED_EDGE('',*,*,#16792,.F.) ;
#22335 = ORIENTED_EDGE('',*,*,#16793,.F.) ;
#22336 = ORIENTED_EDGE('',*,*,#16792,.T.) ;
#22337 = ORIENTED_EDGE('',*,*,#16794,.F.) ;
#22338 = ORIENTED_EDGE('',*,*,#16795,.F.) ;
#22339 = ORIENTED_EDGE('',*,*,#16796,.F.) ;
#22340 = ORIENTED_EDGE('',*,*,#16795,.T.) ;
#22341 = ORIENTED_EDGE('',*,*,#16797,.F.) ;
#22342 = ORIENTED_EDGE('',*,*,#16798,.F.) ;
#22343 = ORIENTED_EDGE('',*,*,#16799,.F.) ;
#22344 = ORIENTED_EDGE('',*,*,#16800,.T.) ;
#22345 = ORIENTED_EDGE('',*,*,#16801,.F.) ;
#22346 = ORIENTED_EDGE('',*,*,#16787,.F.) ;
#22347 = ORIENTED_EDGE('',*,*,#16802,.F.) ;
#22348 = ORIENTED_EDGE('',*,*,#16798,.T.) ;
#22349 = ORIENTED_EDGE('',*,*,#16803,.F.) ;
#22350 = ORIENTED_EDGE('',*,*,#16800,.F.) ;
#22351 = ORIENTED_EDGE('',*,*,#16433,.F.) ;
#22352 = ORIENTED_EDGE('',*,*,#16477,.T.) ;
#22353 = ORIENTED_EDGE('',*,*,#16713,.T.) ;
#22354 = ORIENTED_EDGE('',*,*,#16577,.T.) ;
#22355 = ORIENTED_EDGE('',*,*,#16458,.F.) ;
#22356 = ORIENTED_EDGE('',*,*,#16708,.T.) ;
#22357 = ORIENTED_EDGE('',*,*,#16705,.T.) ;
#22358 = ORIENTED_EDGE('',*,*,#16701,.T.) ;
#22359 = ORIENTED_EDGE('',*,*,#16698,.F.) ;
#22360 = ORIENTED_EDGE('',*,*,#16703,.T.) ;
#22361 = ORIENTED_EDGE('',*,*,#16717,.T.) ;
#22362 = ORIENTED_EDGE('',*,*,#16715,.T.) ;
#22363 = ORIENTED_EDGE('',*,*,#16804,.T.) ;
#22364 = ORIENTED_EDGE('',*,*,#16523,.T.) ;
#22365 = ORIENTED_EDGE('',*,*,#16805,.T.) ;
#22366 = ORIENTED_EDGE('',*,*,#16806,.T.) ;
#22367 = ORIENTED_EDGE('',*,*,#16807,.T.) ;
#22368 = ORIENTED_EDGE('',*,*,#16470,.T.) ;
#22369 = ORIENTED_EDGE('',*,*,#16808,.T.) ;
#22370 = ORIENTED_EDGE('',*,*,#16809,.T.) ;
#22371 = ORIENTED_EDGE('',*,*,#16810,.T.) ;
#22372 = ORIENTED_EDGE('',*,*,#16811,.T.) ;
#22373 = ORIENTED_EDGE('',*,*,#16466,.T.) ;
#22374 = ORIENTED_EDGE('',*,*,#16449,.T.) ;
#22375 = ORIENTED_EDGE('',*,*,#16812,.T.) ;
#22376 = ORIENTED_EDGE('',*,*,#16531,.T.) ;
#22377 = ORIENTED_EDGE('',*,*,#16813,.T.) ;
#22378 = ORIENTED_EDGE('',*,*,#16814,.T.) ;
#22379 = ORIENTED_EDGE('',*,*,#16815,.T.) ;
#22380 = ORIENTED_EDGE('',*,*,#16816,.T.) ;
#22381 = ORIENTED_EDGE('',*,*,#16817,.T.) ;
#22382 = ORIENTED_EDGE('',*,*,#16527,.T.) ;
#22383 = ORIENTED_EDGE('',*,*,#16818,.F.) ;
#22384 = ORIENTED_EDGE('',*,*,#16819,.F.) ;
#22385 = ORIENTED_EDGE('',*,*,#16820,.F.) ;
#22386 = ORIENTED_EDGE('',*,*,#16687,.T.) ;
#22387 = ORIENTED_EDGE('',*,*,#16631,.F.) ;
#22388 = ORIENTED_EDGE('',*,*,#16821,.F.) ;
#22389 = ORIENTED_EDGE('',*,*,#16520,.F.) ;
#22390 = ORIENTED_EDGE('',*,*,#16514,.F.) ;
#22391 = ORIENTED_EDGE('',*,*,#16822,.T.) ;
#22392 = ORIENTED_EDGE('',*,*,#16823,.T.) ;
#22393 = ORIENTED_EDGE('',*,*,#16609,.T.) ;
#22394 = ORIENTED_EDGE('',*,*,#16823,.F.) ;
#22395 = ORIENTED_EDGE('',*,*,#16511,.T.) ;
#22396 = ORIENTED_EDGE('',*,*,#16824,.T.) ;
#22397 = ORIENTED_EDGE('',*,*,#16822,.F.) ;
#22398 = ORIENTED_EDGE('',*,*,#16824,.F.) ;
#22399 = ORIENTED_EDGE('',*,*,#16825,.T.) ;
#22400 = ORIENTED_EDGE('',*,*,#16826,.T.) ;
#22401 = ORIENTED_EDGE('',*,*,#16673,.T.) ;
#22402 = ORIENTED_EDGE('',*,*,#16826,.F.) ;
#22403 = ORIENTED_EDGE('',*,*,#16825,.F.) ;
#22404 = ORIENTED_EDGE('',*,*,#16827,.T.) ;
#22405 = ORIENTED_EDGE('',*,*,#16552,.T.) ;
#22406 = ORIENTED_EDGE('',*,*,#16827,.F.) ;
#22407 = ORIENTED_EDGE('',*,*,#16828,.T.) ;
#22408 = ORIENTED_EDGE('',*,*,#16829,.T.) ;
#22409 = ORIENTED_EDGE('',*,*,#16590,.T.) ;
#22410 = ORIENTED_EDGE('',*,*,#16829,.F.) ;
#22411 = ORIENTED_EDGE('',*,*,#16498,.T.) ;
#22412 = ORIENTED_EDGE('',*,*,#16830,.T.) ;
#22413 = ORIENTED_EDGE('',*,*,#16828,.F.) ;
#22414 = ORIENTED_EDGE('',*,*,#16830,.F.) ;
#22415 = ORIENTED_EDGE('',*,*,#16831,.T.) ;
#22416 = ORIENTED_EDGE('',*,*,#16832,.F.) ;
#22417 = ORIENTED_EDGE('',*,*,#16567,.F.) ;
#22418 = ORIENTED_EDGE('',*,*,#16755,.F.) ;
#22419 = ORIENTED_EDGE('',*,*,#16759,.F.) ;
#22420 = ORIENTED_EDGE('',*,*,#16833,.T.) ;
#22421 = ORIENTED_EDGE('',*,*,#16766,.F.) ;
#22422 = ORIENTED_EDGE('',*,*,#16747,.F.) ;
#22423 = ORIENTED_EDGE('',*,*,#16571,.F.) ;
#22424 = ORIENTED_EDGE('',*,*,#16834,.T.) ;
#22425 = ORIENTED_EDGE('',*,*,#16835,.F.) ;
#22426 = ORIENTED_EDGE('',*,*,#16836,.T.) ;
#22427 = ORIENTED_EDGE('',*,*,#16837,.T.) ;
#22428 = ORIENTED_EDGE('',*,*,#16838,.T.) ;
#22429 = ORIENTED_EDGE('',*,*,#16836,.F.) ;
#22430 = ORIENTED_EDGE('',*,*,#16838,.F.) ;
#22431 = ORIENTED_EDGE('',*,*,#16839,.T.) ;
#22432 = ORIENTED_EDGE('',*,*,#16840,.T.) ;
#22433 = ORIENTED_EDGE('',*,*,#16839,.F.) ;
#22434 = ORIENTED_EDGE('',*,*,#16837,.F.) ;
#22435 = ORIENTED_EDGE('',*,*,#16841,.F.) ;
#22436 = ORIENTED_EDGE('',*,*,#16842,.T.) ;
#22437 = ORIENTED_EDGE('',*,*,#16843,.F.) ;
#22438 = ORIENTED_EDGE('',*,*,#16844,.T.) ;
#22439 = ORIENTED_EDGE('',*,*,#16845,.F.) ;
#22440 = ORIENTED_EDGE('',*,*,#16846,.T.) ;
#22441 = ORIENTED_EDGE('',*,*,#16847,.F.) ;
#22442 = ORIENTED_EDGE('',*,*,#16848,.T.) ;
#22443 = ORIENTED_EDGE('',*,*,#16849,.F.) ;
#22444 = ORIENTED_EDGE('',*,*,#16850,.T.) ;
#22445 = ORIENTED_EDGE('',*,*,#16851,.F.) ;
#22446 = ORIENTED_EDGE('',*,*,#16852,.T.) ;
#22447 = ORIENTED_EDGE('',*,*,#16853,.F.) ;
#22448 = ORIENTED_EDGE('',*,*,#16854,.T.) ;
#22449 = ORIENTED_EDGE('',*,*,#16855,.F.) ;
#22450 = ORIENTED_EDGE('',*,*,#16856,.T.) ;
#22451 = ORIENTED_EDGE('',*,*,#16857,.T.) ;
#22452 = ORIENTED_EDGE('',*,*,#16819,.T.) ;
#22453 = ORIENTED_EDGE('',*,*,#16858,.F.) ;
#22454 = ORIENTED_EDGE('',*,*,#16859,.T.) ;
#22455 = ORIENTED_EDGE('',*,*,#16860,.T.) ;
#22456 = ORIENTED_EDGE('',*,*,#16861,.T.) ;
#22457 = ORIENTED_EDGE('',*,*,#16862,.F.) ;
#22458 = ORIENTED_EDGE('',*,*,#16863,.T.) ;
#22459 = ORIENTED_EDGE('',*,*,#16864,.T.) ;
#22460 = ORIENTED_EDGE('',*,*,#16653,.F.) ;
#22461 = ORIENTED_EDGE('',*,*,#16865,.T.) ;
#22462 = ORIENTED_EDGE('',*,*,#16866,.F.) ;
#22463 = ORIENTED_EDGE('',*,*,#16570,.T.) ;
#22464 = ORIENTED_EDGE('',*,*,#16867,.F.) ;
#22465 = ORIENTED_EDGE('',*,*,#16654,.T.) ;
#22466 = ORIENTED_EDGE('',*,*,#16864,.F.) ;
#22467 = ORIENTED_EDGE('',*,*,#16868,.T.) ;
#22468 = ORIENTED_EDGE('',*,*,#16834,.F.) ;
#22469 = ORIENTED_EDGE('',*,*,#16525,.F.) ;
#22470 = ORIENTED_EDGE('',*,*,#16869,.T.) ;
#22471 = ORIENTED_EDGE('',*,*,#16626,.F.) ;
#22472 = ORIENTED_EDGE('',*,*,#16870,.T.) ;
#22473 = ORIENTED_EDGE('',*,*,#16622,.F.) ;
#22474 = ORIENTED_EDGE('',*,*,#16871,.T.) ;
#22475 = ORIENTED_EDGE('',*,*,#16529,.F.) ;
#22476 = ORIENTED_EDGE('',*,*,#16872,.T.) ;
#22477 = ORIENTED_EDGE('',*,*,#16618,.F.) ;
#22478 = ORIENTED_EDGE('',*,*,#16873,.T.) ;
#22479 = ORIENTED_EDGE('',*,*,#16533,.F.) ;
#22480 = ORIENTED_EDGE('',*,*,#16874,.T.) ;
#22481 = ORIENTED_EDGE('',*,*,#16445,.F.) ;
#22482 = ORIENTED_EDGE('',*,*,#16516,.T.) ;
#22483 = ORIENTED_EDGE('',*,*,#16443,.F.) ;
#22484 = ORIENTED_EDGE('',*,*,#16636,.T.) ;
#22485 = ORIENTED_EDGE('',*,*,#16521,.F.) ;
#22486 = ORIENTED_EDGE('',*,*,#16821,.T.) ;
#22487 = ORIENTED_EDGE('',*,*,#16630,.F.) ;
#22488 = ORIENTED_EDGE('',*,*,#16875,.T.) ;
#22489 = ORIENTED_EDGE('',*,*,#16876,.F.) ;
#22490 = ORIENTED_EDGE('',*,*,#16672,.T.) ;
#22491 = ORIENTED_EDGE('',*,*,#16877,.F.) ;
#22492 = ORIENTED_EDGE('',*,*,#16543,.T.) ;
#22493 = ORIENTED_EDGE('',*,*,#16877,.T.) ;
#22494 = ORIENTED_EDGE('',*,*,#16671,.T.) ;
#22495 = ORIENTED_EDGE('',*,*,#16878,.F.) ;
#22496 = ORIENTED_EDGE('',*,*,#16540,.T.) ;
#22497 = ORIENTED_EDGE('',*,*,#16878,.T.) ;
#22498 = ORIENTED_EDGE('',*,*,#16670,.T.) ;
#22499 = ORIENTED_EDGE('',*,*,#16879,.F.) ;
#22500 = ORIENTED_EDGE('',*,*,#16541,.T.) ;
#22501 = ORIENTED_EDGE('',*,*,#16879,.T.) ;
#22502 = ORIENTED_EDGE('',*,*,#16669,.T.) ;
#22503 = ORIENTED_EDGE('',*,*,#16876,.T.) ;
#22504 = ORIENTED_EDGE('',*,*,#16542,.T.) ;
#22505 = ORIENTED_EDGE('',*,*,#16880,.F.) ;
#22506 = ORIENTED_EDGE('',*,*,#16668,.T.) ;
#22507 = ORIENTED_EDGE('',*,*,#16881,.F.) ;
#22508 = ORIENTED_EDGE('',*,*,#16547,.T.) ;
#22509 = ORIENTED_EDGE('',*,*,#16881,.T.) ;
#22510 = ORIENTED_EDGE('',*,*,#16667,.T.) ;
#22511 = ORIENTED_EDGE('',*,*,#16882,.F.) ;
#22512 = ORIENTED_EDGE('',*,*,#16544,.T.) ;
#22513 = ORIENTED_EDGE('',*,*,#16882,.T.) ;
#22514 = ORIENTED_EDGE('',*,*,#16666,.T.) ;
#22515 = ORIENTED_EDGE('',*,*,#16883,.F.) ;
#22516 = ORIENTED_EDGE('',*,*,#16545,.T.) ;
#22517 = ORIENTED_EDGE('',*,*,#16883,.T.) ;
#22518 = ORIENTED_EDGE('',*,*,#16665,.T.) ;
#22519 = ORIENTED_EDGE('',*,*,#16880,.T.) ;
#22520 = ORIENTED_EDGE('',*,*,#16546,.T.) ;
#22521 = ORIENTED_EDGE('',*,*,#16884,.F.) ;
#22522 = ORIENTED_EDGE('',*,*,#16664,.T.) ;
#22523 = ORIENTED_EDGE('',*,*,#16885,.F.) ;
#22524 = ORIENTED_EDGE('',*,*,#16551,.T.) ;
#22525 = ORIENTED_EDGE('',*,*,#16885,.T.) ;
#22526 = ORIENTED_EDGE('',*,*,#16663,.T.) ;
#22527 = ORIENTED_EDGE('',*,*,#16886,.F.) ;
#22528 = ORIENTED_EDGE('',*,*,#16548,.T.) ;
#22529 = ORIENTED_EDGE('',*,*,#16886,.T.) ;
#22530 = ORIENTED_EDGE('',*,*,#16662,.T.) ;
#22531 = ORIENTED_EDGE('',*,*,#16887,.F.) ;
#22532 = ORIENTED_EDGE('',*,*,#16549,.T.) ;
#22533 = ORIENTED_EDGE('',*,*,#16887,.T.) ;
#22534 = ORIENTED_EDGE('',*,*,#16661,.T.) ;
#22535 = ORIENTED_EDGE('',*,*,#16884,.T.) ;
#22536 = ORIENTED_EDGE('',*,*,#16550,.T.) ;
#22537 = ORIENTED_EDGE('',*,*,#16569,.F.) ;
#22538 = ORIENTED_EDGE('',*,*,#16888,.T.) ;
#22539 = ORIENTED_EDGE('',*,*,#16655,.T.) ;
#22540 = ORIENTED_EDGE('',*,*,#16867,.T.) ;
#22541 = ORIENTED_EDGE('',*,*,#16889,.T.) ;
#22542 = ORIENTED_EDGE('',*,*,#16658,.T.) ;
#22543 = ORIENTED_EDGE('',*,*,#16890,.F.) ;
#22544 = ORIENTED_EDGE('',*,*,#16537,.T.) ;
#22545 = ORIENTED_EDGE('',*,*,#16890,.T.) ;
#22546 = ORIENTED_EDGE('',*,*,#16657,.T.) ;
#22547 = ORIENTED_EDGE('',*,*,#16891,.T.) ;
#22548 = ORIENTED_EDGE('',*,*,#16538,.T.) ;
#22549 = ORIENTED_EDGE('',*,*,#16891,.F.) ;
#22550 = ORIENTED_EDGE('',*,*,#16660,.T.) ;
#22551 = ORIENTED_EDGE('',*,*,#16892,.F.) ;
#22552 = ORIENTED_EDGE('',*,*,#16539,.T.) ;
#22553 = ORIENTED_EDGE('',*,*,#16892,.T.) ;
#22554 = ORIENTED_EDGE('',*,*,#16659,.T.) ;
#22555 = ORIENTED_EDGE('',*,*,#16889,.F.) ;
#22556 = ORIENTED_EDGE('',*,*,#16536,.T.) ;
#22557 = ORIENTED_EDGE('',*,*,#16893,.F.) ;
#22558 = ORIENTED_EDGE('',*,*,#16861,.F.) ;
#22559 = ORIENTED_EDGE('',*,*,#16894,.F.) ;
#22560 = ORIENTED_EDGE('',*,*,#16895,.T.) ;
#22561 = ORIENTED_EDGE('',*,*,#16627,.F.) ;
#22562 = ORIENTED_EDGE('',*,*,#16869,.F.) ;
#22563 = ORIENTED_EDGE('',*,*,#16524,.F.) ;
#22564 = ORIENTED_EDGE('',*,*,#16804,.F.) ;
#22565 = ORIENTED_EDGE('',*,*,#16896,.T.) ;
#22566 = ORIENTED_EDGE('',*,*,#16848,.F.) ;
#22567 = ORIENTED_EDGE('',*,*,#16897,.F.) ;
#22568 = ORIENTED_EDGE('',*,*,#16898,.T.) ;
#22569 = ORIENTED_EDGE('',*,*,#16619,.F.) ;
#22570 = ORIENTED_EDGE('',*,*,#16874,.F.) ;
#22571 = ORIENTED_EDGE('',*,*,#16532,.F.) ;
#22572 = ORIENTED_EDGE('',*,*,#16812,.F.) ;
#22573 = ORIENTED_EDGE('',*,*,#16899,.F.) ;
#22574 = ORIENTED_EDGE('',*,*,#16620,.F.) ;
#22575 = ORIENTED_EDGE('',*,*,#16898,.F.) ;
#22576 = ORIENTED_EDGE('',*,*,#16900,.T.) ;
#22577 = ORIENTED_EDGE('',*,*,#16895,.F.) ;
#22578 = ORIENTED_EDGE('',*,*,#16901,.F.) ;
#22579 = ORIENTED_EDGE('',*,*,#16902,.F.) ;
#22580 = ORIENTED_EDGE('',*,*,#16628,.T.) ;
#22581 = ORIENTED_EDGE('',*,*,#16903,.F.) ;
#22582 = ORIENTED_EDGE('',*,*,#16844,.F.) ;
#22583 = ORIENTED_EDGE('',*,*,#16904,.F.) ;
#22584 = ORIENTED_EDGE('',*,*,#16905,.T.) ;
#22585 = ORIENTED_EDGE('',*,*,#16623,.T.) ;
#22586 = ORIENTED_EDGE('',*,*,#16872,.F.) ;
#22587 = ORIENTED_EDGE('',*,*,#16528,.F.) ;
#22588 = ORIENTED_EDGE('',*,*,#16817,.F.) ;
#22589 = ORIENTED_EDGE('',*,*,#16905,.F.) ;
#22590 = ORIENTED_EDGE('',*,*,#16906,.F.) ;
#22591 = ORIENTED_EDGE('',*,*,#16907,.F.) ;
#22592 = ORIENTED_EDGE('',*,*,#16624,.T.) ;
#22593 = ORIENTED_EDGE('',*,*,#16865,.F.) ;
#22594 = ORIENTED_EDGE('',*,*,#16652,.T.) ;
#22595 = ORIENTED_EDGE('',*,*,#16908,.F.) ;
#22596 = ORIENTED_EDGE('',*,*,#16909,.T.) ;
#22597 = ORIENTED_EDGE('',*,*,#16908,.T.) ;
#22598 = ORIENTED_EDGE('',*,*,#16651,.F.) ;
#22599 = ORIENTED_EDGE('',*,*,#16910,.T.) ;
#22600 = ORIENTED_EDGE('',*,*,#16911,.F.) ;
#22601 = ORIENTED_EDGE('',*,*,#16832,.T.) ;
#22602 = ORIENTED_EDGE('',*,*,#16912,.T.) ;
#22603 = ORIENTED_EDGE('',*,*,#16910,.F.) ;
#22604 = ORIENTED_EDGE('',*,*,#16656,.T.) ;
#22605 = ORIENTED_EDGE('',*,*,#16888,.F.) ;
#22606 = ORIENTED_EDGE('',*,*,#16568,.T.) ;
#22607 = ORIENTED_EDGE('',*,*,#16913,.T.) ;
#22608 = ORIENTED_EDGE('',*,*,#16813,.F.) ;
#22609 = ORIENTED_EDGE('',*,*,#16530,.F.) ;
#22610 = ORIENTED_EDGE('',*,*,#16871,.F.) ;
#22611 = ORIENTED_EDGE('',*,*,#16621,.F.) ;
#22612 = ORIENTED_EDGE('',*,*,#16899,.T.) ;
#22613 = ORIENTED_EDGE('',*,*,#16914,.F.) ;
#22614 = ORIENTED_EDGE('',*,*,#16842,.F.) ;
#22615 = ORIENTED_EDGE('',*,*,#16915,.T.) ;
#22616 = ORIENTED_EDGE('',*,*,#16430,.F.) ;
#22617 = ORIENTED_EDGE('',*,*,#16534,.F.) ;
#22618 = ORIENTED_EDGE('',*,*,#16873,.F.) ;
#22619 = ORIENTED_EDGE('',*,*,#16617,.F.) ;
#22620 = ORIENTED_EDGE('',*,*,#16690,.T.) ;
#22621 = ORIENTED_EDGE('',*,*,#16916,.F.) ;
#22622 = ORIENTED_EDGE('',*,*,#16846,.F.) ;
#22623 = ORIENTED_EDGE('',*,*,#16526,.F.) ;
#22624 = ORIENTED_EDGE('',*,*,#16870,.F.) ;
#22625 = ORIENTED_EDGE('',*,*,#16625,.F.) ;
#22626 = ORIENTED_EDGE('',*,*,#16907,.T.) ;
#22627 = ORIENTED_EDGE('',*,*,#16917,.F.) ;
#22628 = ORIENTED_EDGE('',*,*,#16863,.F.) ;
#22629 = ORIENTED_EDGE('',*,*,#16918,.F.) ;
#22630 = ORIENTED_EDGE('',*,*,#16815,.F.) ;
#22631 = ORIENTED_EDGE('',*,*,#16522,.F.) ;
#22632 = ORIENTED_EDGE('',*,*,#16875,.F.) ;
#22633 = ORIENTED_EDGE('',*,*,#16629,.F.) ;
#22634 = ORIENTED_EDGE('',*,*,#16902,.T.) ;
#22635 = ORIENTED_EDGE('',*,*,#16919,.F.) ;
#22636 = ORIENTED_EDGE('',*,*,#16859,.F.) ;
#22637 = ORIENTED_EDGE('',*,*,#16920,.F.) ;
#22638 = ORIENTED_EDGE('',*,*,#16805,.F.) ;
#22639 = ORIENTED_EDGE('',*,*,#16921,.F.) ;
#22640 = ORIENTED_EDGE('',*,*,#16922,.T.) ;
#22641 = ORIENTED_EDGE('',*,*,#16923,.F.) ;
#22642 = ORIENTED_EDGE('',*,*,#16924,.T.) ;
#22643 = ORIENTED_EDGE('',*,*,#16925,.F.) ;
#22644 = ORIENTED_EDGE('',*,*,#16926,.T.) ;
#22645 = ORIENTED_EDGE('',*,*,#16927,.F.) ;
#22646 = ORIENTED_EDGE('',*,*,#16928,.T.) ;
#22647 = ORIENTED_EDGE('',*,*,#16929,.F.) ;
#22648 = ORIENTED_EDGE('',*,*,#16930,.T.) ;
#22649 = ORIENTED_EDGE('',*,*,#16931,.F.) ;
#22650 = ORIENTED_EDGE('',*,*,#16932,.T.) ;
#22651 = ORIENTED_EDGE('',*,*,#16933,.F.) ;
#22652 = ORIENTED_EDGE('',*,*,#16934,.F.) ;
#22653 = ORIENTED_EDGE('',*,*,#16935,.F.) ;
#22654 = ORIENTED_EDGE('',*,*,#16936,.F.) ;
#22655 = ORIENTED_EDGE('',*,*,#16937,.F.) ;
#22656 = ORIENTED_EDGE('',*,*,#16938,.F.) ;
#22657 = ORIENTED_EDGE('',*,*,#16939,.F.) ;
#22658 = ORIENTED_EDGE('',*,*,#16924,.F.) ;
#22659 = ORIENTED_EDGE('',*,*,#16940,.F.) ;
#22660 = ORIENTED_EDGE('',*,*,#16941,.T.) ;
#22661 = ORIENTED_EDGE('',*,*,#16942,.F.) ;
#22662 = ORIENTED_EDGE('',*,*,#16943,.F.) ;
#22663 = ORIENTED_EDGE('',*,*,#16941,.F.) ;
#22664 = ORIENTED_EDGE('',*,*,#16942,.T.) ;
#22665 = ORIENTED_EDGE('',*,*,#16943,.T.) ;
#22666 = ORIENTED_EDGE('',*,*,#16944,.T.) ;
#22667 = ORIENTED_EDGE('',*,*,#16936,.T.) ;
#22668 = ORIENTED_EDGE('',*,*,#16944,.F.) ;
#22669 = ORIENTED_EDGE('',*,*,#16945,.F.) ;
#22670 = ORIENTED_EDGE('',*,*,#16946,.T.) ;
#22671 = ORIENTED_EDGE('',*,*,#16947,.F.) ;
#22672 = ORIENTED_EDGE('',*,*,#16948,.F.) ;
#22673 = ORIENTED_EDGE('',*,*,#16946,.F.) ;
#22674 = ORIENTED_EDGE('',*,*,#16947,.T.) ;
#22675 = ORIENTED_EDGE('',*,*,#16948,.T.) ;
#22676 = ORIENTED_EDGE('',*,*,#16949,.T.) ;
#22677 = ORIENTED_EDGE('',*,*,#16935,.T.) ;
#22678 = ORIENTED_EDGE('',*,*,#16949,.F.) ;
#22679 = ORIENTED_EDGE('',*,*,#16950,.F.) ;
#22680 = ORIENTED_EDGE('',*,*,#16951,.T.) ;
#22681 = ORIENTED_EDGE('',*,*,#16952,.F.) ;
#22682 = ORIENTED_EDGE('',*,*,#16953,.F.) ;
#22683 = ORIENTED_EDGE('',*,*,#16951,.F.) ;
#22684 = ORIENTED_EDGE('',*,*,#16952,.T.) ;
#22685 = ORIENTED_EDGE('',*,*,#16953,.T.) ;
#22686 = ORIENTED_EDGE('',*,*,#16954,.T.) ;
#22687 = ORIENTED_EDGE('',*,*,#16934,.T.) ;
#22688 = ORIENTED_EDGE('',*,*,#16954,.F.) ;
#22689 = ORIENTED_EDGE('',*,*,#16955,.F.) ;
#22690 = ORIENTED_EDGE('',*,*,#16956,.T.) ;
#22691 = ORIENTED_EDGE('',*,*,#16957,.F.) ;
#22692 = ORIENTED_EDGE('',*,*,#16958,.F.) ;
#22693 = ORIENTED_EDGE('',*,*,#16956,.F.) ;
#22694 = ORIENTED_EDGE('',*,*,#16957,.T.) ;
#22695 = ORIENTED_EDGE('',*,*,#16958,.T.) ;
#22696 = ORIENTED_EDGE('',*,*,#16959,.T.) ;
#22697 = ORIENTED_EDGE('',*,*,#16933,.T.) ;
#22698 = ORIENTED_EDGE('',*,*,#16959,.F.) ;
#22699 = ORIENTED_EDGE('',*,*,#16960,.T.) ;
#22700 = ORIENTED_EDGE('',*,*,#16961,.F.) ;
#22701 = ORIENTED_EDGE('',*,*,#16932,.F.) ;
#22702 = ORIENTED_EDGE('',*,*,#16962,.F.) ;
#22703 = ORIENTED_EDGE('',*,*,#16723,.T.) ;
#22704 = ORIENTED_EDGE('',*,*,#16922,.F.) ;
#22705 = ORIENTED_EDGE('',*,*,#16963,.F.) ;
#22706 = ORIENTED_EDGE('',*,*,#16478,.F.) ;
#22707 = ORIENTED_EDGE('',*,*,#16720,.F.) ;
#22708 = ORIENTED_EDGE('',*,*,#16926,.F.) ;
#22709 = ORIENTED_EDGE('',*,*,#16744,.F.) ;
#22710 = ORIENTED_EDGE('',*,*,#16725,.F.) ;
#22711 = ORIENTED_EDGE('',*,*,#16482,.F.) ;
#22712 = ORIENTED_EDGE('',*,*,#16964,.T.) ;
#22713 = ORIENTED_EDGE('',*,*,#16808,.F.) ;
#22714 = ORIENTED_EDGE('',*,*,#16469,.F.) ;
#22715 = ORIENTED_EDGE('',*,*,#16965,.F.) ;
#22716 = ORIENTED_EDGE('',*,*,#16585,.F.) ;
#22717 = ORIENTED_EDGE('',*,*,#16966,.T.) ;
#22718 = ORIENTED_EDGE('',*,*,#16967,.F.) ;
#22719 = ORIENTED_EDGE('',*,*,#16852,.F.) ;
#22720 = ORIENTED_EDGE('',*,*,#16968,.F.) ;
#22721 = ORIENTED_EDGE('',*,*,#16969,.F.) ;
#22722 = ORIENTED_EDGE('',*,*,#16850,.F.) ;
#22723 = ORIENTED_EDGE('',*,*,#16970,.F.) ;
#22724 = ORIENTED_EDGE('',*,*,#16691,.T.) ;
#22725 = ORIENTED_EDGE('',*,*,#16587,.F.) ;
#22726 = ORIENTED_EDGE('',*,*,#16971,.F.) ;
#22727 = ORIENTED_EDGE('',*,*,#16467,.F.) ;
#22728 = ORIENTED_EDGE('',*,*,#16811,.F.) ;
#22729 = ORIENTED_EDGE('',*,*,#16972,.T.) ;
#22730 = ORIENTED_EDGE('',*,*,#16593,.T.) ;
#22731 = ORIENTED_EDGE('',*,*,#16973,.F.) ;
#22732 = ORIENTED_EDGE('',*,*,#16507,.T.) ;
#22733 = ORIENTED_EDGE('',*,*,#16974,.F.) ;
#22734 = ORIENTED_EDGE('',*,*,#16594,.T.) ;
#22735 = ORIENTED_EDGE('',*,*,#16972,.F.) ;
#22736 = ORIENTED_EDGE('',*,*,#16510,.T.) ;
#22737 = ORIENTED_EDGE('',*,*,#16975,.T.) ;
#22738 = ORIENTED_EDGE('',*,*,#16591,.T.) ;
#22739 = ORIENTED_EDGE('',*,*,#16974,.T.) ;
#22740 = ORIENTED_EDGE('',*,*,#16509,.T.) ;
#22741 = ORIENTED_EDGE('',*,*,#16973,.T.) ;
#22742 = ORIENTED_EDGE('',*,*,#16592,.T.) ;
#22743 = ORIENTED_EDGE('',*,*,#16975,.F.) ;
#22744 = ORIENTED_EDGE('',*,*,#16508,.T.) ;
#22745 = ORIENTED_EDGE('',*,*,#16489,.T.) ;
#22746 = ORIENTED_EDGE('',*,*,#16976,.T.) ;
#22747 = ORIENTED_EDGE('',*,*,#16977,.F.) ;
#22748 = ORIENTED_EDGE('',*,*,#16978,.F.) ;
#22749 = ORIENTED_EDGE('',*,*,#16472,.F.) ;
#22750 = ORIENTED_EDGE('',*,*,#16979,.T.) ;
#22751 = ORIENTED_EDGE('',*,*,#16582,.F.) ;
#22752 = ORIENTED_EDGE('',*,*,#16980,.T.) ;
#22753 = ORIENTED_EDGE('',*,*,#16468,.F.) ;
#22754 = ORIENTED_EDGE('',*,*,#16971,.T.) ;
#22755 = ORIENTED_EDGE('',*,*,#16586,.F.) ;
#22756 = ORIENTED_EDGE('',*,*,#16965,.T.) ;
#22757 = ORIENTED_EDGE('',*,*,#16437,.F.) ;
#22758 = ORIENTED_EDGE('',*,*,#16465,.T.) ;
#22759 = ORIENTED_EDGE('',*,*,#16435,.F.) ;
#22760 = ORIENTED_EDGE('',*,*,#16589,.T.) ;
#22761 = ORIENTED_EDGE('',*,*,#16480,.F.) ;
#22762 = ORIENTED_EDGE('',*,*,#16981,.T.) ;
#22763 = ORIENTED_EDGE('',*,*,#16607,.T.) ;
#22764 = ORIENTED_EDGE('',*,*,#16982,.T.) ;
#22765 = ORIENTED_EDGE('',*,*,#16983,.T.) ;
#22766 = ORIENTED_EDGE('',*,*,#16595,.T.) ;
#22767 = ORIENTED_EDGE('',*,*,#16984,.T.) ;
#22768 = ORIENTED_EDGE('',*,*,#16501,.T.) ;
#22769 = ORIENTED_EDGE('',*,*,#16985,.T.) ;
#22770 = ORIENTED_EDGE('',*,*,#16596,.T.) ;
#22771 = ORIENTED_EDGE('',*,*,#16983,.F.) ;
#22772 = ORIENTED_EDGE('',*,*,#16500,.T.) ;
#22773 = ORIENTED_EDGE('',*,*,#16986,.T.) ;
#22774 = ORIENTED_EDGE('',*,*,#16597,.T.) ;
#22775 = ORIENTED_EDGE('',*,*,#16985,.F.) ;
#22776 = ORIENTED_EDGE('',*,*,#16499,.T.) ;
#22777 = ORIENTED_EDGE('',*,*,#16984,.F.) ;
#22778 = ORIENTED_EDGE('',*,*,#16598,.T.) ;
#22779 = ORIENTED_EDGE('',*,*,#16986,.F.) ;
#22780 = ORIENTED_EDGE('',*,*,#16502,.T.) ;
#22781 = ORIENTED_EDGE('',*,*,#16987,.T.) ;
#22782 = ORIENTED_EDGE('',*,*,#16599,.T.) ;
#22783 = ORIENTED_EDGE('',*,*,#16988,.T.) ;
#22784 = ORIENTED_EDGE('',*,*,#16505,.T.) ;
#22785 = ORIENTED_EDGE('',*,*,#16989,.T.) ;
#22786 = ORIENTED_EDGE('',*,*,#16600,.T.) ;
#22787 = ORIENTED_EDGE('',*,*,#16987,.F.) ;
#22788 = ORIENTED_EDGE('',*,*,#16504,.T.) ;
#22789 = ORIENTED_EDGE('',*,*,#16990,.T.) ;
#22790 = ORIENTED_EDGE('',*,*,#16601,.T.) ;
#22791 = ORIENTED_EDGE('',*,*,#16989,.F.) ;
#22792 = ORIENTED_EDGE('',*,*,#16503,.T.) ;
#22793 = ORIENTED_EDGE('',*,*,#16988,.F.) ;
#22794 = ORIENTED_EDGE('',*,*,#16602,.T.) ;
#22795 = ORIENTED_EDGE('',*,*,#16990,.F.) ;
#22796 = ORIENTED_EDGE('',*,*,#16506,.T.) ;
#22797 = ORIENTED_EDGE('',*,*,#16991,.T.) ;
#22798 = ORIENTED_EDGE('',*,*,#16603,.F.) ;
#22799 = ORIENTED_EDGE('',*,*,#16992,.T.) ;
#22800 = ORIENTED_EDGE('',*,*,#16930,.F.) ;
#22801 = ORIENTED_EDGE('',*,*,#16993,.F.) ;
#22802 = ORIENTED_EDGE('',*,*,#16604,.T.) ;
#22803 = ORIENTED_EDGE('',*,*,#16991,.F.) ;
#22804 = ORIENTED_EDGE('',*,*,#16929,.T.) ;
#22805 = ORIENTED_EDGE('',*,*,#16994,.T.) ;
#22806 = ORIENTED_EDGE('',*,*,#16605,.F.) ;
#22807 = ORIENTED_EDGE('',*,*,#16993,.T.) ;
#22808 = ORIENTED_EDGE('',*,*,#16928,.F.) ;
#22809 = ORIENTED_EDGE('',*,*,#16995,.T.) ;
#22810 = ORIENTED_EDGE('',*,*,#16996,.F.) ;
#22811 = ORIENTED_EDGE('',*,*,#16580,.F.) ;
#22812 = ORIENTED_EDGE('',*,*,#16711,.F.) ;
#22813 = ORIENTED_EDGE('',*,*,#16693,.F.) ;
#22814 = ORIENTED_EDGE('',*,*,#16473,.F.) ;
#22815 = ORIENTED_EDGE('',*,*,#16980,.F.) ;
#22816 = ORIENTED_EDGE('',*,*,#16581,.F.) ;
#22817 = ORIENTED_EDGE('',*,*,#16996,.T.) ;
#22818 = ORIENTED_EDGE('',*,*,#16997,.F.) ;
#22819 = ORIENTED_EDGE('',*,*,#16856,.F.) ;
#22820 = ORIENTED_EDGE('',*,*,#16998,.F.) ;
#22821 = ORIENTED_EDGE('',*,*,#16999,.F.) ;
#22822 = ORIENTED_EDGE('',*,*,#17000,.F.) ;
#22823 = ORIENTED_EDGE('',*,*,#16966,.F.) ;
#22824 = ORIENTED_EDGE('',*,*,#16584,.T.) ;
#22825 = ORIENTED_EDGE('',*,*,#17001,.F.) ;
#22826 = ORIENTED_EDGE('',*,*,#16854,.F.) ;
#22827 = ORIENTED_EDGE('',*,*,#17002,.F.) ;
#22828 = ORIENTED_EDGE('',*,*,#16999,.T.) ;
#22829 = ORIENTED_EDGE('',*,*,#16583,.T.) ;
#22830 = ORIENTED_EDGE('',*,*,#16979,.F.) ;
#22831 = ORIENTED_EDGE('',*,*,#16471,.F.) ;
#22832 = ORIENTED_EDGE('',*,*,#16807,.F.) ;
#22833 = ORIENTED_EDGE('',*,*,#16963,.T.) ;
#22834 = ORIENTED_EDGE('',*,*,#16921,.T.) ;
#22835 = ORIENTED_EDGE('',*,*,#17003,.F.) ;
#22836 = ORIENTED_EDGE('',*,*,#16977,.T.) ;
#22837 = ORIENTED_EDGE('',*,*,#17004,.F.) ;
#22838 = ORIENTED_EDGE('',*,*,#16931,.T.) ;
#22839 = ORIENTED_EDGE('',*,*,#16992,.F.) ;
#22840 = ORIENTED_EDGE('',*,*,#16608,.T.) ;
#22841 = ORIENTED_EDGE('',*,*,#16981,.F.) ;
#22842 = ORIENTED_EDGE('',*,*,#16479,.T.) ;
#22843 = ORIENTED_EDGE('',*,*,#16481,.T.) ;
#22844 = ORIENTED_EDGE('',*,*,#16982,.F.) ;
#22845 = ORIENTED_EDGE('',*,*,#16606,.T.) ;
#22846 = ORIENTED_EDGE('',*,*,#16994,.F.) ;
#22847 = ORIENTED_EDGE('',*,*,#16927,.T.) ;
#22848 = ORIENTED_EDGE('',*,*,#16964,.F.) ;
#22849 = ORIENTED_EDGE('',*,*,#17005,.T.) ;
#22850 = ORIENTED_EDGE('',*,*,#17006,.T.) ;
#22851 = ORIENTED_EDGE('',*,*,#16833,.F.) ;
#22852 = ORIENTED_EDGE('',*,*,#16868,.F.) ;
#22853 = ORIENTED_EDGE('',*,*,#16866,.T.) ;
#22854 = ORIENTED_EDGE('',*,*,#16909,.F.) ;
#22855 = ORIENTED_EDGE('',*,*,#16911,.T.) ;
#22856 = ORIENTED_EDGE('',*,*,#16912,.F.) ;
#22857 = ORIENTED_EDGE('',*,*,#16831,.F.) ;
#22858 = ORIENTED_EDGE('',*,*,#17007,.F.) ;
#22859 = ORIENTED_EDGE('',*,*,#16840,.F.) ;
#22860 = ORIENTED_EDGE('',*,*,#17008,.F.) ;
#22861 = ORIENTED_EDGE('',*,*,#17009,.T.) ;
#22862 = ORIENTED_EDGE('',*,*,#16535,.T.) ;
#22863 = ORIENTED_EDGE('',*,*,#17009,.F.) ;
#22864 = ORIENTED_EDGE('',*,*,#17010,.F.) ;
#22865 = ORIENTED_EDGE('',*,*,#17008,.T.) ;
#22866 = ORIENTED_EDGE('',*,*,#17011,.T.) ;
#22867 = ORIENTED_EDGE('',*,*,#16674,.T.) ;
#22868 = ORIENTED_EDGE('',*,*,#17011,.F.) ;
#22869 = ORIENTED_EDGE('',*,*,#17010,.T.) ;
#22870 = ORIENTED_EDGE('',*,*,#16555,.F.) ;
#22871 = ORIENTED_EDGE('',*,*,#16372,.F.) ;
#22872 = ORIENTED_EDGE('',*,*,#16396,.F.) ;
#22873 = ORIENTED_EDGE('',*,*,#16380,.F.) ;
#22874 = ORIENTED_EDGE('',*,*,#16379,.F.) ;
#22875 = ORIENTED_EDGE('',*,*,#16647,.F.) ;
#22876 = ORIENTED_EDGE('',*,*,#16646,.F.) ;
#22877 = ORIENTED_EDGE('',*,*,#16365,.T.) ;
#22878 = ORIENTED_EDGE('',*,*,#16364,.T.) ;
#22879 = ORIENTED_EDGE('',*,*,#16399,.T.) ;
#22880 = ORIENTED_EDGE('',*,*,#16362,.T.) ;
#22881 = ORIENTED_EDGE('',*,*,#16358,.T.) ;
#22882 = ORIENTED_EDGE('',*,*,#16553,.F.) ;
#22883 = ORIENTED_EDGE('',*,*,#16356,.F.) ;
#22884 = ORIENTED_EDGE('',*,*,#16361,.F.) ;
#22885 = ORIENTED_EDGE('',*,*,#16360,.F.) ;
#22886 = ORIENTED_EDGE('',*,*,#16398,.F.) ;
#22887 = ORIENTED_EDGE('',*,*,#16367,.F.) ;
#22888 = ORIENTED_EDGE('',*,*,#16645,.F.) ;
#22889 = ORIENTED_EDGE('',*,*,#16377,.F.) ;
#22890 = ORIENTED_EDGE('',*,*,#16376,.F.) ;
#22891 = ORIENTED_EDGE('',*,*,#16397,.F.) ;
#22892 = ORIENTED_EDGE('',*,*,#16374,.F.) ;
#22893 = ORIENTED_EDGE('',*,*,#16370,.F.) ;
#22894 = ORIENTED_EDGE('',*,*,#16554,.F.) ;
#22895 = ORIENTED_EDGE('',*,*,#16558,.F.) ;
#22896 = ORIENTED_EDGE('',*,*,#16385,.F.) ;
#22897 = ORIENTED_EDGE('',*,*,#16394,.F.) ;
#22898 = ORIENTED_EDGE('',*,*,#16393,.F.) ;
#22899 = ORIENTED_EDGE('',*,*,#16392,.F.) ;
#22900 = ORIENTED_EDGE('',*,*,#16650,.F.) ;
#22901 = ORIENTED_EDGE('',*,*,#16649,.F.) ;
#22902 = ORIENTED_EDGE('',*,*,#16352,.T.) ;
#22903 = ORIENTED_EDGE('',*,*,#16351,.T.) ;
#22904 = ORIENTED_EDGE('',*,*,#16401,.T.) ;
#22905 = ORIENTED_EDGE('',*,*,#16349,.T.) ;
#22906 = ORIENTED_EDGE('',*,*,#16345,.T.) ;
#22907 = ORIENTED_EDGE('',*,*,#16556,.F.) ;
#22908 = ORIENTED_EDGE('',*,*,#16343,.F.) ;
#22909 = ORIENTED_EDGE('',*,*,#16348,.F.) ;
#22910 = ORIENTED_EDGE('',*,*,#16347,.F.) ;
#22911 = ORIENTED_EDGE('',*,*,#16400,.F.) ;
#22912 = ORIENTED_EDGE('',*,*,#16354,.F.) ;
#22913 = ORIENTED_EDGE('',*,*,#16648,.F.) ;
#22914 = ORIENTED_EDGE('',*,*,#16390,.F.) ;
#22915 = ORIENTED_EDGE('',*,*,#16389,.F.) ;
#22916 = ORIENTED_EDGE('',*,*,#16395,.F.) ;
#22917 = ORIENTED_EDGE('',*,*,#16387,.F.) ;
#22918 = ORIENTED_EDGE('',*,*,#16383,.F.) ;
#22919 = ORIENTED_EDGE('',*,*,#16557,.F.) ;
#22920 = ORIENTED_EDGE('',*,*,#16497,.F.) ;
#22921 = ORIENTED_EDGE('',*,*,#16320,.F.) ;
#22922 = ORIENTED_EDGE('',*,*,#16404,.F.) ;
#22923 = ORIENTED_EDGE('',*,*,#16328,.F.) ;
#22924 = ORIENTED_EDGE('',*,*,#16327,.F.) ;
#22925 = ORIENTED_EDGE('',*,*,#16615,.F.) ;
#22926 = ORIENTED_EDGE('',*,*,#16614,.F.) ;
#22927 = ORIENTED_EDGE('',*,*,#16312,.T.) ;
#22928 = ORIENTED_EDGE('',*,*,#16311,.T.) ;
#22929 = ORIENTED_EDGE('',*,*,#16408,.T.) ;
#22930 = ORIENTED_EDGE('',*,*,#16309,.T.) ;
#22931 = ORIENTED_EDGE('',*,*,#16305,.T.) ;
#22932 = ORIENTED_EDGE('',*,*,#16495,.F.) ;
#22933 = ORIENTED_EDGE('',*,*,#16303,.F.) ;
#22934 = ORIENTED_EDGE('',*,*,#16308,.F.) ;
#22935 = ORIENTED_EDGE('',*,*,#16307,.F.) ;
#22936 = ORIENTED_EDGE('',*,*,#16407,.F.) ;
#22937 = ORIENTED_EDGE('',*,*,#16406,.F.) ;
#22938 = ORIENTED_EDGE('',*,*,#16315,.F.) ;
#22939 = ORIENTED_EDGE('',*,*,#16314,.F.) ;
#22940 = ORIENTED_EDGE('',*,*,#16613,.F.) ;
#22941 = ORIENTED_EDGE('',*,*,#16325,.F.) ;
#22942 = ORIENTED_EDGE('',*,*,#16324,.F.) ;
#22943 = ORIENTED_EDGE('',*,*,#16405,.F.) ;
#22944 = ORIENTED_EDGE('',*,*,#16322,.F.) ;
#22945 = ORIENTED_EDGE('',*,*,#16318,.F.) ;
#22946 = ORIENTED_EDGE('',*,*,#16496,.F.) ;
#22947 = ORIENTED_EDGE('',*,*,#16494,.F.) ;
#22948 = ORIENTED_EDGE('',*,*,#16333,.F.) ;
#22949 = ORIENTED_EDGE('',*,*,#16402,.F.) ;
#22950 = ORIENTED_EDGE('',*,*,#16341,.F.) ;
#22951 = ORIENTED_EDGE('',*,*,#16340,.F.) ;
#22952 = ORIENTED_EDGE('',*,*,#16612,.F.) ;
#22953 = ORIENTED_EDGE('',*,*,#16611,.F.) ;
#22954 = ORIENTED_EDGE('',*,*,#16299,.T.) ;
#22955 = ORIENTED_EDGE('',*,*,#16298,.T.) ;
#22956 = ORIENTED_EDGE('',*,*,#16410,.T.) ;
#22957 = ORIENTED_EDGE('',*,*,#16296,.T.) ;
#22958 = ORIENTED_EDGE('',*,*,#16292,.T.) ;
#22959 = ORIENTED_EDGE('',*,*,#16492,.F.) ;
#22960 = ORIENTED_EDGE('',*,*,#16290,.F.) ;
#22961 = ORIENTED_EDGE('',*,*,#16295,.F.) ;
#22962 = ORIENTED_EDGE('',*,*,#16294,.F.) ;
#22963 = ORIENTED_EDGE('',*,*,#16409,.F.) ;
#22964 = ORIENTED_EDGE('',*,*,#16301,.F.) ;
#22965 = ORIENTED_EDGE('',*,*,#16610,.F.) ;
#22966 = ORIENTED_EDGE('',*,*,#16338,.F.) ;
#22967 = ORIENTED_EDGE('',*,*,#16337,.F.) ;
#22968 = ORIENTED_EDGE('',*,*,#16403,.F.) ;
#22969 = ORIENTED_EDGE('',*,*,#16335,.F.) ;
#22970 = ORIENTED_EDGE('',*,*,#16331,.F.) ;
#22971 = ORIENTED_EDGE('',*,*,#16493,.F.) ;
#22972 = ORIENTED_EDGE('',*,*,#17012,.F.) ;
#22973 = ORIENTED_EDGE('',*,*,#16565,.F.) ;
#22974 = ORIENTED_EDGE('',*,*,#17013,.F.) ;
#22975 = ORIENTED_EDGE('',*,*,#17014,.F.) ;
#22976 = ORIENTED_EDGE('',*,*,#17015,.F.) ;
#22977 = ORIENTED_EDGE('',*,*,#16563,.F.) ;
#22978 = ORIENTED_EDGE('',*,*,#17016,.F.) ;
#22979 = ORIENTED_EDGE('',*,*,#17017,.F.) ;
#22980 = ORIENTED_EDGE('',*,*,#17018,.F.) ;
#22981 = ORIENTED_EDGE('',*,*,#17019,.F.) ;
#22982 = ORIENTED_EDGE('',*,*,#17020,.F.) ;
#22983 = ORIENTED_EDGE('',*,*,#16561,.F.) ;
#22984 = ORIENTED_EDGE('',*,*,#17021,.F.) ;
#22985 = ORIENTED_EDGE('',*,*,#17022,.F.) ;
#22986 = ORIENTED_EDGE('',*,*,#17023,.F.) ;
#22987 = ORIENTED_EDGE('',*,*,#16559,.F.) ;
#22988 = ORIENTED_EDGE('',*,*,#16562,.T.) ;
#22989 = ORIENTED_EDGE('',*,*,#17020,.T.) ;
#22990 = ORIENTED_EDGE('',*,*,#17024,.T.) ;
#22991 = ORIENTED_EDGE('',*,*,#17016,.T.) ;
#22992 = ORIENTED_EDGE('',*,*,#16560,.T.) ;
#22993 = ORIENTED_EDGE('',*,*,#17023,.T.) ;
#22994 = ORIENTED_EDGE('',*,*,#17025,.T.) ;
#22995 = ORIENTED_EDGE('',*,*,#17018,.T.) ;
#22996 = ORIENTED_EDGE('',*,*,#17026,.T.) ;
#22997 = ORIENTED_EDGE('',*,*,#16642,.T.) ;
#22998 = ORIENTED_EDGE('',*,*,#17027,.T.) ;
#22999 = ORIENTED_EDGE('',*,*,#17019,.T.) ;
#23000 = ORIENTED_EDGE('',*,*,#16564,.T.) ;
#23001 = ORIENTED_EDGE('',*,*,#17015,.T.) ;
#23002 = ORIENTED_EDGE('',*,*,#17028,.T.) ;
#23003 = ORIENTED_EDGE('',*,*,#17013,.T.) ;
#23004 = ORIENTED_EDGE('',*,*,#17029,.T.) ;
#23005 = ORIENTED_EDGE('',*,*,#16638,.T.) ;
#23006 = ORIENTED_EDGE('',*,*,#17030,.T.) ;
#23007 = ORIENTED_EDGE('',*,*,#17014,.T.) ;
#23008 = ORIENTED_EDGE('',*,*,#16566,.T.) ;
#23009 = ORIENTED_EDGE('',*,*,#17012,.T.) ;
#23010 = ORIENTED_EDGE('',*,*,#17031,.T.) ;
#23011 = ORIENTED_EDGE('',*,*,#17021,.T.) ;
#23012 = ORIENTED_EDGE('',*,*,#17032,.T.) ;
#23013 = ORIENTED_EDGE('',*,*,#16644,.T.) ;
#23014 = ORIENTED_EDGE('',*,*,#17033,.T.) ;
#23015 = ORIENTED_EDGE('',*,*,#17022,.T.) ;
#23016 = ORIENTED_EDGE('',*,*,#16637,.T.) ;
#23017 = ORIENTED_EDGE('',*,*,#17032,.F.) ;
#23018 = ORIENTED_EDGE('',*,*,#17031,.F.) ;
#23019 = ORIENTED_EDGE('',*,*,#17030,.F.) ;
#23020 = ORIENTED_EDGE('',*,*,#17034,.T.) ;
#23021 = ORIENTED_EDGE('',*,*,#16640,.T.) ;
#23022 = ORIENTED_EDGE('',*,*,#17035,.T.) ;
#23023 = ORIENTED_EDGE('',*,*,#17017,.T.) ;
#23024 = ORIENTED_EDGE('',*,*,#17028,.F.) ;
#23025 = ORIENTED_EDGE('',*,*,#17035,.F.) ;
#23026 = ORIENTED_EDGE('',*,*,#16639,.T.) ;
#23027 = ORIENTED_EDGE('',*,*,#17029,.F.) ;
#23028 = ORIENTED_EDGE('',*,*,#17025,.F.) ;
#23029 = ORIENTED_EDGE('',*,*,#17033,.F.) ;
#23030 = ORIENTED_EDGE('',*,*,#16643,.T.) ;
#23031 = ORIENTED_EDGE('',*,*,#17026,.F.) ;
#23032 = ORIENTED_EDGE('',*,*,#17024,.F.) ;
#23033 = ORIENTED_EDGE('',*,*,#17027,.F.) ;
#23034 = ORIENTED_EDGE('',*,*,#16641,.T.) ;
#23035 = ORIENTED_EDGE('',*,*,#17034,.F.) ;
#23036 = ORIENTED_EDGE('',*,*,#17036,.F.) ;
#23037 = ORIENTED_EDGE('',*,*,#17037,.F.) ;
#23038 = ORIENTED_EDGE('',*,*,#17038,.F.) ;
#23039 = ORIENTED_EDGE('',*,*,#17005,.F.) ;
#23040 = ORIENTED_EDGE('',*,*,#17039,.F.) ;
#23041 = ORIENTED_EDGE('',*,*,#16962,.T.) ;
#23042 = ORIENTED_EDGE('',*,*,#17004,.T.) ;
#23043 = ORIENTED_EDGE('',*,*,#16976,.F.) ;
#23044 = ORIENTED_EDGE('',*,*,#16488,.F.) ;
#23045 = ORIENTED_EDGE('',*,*,#16733,.T.) ;
#23046 = ORIENTED_EDGE('',*,*,#16737,.F.) ;
#23047 = ORIENTED_EDGE('',*,*,#17040,.F.) ;
#23048 = ORIENTED_EDGE('',*,*,#17041,.T.) ;
#23049 = ORIENTED_EDGE('',*,*,#17039,.T.) ;
#23050 = ORIENTED_EDGE('',*,*,#16736,.T.) ;
#23051 = ORIENTED_EDGE('',*,*,#17042,.F.) ;
#23052 = ORIENTED_EDGE('',*,*,#16721,.F.) ;
#23053 = ORIENTED_EDGE('',*,*,#16718,.F.) ;
#23054 = ORIENTED_EDGE('',*,*,#16490,.F.) ;
#23055 = ORIENTED_EDGE('',*,*,#16978,.T.) ;
#23056 = ORIENTED_EDGE('',*,*,#17003,.T.) ;
#23057 = ORIENTED_EDGE('',*,*,#16961,.T.) ;
#23058 = ORIENTED_EDGE('',*,*,#16937,.T.) ;
#23059 = ORIENTED_EDGE('',*,*,#16923,.T.) ;
#23060 = ORIENTED_EDGE('',*,*,#16722,.T.) ;
#23061 = ORIENTED_EDGE('',*,*,#17042,.T.) ;
#23062 = ORIENTED_EDGE('',*,*,#17043,.T.) ;
#23063 = ORIENTED_EDGE('',*,*,#17044,.F.) ;
#23064 = ORIENTED_EDGE('',*,*,#16767,.T.) ;
#23065 = ORIENTED_EDGE('',*,*,#17006,.F.) ;
#23066 = ORIENTED_EDGE('',*,*,#17038,.T.) ;
#23067 = ORIENTED_EDGE('',*,*,#17045,.T.) ;
#23068 = ORIENTED_EDGE('',*,*,#17046,.F.) ;
#23069 = ORIENTED_EDGE('',*,*,#16745,.T.) ;
#23070 = ORIENTED_EDGE('',*,*,#16925,.T.) ;
#23071 = ORIENTED_EDGE('',*,*,#16939,.T.) ;
#23072 = ORIENTED_EDGE('',*,*,#17047,.T.) ;
#23073 = ORIENTED_EDGE('',*,*,#17048,.F.) ;
#23074 = ORIENTED_EDGE('',*,*,#17049,.F.) ;
#23075 = ORIENTED_EDGE('',*,*,#17050,.F.) ;
#23076 = ORIENTED_EDGE('',*,*,#17047,.F.) ;
#23077 = ORIENTED_EDGE('',*,*,#16938,.T.) ;
#23078 = ORIENTED_EDGE('',*,*,#17043,.F.) ;
#23079 = ORIENTED_EDGE('',*,*,#16960,.F.) ;
#23080 = ORIENTED_EDGE('',*,*,#17041,.F.) ;
#23081 = ORIENTED_EDGE('',*,*,#16945,.T.) ;
#23082 = ORIENTED_EDGE('',*,*,#16950,.T.) ;
#23083 = ORIENTED_EDGE('',*,*,#16955,.T.) ;
#23084 = ORIENTED_EDGE('',*,*,#16940,.T.) ;
#23085 = ORIENTED_EDGE('',*,*,#17046,.T.) ;
#23086 = ORIENTED_EDGE('',*,*,#17050,.T.) ;
#23087 = ORIENTED_EDGE('',*,*,#17051,.F.) ;
#23088 = ORIENTED_EDGE('',*,*,#16743,.T.) ;
#23089 = ORIENTED_EDGE('',*,*,#17051,.T.) ;
#23090 = ORIENTED_EDGE('',*,*,#17049,.T.) ;
#23091 = ORIENTED_EDGE('',*,*,#17052,.F.) ;
#23092 = ORIENTED_EDGE('',*,*,#16741,.T.) ;
#23093 = ORIENTED_EDGE('',*,*,#17040,.T.) ;
#23094 = ORIENTED_EDGE('',*,*,#16739,.T.) ;
#23095 = ORIENTED_EDGE('',*,*,#17052,.T.) ;
#23096 = ORIENTED_EDGE('',*,*,#17048,.T.) ;
#23097 = ORIENTED_EDGE('',*,*,#17053,.F.) ;
#23098 = ORIENTED_EDGE('',*,*,#17045,.F.) ;
#23099 = ORIENTED_EDGE('',*,*,#17037,.T.) ;
#23100 = ORIENTED_EDGE('',*,*,#17054,.F.) ;
#23101 = ORIENTED_EDGE('',*,*,#17055,.F.) ;
#23102 = ORIENTED_EDGE('',*,*,#17056,.F.) ;
#23103 = ORIENTED_EDGE('',*,*,#16835,.T.) ;
#23104 = ORIENTED_EDGE('',*,*,#17057,.F.) ;
#23105 = ORIENTED_EDGE('',*,*,#17054,.T.) ;
#23106 = ORIENTED_EDGE('',*,*,#17036,.T.) ;
#23107 = ORIENTED_EDGE('',*,*,#17007,.T.) ;
#23108 = ORIENTED_EDGE('',*,*,#16758,.T.) ;
#23109 = ORIENTED_EDGE('',*,*,#17044,.T.) ;
#23110 = ORIENTED_EDGE('',*,*,#17053,.T.) ;
#23111 = ORIENTED_EDGE('',*,*,#17058,.F.) ;
#23112 = ORIENTED_EDGE('',*,*,#16765,.T.) ;
#23113 = ORIENTED_EDGE('',*,*,#17058,.T.) ;
#23114 = ORIENTED_EDGE('',*,*,#17056,.T.) ;
#23115 = ORIENTED_EDGE('',*,*,#17059,.F.) ;
#23116 = ORIENTED_EDGE('',*,*,#16763,.T.) ;
#23117 = ORIENTED_EDGE('',*,*,#17059,.T.) ;
#23118 = ORIENTED_EDGE('',*,*,#17055,.T.) ;
#23119 = ORIENTED_EDGE('',*,*,#17057,.T.) ;
#23120 = ORIENTED_EDGE('',*,*,#16761,.T.) ;
#23121 = ORIENTED_EDGE('',*,*,#17060,.F.) ;
#23122 = ORIENTED_EDGE('',*,*,#16280,.F.) ;
#23123 = ORIENTED_EDGE('',*,*,#16411,.F.) ;
#23124 = ORIENTED_EDGE('',*,*,#16288,.F.) ;
#23125 = ORIENTED_EDGE('',*,*,#16287,.F.) ;
#23126 = ORIENTED_EDGE('',*,*,#17061,.F.) ;
#23127 = ORIENTED_EDGE('',*,*,#17062,.F.) ;
#23128 = ORIENTED_EDGE('',*,*,#16234,.T.) ;
#23129 = ORIENTED_EDGE('',*,*,#16233,.T.) ;
#23130 = ORIENTED_EDGE('',*,*,#16420,.T.) ;
#23131 = ORIENTED_EDGE('',*,*,#16231,.T.) ;
#23132 = ORIENTED_EDGE('',*,*,#16227,.T.) ;
#23133 = ORIENTED_EDGE('',*,*,#17063,.F.) ;
#23134 = ORIENTED_EDGE('',*,*,#16225,.F.) ;
#23135 = ORIENTED_EDGE('',*,*,#16230,.F.) ;
#23136 = ORIENTED_EDGE('',*,*,#16229,.F.) ;
#23137 = ORIENTED_EDGE('',*,*,#16419,.F.) ;
#23138 = ORIENTED_EDGE('',*,*,#16236,.F.) ;
#23139 = ORIENTED_EDGE('',*,*,#17064,.F.) ;
#23140 = ORIENTED_EDGE('',*,*,#16285,.F.) ;
#23141 = ORIENTED_EDGE('',*,*,#16284,.F.) ;
#23142 = ORIENTED_EDGE('',*,*,#16412,.F.) ;
#23143 = ORIENTED_EDGE('',*,*,#16282,.F.) ;
#23144 = ORIENTED_EDGE('',*,*,#16278,.F.) ;
#23145 = ORIENTED_EDGE('',*,*,#17065,.F.) ;
#23146 = ORIENTED_EDGE('',*,*,#17066,.F.) ;
#23147 = ORIENTED_EDGE('',*,*,#16254,.F.) ;
#23148 = ORIENTED_EDGE('',*,*,#16415,.F.) ;
#23149 = ORIENTED_EDGE('',*,*,#16262,.F.) ;
#23150 = ORIENTED_EDGE('',*,*,#16261,.F.) ;
#23151 = ORIENTED_EDGE('',*,*,#17067,.F.) ;
#23152 = ORIENTED_EDGE('',*,*,#17068,.F.) ;
#23153 = ORIENTED_EDGE('',*,*,#16220,.T.) ;
#23154 = ORIENTED_EDGE('',*,*,#16219,.T.) ;
#23155 = ORIENTED_EDGE('',*,*,#16423,.T.) ;
#23156 = ORIENTED_EDGE('',*,*,#16217,.T.) ;
#23157 = ORIENTED_EDGE('',*,*,#16213,.T.) ;
#23158 = ORIENTED_EDGE('',*,*,#17069,.F.) ;
#23159 = ORIENTED_EDGE('',*,*,#16211,.F.) ;
#23160 = ORIENTED_EDGE('',*,*,#16216,.F.) ;
#23161 = ORIENTED_EDGE('',*,*,#16215,.F.) ;
#23162 = ORIENTED_EDGE('',*,*,#16422,.F.) ;
#23163 = ORIENTED_EDGE('',*,*,#16421,.F.) ;
#23164 = ORIENTED_EDGE('',*,*,#16223,.F.) ;
#23165 = ORIENTED_EDGE('',*,*,#16222,.F.) ;
#23166 = ORIENTED_EDGE('',*,*,#17070,.F.) ;
#23167 = ORIENTED_EDGE('',*,*,#16259,.F.) ;
#23168 = ORIENTED_EDGE('',*,*,#16258,.F.) ;
#23169 = ORIENTED_EDGE('',*,*,#16416,.F.) ;
#23170 = ORIENTED_EDGE('',*,*,#16256,.F.) ;
#23171 = ORIENTED_EDGE('',*,*,#16252,.F.) ;
#23172 = ORIENTED_EDGE('',*,*,#17071,.F.) ;
#23173 = ORIENTED_EDGE('',*,*,#17072,.F.) ;
#23174 = ORIENTED_EDGE('',*,*,#16241,.F.) ;
#23175 = ORIENTED_EDGE('',*,*,#16417,.F.) ;
#23176 = ORIENTED_EDGE('',*,*,#16249,.F.) ;
#23177 = ORIENTED_EDGE('',*,*,#16248,.F.) ;
#23178 = ORIENTED_EDGE('',*,*,#17073,.F.) ;
#23179 = ORIENTED_EDGE('',*,*,#17074,.F.) ;
#23180 = ORIENTED_EDGE('',*,*,#16206,.T.) ;
#23181 = ORIENTED_EDGE('',*,*,#16205,.T.) ;
#23182 = ORIENTED_EDGE('',*,*,#16204,.T.) ;
#23183 = ORIENTED_EDGE('',*,*,#16425,.T.) ;
#23184 = ORIENTED_EDGE('',*,*,#16202,.T.) ;
#23185 = ORIENTED_EDGE('',*,*,#16201,.T.) ;
#23186 = ORIENTED_EDGE('',*,*,#16197,.T.) ;
#23187 = ORIENTED_EDGE('',*,*,#17075,.F.) ;
#23188 = ORIENTED_EDGE('',*,*,#16195,.F.) ;
#23189 = ORIENTED_EDGE('',*,*,#16200,.F.) ;
#23190 = ORIENTED_EDGE('',*,*,#16199,.F.) ;
#23191 = ORIENTED_EDGE('',*,*,#16424,.F.) ;
#23192 = ORIENTED_EDGE('',*,*,#16209,.F.) ;
#23193 = ORIENTED_EDGE('',*,*,#16208,.F.) ;
#23194 = ORIENTED_EDGE('',*,*,#17076,.F.) ;
#23195 = ORIENTED_EDGE('',*,*,#16246,.F.) ;
#23196 = ORIENTED_EDGE('',*,*,#16245,.F.) ;
#23197 = ORIENTED_EDGE('',*,*,#16418,.F.) ;
#23198 = ORIENTED_EDGE('',*,*,#16243,.F.) ;
#23199 = ORIENTED_EDGE('',*,*,#16239,.F.) ;
#23200 = ORIENTED_EDGE('',*,*,#17077,.F.) ;
#23201 = ORIENTED_EDGE('',*,*,#16453,.T.) ;
#23202 = ORIENTED_EDGE('',*,*,#16692,.F.) ;
#23203 = ORIENTED_EDGE('',*,*,#16970,.T.) ;
#23204 = ORIENTED_EDGE('',*,*,#16849,.T.) ;
#23205 = ORIENTED_EDGE('',*,*,#16967,.T.) ;
#23206 = ORIENTED_EDGE('',*,*,#17000,.T.) ;
#23207 = ORIENTED_EDGE('',*,*,#17002,.T.) ;
#23208 = ORIENTED_EDGE('',*,*,#16853,.T.) ;
#23209 = ORIENTED_EDGE('',*,*,#16997,.T.) ;
#23210 = ORIENTED_EDGE('',*,*,#16995,.F.) ;
#23211 = ORIENTED_EDGE('',*,*,#16710,.T.) ;
#23212 = ORIENTED_EDGE('',*,*,#16706,.T.) ;
#23213 = ORIENTED_EDGE('',*,*,#16460,.T.) ;
#23214 = ORIENTED_EDGE('',*,*,#16714,.T.) ;
#23215 = ORIENTED_EDGE('',*,*,#16676,.T.) ;
#23216 = ORIENTED_EDGE('',*,*,#16688,.T.) ;
#23217 = ORIENTED_EDGE('',*,*,#16820,.T.) ;
#23218 = ORIENTED_EDGE('',*,*,#16857,.F.) ;
#23219 = ORIENTED_EDGE('',*,*,#16919,.T.) ;
#23220 = ORIENTED_EDGE('',*,*,#16901,.T.) ;
#23221 = ORIENTED_EDGE('',*,*,#16894,.T.) ;
#23222 = ORIENTED_EDGE('',*,*,#16860,.F.) ;
#23223 = ORIENTED_EDGE('',*,*,#16917,.T.) ;
#23224 = ORIENTED_EDGE('',*,*,#16906,.T.) ;
#23225 = ORIENTED_EDGE('',*,*,#16904,.T.) ;
#23226 = ORIENTED_EDGE('',*,*,#16843,.T.) ;
#23227 = ORIENTED_EDGE('',*,*,#16914,.T.) ;
#23228 = ORIENTED_EDGE('',*,*,#16900,.F.) ;
#23229 = ORIENTED_EDGE('',*,*,#16897,.T.) ;
#23230 = ORIENTED_EDGE('',*,*,#16847,.T.) ;
#23231 = ORIENTED_EDGE('',*,*,#16916,.T.) ;
#23232 = ORIENTED_EDGE('',*,*,#16689,.T.) ;
#23233 = ORIENTED_EDGE('',*,*,#17078,.T.) ;
#23234 = ORIENTED_EDGE('',*,*,#17079,.T.) ;
#23235 = ORIENTED_EDGE('',*,*,#17080,.T.) ;
#23236 = ORIENTED_EDGE('',*,*,#17081,.T.) ;
#23237 = ORIENTED_EDGE('',*,*,#17082,.T.) ;
#23238 = ORIENTED_EDGE('',*,*,#17083,.T.) ;
#23239 = ORIENTED_EDGE('',*,*,#16803,.T.) ;
#23240 = ORIENTED_EDGE('',*,*,#16797,.T.) ;
#23241 = ORIENTED_EDGE('',*,*,#16794,.T.) ;
#23242 = ORIENTED_EDGE('',*,*,#16791,.T.) ;
#23243 = ORIENTED_EDGE('',*,*,#16788,.T.) ;
#23244 = ORIENTED_EDGE('',*,*,#16801,.T.) ;
#23245 = ORIENTED_EDGE('',*,*,#16785,.T.) ;
#23246 = ORIENTED_EDGE('',*,*,#16779,.T.) ;
#23247 = ORIENTED_EDGE('',*,*,#16776,.T.) ;
#23248 = ORIENTED_EDGE('',*,*,#16773,.T.) ;
#23249 = ORIENTED_EDGE('',*,*,#16770,.T.) ;
#23250 = ORIENTED_EDGE('',*,*,#16783,.T.) ;
#23251 = ORIENTED_EDGE('',*,*,#17084,.T.) ;
#23252 = ORIENTED_EDGE('',*,*,#17085,.T.) ;
#23253 = ORIENTED_EDGE('',*,*,#17086,.T.) ;
#23254 = ORIENTED_EDGE('',*,*,#17087,.T.) ;
#23255 = ORIENTED_EDGE('',*,*,#17088,.T.) ;
#23256 = ORIENTED_EDGE('',*,*,#17089,.T.) ;
#23257 = ORIENTED_EDGE('',*,*,#17090,.T.) ;
#23258 = ORIENTED_EDGE('',*,*,#17091,.T.) ;
#23259 = ORIENTED_EDGE('',*,*,#17092,.T.) ;
#23260 = ORIENTED_EDGE('',*,*,#17093,.T.) ;
#23261 = ORIENTED_EDGE('',*,*,#17094,.T.) ;
#23262 = ORIENTED_EDGE('',*,*,#17095,.T.) ;
#23263 = ORIENTED_EDGE('',*,*,#17076,.T.) ;
#23264 = ORIENTED_EDGE('',*,*,#16207,.T.) ;
#23265 = ORIENTED_EDGE('',*,*,#17074,.T.) ;
#23266 = ORIENTED_EDGE('',*,*,#17073,.T.) ;
#23267 = ORIENTED_EDGE('',*,*,#16247,.T.) ;
#23268 = ORIENTED_EDGE('',*,*,#17070,.T.) ;
#23269 = ORIENTED_EDGE('',*,*,#16221,.T.) ;
#23270 = ORIENTED_EDGE('',*,*,#17068,.T.) ;
#23271 = ORIENTED_EDGE('',*,*,#17067,.T.) ;
#23272 = ORIENTED_EDGE('',*,*,#16260,.T.) ;
#23273 = ORIENTED_EDGE('',*,*,#17096,.T.) ;
#23274 = ORIENTED_EDGE('',*,*,#16192,.T.) ;
#23275 = ORIENTED_EDGE('',*,*,#17097,.T.) ;
#23276 = ORIENTED_EDGE('',*,*,#17098,.T.) ;
#23277 = ORIENTED_EDGE('',*,*,#16273,.T.) ;
#23278 = ORIENTED_EDGE('',*,*,#17064,.T.) ;
#23279 = ORIENTED_EDGE('',*,*,#16235,.T.) ;
#23280 = ORIENTED_EDGE('',*,*,#17062,.T.) ;
#23281 = ORIENTED_EDGE('',*,*,#17061,.T.) ;
#23282 = ORIENTED_EDGE('',*,*,#16286,.T.) ;
#23283 = ORIENTED_EDGE('',*,*,#17099,.F.) ;
#23284 = ORIENTED_EDGE('',*,*,#16267,.F.) ;
#23285 = ORIENTED_EDGE('',*,*,#16413,.F.) ;
#23286 = ORIENTED_EDGE('',*,*,#16275,.F.) ;
#23287 = ORIENTED_EDGE('',*,*,#16274,.F.) ;
#23288 = ORIENTED_EDGE('',*,*,#17098,.F.) ;
#23289 = ORIENTED_EDGE('',*,*,#17097,.F.) ;
#23290 = ORIENTED_EDGE('',*,*,#16191,.T.) ;
#23291 = ORIENTED_EDGE('',*,*,#16190,.T.) ;
#23292 = ORIENTED_EDGE('',*,*,#16427,.T.) ;
#23293 = ORIENTED_EDGE('',*,*,#16188,.T.) ;
#23294 = ORIENTED_EDGE('',*,*,#16184,.T.) ;
#23295 = ORIENTED_EDGE('',*,*,#17100,.F.) ;
#23296 = ORIENTED_EDGE('',*,*,#16182,.F.) ;
#23297 = ORIENTED_EDGE('',*,*,#16187,.F.) ;
#23298 = ORIENTED_EDGE('',*,*,#16186,.F.) ;
#23299 = ORIENTED_EDGE('',*,*,#16426,.F.) ;
#23300 = ORIENTED_EDGE('',*,*,#16193,.F.) ;
#23301 = ORIENTED_EDGE('',*,*,#17096,.F.) ;
#23302 = ORIENTED_EDGE('',*,*,#16272,.F.) ;
#23303 = ORIENTED_EDGE('',*,*,#16271,.F.) ;
#23304 = ORIENTED_EDGE('',*,*,#16414,.F.) ;
#23305 = ORIENTED_EDGE('',*,*,#16269,.F.) ;
#23306 = ORIENTED_EDGE('',*,*,#16265,.F.) ;
#23307 = ORIENTED_EDGE('',*,*,#17101,.F.) ;
#23308 = ORIENTED_EDGE('',*,*,#17102,.F.) ;
#23309 = ORIENTED_EDGE('',*,*,#17103,.T.) ;
#23310 = ORIENTED_EDGE('',*,*,#17095,.F.) ;
#23311 = ORIENTED_EDGE('',*,*,#17104,.F.) ;
#23312 = ORIENTED_EDGE('',*,*,#17105,.F.) ;
#23313 = ORIENTED_EDGE('',*,*,#17104,.T.) ;
#23314 = ORIENTED_EDGE('',*,*,#17094,.F.) ;
#23315 = ORIENTED_EDGE('',*,*,#17106,.F.) ;
#23316 = ORIENTED_EDGE('',*,*,#17107,.F.) ;
#23317 = ORIENTED_EDGE('',*,*,#17108,.T.) ;
#23318 = ORIENTED_EDGE('',*,*,#17090,.F.) ;
#23319 = ORIENTED_EDGE('',*,*,#17103,.F.) ;
#23320 = ORIENTED_EDGE('',*,*,#17109,.F.) ;
#23321 = ORIENTED_EDGE('',*,*,#17110,.T.) ;
#23322 = ORIENTED_EDGE('',*,*,#17091,.F.) ;
#23323 = ORIENTED_EDGE('',*,*,#17108,.F.) ;
#23324 = ORIENTED_EDGE('',*,*,#17111,.F.) ;
#23325 = ORIENTED_EDGE('',*,*,#17112,.T.) ;
#23326 = ORIENTED_EDGE('',*,*,#17092,.F.) ;
#23327 = ORIENTED_EDGE('',*,*,#17110,.F.) ;
#23328 = ORIENTED_EDGE('',*,*,#17113,.F.) ;
#23329 = ORIENTED_EDGE('',*,*,#17106,.T.) ;
#23330 = ORIENTED_EDGE('',*,*,#17093,.F.) ;
#23331 = ORIENTED_EDGE('',*,*,#17112,.F.) ;
#23332 = ORIENTED_EDGE('',*,*,#17114,.F.) ;
#23333 = ORIENTED_EDGE('',*,*,#17115,.T.) ;
#23334 = ORIENTED_EDGE('',*,*,#17083,.F.) ;
#23335 = ORIENTED_EDGE('',*,*,#17116,.F.) ;
#23336 = ORIENTED_EDGE('',*,*,#17117,.F.) ;
#23337 = ORIENTED_EDGE('',*,*,#17116,.T.) ;
#23338 = ORIENTED_EDGE('',*,*,#17082,.F.) ;
#23339 = ORIENTED_EDGE('',*,*,#17118,.F.) ;
#23340 = ORIENTED_EDGE('',*,*,#17119,.F.) ;
#23341 = ORIENTED_EDGE('',*,*,#17120,.T.) ;
#23342 = ORIENTED_EDGE('',*,*,#17078,.F.) ;
#23343 = ORIENTED_EDGE('',*,*,#17115,.F.) ;
#23344 = ORIENTED_EDGE('',*,*,#17121,.F.) ;
#23345 = ORIENTED_EDGE('',*,*,#17122,.T.) ;
#23346 = ORIENTED_EDGE('',*,*,#17079,.F.) ;
#23347 = ORIENTED_EDGE('',*,*,#17120,.F.) ;
#23348 = ORIENTED_EDGE('',*,*,#17123,.F.) ;
#23349 = ORIENTED_EDGE('',*,*,#17124,.T.) ;
#23350 = ORIENTED_EDGE('',*,*,#17080,.F.) ;
#23351 = ORIENTED_EDGE('',*,*,#17122,.F.) ;
#23352 = ORIENTED_EDGE('',*,*,#17125,.F.) ;
#23353 = ORIENTED_EDGE('',*,*,#17118,.T.) ;
#23354 = ORIENTED_EDGE('',*,*,#17081,.F.) ;
#23355 = ORIENTED_EDGE('',*,*,#17124,.F.) ;
#23356 = ORIENTED_EDGE('',*,*,#16448,.T.) ;
#23357 = ORIENTED_EDGE('',*,*,#16431,.F.) ;
#23358 = ORIENTED_EDGE('',*,*,#16915,.F.) ;
#23359 = ORIENTED_EDGE('',*,*,#16845,.T.) ;
#23360 = ORIENTED_EDGE('',*,*,#16896,.F.) ;
#23361 = ORIENTED_EDGE('',*,*,#16814,.F.) ;
#23362 = ORIENTED_EDGE('',*,*,#16913,.F.) ;
#23363 = ORIENTED_EDGE('',*,*,#16841,.T.) ;
#23364 = ORIENTED_EDGE('',*,*,#16903,.T.) ;
#23365 = ORIENTED_EDGE('',*,*,#16816,.F.) ;
#23366 = ORIENTED_EDGE('',*,*,#16918,.T.) ;
#23367 = ORIENTED_EDGE('',*,*,#16862,.T.) ;
#23368 = ORIENTED_EDGE('',*,*,#16893,.T.) ;
#23369 = ORIENTED_EDGE('',*,*,#16806,.F.) ;
#23370 = ORIENTED_EDGE('',*,*,#16920,.T.) ;
#23371 = ORIENTED_EDGE('',*,*,#16858,.T.) ;
#23372 = ORIENTED_EDGE('',*,*,#16818,.T.) ;
#23373 = ORIENTED_EDGE('',*,*,#16513,.F.) ;
#23374 = ORIENTED_EDGE('',*,*,#16678,.F.) ;
#23375 = ORIENTED_EDGE('',*,*,#16462,.F.) ;
#23376 = ORIENTED_EDGE('',*,*,#16709,.F.) ;
#23377 = ORIENTED_EDGE('',*,*,#16694,.T.) ;
#23378 = ORIENTED_EDGE('',*,*,#16998,.T.) ;
#23379 = ORIENTED_EDGE('',*,*,#16855,.T.) ;
#23380 = ORIENTED_EDGE('',*,*,#17001,.T.) ;
#23381 = ORIENTED_EDGE('',*,*,#16809,.F.) ;
#23382 = ORIENTED_EDGE('',*,*,#16968,.T.) ;
#23383 = ORIENTED_EDGE('',*,*,#16851,.T.) ;
#23384 = ORIENTED_EDGE('',*,*,#16969,.T.) ;
#23385 = ORIENTED_EDGE('',*,*,#16810,.F.) ;
#23386 = ORIENTED_EDGE('',*,*,#16778,.T.) ;
#23387 = ORIENTED_EDGE('',*,*,#16784,.T.) ;
#23388 = ORIENTED_EDGE('',*,*,#16781,.T.) ;
#23389 = ORIENTED_EDGE('',*,*,#16768,.T.) ;
#23390 = ORIENTED_EDGE('',*,*,#16772,.T.) ;
#23391 = ORIENTED_EDGE('',*,*,#16775,.T.) ;
#23392 = ORIENTED_EDGE('',*,*,#16796,.T.) ;
#23393 = ORIENTED_EDGE('',*,*,#16802,.T.) ;
#23394 = ORIENTED_EDGE('',*,*,#16799,.T.) ;
#23395 = ORIENTED_EDGE('',*,*,#16786,.T.) ;
#23396 = ORIENTED_EDGE('',*,*,#16790,.T.) ;
#23397 = ORIENTED_EDGE('',*,*,#16793,.T.) ;
#23398 = ORIENTED_EDGE('',*,*,#17063,.T.) ;
#23399 = ORIENTED_EDGE('',*,*,#17065,.T.) ;
#23400 = ORIENTED_EDGE('',*,*,#16277,.T.) ;
#23401 = ORIENTED_EDGE('',*,*,#16281,.T.) ;
#23402 = ORIENTED_EDGE('',*,*,#17060,.T.) ;
#23403 = ORIENTED_EDGE('',*,*,#16226,.T.) ;
#23404 = ORIENTED_EDGE('',*,*,#17069,.T.) ;
#23405 = ORIENTED_EDGE('',*,*,#17071,.T.) ;
#23406 = ORIENTED_EDGE('',*,*,#16251,.T.) ;
#23407 = ORIENTED_EDGE('',*,*,#16255,.T.) ;
#23408 = ORIENTED_EDGE('',*,*,#17066,.T.) ;
#23409 = ORIENTED_EDGE('',*,*,#16212,.T.) ;
#23410 = ORIENTED_EDGE('',*,*,#17075,.T.) ;
#23411 = ORIENTED_EDGE('',*,*,#17077,.T.) ;
#23412 = ORIENTED_EDGE('',*,*,#16238,.T.) ;
#23413 = ORIENTED_EDGE('',*,*,#16242,.T.) ;
#23414 = ORIENTED_EDGE('',*,*,#17072,.T.) ;
#23415 = ORIENTED_EDGE('',*,*,#16196,.T.) ;
#23416 = ORIENTED_EDGE('',*,*,#17100,.T.) ;
#23417 = ORIENTED_EDGE('',*,*,#17101,.T.) ;
#23418 = ORIENTED_EDGE('',*,*,#16264,.T.) ;
#23419 = ORIENTED_EDGE('',*,*,#16268,.T.) ;
#23420 = ORIENTED_EDGE('',*,*,#17099,.T.) ;
#23421 = ORIENTED_EDGE('',*,*,#16183,.T.) ;
#23422 = ORIENTED_EDGE('',*,*,#17107,.T.) ;
#23423 = ORIENTED_EDGE('',*,*,#17102,.T.) ;
#23424 = ORIENTED_EDGE('',*,*,#17105,.T.) ;
#23425 = ORIENTED_EDGE('',*,*,#17113,.T.) ;
#23426 = ORIENTED_EDGE('',*,*,#17111,.T.) ;
#23427 = ORIENTED_EDGE('',*,*,#17109,.T.) ;
#23428 = ORIENTED_EDGE('',*,*,#17119,.T.) ;
#23429 = ORIENTED_EDGE('',*,*,#17114,.T.) ;
#23430 = ORIENTED_EDGE('',*,*,#17117,.T.) ;
#23431 = ORIENTED_EDGE('',*,*,#17125,.T.) ;
#23432 = ORIENTED_EDGE('',*,*,#17123,.T.) ;
#23433 = ORIENTED_EDGE('',*,*,#17121,.T.) ;
#23434 = ORIENTED_EDGE('',*,*,#17126,.T.) ;
#23435 = ORIENTED_EDGE('',*,*,#17127,.T.) ;
#23436 = ORIENTED_EDGE('',*,*,#17128,.T.) ;
#23437 = ORIENTED_EDGE('',*,*,#17129,.T.) ;
#23438 = ORIENTED_EDGE('',*,*,#17130,.T.) ;
#23439 = ORIENTED_EDGE('',*,*,#17131,.T.) ;
#23440 = ORIENTED_EDGE('',*,*,#17127,.F.) ;
#23441 = ORIENTED_EDGE('',*,*,#17132,.T.) ;
#23442 = ORIENTED_EDGE('',*,*,#17089,.F.) ;
#23443 = ORIENTED_EDGE('',*,*,#17133,.F.) ;
#23444 = ORIENTED_EDGE('',*,*,#17128,.F.) ;
#23445 = ORIENTED_EDGE('',*,*,#17133,.T.) ;
#23446 = ORIENTED_EDGE('',*,*,#17088,.F.) ;
#23447 = ORIENTED_EDGE('',*,*,#17134,.F.) ;
#23448 = ORIENTED_EDGE('',*,*,#17126,.F.) ;
#23449 = ORIENTED_EDGE('',*,*,#17135,.T.) ;
#23450 = ORIENTED_EDGE('',*,*,#17084,.F.) ;
#23451 = ORIENTED_EDGE('',*,*,#17132,.F.) ;
#23452 = ORIENTED_EDGE('',*,*,#17131,.F.) ;
#23453 = ORIENTED_EDGE('',*,*,#17136,.T.) ;
#23454 = ORIENTED_EDGE('',*,*,#17085,.F.) ;
#23455 = ORIENTED_EDGE('',*,*,#17135,.F.) ;
#23456 = ORIENTED_EDGE('',*,*,#17130,.F.) ;
#23457 = ORIENTED_EDGE('',*,*,#17137,.T.) ;
#23458 = ORIENTED_EDGE('',*,*,#17086,.F.) ;
#23459 = ORIENTED_EDGE('',*,*,#17136,.F.) ;
#23460 = ORIENTED_EDGE('',*,*,#17129,.F.) ;
#23461 = ORIENTED_EDGE('',*,*,#17134,.T.) ;
#23462 = ORIENTED_EDGE('',*,*,#17087,.F.) ;
#23463 = ORIENTED_EDGE('',*,*,#17137,.F.) ;
#23464 = ORIENTED_EDGE('',*,*,#17138,.F.) ;
#23465 = ORIENTED_EDGE('',*,*,#17139,.T.) ;
#23466 = ORIENTED_EDGE('',*,*,#17140,.T.) ;
#23467 = ORIENTED_EDGE('',*,*,#17141,.F.) ;
#23468 = ORIENTED_EDGE('',*,*,#17142,.F.) ;
#23469 = ORIENTED_EDGE('',*,*,#17143,.F.) ;
#23470 = ORIENTED_EDGE('',*,*,#17144,.T.) ;
#23471 = ORIENTED_EDGE('',*,*,#17139,.F.) ;
#23472 = ORIENTED_EDGE('',*,*,#17145,.F.) ;
#23473 = ORIENTED_EDGE('',*,*,#17141,.T.) ;
#23474 = ORIENTED_EDGE('',*,*,#17146,.T.) ;
#23475 = ORIENTED_EDGE('',*,*,#17147,.F.) ;
#23476 = ORIENTED_EDGE('',*,*,#17146,.F.) ;
#23477 = ORIENTED_EDGE('',*,*,#17140,.F.) ;
#23478 = ORIENTED_EDGE('',*,*,#17144,.F.) ;
#23479 = ORIENTED_EDGE('',*,*,#17148,.F.) ;
#23480 = ORIENTED_EDGE('',*,*,#17149,.F.) ;
#23481 = ORIENTED_EDGE('',*,*,#17150,.T.) ;
#23482 = ORIENTED_EDGE('',*,*,#17151,.T.) ;
#23483 = ORIENTED_EDGE('',*,*,#17152,.F.) ;
#23484 = ORIENTED_EDGE('',*,*,#17153,.F.) ;
#23485 = ORIENTED_EDGE('',*,*,#17154,.F.) ;
#23486 = ORIENTED_EDGE('',*,*,#17155,.T.) ;
#23487 = ORIENTED_EDGE('',*,*,#17150,.F.) ;
#23488 = ORIENTED_EDGE('',*,*,#17156,.F.) ;
#23489 = ORIENTED_EDGE('',*,*,#17152,.T.) ;
#23490 = ORIENTED_EDGE('',*,*,#17157,.T.) ;
#23491 = ORIENTED_EDGE('',*,*,#17158,.F.) ;
#23492 = ORIENTED_EDGE('',*,*,#17157,.F.) ;
#23493 = ORIENTED_EDGE('',*,*,#17151,.F.) ;
#23494 = ORIENTED_EDGE('',*,*,#17155,.F.) ;
#23495 = ORIENTED_EDGE('',*,*,#17159,.F.) ;
#23496 = ORIENTED_EDGE('',*,*,#17160,.F.) ;
#23497 = ORIENTED_EDGE('',*,*,#17161,.T.) ;
#23498 = ORIENTED_EDGE('',*,*,#17162,.T.) ;
#23499 = ORIENTED_EDGE('',*,*,#17163,.F.) ;
#23500 = ORIENTED_EDGE('',*,*,#17164,.F.) ;
#23501 = ORIENTED_EDGE('',*,*,#17165,.T.) ;
#23502 = ORIENTED_EDGE('',*,*,#17166,.T.) ;
#23503 = ORIENTED_EDGE('',*,*,#17161,.F.) ;
#23504 = ORIENTED_EDGE('',*,*,#17167,.F.) ;
#23505 = ORIENTED_EDGE('',*,*,#17168,.F.) ;
#23506 = ORIENTED_EDGE('',*,*,#17169,.T.) ;
#23507 = ORIENTED_EDGE('',*,*,#17165,.F.) ;
#23508 = ORIENTED_EDGE('',*,*,#17169,.F.) ;
#23509 = ORIENTED_EDGE('',*,*,#17170,.F.) ;
#23510 = ORIENTED_EDGE('',*,*,#17162,.F.) ;
#23511 = ORIENTED_EDGE('',*,*,#17166,.F.) ;
#23512 = ORIENTED_EDGE('',*,*,#17171,.F.) ;
#23513 = ORIENTED_EDGE('',*,*,#17172,.T.) ;
#23514 = ORIENTED_EDGE('',*,*,#17173,.T.) ;
#23515 = ORIENTED_EDGE('',*,*,#17174,.F.) ;
#23516 = ORIENTED_EDGE('',*,*,#17175,.F.) ;
#23517 = ORIENTED_EDGE('',*,*,#17176,.F.) ;
#23518 = ORIENTED_EDGE('',*,*,#17177,.T.) ;
#23519 = ORIENTED_EDGE('',*,*,#17172,.F.) ;
#23520 = ORIENTED_EDGE('',*,*,#17178,.F.) ;
#23521 = ORIENTED_EDGE('',*,*,#17174,.T.) ;
#23522 = ORIENTED_EDGE('',*,*,#17179,.T.) ;
#23523 = ORIENTED_EDGE('',*,*,#17180,.F.) ;
#23524 = ORIENTED_EDGE('',*,*,#17179,.F.) ;
#23525 = ORIENTED_EDGE('',*,*,#17173,.F.) ;
#23526 = ORIENTED_EDGE('',*,*,#17177,.F.) ;
#23527 = ORIENTED_EDGE('',*,*,#17181,.F.) ;
#23528 = ORIENTED_EDGE('',*,*,#17182,.F.) ;
#23529 = ORIENTED_EDGE('',*,*,#17183,.T.) ;
#23530 = ORIENTED_EDGE('',*,*,#17184,.T.) ;
#23531 = ORIENTED_EDGE('',*,*,#17185,.F.) ;
#23532 = ORIENTED_EDGE('',*,*,#17186,.F.) ;
#23533 = ORIENTED_EDGE('',*,*,#17187,.F.) ;
#23534 = ORIENTED_EDGE('',*,*,#17188,.T.) ;
#23535 = ORIENTED_EDGE('',*,*,#17183,.F.) ;
#23536 = ORIENTED_EDGE('',*,*,#17189,.F.) ;
#23537 = ORIENTED_EDGE('',*,*,#17185,.T.) ;
#23538 = ORIENTED_EDGE('',*,*,#17190,.T.) ;
#23539 = ORIENTED_EDGE('',*,*,#17191,.F.) ;
#23540 = ORIENTED_EDGE('',*,*,#17190,.F.) ;
#23541 = ORIENTED_EDGE('',*,*,#17184,.F.) ;
#23542 = ORIENTED_EDGE('',*,*,#17188,.F.) ;
#23543 = ORIENTED_EDGE('',*,*,#17192,.F.) ;
#23544 = ORIENTED_EDGE('',*,*,#17193,.F.) ;
#23545 = ORIENTED_EDGE('',*,*,#17194,.T.) ;
#23546 = ORIENTED_EDGE('',*,*,#17195,.T.) ;
#23547 = ORIENTED_EDGE('',*,*,#17196,.F.) ;
#23548 = ORIENTED_EDGE('',*,*,#17197,.F.) ;
#23549 = ORIENTED_EDGE('',*,*,#17198,.F.) ;
#23550 = ORIENTED_EDGE('',*,*,#17199,.T.) ;
#23551 = ORIENTED_EDGE('',*,*,#17194,.F.) ;
#23552 = ORIENTED_EDGE('',*,*,#17200,.F.) ;
#23553 = ORIENTED_EDGE('',*,*,#17196,.T.) ;
#23554 = ORIENTED_EDGE('',*,*,#17201,.T.) ;
#23555 = ORIENTED_EDGE('',*,*,#17202,.F.) ;
#23556 = ORIENTED_EDGE('',*,*,#17201,.F.) ;
#23557 = ORIENTED_EDGE('',*,*,#17195,.F.) ;
#23558 = ORIENTED_EDGE('',*,*,#17199,.F.) ;
#23559 = ORIENTED_EDGE('',*,*,#17203,.F.) ;
#23560 = ORIENTED_EDGE('',*,*,#17204,.F.) ;
#23561 = ORIENTED_EDGE('',*,*,#17205,.T.) ;
#23562 = ORIENTED_EDGE('',*,*,#17206,.T.) ;
#23563 = ORIENTED_EDGE('',*,*,#17207,.F.) ;
#23564 = ORIENTED_EDGE('',*,*,#17208,.F.) ;
#23565 = ORIENTED_EDGE('',*,*,#17209,.T.) ;
#23566 = ORIENTED_EDGE('',*,*,#17210,.T.) ;
#23567 = ORIENTED_EDGE('',*,*,#17205,.F.) ;
#23568 = ORIENTED_EDGE('',*,*,#17211,.F.) ;
#23569 = ORIENTED_EDGE('',*,*,#17212,.F.) ;
#23570 = ORIENTED_EDGE('',*,*,#17213,.T.) ;
#23571 = ORIENTED_EDGE('',*,*,#17209,.F.) ;
#23572 = ORIENTED_EDGE('',*,*,#17213,.F.) ;
#23573 = ORIENTED_EDGE('',*,*,#17214,.F.) ;
#23574 = ORIENTED_EDGE('',*,*,#17206,.F.) ;
#23575 = ORIENTED_EDGE('',*,*,#17210,.F.) ;
#23576 = ORIENTED_EDGE('',*,*,#17215,.F.) ;
#23577 = ORIENTED_EDGE('',*,*,#17216,.T.) ;
#23578 = ORIENTED_EDGE('',*,*,#17217,.T.) ;
#23579 = ORIENTED_EDGE('',*,*,#17218,.F.) ;
#23580 = ORIENTED_EDGE('',*,*,#17219,.F.) ;
#23581 = ORIENTED_EDGE('',*,*,#17220,.F.) ;
#23582 = ORIENTED_EDGE('',*,*,#17221,.T.) ;
#23583 = ORIENTED_EDGE('',*,*,#17216,.F.) ;
#23584 = ORIENTED_EDGE('',*,*,#17222,.F.) ;
#23585 = ORIENTED_EDGE('',*,*,#17218,.T.) ;
#23586 = ORIENTED_EDGE('',*,*,#17223,.T.) ;
#23587 = ORIENTED_EDGE('',*,*,#17224,.F.) ;
#23588 = ORIENTED_EDGE('',*,*,#17223,.F.) ;
#23589 = ORIENTED_EDGE('',*,*,#17217,.F.) ;
#23590 = ORIENTED_EDGE('',*,*,#17221,.F.) ;
#23591 = ORIENTED_EDGE('',*,*,#17225,.F.) ;
#23592 = ORIENTED_EDGE('',*,*,#17226,.F.) ;
#23593 = ORIENTED_EDGE('',*,*,#17227,.T.) ;
#23594 = ORIENTED_EDGE('',*,*,#17228,.T.) ;
#23595 = ORIENTED_EDGE('',*,*,#17229,.F.) ;
#23596 = ORIENTED_EDGE('',*,*,#17230,.F.) ;
#23597 = ORIENTED_EDGE('',*,*,#17231,.F.) ;
#23598 = ORIENTED_EDGE('',*,*,#17232,.T.) ;
#23599 = ORIENTED_EDGE('',*,*,#17227,.F.) ;
#23600 = ORIENTED_EDGE('',*,*,#17233,.F.) ;
#23601 = ORIENTED_EDGE('',*,*,#17229,.T.) ;
#23602 = ORIENTED_EDGE('',*,*,#17234,.T.) ;
#23603 = ORIENTED_EDGE('',*,*,#17235,.F.) ;
#23604 = ORIENTED_EDGE('',*,*,#17234,.F.) ;
#23605 = ORIENTED_EDGE('',*,*,#17228,.F.) ;
#23606 = ORIENTED_EDGE('',*,*,#17232,.F.) ;
#23607 = ORIENTED_EDGE('',*,*,#17236,.F.) ;
#23608 = ORIENTED_EDGE('',*,*,#17147,.T.) ;
#23609 = ORIENTED_EDGE('',*,*,#17148,.T.) ;
#23610 = ORIENTED_EDGE('',*,*,#17143,.T.) ;
#23611 = ORIENTED_EDGE('',*,*,#17237,.F.) ;
#23612 = ORIENTED_EDGE('',*,*,#17180,.T.) ;
#23613 = ORIENTED_EDGE('',*,*,#17181,.T.) ;
#23614 = ORIENTED_EDGE('',*,*,#17176,.T.) ;
#23615 = ORIENTED_EDGE('',*,*,#17238,.F.) ;
#23616 = ORIENTED_EDGE('',*,*,#17224,.T.) ;
#23617 = ORIENTED_EDGE('',*,*,#17225,.T.) ;
#23618 = ORIENTED_EDGE('',*,*,#17220,.T.) ;
#23619 = ORIENTED_EDGE('',*,*,#17239,.F.) ;
#23620 = ORIENTED_EDGE('',*,*,#17202,.T.) ;
#23621 = ORIENTED_EDGE('',*,*,#17203,.T.) ;
#23622 = ORIENTED_EDGE('',*,*,#17198,.T.) ;
#23623 = ORIENTED_EDGE('',*,*,#17240,.F.) ;
#23624 = ORIENTED_EDGE('',*,*,#17158,.T.) ;
#23625 = ORIENTED_EDGE('',*,*,#17159,.T.) ;
#23626 = ORIENTED_EDGE('',*,*,#17154,.T.) ;
#23627 = ORIENTED_EDGE('',*,*,#17241,.F.) ;
#23628 = ORIENTED_EDGE('',*,*,#17163,.T.) ;
#23629 = ORIENTED_EDGE('',*,*,#17170,.T.) ;
#23630 = ORIENTED_EDGE('',*,*,#17168,.T.) ;
#23631 = ORIENTED_EDGE('',*,*,#17242,.F.) ;
#23632 = ORIENTED_EDGE('',*,*,#17207,.T.) ;
#23633 = ORIENTED_EDGE('',*,*,#17214,.T.) ;
#23634 = ORIENTED_EDGE('',*,*,#17212,.T.) ;
#23635 = ORIENTED_EDGE('',*,*,#17243,.F.) ;
#23636 = ORIENTED_EDGE('',*,*,#17244,.F.) ;
#23637 = ORIENTED_EDGE('',*,*,#17245,.T.) ;
#23638 = ORIENTED_EDGE('',*,*,#17246,.T.) ;
#23639 = ORIENTED_EDGE('',*,*,#17247,.T.) ;
#23640 = ORIENTED_EDGE('',*,*,#17248,.T.) ;
#23641 = ORIENTED_EDGE('',*,*,#17249,.T.) ;
#23642 = ORIENTED_EDGE('',*,*,#17250,.T.) ;
#23643 = ORIENTED_EDGE('',*,*,#17251,.T.) ;
#23644 = ORIENTED_EDGE('',*,*,#17252,.T.) ;
#23645 = ORIENTED_EDGE('',*,*,#17253,.T.) ;
#23646 = ORIENTED_EDGE('',*,*,#17254,.T.) ;
#23647 = ORIENTED_EDGE('',*,*,#17255,.T.) ;
#23648 = ORIENTED_EDGE('',*,*,#17256,.T.) ;
#23649 = ORIENTED_EDGE('',*,*,#17257,.T.) ;
#23650 = ORIENTED_EDGE('',*,*,#17258,.T.) ;
#23651 = ORIENTED_EDGE('',*,*,#17259,.T.) ;
#23652 = ORIENTED_EDGE('',*,*,#17260,.T.) ;
#23653 = ORIENTED_EDGE('',*,*,#17261,.T.) ;
#23654 = ORIENTED_EDGE('',*,*,#17262,.T.) ;
#23655 = ORIENTED_EDGE('',*,*,#17263,.T.) ;
#23656 = ORIENTED_EDGE('',*,*,#17264,.T.) ;
#23657 = ORIENTED_EDGE('',*,*,#17265,.T.) ;
#23658 = ORIENTED_EDGE('',*,*,#17266,.T.) ;
#23659 = ORIENTED_EDGE('',*,*,#17267,.T.) ;
#23660 = ORIENTED_EDGE('',*,*,#17268,.T.) ;
#23661 = ORIENTED_EDGE('',*,*,#17269,.T.) ;
#23662 = ORIENTED_EDGE('',*,*,#17270,.T.) ;
#23663 = ORIENTED_EDGE('',*,*,#17271,.T.) ;
#23664 = ORIENTED_EDGE('',*,*,#17272,.T.) ;
#23665 = ORIENTED_EDGE('',*,*,#17273,.T.) ;
#23666 = ORIENTED_EDGE('',*,*,#17274,.T.) ;
#23667 = ORIENTED_EDGE('',*,*,#17275,.T.) ;
#23668 = ORIENTED_EDGE('',*,*,#17276,.T.) ;
#23669 = ORIENTED_EDGE('',*,*,#17277,.T.) ;
#23670 = ORIENTED_EDGE('',*,*,#17278,.T.) ;
#23671 = ORIENTED_EDGE('',*,*,#17279,.T.) ;
#23672 = ORIENTED_EDGE('',*,*,#17280,.T.) ;
#23673 = ORIENTED_EDGE('',*,*,#17281,.T.) ;
#23674 = ORIENTED_EDGE('',*,*,#17282,.T.) ;
#23675 = ORIENTED_EDGE('',*,*,#17283,.F.) ;
#23676 = ORIENTED_EDGE('',*,*,#17235,.T.) ;
#23677 = ORIENTED_EDGE('',*,*,#17236,.T.) ;
#23678 = ORIENTED_EDGE('',*,*,#17231,.T.) ;
#23679 = ORIENTED_EDGE('',*,*,#17284,.F.) ;
#23680 = ORIENTED_EDGE('',*,*,#17191,.T.) ;
#23681 = ORIENTED_EDGE('',*,*,#17192,.T.) ;
#23682 = ORIENTED_EDGE('',*,*,#17187,.T.) ;
#23683 = ORIENTED_EDGE('',*,*,#17285,.F.) ;
#23684 = ORIENTED_EDGE('',*,*,#17286,.T.) ;
#23685 = ORIENTED_EDGE('',*,*,#17287,.T.) ;
#23686 = ORIENTED_EDGE('',*,*,#17288,.T.) ;
#23687 = ORIENTED_EDGE('',*,*,#17287,.F.) ;
#23688 = ORIENTED_EDGE('',*,*,#17289,.T.) ;
#23689 = ORIENTED_EDGE('',*,*,#17290,.T.) ;
#23690 = ORIENTED_EDGE('',*,*,#17286,.F.) ;
#23691 = ORIENTED_EDGE('',*,*,#17290,.F.) ;
#23692 = ORIENTED_EDGE('',*,*,#17291,.F.) ;
#23693 = ORIENTED_EDGE('',*,*,#17292,.F.) ;
#23694 = ORIENTED_EDGE('',*,*,#17293,.F.) ;
#23695 = ORIENTED_EDGE('',*,*,#17294,.F.) ;
#23696 = ORIENTED_EDGE('',*,*,#17295,.T.) ;
#23697 = ORIENTED_EDGE('',*,*,#17296,.F.) ;
#23698 = ORIENTED_EDGE('',*,*,#17297,.T.) ;
#23699 = ORIENTED_EDGE('',*,*,#17298,.F.) ;
#23700 = ORIENTED_EDGE('',*,*,#17299,.T.) ;
#23701 = ORIENTED_EDGE('',*,*,#17300,.F.) ;
#23702 = ORIENTED_EDGE('',*,*,#17301,.T.) ;
#23703 = ORIENTED_EDGE('',*,*,#17302,.F.) ;
#23704 = ORIENTED_EDGE('',*,*,#17288,.F.) ;
#23705 = ORIENTED_EDGE('',*,*,#17303,.T.) ;
#23706 = ORIENTED_EDGE('',*,*,#17304,.T.) ;
#23707 = ORIENTED_EDGE('',*,*,#17305,.T.) ;
#23708 = ORIENTED_EDGE('',*,*,#17304,.F.) ;
#23709 = ORIENTED_EDGE('',*,*,#17306,.T.) ;
#23710 = ORIENTED_EDGE('',*,*,#17307,.T.) ;
#23711 = ORIENTED_EDGE('',*,*,#17303,.F.) ;
#23712 = ORIENTED_EDGE('',*,*,#17307,.F.) ;
#23713 = ORIENTED_EDGE('',*,*,#17308,.F.) ;
#23714 = ORIENTED_EDGE('',*,*,#17309,.F.) ;
#23715 = ORIENTED_EDGE('',*,*,#17310,.F.) ;
#23716 = ORIENTED_EDGE('',*,*,#17311,.F.) ;
#23717 = ORIENTED_EDGE('',*,*,#17312,.T.) ;
#23718 = ORIENTED_EDGE('',*,*,#17313,.F.) ;
#23719 = ORIENTED_EDGE('',*,*,#17314,.T.) ;
#23720 = ORIENTED_EDGE('',*,*,#17315,.F.) ;
#23721 = ORIENTED_EDGE('',*,*,#17316,.T.) ;
#23722 = ORIENTED_EDGE('',*,*,#17317,.F.) ;
#23723 = ORIENTED_EDGE('',*,*,#17318,.T.) ;
#23724 = ORIENTED_EDGE('',*,*,#17319,.F.) ;
#23725 = ORIENTED_EDGE('',*,*,#17305,.F.) ;
#23726 = ORIENTED_EDGE('',*,*,#17320,.T.) ;
#23727 = ORIENTED_EDGE('',*,*,#17321,.T.) ;
#23728 = ORIENTED_EDGE('',*,*,#17322,.T.) ;
#23729 = ORIENTED_EDGE('',*,*,#17321,.F.) ;
#23730 = ORIENTED_EDGE('',*,*,#17323,.T.) ;
#23731 = ORIENTED_EDGE('',*,*,#17324,.T.) ;
#23732 = ORIENTED_EDGE('',*,*,#17320,.F.) ;
#23733 = ORIENTED_EDGE('',*,*,#17324,.F.) ;
#23734 = ORIENTED_EDGE('',*,*,#17325,.F.) ;
#23735 = ORIENTED_EDGE('',*,*,#17326,.F.) ;
#23736 = ORIENTED_EDGE('',*,*,#17327,.F.) ;
#23737 = ORIENTED_EDGE('',*,*,#17328,.F.) ;
#23738 = ORIENTED_EDGE('',*,*,#17329,.T.) ;
#23739 = ORIENTED_EDGE('',*,*,#17330,.F.) ;
#23740 = ORIENTED_EDGE('',*,*,#17331,.T.) ;
#23741 = ORIENTED_EDGE('',*,*,#17332,.F.) ;
#23742 = ORIENTED_EDGE('',*,*,#17333,.T.) ;
#23743 = ORIENTED_EDGE('',*,*,#17334,.F.) ;
#23744 = ORIENTED_EDGE('',*,*,#17335,.T.) ;
#23745 = ORIENTED_EDGE('',*,*,#17336,.F.) ;
#23746 = ORIENTED_EDGE('',*,*,#17322,.F.) ;
#23747 = ORIENTED_EDGE('',*,*,#17337,.T.) ;
#23748 = ORIENTED_EDGE('',*,*,#17338,.T.) ;
#23749 = ORIENTED_EDGE('',*,*,#17339,.T.) ;
#23750 = ORIENTED_EDGE('',*,*,#17338,.F.) ;
#23751 = ORIENTED_EDGE('',*,*,#17340,.T.) ;
#23752 = ORIENTED_EDGE('',*,*,#17341,.T.) ;
#23753 = ORIENTED_EDGE('',*,*,#17337,.F.) ;
#23754 = ORIENTED_EDGE('',*,*,#17341,.F.) ;
#23755 = ORIENTED_EDGE('',*,*,#17342,.F.) ;
#23756 = ORIENTED_EDGE('',*,*,#17343,.F.) ;
#23757 = ORIENTED_EDGE('',*,*,#17344,.F.) ;
#23758 = ORIENTED_EDGE('',*,*,#17345,.F.) ;
#23759 = ORIENTED_EDGE('',*,*,#17346,.T.) ;
#23760 = ORIENTED_EDGE('',*,*,#17347,.F.) ;
#23761 = ORIENTED_EDGE('',*,*,#17348,.T.) ;
#23762 = ORIENTED_EDGE('',*,*,#17349,.F.) ;
#23763 = ORIENTED_EDGE('',*,*,#17350,.T.) ;
#23764 = ORIENTED_EDGE('',*,*,#17351,.F.) ;
#23765 = ORIENTED_EDGE('',*,*,#17352,.T.) ;
#23766 = ORIENTED_EDGE('',*,*,#17353,.F.) ;
#23767 = ORIENTED_EDGE('',*,*,#17339,.F.) ;
#23768 = ORIENTED_EDGE('',*,*,#17354,.T.) ;
#23769 = ORIENTED_EDGE('',*,*,#17355,.T.) ;
#23770 = ORIENTED_EDGE('',*,*,#17356,.T.) ;
#23771 = ORIENTED_EDGE('',*,*,#17355,.F.) ;
#23772 = ORIENTED_EDGE('',*,*,#17357,.T.) ;
#23773 = ORIENTED_EDGE('',*,*,#17358,.T.) ;
#23774 = ORIENTED_EDGE('',*,*,#17354,.F.) ;
#23775 = ORIENTED_EDGE('',*,*,#17358,.F.) ;
#23776 = ORIENTED_EDGE('',*,*,#17359,.F.) ;
#23777 = ORIENTED_EDGE('',*,*,#17360,.F.) ;
#23778 = ORIENTED_EDGE('',*,*,#17361,.F.) ;
#23779 = ORIENTED_EDGE('',*,*,#17362,.F.) ;
#23780 = ORIENTED_EDGE('',*,*,#17363,.T.) ;
#23781 = ORIENTED_EDGE('',*,*,#17364,.F.) ;
#23782 = ORIENTED_EDGE('',*,*,#17365,.T.) ;
#23783 = ORIENTED_EDGE('',*,*,#17366,.F.) ;
#23784 = ORIENTED_EDGE('',*,*,#17367,.T.) ;
#23785 = ORIENTED_EDGE('',*,*,#17368,.F.) ;
#23786 = ORIENTED_EDGE('',*,*,#17369,.T.) ;
#23787 = ORIENTED_EDGE('',*,*,#17370,.F.) ;
#23788 = ORIENTED_EDGE('',*,*,#17356,.F.) ;
#23789 = ORIENTED_EDGE('',*,*,#17371,.T.) ;
#23790 = ORIENTED_EDGE('',*,*,#17372,.T.) ;
#23791 = ORIENTED_EDGE('',*,*,#17373,.T.) ;
#23792 = ORIENTED_EDGE('',*,*,#17372,.F.) ;
#23793 = ORIENTED_EDGE('',*,*,#17374,.T.) ;
#23794 = ORIENTED_EDGE('',*,*,#17375,.T.) ;
#23795 = ORIENTED_EDGE('',*,*,#17371,.F.) ;
#23796 = ORIENTED_EDGE('',*,*,#17375,.F.) ;
#23797 = ORIENTED_EDGE('',*,*,#17376,.F.) ;
#23798 = ORIENTED_EDGE('',*,*,#17377,.F.) ;
#23799 = ORIENTED_EDGE('',*,*,#17378,.F.) ;
#23800 = ORIENTED_EDGE('',*,*,#17379,.F.) ;
#23801 = ORIENTED_EDGE('',*,*,#17380,.T.) ;
#23802 = ORIENTED_EDGE('',*,*,#17381,.F.) ;
#23803 = ORIENTED_EDGE('',*,*,#17382,.T.) ;
#23804 = ORIENTED_EDGE('',*,*,#17383,.F.) ;
#23805 = ORIENTED_EDGE('',*,*,#17384,.T.) ;
#23806 = ORIENTED_EDGE('',*,*,#17385,.F.) ;
#23807 = ORIENTED_EDGE('',*,*,#17386,.T.) ;
#23808 = ORIENTED_EDGE('',*,*,#17387,.F.) ;
#23809 = ORIENTED_EDGE('',*,*,#17373,.F.) ;
#23810 = ORIENTED_EDGE('',*,*,#17388,.T.) ;
#23811 = ORIENTED_EDGE('',*,*,#17389,.T.) ;
#23812 = ORIENTED_EDGE('',*,*,#17390,.T.) ;
#23813 = ORIENTED_EDGE('',*,*,#17389,.F.) ;
#23814 = ORIENTED_EDGE('',*,*,#17391,.T.) ;
#23815 = ORIENTED_EDGE('',*,*,#17392,.T.) ;
#23816 = ORIENTED_EDGE('',*,*,#17388,.F.) ;
#23817 = ORIENTED_EDGE('',*,*,#17392,.F.) ;
#23818 = ORIENTED_EDGE('',*,*,#17393,.F.) ;
#23819 = ORIENTED_EDGE('',*,*,#17394,.F.) ;
#23820 = ORIENTED_EDGE('',*,*,#17395,.F.) ;
#23821 = ORIENTED_EDGE('',*,*,#17396,.F.) ;
#23822 = ORIENTED_EDGE('',*,*,#17397,.T.) ;
#23823 = ORIENTED_EDGE('',*,*,#17398,.F.) ;
#23824 = ORIENTED_EDGE('',*,*,#17399,.T.) ;
#23825 = ORIENTED_EDGE('',*,*,#17400,.F.) ;
#23826 = ORIENTED_EDGE('',*,*,#17401,.T.) ;
#23827 = ORIENTED_EDGE('',*,*,#17402,.F.) ;
#23828 = ORIENTED_EDGE('',*,*,#17403,.T.) ;
#23829 = ORIENTED_EDGE('',*,*,#17404,.F.) ;
#23830 = ORIENTED_EDGE('',*,*,#17390,.F.) ;
#23831 = ORIENTED_EDGE('',*,*,#17405,.T.) ;
#23832 = ORIENTED_EDGE('',*,*,#17406,.T.) ;
#23833 = ORIENTED_EDGE('',*,*,#17407,.T.) ;
#23834 = ORIENTED_EDGE('',*,*,#17406,.F.) ;
#23835 = ORIENTED_EDGE('',*,*,#17408,.T.) ;
#23836 = ORIENTED_EDGE('',*,*,#17409,.T.) ;
#23837 = ORIENTED_EDGE('',*,*,#17405,.F.) ;
#23838 = ORIENTED_EDGE('',*,*,#17409,.F.) ;
#23839 = ORIENTED_EDGE('',*,*,#17410,.F.) ;
#23840 = ORIENTED_EDGE('',*,*,#17411,.F.) ;
#23841 = ORIENTED_EDGE('',*,*,#17412,.F.) ;
#23842 = ORIENTED_EDGE('',*,*,#17413,.F.) ;
#23843 = ORIENTED_EDGE('',*,*,#17414,.T.) ;
#23844 = ORIENTED_EDGE('',*,*,#17415,.F.) ;
#23845 = ORIENTED_EDGE('',*,*,#17416,.T.) ;
#23846 = ORIENTED_EDGE('',*,*,#17417,.F.) ;
#23847 = ORIENTED_EDGE('',*,*,#17418,.T.) ;
#23848 = ORIENTED_EDGE('',*,*,#17419,.F.) ;
#23849 = ORIENTED_EDGE('',*,*,#17420,.T.) ;
#23850 = ORIENTED_EDGE('',*,*,#17421,.F.) ;
#23851 = ORIENTED_EDGE('',*,*,#17407,.F.) ;
#23852 = ORIENTED_EDGE('',*,*,#17422,.T.) ;
#23853 = ORIENTED_EDGE('',*,*,#17423,.T.) ;
#23854 = ORIENTED_EDGE('',*,*,#17424,.T.) ;
#23855 = ORIENTED_EDGE('',*,*,#17423,.F.) ;
#23856 = ORIENTED_EDGE('',*,*,#17425,.F.) ;
#23857 = ORIENTED_EDGE('',*,*,#17426,.F.) ;
#23858 = ORIENTED_EDGE('',*,*,#17427,.F.) ;
#23859 = ORIENTED_EDGE('',*,*,#17428,.F.) ;
#23860 = ORIENTED_EDGE('',*,*,#17429,.F.) ;
#23861 = ORIENTED_EDGE('',*,*,#17430,.F.) ;
#23862 = ORIENTED_EDGE('',*,*,#17431,.F.) ;
#23863 = ORIENTED_EDGE('',*,*,#17432,.F.) ;
#23864 = ORIENTED_EDGE('',*,*,#17433,.F.) ;
#23865 = ORIENTED_EDGE('',*,*,#17434,.F.) ;
#23866 = ORIENTED_EDGE('',*,*,#17435,.F.) ;
#23867 = ORIENTED_EDGE('',*,*,#17436,.F.) ;
#23868 = ORIENTED_EDGE('',*,*,#17424,.F.) ;
#23869 = ORIENTED_EDGE('',*,*,#17437,.F.) ;
#23870 = ORIENTED_EDGE('',*,*,#17438,.T.) ;
#23871 = ORIENTED_EDGE('',*,*,#17422,.F.) ;
#23872 = ORIENTED_EDGE('',*,*,#17438,.F.) ;
#23873 = ORIENTED_EDGE('',*,*,#17439,.T.) ;
#23874 = ORIENTED_EDGE('',*,*,#17289,.F.) ;
#23875 = ORIENTED_EDGE('',*,*,#17440,.T.) ;
#23876 = ORIENTED_EDGE('',*,*,#17306,.F.) ;
#23877 = ORIENTED_EDGE('',*,*,#17441,.T.) ;
#23878 = ORIENTED_EDGE('',*,*,#17323,.F.) ;
#23879 = ORIENTED_EDGE('',*,*,#17442,.T.) ;
#23880 = ORIENTED_EDGE('',*,*,#17340,.F.) ;
#23881 = ORIENTED_EDGE('',*,*,#17443,.T.) ;
#23882 = ORIENTED_EDGE('',*,*,#17357,.F.) ;
#23883 = ORIENTED_EDGE('',*,*,#17444,.T.) ;
#23884 = ORIENTED_EDGE('',*,*,#17374,.F.) ;
#23885 = ORIENTED_EDGE('',*,*,#17445,.T.) ;
#23886 = ORIENTED_EDGE('',*,*,#17391,.F.) ;
#23887 = ORIENTED_EDGE('',*,*,#17446,.T.) ;
#23888 = ORIENTED_EDGE('',*,*,#17408,.F.) ;
#23889 = ORIENTED_EDGE('',*,*,#17447,.T.) ;
#23890 = ORIENTED_EDGE('',*,*,#17448,.T.) ;
#23891 = ORIENTED_EDGE('',*,*,#17449,.T.) ;
#23892 = ORIENTED_EDGE('',*,*,#17295,.F.) ;
#23893 = ORIENTED_EDGE('',*,*,#17450,.T.) ;
#23894 = ORIENTED_EDGE('',*,*,#17296,.T.) ;
#23895 = ORIENTED_EDGE('',*,*,#17449,.F.) ;
#23896 = ORIENTED_EDGE('',*,*,#17451,.F.) ;
#23897 = ORIENTED_EDGE('',*,*,#17452,.T.) ;
#23898 = ORIENTED_EDGE('',*,*,#17297,.F.) ;
#23899 = ORIENTED_EDGE('',*,*,#17450,.F.) ;
#23900 = ORIENTED_EDGE('',*,*,#17453,.T.) ;
#23901 = ORIENTED_EDGE('',*,*,#17454,.T.) ;
#23902 = ORIENTED_EDGE('',*,*,#17298,.T.) ;
#23903 = ORIENTED_EDGE('',*,*,#17452,.F.) ;
#23904 = ORIENTED_EDGE('',*,*,#17455,.T.) ;
#23905 = ORIENTED_EDGE('',*,*,#17456,.T.) ;
#23906 = ORIENTED_EDGE('',*,*,#17299,.F.) ;
#23907 = ORIENTED_EDGE('',*,*,#17454,.F.) ;
#23908 = ORIENTED_EDGE('',*,*,#17457,.T.) ;
#23909 = ORIENTED_EDGE('',*,*,#17458,.T.) ;
#23910 = ORIENTED_EDGE('',*,*,#17300,.T.) ;
#23911 = ORIENTED_EDGE('',*,*,#17456,.F.) ;
#23912 = ORIENTED_EDGE('',*,*,#17459,.F.) ;
#23913 = ORIENTED_EDGE('',*,*,#17460,.T.) ;
#23914 = ORIENTED_EDGE('',*,*,#17301,.F.) ;
#23915 = ORIENTED_EDGE('',*,*,#17458,.F.) ;
#23916 = ORIENTED_EDGE('',*,*,#17461,.T.) ;
#23917 = ORIENTED_EDGE('',*,*,#17447,.F.) ;
#23918 = ORIENTED_EDGE('',*,*,#17302,.T.) ;
#23919 = ORIENTED_EDGE('',*,*,#17460,.F.) ;
#23920 = ORIENTED_EDGE('',*,*,#17462,.T.) ;
#23921 = ORIENTED_EDGE('',*,*,#17455,.F.) ;
#23922 = ORIENTED_EDGE('',*,*,#17463,.F.) ;
#23923 = ORIENTED_EDGE('',*,*,#17464,.F.) ;
#23924 = ORIENTED_EDGE('',*,*,#17465,.F.) ;
#23925 = ORIENTED_EDGE('',*,*,#17453,.F.) ;
#23926 = ORIENTED_EDGE('',*,*,#17466,.T.) ;
#23927 = ORIENTED_EDGE('',*,*,#17467,.T.) ;
#23928 = ORIENTED_EDGE('',*,*,#17468,.T.) ;
#23929 = ORIENTED_EDGE('',*,*,#17469,.T.) ;
#23930 = ORIENTED_EDGE('',*,*,#17470,.F.) ;
#23931 = ORIENTED_EDGE('',*,*,#17471,.T.) ;
#23932 = ORIENTED_EDGE('',*,*,#17472,.T.) ;
#23933 = ORIENTED_EDGE('',*,*,#17473,.T.) ;
#23934 = ORIENTED_EDGE('',*,*,#17463,.T.) ;
#23935 = ORIENTED_EDGE('',*,*,#17451,.T.) ;
#23936 = ORIENTED_EDGE('',*,*,#17474,.F.) ;
#23937 = ORIENTED_EDGE('',*,*,#17475,.F.) ;
#23938 = ORIENTED_EDGE('',*,*,#17466,.F.) ;
#23939 = ORIENTED_EDGE('',*,*,#17448,.F.) ;
#23940 = ORIENTED_EDGE('',*,*,#17476,.T.) ;
#23941 = ORIENTED_EDGE('',*,*,#17477,.T.) ;
#23942 = ORIENTED_EDGE('',*,*,#17474,.T.) ;
#23943 = ORIENTED_EDGE('',*,*,#17478,.T.) ;
#23944 = ORIENTED_EDGE('',*,*,#17479,.T.) ;
#23945 = ORIENTED_EDGE('',*,*,#17480,.T.) ;
#23946 = ORIENTED_EDGE('',*,*,#17312,.F.) ;
#23947 = ORIENTED_EDGE('',*,*,#17481,.T.) ;
#23948 = ORIENTED_EDGE('',*,*,#17313,.T.) ;
#23949 = ORIENTED_EDGE('',*,*,#17480,.F.) ;
#23950 = ORIENTED_EDGE('',*,*,#17482,.F.) ;
#23951 = ORIENTED_EDGE('',*,*,#17483,.T.) ;
#23952 = ORIENTED_EDGE('',*,*,#17314,.F.) ;
#23953 = ORIENTED_EDGE('',*,*,#17481,.F.) ;
#23954 = ORIENTED_EDGE('',*,*,#17484,.T.) ;
#23955 = ORIENTED_EDGE('',*,*,#17485,.T.) ;
#23956 = ORIENTED_EDGE('',*,*,#17315,.T.) ;
#23957 = ORIENTED_EDGE('',*,*,#17483,.F.) ;
#23958 = ORIENTED_EDGE('',*,*,#17486,.T.) ;
#23959 = ORIENTED_EDGE('',*,*,#17487,.T.) ;
#23960 = ORIENTED_EDGE('',*,*,#17316,.F.) ;
#23961 = ORIENTED_EDGE('',*,*,#17485,.F.) ;
#23962 = ORIENTED_EDGE('',*,*,#17488,.T.) ;
#23963 = ORIENTED_EDGE('',*,*,#17489,.T.) ;
#23964 = ORIENTED_EDGE('',*,*,#17317,.T.) ;
#23965 = ORIENTED_EDGE('',*,*,#17487,.F.) ;
#23966 = ORIENTED_EDGE('',*,*,#17490,.F.) ;
#23967 = ORIENTED_EDGE('',*,*,#17491,.T.) ;
#23968 = ORIENTED_EDGE('',*,*,#17318,.F.) ;
#23969 = ORIENTED_EDGE('',*,*,#17489,.F.) ;
#23970 = ORIENTED_EDGE('',*,*,#17492,.T.) ;
#23971 = ORIENTED_EDGE('',*,*,#17478,.F.) ;
#23972 = ORIENTED_EDGE('',*,*,#17319,.T.) ;
#23973 = ORIENTED_EDGE('',*,*,#17491,.F.) ;
#23974 = ORIENTED_EDGE('',*,*,#17493,.T.) ;
#23975 = ORIENTED_EDGE('',*,*,#17486,.F.) ;
#23976 = ORIENTED_EDGE('',*,*,#17494,.F.) ;
#23977 = ORIENTED_EDGE('',*,*,#17495,.F.) ;
#23978 = ORIENTED_EDGE('',*,*,#17496,.F.) ;
#23979 = ORIENTED_EDGE('',*,*,#17484,.F.) ;
#23980 = ORIENTED_EDGE('',*,*,#17497,.T.) ;
#23981 = ORIENTED_EDGE('',*,*,#17498,.T.) ;
#23982 = ORIENTED_EDGE('',*,*,#17499,.T.) ;
#23983 = ORIENTED_EDGE('',*,*,#17500,.T.) ;
#23984 = ORIENTED_EDGE('',*,*,#17501,.F.) ;
#23985 = ORIENTED_EDGE('',*,*,#17502,.T.) ;
#23986 = ORIENTED_EDGE('',*,*,#17503,.T.) ;
#23987 = ORIENTED_EDGE('',*,*,#17504,.T.) ;
#23988 = ORIENTED_EDGE('',*,*,#17494,.T.) ;
#23989 = ORIENTED_EDGE('',*,*,#17482,.T.) ;
#23990 = ORIENTED_EDGE('',*,*,#17505,.F.) ;
#23991 = ORIENTED_EDGE('',*,*,#17506,.F.) ;
#23992 = ORIENTED_EDGE('',*,*,#17497,.F.) ;
#23993 = ORIENTED_EDGE('',*,*,#17479,.F.) ;
#23994 = ORIENTED_EDGE('',*,*,#17507,.T.) ;
#23995 = ORIENTED_EDGE('',*,*,#17508,.T.) ;
#23996 = ORIENTED_EDGE('',*,*,#17505,.T.) ;
#23997 = ORIENTED_EDGE('',*,*,#17509,.T.) ;
#23998 = ORIENTED_EDGE('',*,*,#17510,.T.) ;
#23999 = ORIENTED_EDGE('',*,*,#17511,.T.) ;
#24000 = ORIENTED_EDGE('',*,*,#17329,.F.) ;
#24001 = ORIENTED_EDGE('',*,*,#17512,.T.) ;
#24002 = ORIENTED_EDGE('',*,*,#17330,.T.) ;
#24003 = ORIENTED_EDGE('',*,*,#17511,.F.) ;
#24004 = ORIENTED_EDGE('',*,*,#17513,.F.) ;
#24005 = ORIENTED_EDGE('',*,*,#17514,.T.) ;
#24006 = ORIENTED_EDGE('',*,*,#17331,.F.) ;
#24007 = ORIENTED_EDGE('',*,*,#17512,.F.) ;
#24008 = ORIENTED_EDGE('',*,*,#17515,.T.) ;
#24009 = ORIENTED_EDGE('',*,*,#17516,.T.) ;
#24010 = ORIENTED_EDGE('',*,*,#17332,.T.) ;
#24011 = ORIENTED_EDGE('',*,*,#17514,.F.) ;
#24012 = ORIENTED_EDGE('',*,*,#17517,.T.) ;
#24013 = ORIENTED_EDGE('',*,*,#17518,.T.) ;
#24014 = ORIENTED_EDGE('',*,*,#17333,.F.) ;
#24015 = ORIENTED_EDGE('',*,*,#17516,.F.) ;
#24016 = ORIENTED_EDGE('',*,*,#17519,.T.) ;
#24017 = ORIENTED_EDGE('',*,*,#17520,.T.) ;
#24018 = ORIENTED_EDGE('',*,*,#17334,.T.) ;
#24019 = ORIENTED_EDGE('',*,*,#17518,.F.) ;
#24020 = ORIENTED_EDGE('',*,*,#17521,.F.) ;
#24021 = ORIENTED_EDGE('',*,*,#17522,.T.) ;
#24022 = ORIENTED_EDGE('',*,*,#17335,.F.) ;
#24023 = ORIENTED_EDGE('',*,*,#17520,.F.) ;
#24024 = ORIENTED_EDGE('',*,*,#17523,.T.) ;
#24025 = ORIENTED_EDGE('',*,*,#17509,.F.) ;
#24026 = ORIENTED_EDGE('',*,*,#17336,.T.) ;
#24027 = ORIENTED_EDGE('',*,*,#17522,.F.) ;
#24028 = ORIENTED_EDGE('',*,*,#17524,.T.) ;
#24029 = ORIENTED_EDGE('',*,*,#17517,.F.) ;
#24030 = ORIENTED_EDGE('',*,*,#17525,.F.) ;
#24031 = ORIENTED_EDGE('',*,*,#17526,.F.) ;
#24032 = ORIENTED_EDGE('',*,*,#17527,.F.) ;
#24033 = ORIENTED_EDGE('',*,*,#17515,.F.) ;
#24034 = ORIENTED_EDGE('',*,*,#17528,.T.) ;
#24035 = ORIENTED_EDGE('',*,*,#17529,.T.) ;
#24036 = ORIENTED_EDGE('',*,*,#17530,.T.) ;
#24037 = ORIENTED_EDGE('',*,*,#17531,.T.) ;
#24038 = ORIENTED_EDGE('',*,*,#17532,.F.) ;
#24039 = ORIENTED_EDGE('',*,*,#17533,.T.) ;
#24040 = ORIENTED_EDGE('',*,*,#17534,.T.) ;
#24041 = ORIENTED_EDGE('',*,*,#17535,.T.) ;
#24042 = ORIENTED_EDGE('',*,*,#17525,.T.) ;
#24043 = ORIENTED_EDGE('',*,*,#17513,.T.) ;
#24044 = ORIENTED_EDGE('',*,*,#17536,.F.) ;
#24045 = ORIENTED_EDGE('',*,*,#17537,.F.) ;
#24046 = ORIENTED_EDGE('',*,*,#17528,.F.) ;
#24047 = ORIENTED_EDGE('',*,*,#17510,.F.) ;
#24048 = ORIENTED_EDGE('',*,*,#17538,.T.) ;
#24049 = ORIENTED_EDGE('',*,*,#17539,.T.) ;
#24050 = ORIENTED_EDGE('',*,*,#17536,.T.) ;
#24051 = ORIENTED_EDGE('',*,*,#17540,.T.) ;
#24052 = ORIENTED_EDGE('',*,*,#17541,.T.) ;
#24053 = ORIENTED_EDGE('',*,*,#17542,.T.) ;
#24054 = ORIENTED_EDGE('',*,*,#17346,.F.) ;
#24055 = ORIENTED_EDGE('',*,*,#17543,.T.) ;
#24056 = ORIENTED_EDGE('',*,*,#17347,.T.) ;
#24057 = ORIENTED_EDGE('',*,*,#17542,.F.) ;
#24058 = ORIENTED_EDGE('',*,*,#17544,.F.) ;
#24059 = ORIENTED_EDGE('',*,*,#17545,.T.) ;
#24060 = ORIENTED_EDGE('',*,*,#17348,.F.) ;
#24061 = ORIENTED_EDGE('',*,*,#17543,.F.) ;
#24062 = ORIENTED_EDGE('',*,*,#17546,.T.) ;
#24063 = ORIENTED_EDGE('',*,*,#17547,.T.) ;
#24064 = ORIENTED_EDGE('',*,*,#17349,.T.) ;
#24065 = ORIENTED_EDGE('',*,*,#17545,.F.) ;
#24066 = ORIENTED_EDGE('',*,*,#17548,.T.) ;
#24067 = ORIENTED_EDGE('',*,*,#17549,.T.) ;
#24068 = ORIENTED_EDGE('',*,*,#17350,.F.) ;
#24069 = ORIENTED_EDGE('',*,*,#17547,.F.) ;
#24070 = ORIENTED_EDGE('',*,*,#17550,.T.) ;
#24071 = ORIENTED_EDGE('',*,*,#17551,.T.) ;
#24072 = ORIENTED_EDGE('',*,*,#17351,.T.) ;
#24073 = ORIENTED_EDGE('',*,*,#17549,.F.) ;
#24074 = ORIENTED_EDGE('',*,*,#17552,.F.) ;
#24075 = ORIENTED_EDGE('',*,*,#17553,.T.) ;
#24076 = ORIENTED_EDGE('',*,*,#17352,.F.) ;
#24077 = ORIENTED_EDGE('',*,*,#17551,.F.) ;
#24078 = ORIENTED_EDGE('',*,*,#17554,.T.) ;
#24079 = ORIENTED_EDGE('',*,*,#17540,.F.) ;
#24080 = ORIENTED_EDGE('',*,*,#17353,.T.) ;
#24081 = ORIENTED_EDGE('',*,*,#17553,.F.) ;
#24082 = ORIENTED_EDGE('',*,*,#17555,.T.) ;
#24083 = ORIENTED_EDGE('',*,*,#17548,.F.) ;
#24084 = ORIENTED_EDGE('',*,*,#17556,.F.) ;
#24085 = ORIENTED_EDGE('',*,*,#17557,.F.) ;
#24086 = ORIENTED_EDGE('',*,*,#17558,.F.) ;
#24087 = ORIENTED_EDGE('',*,*,#17546,.F.) ;
#24088 = ORIENTED_EDGE('',*,*,#17559,.T.) ;
#24089 = ORIENTED_EDGE('',*,*,#17560,.T.) ;
#24090 = ORIENTED_EDGE('',*,*,#17561,.T.) ;
#24091 = ORIENTED_EDGE('',*,*,#17562,.T.) ;
#24092 = ORIENTED_EDGE('',*,*,#17563,.F.) ;
#24093 = ORIENTED_EDGE('',*,*,#17564,.T.) ;
#24094 = ORIENTED_EDGE('',*,*,#17565,.T.) ;
#24095 = ORIENTED_EDGE('',*,*,#17566,.T.) ;
#24096 = ORIENTED_EDGE('',*,*,#17556,.T.) ;
#24097 = ORIENTED_EDGE('',*,*,#17544,.T.) ;
#24098 = ORIENTED_EDGE('',*,*,#17567,.F.) ;
#24099 = ORIENTED_EDGE('',*,*,#17568,.F.) ;
#24100 = ORIENTED_EDGE('',*,*,#17559,.F.) ;
#24101 = ORIENTED_EDGE('',*,*,#17541,.F.) ;
#24102 = ORIENTED_EDGE('',*,*,#17569,.T.) ;
#24103 = ORIENTED_EDGE('',*,*,#17570,.T.) ;
#24104 = ORIENTED_EDGE('',*,*,#17567,.T.) ;
#24105 = ORIENTED_EDGE('',*,*,#17571,.T.) ;
#24106 = ORIENTED_EDGE('',*,*,#17572,.T.) ;
#24107 = ORIENTED_EDGE('',*,*,#17573,.T.) ;
#24108 = ORIENTED_EDGE('',*,*,#17363,.F.) ;
#24109 = ORIENTED_EDGE('',*,*,#17574,.T.) ;
#24110 = ORIENTED_EDGE('',*,*,#17364,.T.) ;
#24111 = ORIENTED_EDGE('',*,*,#17573,.F.) ;
#24112 = ORIENTED_EDGE('',*,*,#17575,.F.) ;
#24113 = ORIENTED_EDGE('',*,*,#17576,.T.) ;
#24114 = ORIENTED_EDGE('',*,*,#17365,.F.) ;
#24115 = ORIENTED_EDGE('',*,*,#17574,.F.) ;
#24116 = ORIENTED_EDGE('',*,*,#17577,.T.) ;
#24117 = ORIENTED_EDGE('',*,*,#17578,.T.) ;
#24118 = ORIENTED_EDGE('',*,*,#17366,.T.) ;
#24119 = ORIENTED_EDGE('',*,*,#17576,.F.) ;
#24120 = ORIENTED_EDGE('',*,*,#17579,.T.) ;
#24121 = ORIENTED_EDGE('',*,*,#17580,.T.) ;
#24122 = ORIENTED_EDGE('',*,*,#17367,.F.) ;
#24123 = ORIENTED_EDGE('',*,*,#17578,.F.) ;
#24124 = ORIENTED_EDGE('',*,*,#17581,.T.) ;
#24125 = ORIENTED_EDGE('',*,*,#17582,.T.) ;
#24126 = ORIENTED_EDGE('',*,*,#17368,.T.) ;
#24127 = ORIENTED_EDGE('',*,*,#17580,.F.) ;
#24128 = ORIENTED_EDGE('',*,*,#17583,.F.) ;
#24129 = ORIENTED_EDGE('',*,*,#17584,.T.) ;
#24130 = ORIENTED_EDGE('',*,*,#17369,.F.) ;
#24131 = ORIENTED_EDGE('',*,*,#17582,.F.) ;
#24132 = ORIENTED_EDGE('',*,*,#17585,.T.) ;
#24133 = ORIENTED_EDGE('',*,*,#17571,.F.) ;
#24134 = ORIENTED_EDGE('',*,*,#17370,.T.) ;
#24135 = ORIENTED_EDGE('',*,*,#17584,.F.) ;
#24136 = ORIENTED_EDGE('',*,*,#17586,.T.) ;
#24137 = ORIENTED_EDGE('',*,*,#17579,.F.) ;
#24138 = ORIENTED_EDGE('',*,*,#17587,.F.) ;
#24139 = ORIENTED_EDGE('',*,*,#17588,.F.) ;
#24140 = ORIENTED_EDGE('',*,*,#17589,.F.) ;
#24141 = ORIENTED_EDGE('',*,*,#17577,.F.) ;
#24142 = ORIENTED_EDGE('',*,*,#17590,.T.) ;
#24143 = ORIENTED_EDGE('',*,*,#17591,.T.) ;
#24144 = ORIENTED_EDGE('',*,*,#17592,.T.) ;
#24145 = ORIENTED_EDGE('',*,*,#17593,.T.) ;
#24146 = ORIENTED_EDGE('',*,*,#17594,.F.) ;
#24147 = ORIENTED_EDGE('',*,*,#17595,.T.) ;
#24148 = ORIENTED_EDGE('',*,*,#17596,.T.) ;
#24149 = ORIENTED_EDGE('',*,*,#17597,.T.) ;
#24150 = ORIENTED_EDGE('',*,*,#17587,.T.) ;
#24151 = ORIENTED_EDGE('',*,*,#17575,.T.) ;
#24152 = ORIENTED_EDGE('',*,*,#17598,.F.) ;
#24153 = ORIENTED_EDGE('',*,*,#17599,.F.) ;
#24154 = ORIENTED_EDGE('',*,*,#17590,.F.) ;
#24155 = ORIENTED_EDGE('',*,*,#17572,.F.) ;
#24156 = ORIENTED_EDGE('',*,*,#17600,.T.) ;
#24157 = ORIENTED_EDGE('',*,*,#17601,.T.) ;
#24158 = ORIENTED_EDGE('',*,*,#17598,.T.) ;
#24159 = ORIENTED_EDGE('',*,*,#17602,.T.) ;
#24160 = ORIENTED_EDGE('',*,*,#17603,.T.) ;
#24161 = ORIENTED_EDGE('',*,*,#17604,.T.) ;
#24162 = ORIENTED_EDGE('',*,*,#17380,.F.) ;
#24163 = ORIENTED_EDGE('',*,*,#17605,.T.) ;
#24164 = ORIENTED_EDGE('',*,*,#17381,.T.) ;
#24165 = ORIENTED_EDGE('',*,*,#17604,.F.) ;
#24166 = ORIENTED_EDGE('',*,*,#17606,.F.) ;
#24167 = ORIENTED_EDGE('',*,*,#17607,.T.) ;
#24168 = ORIENTED_EDGE('',*,*,#17382,.F.) ;
#24169 = ORIENTED_EDGE('',*,*,#17605,.F.) ;
#24170 = ORIENTED_EDGE('',*,*,#17608,.T.) ;
#24171 = ORIENTED_EDGE('',*,*,#17609,.T.) ;
#24172 = ORIENTED_EDGE('',*,*,#17383,.T.) ;
#24173 = ORIENTED_EDGE('',*,*,#17607,.F.) ;
#24174 = ORIENTED_EDGE('',*,*,#17610,.T.) ;
#24175 = ORIENTED_EDGE('',*,*,#17611,.T.) ;
#24176 = ORIENTED_EDGE('',*,*,#17384,.F.) ;
#24177 = ORIENTED_EDGE('',*,*,#17609,.F.) ;
#24178 = ORIENTED_EDGE('',*,*,#17612,.T.) ;
#24179 = ORIENTED_EDGE('',*,*,#17613,.T.) ;
#24180 = ORIENTED_EDGE('',*,*,#17385,.T.) ;
#24181 = ORIENTED_EDGE('',*,*,#17611,.F.) ;
#24182 = ORIENTED_EDGE('',*,*,#17614,.F.) ;
#24183 = ORIENTED_EDGE('',*,*,#17615,.T.) ;
#24184 = ORIENTED_EDGE('',*,*,#17386,.F.) ;
#24185 = ORIENTED_EDGE('',*,*,#17613,.F.) ;
#24186 = ORIENTED_EDGE('',*,*,#17616,.T.) ;
#24187 = ORIENTED_EDGE('',*,*,#17602,.F.) ;
#24188 = ORIENTED_EDGE('',*,*,#17387,.T.) ;
#24189 = ORIENTED_EDGE('',*,*,#17615,.F.) ;
#24190 = ORIENTED_EDGE('',*,*,#17617,.T.) ;
#24191 = ORIENTED_EDGE('',*,*,#17610,.F.) ;
#24192 = ORIENTED_EDGE('',*,*,#17618,.F.) ;
#24193 = ORIENTED_EDGE('',*,*,#17619,.F.) ;
#24194 = ORIENTED_EDGE('',*,*,#17620,.F.) ;
#24195 = ORIENTED_EDGE('',*,*,#17608,.F.) ;
#24196 = ORIENTED_EDGE('',*,*,#17621,.T.) ;
#24197 = ORIENTED_EDGE('',*,*,#17622,.T.) ;
#24198 = ORIENTED_EDGE('',*,*,#17623,.T.) ;
#24199 = ORIENTED_EDGE('',*,*,#17624,.T.) ;
#24200 = ORIENTED_EDGE('',*,*,#17625,.F.) ;
#24201 = ORIENTED_EDGE('',*,*,#17626,.T.) ;
#24202 = ORIENTED_EDGE('',*,*,#17627,.T.) ;
#24203 = ORIENTED_EDGE('',*,*,#17628,.T.) ;
#24204 = ORIENTED_EDGE('',*,*,#17618,.T.) ;
#24205 = ORIENTED_EDGE('',*,*,#17606,.T.) ;
#24206 = ORIENTED_EDGE('',*,*,#17629,.F.) ;
#24207 = ORIENTED_EDGE('',*,*,#17630,.F.) ;
#24208 = ORIENTED_EDGE('',*,*,#17621,.F.) ;
#24209 = ORIENTED_EDGE('',*,*,#17603,.F.) ;
#24210 = ORIENTED_EDGE('',*,*,#17631,.T.) ;
#24211 = ORIENTED_EDGE('',*,*,#17632,.T.) ;
#24212 = ORIENTED_EDGE('',*,*,#17629,.T.) ;
#24213 = ORIENTED_EDGE('',*,*,#17633,.T.) ;
#24214 = ORIENTED_EDGE('',*,*,#17634,.T.) ;
#24215 = ORIENTED_EDGE('',*,*,#17635,.T.) ;
#24216 = ORIENTED_EDGE('',*,*,#17397,.F.) ;
#24217 = ORIENTED_EDGE('',*,*,#17636,.T.) ;
#24218 = ORIENTED_EDGE('',*,*,#17398,.T.) ;
#24219 = ORIENTED_EDGE('',*,*,#17635,.F.) ;
#24220 = ORIENTED_EDGE('',*,*,#17637,.F.) ;
#24221 = ORIENTED_EDGE('',*,*,#17638,.T.) ;
#24222 = ORIENTED_EDGE('',*,*,#17399,.F.) ;
#24223 = ORIENTED_EDGE('',*,*,#17636,.F.) ;
#24224 = ORIENTED_EDGE('',*,*,#17639,.T.) ;
#24225 = ORIENTED_EDGE('',*,*,#17640,.T.) ;
#24226 = ORIENTED_EDGE('',*,*,#17400,.T.) ;
#24227 = ORIENTED_EDGE('',*,*,#17638,.F.) ;
#24228 = ORIENTED_EDGE('',*,*,#17641,.T.) ;
#24229 = ORIENTED_EDGE('',*,*,#17642,.T.) ;
#24230 = ORIENTED_EDGE('',*,*,#17401,.F.) ;
#24231 = ORIENTED_EDGE('',*,*,#17640,.F.) ;
#24232 = ORIENTED_EDGE('',*,*,#17643,.T.) ;
#24233 = ORIENTED_EDGE('',*,*,#17644,.T.) ;
#24234 = ORIENTED_EDGE('',*,*,#17402,.T.) ;
#24235 = ORIENTED_EDGE('',*,*,#17642,.F.) ;
#24236 = ORIENTED_EDGE('',*,*,#17645,.F.) ;
#24237 = ORIENTED_EDGE('',*,*,#17646,.T.) ;
#24238 = ORIENTED_EDGE('',*,*,#17403,.F.) ;
#24239 = ORIENTED_EDGE('',*,*,#17644,.F.) ;
#24240 = ORIENTED_EDGE('',*,*,#17647,.T.) ;
#24241 = ORIENTED_EDGE('',*,*,#17633,.F.) ;
#24242 = ORIENTED_EDGE('',*,*,#17404,.T.) ;
#24243 = ORIENTED_EDGE('',*,*,#17646,.F.) ;
#24244 = ORIENTED_EDGE('',*,*,#17648,.T.) ;
#24245 = ORIENTED_EDGE('',*,*,#17641,.F.) ;
#24246 = ORIENTED_EDGE('',*,*,#17649,.F.) ;
#24247 = ORIENTED_EDGE('',*,*,#17650,.F.) ;
#24248 = ORIENTED_EDGE('',*,*,#17651,.F.) ;
#24249 = ORIENTED_EDGE('',*,*,#17639,.F.) ;
#24250 = ORIENTED_EDGE('',*,*,#17652,.T.) ;
#24251 = ORIENTED_EDGE('',*,*,#17653,.T.) ;
#24252 = ORIENTED_EDGE('',*,*,#17654,.T.) ;
#24253 = ORIENTED_EDGE('',*,*,#17655,.T.) ;
#24254 = ORIENTED_EDGE('',*,*,#17656,.F.) ;
#24255 = ORIENTED_EDGE('',*,*,#17657,.T.) ;
#24256 = ORIENTED_EDGE('',*,*,#17658,.T.) ;
#24257 = ORIENTED_EDGE('',*,*,#17659,.T.) ;
#24258 = ORIENTED_EDGE('',*,*,#17649,.T.) ;
#24259 = ORIENTED_EDGE('',*,*,#17637,.T.) ;
#24260 = ORIENTED_EDGE('',*,*,#17660,.F.) ;
#24261 = ORIENTED_EDGE('',*,*,#17661,.F.) ;
#24262 = ORIENTED_EDGE('',*,*,#17652,.F.) ;
#24263 = ORIENTED_EDGE('',*,*,#17634,.F.) ;
#24264 = ORIENTED_EDGE('',*,*,#17662,.T.) ;
#24265 = ORIENTED_EDGE('',*,*,#17663,.T.) ;
#24266 = ORIENTED_EDGE('',*,*,#17660,.T.) ;
#24267 = ORIENTED_EDGE('',*,*,#17664,.T.) ;
#24268 = ORIENTED_EDGE('',*,*,#17665,.T.) ;
#24269 = ORIENTED_EDGE('',*,*,#17666,.T.) ;
#24270 = ORIENTED_EDGE('',*,*,#17414,.F.) ;
#24271 = ORIENTED_EDGE('',*,*,#17667,.T.) ;
#24272 = ORIENTED_EDGE('',*,*,#17415,.T.) ;
#24273 = ORIENTED_EDGE('',*,*,#17666,.F.) ;
#24274 = ORIENTED_EDGE('',*,*,#17668,.F.) ;
#24275 = ORIENTED_EDGE('',*,*,#17669,.T.) ;
#24276 = ORIENTED_EDGE('',*,*,#17416,.F.) ;
#24277 = ORIENTED_EDGE('',*,*,#17667,.F.) ;
#24278 = ORIENTED_EDGE('',*,*,#17670,.T.) ;
#24279 = ORIENTED_EDGE('',*,*,#17671,.T.) ;
#24280 = ORIENTED_EDGE('',*,*,#17417,.T.) ;
#24281 = ORIENTED_EDGE('',*,*,#17669,.F.) ;
#24282 = ORIENTED_EDGE('',*,*,#17672,.T.) ;
#24283 = ORIENTED_EDGE('',*,*,#17673,.T.) ;
#24284 = ORIENTED_EDGE('',*,*,#17418,.F.) ;
#24285 = ORIENTED_EDGE('',*,*,#17671,.F.) ;
#24286 = ORIENTED_EDGE('',*,*,#17674,.T.) ;
#24287 = ORIENTED_EDGE('',*,*,#17675,.T.) ;
#24288 = ORIENTED_EDGE('',*,*,#17419,.T.) ;
#24289 = ORIENTED_EDGE('',*,*,#17673,.F.) ;
#24290 = ORIENTED_EDGE('',*,*,#17676,.F.) ;
#24291 = ORIENTED_EDGE('',*,*,#17677,.T.) ;
#24292 = ORIENTED_EDGE('',*,*,#17420,.F.) ;
#24293 = ORIENTED_EDGE('',*,*,#17675,.F.) ;
#24294 = ORIENTED_EDGE('',*,*,#17678,.T.) ;
#24295 = ORIENTED_EDGE('',*,*,#17664,.F.) ;
#24296 = ORIENTED_EDGE('',*,*,#17421,.T.) ;
#24297 = ORIENTED_EDGE('',*,*,#17677,.F.) ;
#24298 = ORIENTED_EDGE('',*,*,#17679,.T.) ;
#24299 = ORIENTED_EDGE('',*,*,#17672,.F.) ;
#24300 = ORIENTED_EDGE('',*,*,#17680,.F.) ;
#24301 = ORIENTED_EDGE('',*,*,#17681,.F.) ;
#24302 = ORIENTED_EDGE('',*,*,#17682,.F.) ;
#24303 = ORIENTED_EDGE('',*,*,#17670,.F.) ;
#24304 = ORIENTED_EDGE('',*,*,#17683,.T.) ;
#24305 = ORIENTED_EDGE('',*,*,#17684,.T.) ;
#24306 = ORIENTED_EDGE('',*,*,#17685,.T.) ;
#24307 = ORIENTED_EDGE('',*,*,#17686,.T.) ;
#24308 = ORIENTED_EDGE('',*,*,#17687,.F.) ;
#24309 = ORIENTED_EDGE('',*,*,#17688,.T.) ;
#24310 = ORIENTED_EDGE('',*,*,#17689,.T.) ;
#24311 = ORIENTED_EDGE('',*,*,#17690,.T.) ;
#24312 = ORIENTED_EDGE('',*,*,#17680,.T.) ;
#24313 = ORIENTED_EDGE('',*,*,#17668,.T.) ;
#24314 = ORIENTED_EDGE('',*,*,#17691,.F.) ;
#24315 = ORIENTED_EDGE('',*,*,#17692,.F.) ;
#24316 = ORIENTED_EDGE('',*,*,#17683,.F.) ;
#24317 = ORIENTED_EDGE('',*,*,#17665,.F.) ;
#24318 = ORIENTED_EDGE('',*,*,#17693,.T.) ;
#24319 = ORIENTED_EDGE('',*,*,#17694,.T.) ;
#24320 = ORIENTED_EDGE('',*,*,#17691,.T.) ;
#24321 = ORIENTED_EDGE('',*,*,#17695,.T.) ;
#24322 = ORIENTED_EDGE('',*,*,#17696,.T.) ;
#24323 = ORIENTED_EDGE('',*,*,#17697,.T.) ;
#24324 = ORIENTED_EDGE('',*,*,#17429,.T.) ;
#24325 = ORIENTED_EDGE('',*,*,#17698,.T.) ;
#24326 = ORIENTED_EDGE('',*,*,#17430,.T.) ;
#24327 = ORIENTED_EDGE('',*,*,#17697,.F.) ;
#24328 = ORIENTED_EDGE('',*,*,#17699,.T.) ;
#24329 = ORIENTED_EDGE('',*,*,#17700,.T.) ;
#24330 = ORIENTED_EDGE('',*,*,#17431,.T.) ;
#24331 = ORIENTED_EDGE('',*,*,#17698,.F.) ;
#24332 = ORIENTED_EDGE('',*,*,#17701,.T.) ;
#24333 = ORIENTED_EDGE('',*,*,#17702,.T.) ;
#24334 = ORIENTED_EDGE('',*,*,#17432,.T.) ;
#24335 = ORIENTED_EDGE('',*,*,#17700,.F.) ;
#24336 = ORIENTED_EDGE('',*,*,#17703,.T.) ;
#24337 = ORIENTED_EDGE('',*,*,#17704,.T.) ;
#24338 = ORIENTED_EDGE('',*,*,#17433,.T.) ;
#24339 = ORIENTED_EDGE('',*,*,#17702,.F.) ;
#24340 = ORIENTED_EDGE('',*,*,#17705,.T.) ;
#24341 = ORIENTED_EDGE('',*,*,#17706,.T.) ;
#24342 = ORIENTED_EDGE('',*,*,#17434,.T.) ;
#24343 = ORIENTED_EDGE('',*,*,#17704,.F.) ;
#24344 = ORIENTED_EDGE('',*,*,#17707,.T.) ;
#24345 = ORIENTED_EDGE('',*,*,#17708,.T.) ;
#24346 = ORIENTED_EDGE('',*,*,#17435,.T.) ;
#24347 = ORIENTED_EDGE('',*,*,#17706,.F.) ;
#24348 = ORIENTED_EDGE('',*,*,#17709,.T.) ;
#24349 = ORIENTED_EDGE('',*,*,#17695,.F.) ;
#24350 = ORIENTED_EDGE('',*,*,#17436,.T.) ;
#24351 = ORIENTED_EDGE('',*,*,#17708,.F.) ;
#24352 = ORIENTED_EDGE('',*,*,#17710,.T.) ;
#24353 = ORIENTED_EDGE('',*,*,#17703,.F.) ;
#24354 = ORIENTED_EDGE('',*,*,#17711,.F.) ;
#24355 = ORIENTED_EDGE('',*,*,#17712,.F.) ;
#24356 = ORIENTED_EDGE('',*,*,#17713,.F.) ;
#24357 = ORIENTED_EDGE('',*,*,#17714,.F.) ;
#24358 = ORIENTED_EDGE('',*,*,#17715,.T.) ;
#24359 = ORIENTED_EDGE('',*,*,#17716,.T.) ;
#24360 = ORIENTED_EDGE('',*,*,#17717,.T.) ;
#24361 = ORIENTED_EDGE('',*,*,#17711,.T.) ;
#24362 = ORIENTED_EDGE('',*,*,#17701,.F.) ;
#24363 = ORIENTED_EDGE('',*,*,#17718,.T.) ;
#24364 = ORIENTED_EDGE('',*,*,#17719,.T.) ;
#24365 = ORIENTED_EDGE('',*,*,#17720,.T.) ;
#24366 = ORIENTED_EDGE('',*,*,#17721,.T.) ;
#24367 = ORIENTED_EDGE('',*,*,#17699,.F.) ;
#24368 = ORIENTED_EDGE('',*,*,#17722,.F.) ;
#24369 = ORIENTED_EDGE('',*,*,#17723,.F.) ;
#24370 = ORIENTED_EDGE('',*,*,#17718,.F.) ;
#24371 = ORIENTED_EDGE('',*,*,#17696,.F.) ;
#24372 = ORIENTED_EDGE('',*,*,#17724,.T.) ;
#24373 = ORIENTED_EDGE('',*,*,#17725,.T.) ;
#24374 = ORIENTED_EDGE('',*,*,#17722,.T.) ;
#24375 = ORIENTED_EDGE('',*,*,#17726,.T.) ;
#24376 = ORIENTED_EDGE('',*,*,#17727,.T.) ;
#24377 = ORIENTED_EDGE('',*,*,#17728,.T.) ;
#24378 = ORIENTED_EDGE('',*,*,#17729,.F.) ;
#24379 = ORIENTED_EDGE('',*,*,#17730,.T.) ;
#24380 = ORIENTED_EDGE('',*,*,#17731,.T.) ;
#24381 = ORIENTED_EDGE('',*,*,#17728,.F.) ;
#24382 = ORIENTED_EDGE('',*,*,#17732,.T.) ;
#24383 = ORIENTED_EDGE('',*,*,#17733,.T.) ;
#24384 = ORIENTED_EDGE('',*,*,#17734,.F.) ;
#24385 = ORIENTED_EDGE('',*,*,#17730,.F.) ;
#24386 = ORIENTED_EDGE('',*,*,#17735,.T.) ;
#24387 = ORIENTED_EDGE('',*,*,#17736,.T.) ;
#24388 = ORIENTED_EDGE('',*,*,#17737,.T.) ;
#24389 = ORIENTED_EDGE('',*,*,#17733,.F.) ;
#24390 = ORIENTED_EDGE('',*,*,#17738,.F.) ;
#24391 = ORIENTED_EDGE('',*,*,#17739,.T.) ;
#24392 = ORIENTED_EDGE('',*,*,#17740,.F.) ;
#24393 = ORIENTED_EDGE('',*,*,#17736,.F.) ;
#24394 = ORIENTED_EDGE('',*,*,#17741,.T.) ;
#24395 = ORIENTED_EDGE('',*,*,#17742,.T.) ;
#24396 = ORIENTED_EDGE('',*,*,#17743,.T.) ;
#24397 = ORIENTED_EDGE('',*,*,#17739,.F.) ;
#24398 = ORIENTED_EDGE('',*,*,#17744,.T.) ;
#24399 = ORIENTED_EDGE('',*,*,#17745,.T.) ;
#24400 = ORIENTED_EDGE('',*,*,#17746,.F.) ;
#24401 = ORIENTED_EDGE('',*,*,#17742,.F.) ;
#24402 = ORIENTED_EDGE('',*,*,#17747,.T.) ;
#24403 = ORIENTED_EDGE('',*,*,#17726,.F.) ;
#24404 = ORIENTED_EDGE('',*,*,#17748,.T.) ;
#24405 = ORIENTED_EDGE('',*,*,#17745,.F.) ;
#24406 = ORIENTED_EDGE('',*,*,#17749,.F.) ;
#24407 = ORIENTED_EDGE('',*,*,#17738,.T.) ;
#24408 = ORIENTED_EDGE('',*,*,#17750,.F.) ;
#24409 = ORIENTED_EDGE('',*,*,#17751,.F.) ;
#24410 = ORIENTED_EDGE('',*,*,#17752,.F.) ;
#24411 = ORIENTED_EDGE('',*,*,#17735,.F.) ;
#24412 = ORIENTED_EDGE('',*,*,#17753,.T.) ;
#24413 = ORIENTED_EDGE('',*,*,#17754,.T.) ;
#24414 = ORIENTED_EDGE('',*,*,#17750,.T.) ;
#24415 = ORIENTED_EDGE('',*,*,#17732,.F.) ;
#24416 = ORIENTED_EDGE('',*,*,#17755,.F.) ;
#24417 = ORIENTED_EDGE('',*,*,#17756,.F.) ;
#24418 = ORIENTED_EDGE('',*,*,#17753,.F.) ;
#24419 = ORIENTED_EDGE('',*,*,#17727,.F.) ;
#24420 = ORIENTED_EDGE('',*,*,#17757,.T.) ;
#24421 = ORIENTED_EDGE('',*,*,#17758,.T.) ;
#24422 = ORIENTED_EDGE('',*,*,#17755,.T.) ;
#24423 = ORIENTED_EDGE('',*,*,#17759,.T.) ;
#24424 = ORIENTED_EDGE('',*,*,#17760,.T.) ;
#24425 = ORIENTED_EDGE('',*,*,#17761,.T.) ;
#24426 = ORIENTED_EDGE('',*,*,#17762,.F.) ;
#24427 = ORIENTED_EDGE('',*,*,#17763,.T.) ;
#24428 = ORIENTED_EDGE('',*,*,#17764,.T.) ;
#24429 = ORIENTED_EDGE('',*,*,#17761,.F.) ;
#24430 = ORIENTED_EDGE('',*,*,#17765,.T.) ;
#24431 = ORIENTED_EDGE('',*,*,#17766,.T.) ;
#24432 = ORIENTED_EDGE('',*,*,#17767,.F.) ;
#24433 = ORIENTED_EDGE('',*,*,#17763,.F.) ;
#24434 = ORIENTED_EDGE('',*,*,#17768,.T.) ;
#24435 = ORIENTED_EDGE('',*,*,#17769,.T.) ;
#24436 = ORIENTED_EDGE('',*,*,#17770,.T.) ;
#24437 = ORIENTED_EDGE('',*,*,#17766,.F.) ;
#24438 = ORIENTED_EDGE('',*,*,#17771,.F.) ;
#24439 = ORIENTED_EDGE('',*,*,#17772,.T.) ;
#24440 = ORIENTED_EDGE('',*,*,#17773,.F.) ;
#24441 = ORIENTED_EDGE('',*,*,#17769,.F.) ;
#24442 = ORIENTED_EDGE('',*,*,#17774,.T.) ;
#24443 = ORIENTED_EDGE('',*,*,#17775,.T.) ;
#24444 = ORIENTED_EDGE('',*,*,#17776,.T.) ;
#24445 = ORIENTED_EDGE('',*,*,#17772,.F.) ;
#24446 = ORIENTED_EDGE('',*,*,#17777,.T.) ;
#24447 = ORIENTED_EDGE('',*,*,#17778,.T.) ;
#24448 = ORIENTED_EDGE('',*,*,#17779,.F.) ;
#24449 = ORIENTED_EDGE('',*,*,#17775,.F.) ;
#24450 = ORIENTED_EDGE('',*,*,#17780,.T.) ;
#24451 = ORIENTED_EDGE('',*,*,#17759,.F.) ;
#24452 = ORIENTED_EDGE('',*,*,#17781,.T.) ;
#24453 = ORIENTED_EDGE('',*,*,#17778,.F.) ;
#24454 = ORIENTED_EDGE('',*,*,#17782,.F.) ;
#24455 = ORIENTED_EDGE('',*,*,#17771,.T.) ;
#24456 = ORIENTED_EDGE('',*,*,#17783,.F.) ;
#24457 = ORIENTED_EDGE('',*,*,#17784,.F.) ;
#24458 = ORIENTED_EDGE('',*,*,#17785,.F.) ;
#24459 = ORIENTED_EDGE('',*,*,#17768,.F.) ;
#24460 = ORIENTED_EDGE('',*,*,#17786,.T.) ;
#24461 = ORIENTED_EDGE('',*,*,#17787,.T.) ;
#24462 = ORIENTED_EDGE('',*,*,#17783,.T.) ;
#24463 = ORIENTED_EDGE('',*,*,#17765,.F.) ;
#24464 = ORIENTED_EDGE('',*,*,#17788,.F.) ;
#24465 = ORIENTED_EDGE('',*,*,#17789,.F.) ;
#24466 = ORIENTED_EDGE('',*,*,#17786,.F.) ;
#24467 = ORIENTED_EDGE('',*,*,#17760,.F.) ;
#24468 = ORIENTED_EDGE('',*,*,#17790,.T.) ;
#24469 = ORIENTED_EDGE('',*,*,#17791,.T.) ;
#24470 = ORIENTED_EDGE('',*,*,#17788,.T.) ;
#24471 = ORIENTED_EDGE('',*,*,#17792,.T.) ;
#24472 = ORIENTED_EDGE('',*,*,#17793,.T.) ;
#24473 = ORIENTED_EDGE('',*,*,#17794,.T.) ;
#24474 = ORIENTED_EDGE('',*,*,#17795,.F.) ;
#24475 = ORIENTED_EDGE('',*,*,#17796,.T.) ;
#24476 = ORIENTED_EDGE('',*,*,#17797,.T.) ;
#24477 = ORIENTED_EDGE('',*,*,#17794,.F.) ;
#24478 = ORIENTED_EDGE('',*,*,#17798,.T.) ;
#24479 = ORIENTED_EDGE('',*,*,#17799,.T.) ;
#24480 = ORIENTED_EDGE('',*,*,#17800,.F.) ;
#24481 = ORIENTED_EDGE('',*,*,#17796,.F.) ;
#24482 = ORIENTED_EDGE('',*,*,#17801,.T.) ;
#24483 = ORIENTED_EDGE('',*,*,#17802,.T.) ;
#24484 = ORIENTED_EDGE('',*,*,#17803,.T.) ;
#24485 = ORIENTED_EDGE('',*,*,#17799,.F.) ;
#24486 = ORIENTED_EDGE('',*,*,#17804,.F.) ;
#24487 = ORIENTED_EDGE('',*,*,#17805,.T.) ;
#24488 = ORIENTED_EDGE('',*,*,#17806,.F.) ;
#24489 = ORIENTED_EDGE('',*,*,#17802,.F.) ;
#24490 = ORIENTED_EDGE('',*,*,#17807,.T.) ;
#24491 = ORIENTED_EDGE('',*,*,#17808,.T.) ;
#24492 = ORIENTED_EDGE('',*,*,#17809,.T.) ;
#24493 = ORIENTED_EDGE('',*,*,#17805,.F.) ;
#24494 = ORIENTED_EDGE('',*,*,#17810,.T.) ;
#24495 = ORIENTED_EDGE('',*,*,#17811,.T.) ;
#24496 = ORIENTED_EDGE('',*,*,#17812,.F.) ;
#24497 = ORIENTED_EDGE('',*,*,#17808,.F.) ;
#24498 = ORIENTED_EDGE('',*,*,#17813,.T.) ;
#24499 = ORIENTED_EDGE('',*,*,#17792,.F.) ;
#24500 = ORIENTED_EDGE('',*,*,#17814,.T.) ;
#24501 = ORIENTED_EDGE('',*,*,#17811,.F.) ;
#24502 = ORIENTED_EDGE('',*,*,#17815,.F.) ;
#24503 = ORIENTED_EDGE('',*,*,#17804,.T.) ;
#24504 = ORIENTED_EDGE('',*,*,#17816,.F.) ;
#24505 = ORIENTED_EDGE('',*,*,#17817,.F.) ;
#24506 = ORIENTED_EDGE('',*,*,#17818,.F.) ;
#24507 = ORIENTED_EDGE('',*,*,#17801,.F.) ;
#24508 = ORIENTED_EDGE('',*,*,#17819,.T.) ;
#24509 = ORIENTED_EDGE('',*,*,#17820,.T.) ;
#24510 = ORIENTED_EDGE('',*,*,#17816,.T.) ;
#24511 = ORIENTED_EDGE('',*,*,#17798,.F.) ;
#24512 = ORIENTED_EDGE('',*,*,#17821,.F.) ;
#24513 = ORIENTED_EDGE('',*,*,#17822,.F.) ;
#24514 = ORIENTED_EDGE('',*,*,#17819,.F.) ;
#24515 = ORIENTED_EDGE('',*,*,#17793,.F.) ;
#24516 = ORIENTED_EDGE('',*,*,#17823,.T.) ;
#24517 = ORIENTED_EDGE('',*,*,#17824,.T.) ;
#24518 = ORIENTED_EDGE('',*,*,#17821,.T.) ;
#24519 = ORIENTED_EDGE('',*,*,#17825,.T.) ;
#24520 = ORIENTED_EDGE('',*,*,#17826,.T.) ;
#24521 = ORIENTED_EDGE('',*,*,#17827,.T.) ;
#24522 = ORIENTED_EDGE('',*,*,#17828,.F.) ;
#24523 = ORIENTED_EDGE('',*,*,#17829,.T.) ;
#24524 = ORIENTED_EDGE('',*,*,#17830,.T.) ;
#24525 = ORIENTED_EDGE('',*,*,#17827,.F.) ;
#24526 = ORIENTED_EDGE('',*,*,#17831,.T.) ;
#24527 = ORIENTED_EDGE('',*,*,#17832,.T.) ;
#24528 = ORIENTED_EDGE('',*,*,#17833,.F.) ;
#24529 = ORIENTED_EDGE('',*,*,#17829,.F.) ;
#24530 = ORIENTED_EDGE('',*,*,#17834,.T.) ;
#24531 = ORIENTED_EDGE('',*,*,#17835,.T.) ;
#24532 = ORIENTED_EDGE('',*,*,#17836,.T.) ;
#24533 = ORIENTED_EDGE('',*,*,#17832,.F.) ;
#24534 = ORIENTED_EDGE('',*,*,#17837,.F.) ;
#24535 = ORIENTED_EDGE('',*,*,#17838,.T.) ;
#24536 = ORIENTED_EDGE('',*,*,#17839,.F.) ;
#24537 = ORIENTED_EDGE('',*,*,#17835,.F.) ;
#24538 = ORIENTED_EDGE('',*,*,#17840,.T.) ;
#24539 = ORIENTED_EDGE('',*,*,#17841,.T.) ;
#24540 = ORIENTED_EDGE('',*,*,#17842,.T.) ;
#24541 = ORIENTED_EDGE('',*,*,#17838,.F.) ;
#24542 = ORIENTED_EDGE('',*,*,#17843,.T.) ;
#24543 = ORIENTED_EDGE('',*,*,#17844,.T.) ;
#24544 = ORIENTED_EDGE('',*,*,#17845,.F.) ;
#24545 = ORIENTED_EDGE('',*,*,#17841,.F.) ;
#24546 = ORIENTED_EDGE('',*,*,#17846,.T.) ;
#24547 = ORIENTED_EDGE('',*,*,#17825,.F.) ;
#24548 = ORIENTED_EDGE('',*,*,#17847,.T.) ;
#24549 = ORIENTED_EDGE('',*,*,#17844,.F.) ;
#24550 = ORIENTED_EDGE('',*,*,#17848,.F.) ;
#24551 = ORIENTED_EDGE('',*,*,#17837,.T.) ;
#24552 = ORIENTED_EDGE('',*,*,#17849,.F.) ;
#24553 = ORIENTED_EDGE('',*,*,#17850,.F.) ;
#24554 = ORIENTED_EDGE('',*,*,#17851,.F.) ;
#24555 = ORIENTED_EDGE('',*,*,#17834,.F.) ;
#24556 = ORIENTED_EDGE('',*,*,#17852,.T.) ;
#24557 = ORIENTED_EDGE('',*,*,#17853,.T.) ;
#24558 = ORIENTED_EDGE('',*,*,#17849,.T.) ;
#24559 = ORIENTED_EDGE('',*,*,#17831,.F.) ;
#24560 = ORIENTED_EDGE('',*,*,#17854,.F.) ;
#24561 = ORIENTED_EDGE('',*,*,#17855,.F.) ;
#24562 = ORIENTED_EDGE('',*,*,#17852,.F.) ;
#24563 = ORIENTED_EDGE('',*,*,#17826,.F.) ;
#24564 = ORIENTED_EDGE('',*,*,#17856,.T.) ;
#24565 = ORIENTED_EDGE('',*,*,#17857,.T.) ;
#24566 = ORIENTED_EDGE('',*,*,#17854,.T.) ;
#24567 = ORIENTED_EDGE('',*,*,#17858,.T.) ;
#24568 = ORIENTED_EDGE('',*,*,#17859,.T.) ;
#24569 = ORIENTED_EDGE('',*,*,#17860,.T.) ;
#24570 = ORIENTED_EDGE('',*,*,#17861,.F.) ;
#24571 = ORIENTED_EDGE('',*,*,#17862,.T.) ;
#24572 = ORIENTED_EDGE('',*,*,#17863,.T.) ;
#24573 = ORIENTED_EDGE('',*,*,#17860,.F.) ;
#24574 = ORIENTED_EDGE('',*,*,#17864,.T.) ;
#24575 = ORIENTED_EDGE('',*,*,#17865,.T.) ;
#24576 = ORIENTED_EDGE('',*,*,#17866,.F.) ;
#24577 = ORIENTED_EDGE('',*,*,#17862,.F.) ;
#24578 = ORIENTED_EDGE('',*,*,#17867,.T.) ;
#24579 = ORIENTED_EDGE('',*,*,#17868,.T.) ;
#24580 = ORIENTED_EDGE('',*,*,#17869,.T.) ;
#24581 = ORIENTED_EDGE('',*,*,#17865,.F.) ;
#24582 = ORIENTED_EDGE('',*,*,#17870,.F.) ;
#24583 = ORIENTED_EDGE('',*,*,#17871,.T.) ;
#24584 = ORIENTED_EDGE('',*,*,#17872,.F.) ;
#24585 = ORIENTED_EDGE('',*,*,#17868,.F.) ;
#24586 = ORIENTED_EDGE('',*,*,#17873,.T.) ;
#24587 = ORIENTED_EDGE('',*,*,#17874,.T.) ;
#24588 = ORIENTED_EDGE('',*,*,#17875,.T.) ;
#24589 = ORIENTED_EDGE('',*,*,#17871,.F.) ;
#24590 = ORIENTED_EDGE('',*,*,#17876,.T.) ;
#24591 = ORIENTED_EDGE('',*,*,#17877,.T.) ;
#24592 = ORIENTED_EDGE('',*,*,#17878,.F.) ;
#24593 = ORIENTED_EDGE('',*,*,#17874,.F.) ;
#24594 = ORIENTED_EDGE('',*,*,#17879,.T.) ;
#24595 = ORIENTED_EDGE('',*,*,#17858,.F.) ;
#24596 = ORIENTED_EDGE('',*,*,#17880,.T.) ;
#24597 = ORIENTED_EDGE('',*,*,#17877,.F.) ;
#24598 = ORIENTED_EDGE('',*,*,#17881,.F.) ;
#24599 = ORIENTED_EDGE('',*,*,#17870,.T.) ;
#24600 = ORIENTED_EDGE('',*,*,#17882,.F.) ;
#24601 = ORIENTED_EDGE('',*,*,#17883,.F.) ;
#24602 = ORIENTED_EDGE('',*,*,#17884,.F.) ;
#24603 = ORIENTED_EDGE('',*,*,#17867,.F.) ;
#24604 = ORIENTED_EDGE('',*,*,#17885,.T.) ;
#24605 = ORIENTED_EDGE('',*,*,#17886,.T.) ;
#24606 = ORIENTED_EDGE('',*,*,#17882,.T.) ;
#24607 = ORIENTED_EDGE('',*,*,#17864,.F.) ;
#24608 = ORIENTED_EDGE('',*,*,#17887,.F.) ;
#24609 = ORIENTED_EDGE('',*,*,#17888,.F.) ;
#24610 = ORIENTED_EDGE('',*,*,#17885,.F.) ;
#24611 = ORIENTED_EDGE('',*,*,#17859,.F.) ;
#24612 = ORIENTED_EDGE('',*,*,#17889,.T.) ;
#24613 = ORIENTED_EDGE('',*,*,#17890,.T.) ;
#24614 = ORIENTED_EDGE('',*,*,#17887,.T.) ;
#24615 = ORIENTED_EDGE('',*,*,#17891,.T.) ;
#24616 = ORIENTED_EDGE('',*,*,#17892,.T.) ;
#24617 = ORIENTED_EDGE('',*,*,#17893,.T.) ;
#24618 = ORIENTED_EDGE('',*,*,#17894,.F.) ;
#24619 = ORIENTED_EDGE('',*,*,#17895,.T.) ;
#24620 = ORIENTED_EDGE('',*,*,#17896,.T.) ;
#24621 = ORIENTED_EDGE('',*,*,#17893,.F.) ;
#24622 = ORIENTED_EDGE('',*,*,#17897,.T.) ;
#24623 = ORIENTED_EDGE('',*,*,#17898,.T.) ;
#24624 = ORIENTED_EDGE('',*,*,#17899,.F.) ;
#24625 = ORIENTED_EDGE('',*,*,#17895,.F.) ;
#24626 = ORIENTED_EDGE('',*,*,#17900,.T.) ;
#24627 = ORIENTED_EDGE('',*,*,#17901,.T.) ;
#24628 = ORIENTED_EDGE('',*,*,#17902,.T.) ;
#24629 = ORIENTED_EDGE('',*,*,#17898,.F.) ;
#24630 = ORIENTED_EDGE('',*,*,#17903,.F.) ;
#24631 = ORIENTED_EDGE('',*,*,#17904,.T.) ;
#24632 = ORIENTED_EDGE('',*,*,#17905,.F.) ;
#24633 = ORIENTED_EDGE('',*,*,#17901,.F.) ;
#24634 = ORIENTED_EDGE('',*,*,#17906,.T.) ;
#24635 = ORIENTED_EDGE('',*,*,#17907,.T.) ;
#24636 = ORIENTED_EDGE('',*,*,#17908,.T.) ;
#24637 = ORIENTED_EDGE('',*,*,#17904,.F.) ;
#24638 = ORIENTED_EDGE('',*,*,#17909,.T.) ;
#24639 = ORIENTED_EDGE('',*,*,#17910,.T.) ;
#24640 = ORIENTED_EDGE('',*,*,#17911,.F.) ;
#24641 = ORIENTED_EDGE('',*,*,#17907,.F.) ;
#24642 = ORIENTED_EDGE('',*,*,#17912,.T.) ;
#24643 = ORIENTED_EDGE('',*,*,#17891,.F.) ;
#24644 = ORIENTED_EDGE('',*,*,#17913,.T.) ;
#24645 = ORIENTED_EDGE('',*,*,#17910,.F.) ;
#24646 = ORIENTED_EDGE('',*,*,#17914,.F.) ;
#24647 = ORIENTED_EDGE('',*,*,#17903,.T.) ;
#24648 = ORIENTED_EDGE('',*,*,#17915,.F.) ;
#24649 = ORIENTED_EDGE('',*,*,#17916,.F.) ;
#24650 = ORIENTED_EDGE('',*,*,#17917,.F.) ;
#24651 = ORIENTED_EDGE('',*,*,#17900,.F.) ;
#24652 = ORIENTED_EDGE('',*,*,#17918,.T.) ;
#24653 = ORIENTED_EDGE('',*,*,#17919,.T.) ;
#24654 = ORIENTED_EDGE('',*,*,#17915,.T.) ;
#24655 = ORIENTED_EDGE('',*,*,#17897,.F.) ;
#24656 = ORIENTED_EDGE('',*,*,#17920,.F.) ;
#24657 = ORIENTED_EDGE('',*,*,#17921,.F.) ;
#24658 = ORIENTED_EDGE('',*,*,#17918,.F.) ;
#24659 = ORIENTED_EDGE('',*,*,#17892,.F.) ;
#24660 = ORIENTED_EDGE('',*,*,#17922,.T.) ;
#24661 = ORIENTED_EDGE('',*,*,#17923,.T.) ;
#24662 = ORIENTED_EDGE('',*,*,#17920,.T.) ;
#24663 = ORIENTED_EDGE('',*,*,#17924,.T.) ;
#24664 = ORIENTED_EDGE('',*,*,#17925,.T.) ;
#24665 = ORIENTED_EDGE('',*,*,#17926,.T.) ;
#24666 = ORIENTED_EDGE('',*,*,#17927,.F.) ;
#24667 = ORIENTED_EDGE('',*,*,#17928,.T.) ;
#24668 = ORIENTED_EDGE('',*,*,#17929,.T.) ;
#24669 = ORIENTED_EDGE('',*,*,#17926,.F.) ;
#24670 = ORIENTED_EDGE('',*,*,#17930,.T.) ;
#24671 = ORIENTED_EDGE('',*,*,#17931,.T.) ;
#24672 = ORIENTED_EDGE('',*,*,#17932,.F.) ;
#24673 = ORIENTED_EDGE('',*,*,#17928,.F.) ;
#24674 = ORIENTED_EDGE('',*,*,#17933,.T.) ;
#24675 = ORIENTED_EDGE('',*,*,#17934,.T.) ;
#24676 = ORIENTED_EDGE('',*,*,#17935,.T.) ;
#24677 = ORIENTED_EDGE('',*,*,#17931,.F.) ;
#24678 = ORIENTED_EDGE('',*,*,#17936,.F.) ;
#24679 = ORIENTED_EDGE('',*,*,#17937,.T.) ;
#24680 = ORIENTED_EDGE('',*,*,#17938,.F.) ;
#24681 = ORIENTED_EDGE('',*,*,#17934,.F.) ;
#24682 = ORIENTED_EDGE('',*,*,#17939,.T.) ;
#24683 = ORIENTED_EDGE('',*,*,#17940,.T.) ;
#24684 = ORIENTED_EDGE('',*,*,#17941,.T.) ;
#24685 = ORIENTED_EDGE('',*,*,#17937,.F.) ;
#24686 = ORIENTED_EDGE('',*,*,#17942,.T.) ;
#24687 = ORIENTED_EDGE('',*,*,#17943,.T.) ;
#24688 = ORIENTED_EDGE('',*,*,#17944,.F.) ;
#24689 = ORIENTED_EDGE('',*,*,#17940,.F.) ;
#24690 = ORIENTED_EDGE('',*,*,#17945,.T.) ;
#24691 = ORIENTED_EDGE('',*,*,#17924,.F.) ;
#24692 = ORIENTED_EDGE('',*,*,#17946,.T.) ;
#24693 = ORIENTED_EDGE('',*,*,#17943,.F.) ;
#24694 = ORIENTED_EDGE('',*,*,#17947,.F.) ;
#24695 = ORIENTED_EDGE('',*,*,#17936,.T.) ;
#24696 = ORIENTED_EDGE('',*,*,#17948,.F.) ;
#24697 = ORIENTED_EDGE('',*,*,#17949,.F.) ;
#24698 = ORIENTED_EDGE('',*,*,#17950,.F.) ;
#24699 = ORIENTED_EDGE('',*,*,#17933,.F.) ;
#24700 = ORIENTED_EDGE('',*,*,#17951,.T.) ;
#24701 = ORIENTED_EDGE('',*,*,#17952,.T.) ;
#24702 = ORIENTED_EDGE('',*,*,#17948,.T.) ;
#24703 = ORIENTED_EDGE('',*,*,#17930,.F.) ;
#24704 = ORIENTED_EDGE('',*,*,#17953,.F.) ;
#24705 = ORIENTED_EDGE('',*,*,#17954,.F.) ;
#24706 = ORIENTED_EDGE('',*,*,#17951,.F.) ;
#24707 = ORIENTED_EDGE('',*,*,#17925,.F.) ;
#24708 = ORIENTED_EDGE('',*,*,#17955,.T.) ;
#24709 = ORIENTED_EDGE('',*,*,#17956,.T.) ;
#24710 = ORIENTED_EDGE('',*,*,#17953,.T.) ;
#24711 = ORIENTED_EDGE('',*,*,#17957,.T.) ;
#24712 = ORIENTED_EDGE('',*,*,#17958,.T.) ;
#24713 = ORIENTED_EDGE('',*,*,#17959,.T.) ;
#24714 = ORIENTED_EDGE('',*,*,#17960,.F.) ;
#24715 = ORIENTED_EDGE('',*,*,#17961,.T.) ;
#24716 = ORIENTED_EDGE('',*,*,#17962,.T.) ;
#24717 = ORIENTED_EDGE('',*,*,#17959,.F.) ;
#24718 = ORIENTED_EDGE('',*,*,#17963,.T.) ;
#24719 = ORIENTED_EDGE('',*,*,#17964,.T.) ;
#24720 = ORIENTED_EDGE('',*,*,#17965,.F.) ;
#24721 = ORIENTED_EDGE('',*,*,#17961,.F.) ;
#24722 = ORIENTED_EDGE('',*,*,#17966,.T.) ;
#24723 = ORIENTED_EDGE('',*,*,#17967,.T.) ;
#24724 = ORIENTED_EDGE('',*,*,#17968,.T.) ;
#24725 = ORIENTED_EDGE('',*,*,#17964,.F.) ;
#24726 = ORIENTED_EDGE('',*,*,#17969,.F.) ;
#24727 = ORIENTED_EDGE('',*,*,#17970,.T.) ;
#24728 = ORIENTED_EDGE('',*,*,#17971,.F.) ;
#24729 = ORIENTED_EDGE('',*,*,#17967,.F.) ;
#24730 = ORIENTED_EDGE('',*,*,#17972,.T.) ;
#24731 = ORIENTED_EDGE('',*,*,#17973,.T.) ;
#24732 = ORIENTED_EDGE('',*,*,#17974,.T.) ;
#24733 = ORIENTED_EDGE('',*,*,#17970,.F.) ;
#24734 = ORIENTED_EDGE('',*,*,#17975,.T.) ;
#24735 = ORIENTED_EDGE('',*,*,#17976,.T.) ;
#24736 = ORIENTED_EDGE('',*,*,#17977,.F.) ;
#24737 = ORIENTED_EDGE('',*,*,#17973,.F.) ;
#24738 = ORIENTED_EDGE('',*,*,#17978,.T.) ;
#24739 = ORIENTED_EDGE('',*,*,#17957,.F.) ;
#24740 = ORIENTED_EDGE('',*,*,#17979,.T.) ;
#24741 = ORIENTED_EDGE('',*,*,#17976,.F.) ;
#24742 = ORIENTED_EDGE('',*,*,#17980,.F.) ;
#24743 = ORIENTED_EDGE('',*,*,#17969,.T.) ;
#24744 = ORIENTED_EDGE('',*,*,#17981,.F.) ;
#24745 = ORIENTED_EDGE('',*,*,#17982,.F.) ;
#24746 = ORIENTED_EDGE('',*,*,#17983,.F.) ;
#24747 = ORIENTED_EDGE('',*,*,#17966,.F.) ;
#24748 = ORIENTED_EDGE('',*,*,#17984,.T.) ;
#24749 = ORIENTED_EDGE('',*,*,#17985,.T.) ;
#24750 = ORIENTED_EDGE('',*,*,#17981,.T.) ;
#24751 = ORIENTED_EDGE('',*,*,#17963,.F.) ;
#24752 = ORIENTED_EDGE('',*,*,#17986,.F.) ;
#24753 = ORIENTED_EDGE('',*,*,#17987,.F.) ;
#24754 = ORIENTED_EDGE('',*,*,#17984,.F.) ;
#24755 = ORIENTED_EDGE('',*,*,#17958,.F.) ;
#24756 = ORIENTED_EDGE('',*,*,#17988,.T.) ;
#24757 = ORIENTED_EDGE('',*,*,#17989,.T.) ;
#24758 = ORIENTED_EDGE('',*,*,#17986,.T.) ;
#24759 = ORIENTED_EDGE('',*,*,#17990,.T.) ;
#24760 = ORIENTED_EDGE('',*,*,#17991,.T.) ;
#24761 = ORIENTED_EDGE('',*,*,#17992,.T.) ;
#24762 = ORIENTED_EDGE('',*,*,#17993,.F.) ;
#24763 = ORIENTED_EDGE('',*,*,#17994,.T.) ;
#24764 = ORIENTED_EDGE('',*,*,#17995,.T.) ;
#24765 = ORIENTED_EDGE('',*,*,#17992,.F.) ;
#24766 = ORIENTED_EDGE('',*,*,#17996,.T.) ;
#24767 = ORIENTED_EDGE('',*,*,#17997,.T.) ;
#24768 = ORIENTED_EDGE('',*,*,#17998,.F.) ;
#24769 = ORIENTED_EDGE('',*,*,#17994,.F.) ;
#24770 = ORIENTED_EDGE('',*,*,#17999,.T.) ;
#24771 = ORIENTED_EDGE('',*,*,#18000,.T.) ;
#24772 = ORIENTED_EDGE('',*,*,#18001,.T.) ;
#24773 = ORIENTED_EDGE('',*,*,#17997,.F.) ;
#24774 = ORIENTED_EDGE('',*,*,#18002,.F.) ;
#24775 = ORIENTED_EDGE('',*,*,#18003,.T.) ;
#24776 = ORIENTED_EDGE('',*,*,#18004,.F.) ;
#24777 = ORIENTED_EDGE('',*,*,#18000,.F.) ;
#24778 = ORIENTED_EDGE('',*,*,#18005,.T.) ;
#24779 = ORIENTED_EDGE('',*,*,#18006,.T.) ;
#24780 = ORIENTED_EDGE('',*,*,#18007,.T.) ;
#24781 = ORIENTED_EDGE('',*,*,#18003,.F.) ;
#24782 = ORIENTED_EDGE('',*,*,#18008,.T.) ;
#24783 = ORIENTED_EDGE('',*,*,#18009,.T.) ;
#24784 = ORIENTED_EDGE('',*,*,#18010,.F.) ;
#24785 = ORIENTED_EDGE('',*,*,#18006,.F.) ;
#24786 = ORIENTED_EDGE('',*,*,#17470,.T.) ;
#24787 = ORIENTED_EDGE('',*,*,#17990,.F.) ;
#24788 = ORIENTED_EDGE('',*,*,#18011,.T.) ;
#24789 = ORIENTED_EDGE('',*,*,#18009,.F.) ;
#24790 = ORIENTED_EDGE('',*,*,#18012,.F.) ;
#24791 = ORIENTED_EDGE('',*,*,#18002,.T.) ;
#24792 = ORIENTED_EDGE('',*,*,#18013,.F.) ;
#24793 = ORIENTED_EDGE('',*,*,#18014,.T.) ;
#24794 = ORIENTED_EDGE('',*,*,#18015,.T.) ;
#24795 = ORIENTED_EDGE('',*,*,#17461,.F.) ;
#24796 = ORIENTED_EDGE('',*,*,#18016,.T.) ;
#24797 = ORIENTED_EDGE('',*,*,#18017,.T.) ;
#24798 = ORIENTED_EDGE('',*,*,#18018,.T.) ;
#24799 = ORIENTED_EDGE('',*,*,#18013,.T.) ;
#24800 = ORIENTED_EDGE('',*,*,#17999,.F.) ;
#24801 = ORIENTED_EDGE('',*,*,#18019,.T.) ;
#24802 = ORIENTED_EDGE('',*,*,#18020,.T.) ;
#24803 = ORIENTED_EDGE('',*,*,#18021,.T.) ;
#24804 = ORIENTED_EDGE('',*,*,#18022,.T.) ;
#24805 = ORIENTED_EDGE('',*,*,#17996,.F.) ;
#24806 = ORIENTED_EDGE('',*,*,#18023,.F.) ;
#24807 = ORIENTED_EDGE('',*,*,#18024,.T.) ;
#24808 = ORIENTED_EDGE('',*,*,#18019,.F.) ;
#24809 = ORIENTED_EDGE('',*,*,#17991,.F.) ;
#24810 = ORIENTED_EDGE('',*,*,#18025,.T.) ;
#24811 = ORIENTED_EDGE('',*,*,#18026,.T.) ;
#24812 = ORIENTED_EDGE('',*,*,#18023,.T.) ;
#24813 = ORIENTED_EDGE('',*,*,#18027,.T.) ;
#24814 = ORIENTED_EDGE('',*,*,#18028,.T.) ;
#24815 = ORIENTED_EDGE('',*,*,#18029,.T.) ;
#24816 = ORIENTED_EDGE('',*,*,#18030,.F.) ;
#24817 = ORIENTED_EDGE('',*,*,#18031,.T.) ;
#24818 = ORIENTED_EDGE('',*,*,#18032,.T.) ;
#24819 = ORIENTED_EDGE('',*,*,#18029,.F.) ;
#24820 = ORIENTED_EDGE('',*,*,#18033,.T.) ;
#24821 = ORIENTED_EDGE('',*,*,#18034,.T.) ;
#24822 = ORIENTED_EDGE('',*,*,#18035,.F.) ;
#24823 = ORIENTED_EDGE('',*,*,#18031,.F.) ;
#24824 = ORIENTED_EDGE('',*,*,#18036,.T.) ;
#24825 = ORIENTED_EDGE('',*,*,#18037,.T.) ;
#24826 = ORIENTED_EDGE('',*,*,#18038,.T.) ;
#24827 = ORIENTED_EDGE('',*,*,#18034,.F.) ;
#24828 = ORIENTED_EDGE('',*,*,#18039,.F.) ;
#24829 = ORIENTED_EDGE('',*,*,#18040,.T.) ;
#24830 = ORIENTED_EDGE('',*,*,#18041,.F.) ;
#24831 = ORIENTED_EDGE('',*,*,#18037,.F.) ;
#24832 = ORIENTED_EDGE('',*,*,#18042,.T.) ;
#24833 = ORIENTED_EDGE('',*,*,#18043,.T.) ;
#24834 = ORIENTED_EDGE('',*,*,#18044,.T.) ;
#24835 = ORIENTED_EDGE('',*,*,#18040,.F.) ;
#24836 = ORIENTED_EDGE('',*,*,#18045,.T.) ;
#24837 = ORIENTED_EDGE('',*,*,#18046,.T.) ;
#24838 = ORIENTED_EDGE('',*,*,#18047,.F.) ;
#24839 = ORIENTED_EDGE('',*,*,#18043,.F.) ;
#24840 = ORIENTED_EDGE('',*,*,#17501,.T.) ;
#24841 = ORIENTED_EDGE('',*,*,#18027,.F.) ;
#24842 = ORIENTED_EDGE('',*,*,#18048,.T.) ;
#24843 = ORIENTED_EDGE('',*,*,#18046,.F.) ;
#24844 = ORIENTED_EDGE('',*,*,#18049,.F.) ;
#24845 = ORIENTED_EDGE('',*,*,#18039,.T.) ;
#24846 = ORIENTED_EDGE('',*,*,#18050,.F.) ;
#24847 = ORIENTED_EDGE('',*,*,#18051,.T.) ;
#24848 = ORIENTED_EDGE('',*,*,#18052,.T.) ;
#24849 = ORIENTED_EDGE('',*,*,#17492,.F.) ;
#24850 = ORIENTED_EDGE('',*,*,#18053,.T.) ;
#24851 = ORIENTED_EDGE('',*,*,#18054,.T.) ;
#24852 = ORIENTED_EDGE('',*,*,#18055,.T.) ;
#24853 = ORIENTED_EDGE('',*,*,#18050,.T.) ;
#24854 = ORIENTED_EDGE('',*,*,#18036,.F.) ;
#24855 = ORIENTED_EDGE('',*,*,#18056,.T.) ;
#24856 = ORIENTED_EDGE('',*,*,#18057,.T.) ;
#24857 = ORIENTED_EDGE('',*,*,#18058,.T.) ;
#24858 = ORIENTED_EDGE('',*,*,#18059,.T.) ;
#24859 = ORIENTED_EDGE('',*,*,#18033,.F.) ;
#24860 = ORIENTED_EDGE('',*,*,#18060,.F.) ;
#24861 = ORIENTED_EDGE('',*,*,#18061,.T.) ;
#24862 = ORIENTED_EDGE('',*,*,#18056,.F.) ;
#24863 = ORIENTED_EDGE('',*,*,#18028,.F.) ;
#24864 = ORIENTED_EDGE('',*,*,#18062,.T.) ;
#24865 = ORIENTED_EDGE('',*,*,#18063,.T.) ;
#24866 = ORIENTED_EDGE('',*,*,#18060,.T.) ;
#24867 = ORIENTED_EDGE('',*,*,#18064,.T.) ;
#24868 = ORIENTED_EDGE('',*,*,#18065,.T.) ;
#24869 = ORIENTED_EDGE('',*,*,#18066,.T.) ;
#24870 = ORIENTED_EDGE('',*,*,#18067,.F.) ;
#24871 = ORIENTED_EDGE('',*,*,#18068,.T.) ;
#24872 = ORIENTED_EDGE('',*,*,#18069,.T.) ;
#24873 = ORIENTED_EDGE('',*,*,#18066,.F.) ;
#24874 = ORIENTED_EDGE('',*,*,#18070,.T.) ;
#24875 = ORIENTED_EDGE('',*,*,#18071,.T.) ;
#24876 = ORIENTED_EDGE('',*,*,#18072,.F.) ;
#24877 = ORIENTED_EDGE('',*,*,#18068,.F.) ;
#24878 = ORIENTED_EDGE('',*,*,#18073,.T.) ;
#24879 = ORIENTED_EDGE('',*,*,#18074,.T.) ;
#24880 = ORIENTED_EDGE('',*,*,#18075,.T.) ;
#24881 = ORIENTED_EDGE('',*,*,#18071,.F.) ;
#24882 = ORIENTED_EDGE('',*,*,#18076,.F.) ;
#24883 = ORIENTED_EDGE('',*,*,#18077,.T.) ;
#24884 = ORIENTED_EDGE('',*,*,#18078,.F.) ;
#24885 = ORIENTED_EDGE('',*,*,#18074,.F.) ;
#24886 = ORIENTED_EDGE('',*,*,#18079,.T.) ;
#24887 = ORIENTED_EDGE('',*,*,#18080,.T.) ;
#24888 = ORIENTED_EDGE('',*,*,#18081,.T.) ;
#24889 = ORIENTED_EDGE('',*,*,#18077,.F.) ;
#24890 = ORIENTED_EDGE('',*,*,#18082,.T.) ;
#24891 = ORIENTED_EDGE('',*,*,#18083,.T.) ;
#24892 = ORIENTED_EDGE('',*,*,#18084,.F.) ;
#24893 = ORIENTED_EDGE('',*,*,#18080,.F.) ;
#24894 = ORIENTED_EDGE('',*,*,#17532,.T.) ;
#24895 = ORIENTED_EDGE('',*,*,#18064,.F.) ;
#24896 = ORIENTED_EDGE('',*,*,#18085,.T.) ;
#24897 = ORIENTED_EDGE('',*,*,#18083,.F.) ;
#24898 = ORIENTED_EDGE('',*,*,#18086,.F.) ;
#24899 = ORIENTED_EDGE('',*,*,#18076,.T.) ;
#24900 = ORIENTED_EDGE('',*,*,#18087,.F.) ;
#24901 = ORIENTED_EDGE('',*,*,#18088,.T.) ;
#24902 = ORIENTED_EDGE('',*,*,#18089,.T.) ;
#24903 = ORIENTED_EDGE('',*,*,#17523,.F.) ;
#24904 = ORIENTED_EDGE('',*,*,#18090,.T.) ;
#24905 = ORIENTED_EDGE('',*,*,#18091,.T.) ;
#24906 = ORIENTED_EDGE('',*,*,#18092,.T.) ;
#24907 = ORIENTED_EDGE('',*,*,#18087,.T.) ;
#24908 = ORIENTED_EDGE('',*,*,#18073,.F.) ;
#24909 = ORIENTED_EDGE('',*,*,#18093,.T.) ;
#24910 = ORIENTED_EDGE('',*,*,#18094,.T.) ;
#24911 = ORIENTED_EDGE('',*,*,#18095,.T.) ;
#24912 = ORIENTED_EDGE('',*,*,#18096,.T.) ;
#24913 = ORIENTED_EDGE('',*,*,#18070,.F.) ;
#24914 = ORIENTED_EDGE('',*,*,#18097,.F.) ;
#24915 = ORIENTED_EDGE('',*,*,#18098,.T.) ;
#24916 = ORIENTED_EDGE('',*,*,#18093,.F.) ;
#24917 = ORIENTED_EDGE('',*,*,#18065,.F.) ;
#24918 = ORIENTED_EDGE('',*,*,#18099,.T.) ;
#24919 = ORIENTED_EDGE('',*,*,#18100,.T.) ;
#24920 = ORIENTED_EDGE('',*,*,#18097,.T.) ;
#24921 = ORIENTED_EDGE('',*,*,#18101,.T.) ;
#24922 = ORIENTED_EDGE('',*,*,#18102,.T.) ;
#24923 = ORIENTED_EDGE('',*,*,#18103,.T.) ;
#24924 = ORIENTED_EDGE('',*,*,#18104,.F.) ;
#24925 = ORIENTED_EDGE('',*,*,#18105,.T.) ;
#24926 = ORIENTED_EDGE('',*,*,#18106,.T.) ;
#24927 = ORIENTED_EDGE('',*,*,#18103,.F.) ;
#24928 = ORIENTED_EDGE('',*,*,#18107,.T.) ;
#24929 = ORIENTED_EDGE('',*,*,#18108,.T.) ;
#24930 = ORIENTED_EDGE('',*,*,#18109,.F.) ;
#24931 = ORIENTED_EDGE('',*,*,#18105,.F.) ;
#24932 = ORIENTED_EDGE('',*,*,#18110,.T.) ;
#24933 = ORIENTED_EDGE('',*,*,#18111,.T.) ;
#24934 = ORIENTED_EDGE('',*,*,#18112,.T.) ;
#24935 = ORIENTED_EDGE('',*,*,#18108,.F.) ;
#24936 = ORIENTED_EDGE('',*,*,#18113,.F.) ;
#24937 = ORIENTED_EDGE('',*,*,#18114,.T.) ;
#24938 = ORIENTED_EDGE('',*,*,#18115,.F.) ;
#24939 = ORIENTED_EDGE('',*,*,#18111,.F.) ;
#24940 = ORIENTED_EDGE('',*,*,#18116,.T.) ;
#24941 = ORIENTED_EDGE('',*,*,#18117,.T.) ;
#24942 = ORIENTED_EDGE('',*,*,#18118,.T.) ;
#24943 = ORIENTED_EDGE('',*,*,#18114,.F.) ;
#24944 = ORIENTED_EDGE('',*,*,#18119,.T.) ;
#24945 = ORIENTED_EDGE('',*,*,#18120,.T.) ;
#24946 = ORIENTED_EDGE('',*,*,#18121,.F.) ;
#24947 = ORIENTED_EDGE('',*,*,#18117,.F.) ;
#24948 = ORIENTED_EDGE('',*,*,#17563,.T.) ;
#24949 = ORIENTED_EDGE('',*,*,#18101,.F.) ;
#24950 = ORIENTED_EDGE('',*,*,#18122,.T.) ;
#24951 = ORIENTED_EDGE('',*,*,#18120,.F.) ;
#24952 = ORIENTED_EDGE('',*,*,#18123,.F.) ;
#24953 = ORIENTED_EDGE('',*,*,#18113,.T.) ;
#24954 = ORIENTED_EDGE('',*,*,#18124,.F.) ;
#24955 = ORIENTED_EDGE('',*,*,#18125,.T.) ;
#24956 = ORIENTED_EDGE('',*,*,#18126,.T.) ;
#24957 = ORIENTED_EDGE('',*,*,#17554,.F.) ;
#24958 = ORIENTED_EDGE('',*,*,#18127,.T.) ;
#24959 = ORIENTED_EDGE('',*,*,#18128,.T.) ;
#24960 = ORIENTED_EDGE('',*,*,#18129,.T.) ;
#24961 = ORIENTED_EDGE('',*,*,#18124,.T.) ;
#24962 = ORIENTED_EDGE('',*,*,#18110,.F.) ;
#24963 = ORIENTED_EDGE('',*,*,#18130,.T.) ;
#24964 = ORIENTED_EDGE('',*,*,#18131,.T.) ;
#24965 = ORIENTED_EDGE('',*,*,#18132,.T.) ;
#24966 = ORIENTED_EDGE('',*,*,#18133,.T.) ;
#24967 = ORIENTED_EDGE('',*,*,#18107,.F.) ;
#24968 = ORIENTED_EDGE('',*,*,#18134,.F.) ;
#24969 = ORIENTED_EDGE('',*,*,#18135,.T.) ;
#24970 = ORIENTED_EDGE('',*,*,#18130,.F.) ;
#24971 = ORIENTED_EDGE('',*,*,#18102,.F.) ;
#24972 = ORIENTED_EDGE('',*,*,#18136,.T.) ;
#24973 = ORIENTED_EDGE('',*,*,#18137,.T.) ;
#24974 = ORIENTED_EDGE('',*,*,#18134,.T.) ;
#24975 = ORIENTED_EDGE('',*,*,#18138,.T.) ;
#24976 = ORIENTED_EDGE('',*,*,#18139,.T.) ;
#24977 = ORIENTED_EDGE('',*,*,#18140,.T.) ;
#24978 = ORIENTED_EDGE('',*,*,#18141,.F.) ;
#24979 = ORIENTED_EDGE('',*,*,#18142,.T.) ;
#24980 = ORIENTED_EDGE('',*,*,#18143,.T.) ;
#24981 = ORIENTED_EDGE('',*,*,#18140,.F.) ;
#24982 = ORIENTED_EDGE('',*,*,#18144,.T.) ;
#24983 = ORIENTED_EDGE('',*,*,#18145,.T.) ;
#24984 = ORIENTED_EDGE('',*,*,#18146,.F.) ;
#24985 = ORIENTED_EDGE('',*,*,#18142,.F.) ;
#24986 = ORIENTED_EDGE('',*,*,#18147,.T.) ;
#24987 = ORIENTED_EDGE('',*,*,#18148,.T.) ;
#24988 = ORIENTED_EDGE('',*,*,#18149,.T.) ;
#24989 = ORIENTED_EDGE('',*,*,#18145,.F.) ;
#24990 = ORIENTED_EDGE('',*,*,#18150,.F.) ;
#24991 = ORIENTED_EDGE('',*,*,#18151,.T.) ;
#24992 = ORIENTED_EDGE('',*,*,#18152,.F.) ;
#24993 = ORIENTED_EDGE('',*,*,#18148,.F.) ;
#24994 = ORIENTED_EDGE('',*,*,#18153,.T.) ;
#24995 = ORIENTED_EDGE('',*,*,#18154,.T.) ;
#24996 = ORIENTED_EDGE('',*,*,#18155,.T.) ;
#24997 = ORIENTED_EDGE('',*,*,#18151,.F.) ;
#24998 = ORIENTED_EDGE('',*,*,#18156,.T.) ;
#24999 = ORIENTED_EDGE('',*,*,#18157,.T.) ;
#25000 = ORIENTED_EDGE('',*,*,#18158,.F.) ;
#25001 = ORIENTED_EDGE('',*,*,#18154,.F.) ;
#25002 = ORIENTED_EDGE('',*,*,#17594,.T.) ;
#25003 = ORIENTED_EDGE('',*,*,#18138,.F.) ;
#25004 = ORIENTED_EDGE('',*,*,#18159,.T.) ;
#25005 = ORIENTED_EDGE('',*,*,#18157,.F.) ;
#25006 = ORIENTED_EDGE('',*,*,#18160,.F.) ;
#25007 = ORIENTED_EDGE('',*,*,#18150,.T.) ;
#25008 = ORIENTED_EDGE('',*,*,#18161,.F.) ;
#25009 = ORIENTED_EDGE('',*,*,#18162,.T.) ;
#25010 = ORIENTED_EDGE('',*,*,#18163,.T.) ;
#25011 = ORIENTED_EDGE('',*,*,#17585,.F.) ;
#25012 = ORIENTED_EDGE('',*,*,#18164,.T.) ;
#25013 = ORIENTED_EDGE('',*,*,#18165,.T.) ;
#25014 = ORIENTED_EDGE('',*,*,#18166,.T.) ;
#25015 = ORIENTED_EDGE('',*,*,#18161,.T.) ;
#25016 = ORIENTED_EDGE('',*,*,#18147,.F.) ;
#25017 = ORIENTED_EDGE('',*,*,#18167,.T.) ;
#25018 = ORIENTED_EDGE('',*,*,#18168,.T.) ;
#25019 = ORIENTED_EDGE('',*,*,#18169,.T.) ;
#25020 = ORIENTED_EDGE('',*,*,#18170,.T.) ;
#25021 = ORIENTED_EDGE('',*,*,#18144,.F.) ;
#25022 = ORIENTED_EDGE('',*,*,#18171,.F.) ;
#25023 = ORIENTED_EDGE('',*,*,#18172,.T.) ;
#25024 = ORIENTED_EDGE('',*,*,#18167,.F.) ;
#25025 = ORIENTED_EDGE('',*,*,#18139,.F.) ;
#25026 = ORIENTED_EDGE('',*,*,#18173,.T.) ;
#25027 = ORIENTED_EDGE('',*,*,#18174,.T.) ;
#25028 = ORIENTED_EDGE('',*,*,#18171,.T.) ;
#25029 = ORIENTED_EDGE('',*,*,#18175,.T.) ;
#25030 = ORIENTED_EDGE('',*,*,#18176,.T.) ;
#25031 = ORIENTED_EDGE('',*,*,#18177,.T.) ;
#25032 = ORIENTED_EDGE('',*,*,#18178,.F.) ;
#25033 = ORIENTED_EDGE('',*,*,#18179,.T.) ;
#25034 = ORIENTED_EDGE('',*,*,#18180,.T.) ;
#25035 = ORIENTED_EDGE('',*,*,#18177,.F.) ;
#25036 = ORIENTED_EDGE('',*,*,#18181,.T.) ;
#25037 = ORIENTED_EDGE('',*,*,#18182,.T.) ;
#25038 = ORIENTED_EDGE('',*,*,#18183,.F.) ;
#25039 = ORIENTED_EDGE('',*,*,#18179,.F.) ;
#25040 = ORIENTED_EDGE('',*,*,#18184,.T.) ;
#25041 = ORIENTED_EDGE('',*,*,#18185,.T.) ;
#25042 = ORIENTED_EDGE('',*,*,#18186,.T.) ;
#25043 = ORIENTED_EDGE('',*,*,#18182,.F.) ;
#25044 = ORIENTED_EDGE('',*,*,#18187,.F.) ;
#25045 = ORIENTED_EDGE('',*,*,#18188,.T.) ;
#25046 = ORIENTED_EDGE('',*,*,#18189,.F.) ;
#25047 = ORIENTED_EDGE('',*,*,#18185,.F.) ;
#25048 = ORIENTED_EDGE('',*,*,#18190,.T.) ;
#25049 = ORIENTED_EDGE('',*,*,#18191,.T.) ;
#25050 = ORIENTED_EDGE('',*,*,#18192,.T.) ;
#25051 = ORIENTED_EDGE('',*,*,#18188,.F.) ;
#25052 = ORIENTED_EDGE('',*,*,#18193,.T.) ;
#25053 = ORIENTED_EDGE('',*,*,#18194,.T.) ;
#25054 = ORIENTED_EDGE('',*,*,#18195,.F.) ;
#25055 = ORIENTED_EDGE('',*,*,#18191,.F.) ;
#25056 = ORIENTED_EDGE('',*,*,#17625,.T.) ;
#25057 = ORIENTED_EDGE('',*,*,#18175,.F.) ;
#25058 = ORIENTED_EDGE('',*,*,#18196,.T.) ;
#25059 = ORIENTED_EDGE('',*,*,#18194,.F.) ;
#25060 = ORIENTED_EDGE('',*,*,#18197,.F.) ;
#25061 = ORIENTED_EDGE('',*,*,#18187,.T.) ;
#25062 = ORIENTED_EDGE('',*,*,#18198,.F.) ;
#25063 = ORIENTED_EDGE('',*,*,#18199,.T.) ;
#25064 = ORIENTED_EDGE('',*,*,#18200,.T.) ;
#25065 = ORIENTED_EDGE('',*,*,#17616,.F.) ;
#25066 = ORIENTED_EDGE('',*,*,#18201,.T.) ;
#25067 = ORIENTED_EDGE('',*,*,#18202,.T.) ;
#25068 = ORIENTED_EDGE('',*,*,#18203,.T.) ;
#25069 = ORIENTED_EDGE('',*,*,#18198,.T.) ;
#25070 = ORIENTED_EDGE('',*,*,#18184,.F.) ;
#25071 = ORIENTED_EDGE('',*,*,#18204,.T.) ;
#25072 = ORIENTED_EDGE('',*,*,#18205,.T.) ;
#25073 = ORIENTED_EDGE('',*,*,#18206,.T.) ;
#25074 = ORIENTED_EDGE('',*,*,#18207,.T.) ;
#25075 = ORIENTED_EDGE('',*,*,#18181,.F.) ;
#25076 = ORIENTED_EDGE('',*,*,#18208,.F.) ;
#25077 = ORIENTED_EDGE('',*,*,#18209,.T.) ;
#25078 = ORIENTED_EDGE('',*,*,#18204,.F.) ;
#25079 = ORIENTED_EDGE('',*,*,#18176,.F.) ;
#25080 = ORIENTED_EDGE('',*,*,#18210,.T.) ;
#25081 = ORIENTED_EDGE('',*,*,#18211,.T.) ;
#25082 = ORIENTED_EDGE('',*,*,#18208,.T.) ;
#25083 = ORIENTED_EDGE('',*,*,#18212,.T.) ;
#25084 = ORIENTED_EDGE('',*,*,#18213,.T.) ;
#25085 = ORIENTED_EDGE('',*,*,#18214,.T.) ;
#25086 = ORIENTED_EDGE('',*,*,#18215,.F.) ;
#25087 = ORIENTED_EDGE('',*,*,#18216,.T.) ;
#25088 = ORIENTED_EDGE('',*,*,#18217,.T.) ;
#25089 = ORIENTED_EDGE('',*,*,#18214,.F.) ;
#25090 = ORIENTED_EDGE('',*,*,#18218,.T.) ;
#25091 = ORIENTED_EDGE('',*,*,#18219,.T.) ;
#25092 = ORIENTED_EDGE('',*,*,#18220,.F.) ;
#25093 = ORIENTED_EDGE('',*,*,#18216,.F.) ;
#25094 = ORIENTED_EDGE('',*,*,#18221,.T.) ;
#25095 = ORIENTED_EDGE('',*,*,#18222,.T.) ;
#25096 = ORIENTED_EDGE('',*,*,#18223,.T.) ;
#25097 = ORIENTED_EDGE('',*,*,#18219,.F.) ;
#25098 = ORIENTED_EDGE('',*,*,#18224,.F.) ;
#25099 = ORIENTED_EDGE('',*,*,#18225,.T.) ;
#25100 = ORIENTED_EDGE('',*,*,#18226,.F.) ;
#25101 = ORIENTED_EDGE('',*,*,#18222,.F.) ;
#25102 = ORIENTED_EDGE('',*,*,#18227,.T.) ;
#25103 = ORIENTED_EDGE('',*,*,#18228,.T.) ;
#25104 = ORIENTED_EDGE('',*,*,#18229,.T.) ;
#25105 = ORIENTED_EDGE('',*,*,#18225,.F.) ;
#25106 = ORIENTED_EDGE('',*,*,#18230,.T.) ;
#25107 = ORIENTED_EDGE('',*,*,#18231,.T.) ;
#25108 = ORIENTED_EDGE('',*,*,#18232,.F.) ;
#25109 = ORIENTED_EDGE('',*,*,#18228,.F.) ;
#25110 = ORIENTED_EDGE('',*,*,#17656,.T.) ;
#25111 = ORIENTED_EDGE('',*,*,#18212,.F.) ;
#25112 = ORIENTED_EDGE('',*,*,#18233,.T.) ;
#25113 = ORIENTED_EDGE('',*,*,#18231,.F.) ;
#25114 = ORIENTED_EDGE('',*,*,#18234,.F.) ;
#25115 = ORIENTED_EDGE('',*,*,#18224,.T.) ;
#25116 = ORIENTED_EDGE('',*,*,#18235,.F.) ;
#25117 = ORIENTED_EDGE('',*,*,#18236,.T.) ;
#25118 = ORIENTED_EDGE('',*,*,#18237,.T.) ;
#25119 = ORIENTED_EDGE('',*,*,#17647,.F.) ;
#25120 = ORIENTED_EDGE('',*,*,#18238,.T.) ;
#25121 = ORIENTED_EDGE('',*,*,#18239,.T.) ;
#25122 = ORIENTED_EDGE('',*,*,#18240,.T.) ;
#25123 = ORIENTED_EDGE('',*,*,#18235,.T.) ;
#25124 = ORIENTED_EDGE('',*,*,#18221,.F.) ;
#25125 = ORIENTED_EDGE('',*,*,#18241,.T.) ;
#25126 = ORIENTED_EDGE('',*,*,#18242,.T.) ;
#25127 = ORIENTED_EDGE('',*,*,#18243,.T.) ;
#25128 = ORIENTED_EDGE('',*,*,#18244,.T.) ;
#25129 = ORIENTED_EDGE('',*,*,#18218,.F.) ;
#25130 = ORIENTED_EDGE('',*,*,#18245,.F.) ;
#25131 = ORIENTED_EDGE('',*,*,#18246,.T.) ;
#25132 = ORIENTED_EDGE('',*,*,#18241,.F.) ;
#25133 = ORIENTED_EDGE('',*,*,#18213,.F.) ;
#25134 = ORIENTED_EDGE('',*,*,#18247,.T.) ;
#25135 = ORIENTED_EDGE('',*,*,#18248,.T.) ;
#25136 = ORIENTED_EDGE('',*,*,#18245,.T.) ;
#25137 = ORIENTED_EDGE('',*,*,#18249,.T.) ;
#25138 = ORIENTED_EDGE('',*,*,#18250,.T.) ;
#25139 = ORIENTED_EDGE('',*,*,#18251,.T.) ;
#25140 = ORIENTED_EDGE('',*,*,#18252,.F.) ;
#25141 = ORIENTED_EDGE('',*,*,#18253,.T.) ;
#25142 = ORIENTED_EDGE('',*,*,#18254,.T.) ;
#25143 = ORIENTED_EDGE('',*,*,#18251,.F.) ;
#25144 = ORIENTED_EDGE('',*,*,#18255,.T.) ;
#25145 = ORIENTED_EDGE('',*,*,#18256,.T.) ;
#25146 = ORIENTED_EDGE('',*,*,#18257,.F.) ;
#25147 = ORIENTED_EDGE('',*,*,#18253,.F.) ;
#25148 = ORIENTED_EDGE('',*,*,#18258,.T.) ;
#25149 = ORIENTED_EDGE('',*,*,#18259,.T.) ;
#25150 = ORIENTED_EDGE('',*,*,#18260,.T.) ;
#25151 = ORIENTED_EDGE('',*,*,#18256,.F.) ;
#25152 = ORIENTED_EDGE('',*,*,#18261,.F.) ;
#25153 = ORIENTED_EDGE('',*,*,#18262,.T.) ;
#25154 = ORIENTED_EDGE('',*,*,#18263,.F.) ;
#25155 = ORIENTED_EDGE('',*,*,#18259,.F.) ;
#25156 = ORIENTED_EDGE('',*,*,#18264,.T.) ;
#25157 = ORIENTED_EDGE('',*,*,#18265,.T.) ;
#25158 = ORIENTED_EDGE('',*,*,#18266,.T.) ;
#25159 = ORIENTED_EDGE('',*,*,#18262,.F.) ;
#25160 = ORIENTED_EDGE('',*,*,#18267,.T.) ;
#25161 = ORIENTED_EDGE('',*,*,#18268,.T.) ;
#25162 = ORIENTED_EDGE('',*,*,#18269,.F.) ;
#25163 = ORIENTED_EDGE('',*,*,#18265,.F.) ;
#25164 = ORIENTED_EDGE('',*,*,#17687,.T.) ;
#25165 = ORIENTED_EDGE('',*,*,#18249,.F.) ;
#25166 = ORIENTED_EDGE('',*,*,#18270,.T.) ;
#25167 = ORIENTED_EDGE('',*,*,#18268,.F.) ;
#25168 = ORIENTED_EDGE('',*,*,#18271,.F.) ;
#25169 = ORIENTED_EDGE('',*,*,#18261,.T.) ;
#25170 = ORIENTED_EDGE('',*,*,#18272,.F.) ;
#25171 = ORIENTED_EDGE('',*,*,#18273,.T.) ;
#25172 = ORIENTED_EDGE('',*,*,#18274,.T.) ;
#25173 = ORIENTED_EDGE('',*,*,#17678,.F.) ;
#25174 = ORIENTED_EDGE('',*,*,#18275,.T.) ;
#25175 = ORIENTED_EDGE('',*,*,#18276,.T.) ;
#25176 = ORIENTED_EDGE('',*,*,#18277,.T.) ;
#25177 = ORIENTED_EDGE('',*,*,#18272,.T.) ;
#25178 = ORIENTED_EDGE('',*,*,#18258,.F.) ;
#25179 = ORIENTED_EDGE('',*,*,#18278,.T.) ;
#25180 = ORIENTED_EDGE('',*,*,#18279,.T.) ;
#25181 = ORIENTED_EDGE('',*,*,#18280,.T.) ;
#25182 = ORIENTED_EDGE('',*,*,#18281,.T.) ;
#25183 = ORIENTED_EDGE('',*,*,#18255,.F.) ;
#25184 = ORIENTED_EDGE('',*,*,#18282,.F.) ;
#25185 = ORIENTED_EDGE('',*,*,#18283,.T.) ;
#25186 = ORIENTED_EDGE('',*,*,#18278,.F.) ;
#25187 = ORIENTED_EDGE('',*,*,#18250,.F.) ;
#25188 = ORIENTED_EDGE('',*,*,#18284,.T.) ;
#25189 = ORIENTED_EDGE('',*,*,#18285,.T.) ;
#25190 = ORIENTED_EDGE('',*,*,#18282,.T.) ;
#25191 = ORIENTED_EDGE('',*,*,#18286,.T.) ;
#25192 = ORIENTED_EDGE('',*,*,#18287,.T.) ;
#25193 = ORIENTED_EDGE('',*,*,#18288,.T.) ;
#25194 = ORIENTED_EDGE('',*,*,#18289,.T.) ;
#25195 = ORIENTED_EDGE('',*,*,#18290,.T.) ;
#25196 = ORIENTED_EDGE('',*,*,#18291,.T.) ;
#25197 = ORIENTED_EDGE('',*,*,#18288,.F.) ;
#25198 = ORIENTED_EDGE('',*,*,#18292,.T.) ;
#25199 = ORIENTED_EDGE('',*,*,#18293,.T.) ;
#25200 = ORIENTED_EDGE('',*,*,#18294,.T.) ;
#25201 = ORIENTED_EDGE('',*,*,#18290,.F.) ;
#25202 = ORIENTED_EDGE('',*,*,#18295,.T.) ;
#25203 = ORIENTED_EDGE('',*,*,#18296,.T.) ;
#25204 = ORIENTED_EDGE('',*,*,#18297,.T.) ;
#25205 = ORIENTED_EDGE('',*,*,#18293,.F.) ;
#25206 = ORIENTED_EDGE('',*,*,#18298,.T.) ;
#25207 = ORIENTED_EDGE('',*,*,#18299,.T.) ;
#25208 = ORIENTED_EDGE('',*,*,#18300,.T.) ;
#25209 = ORIENTED_EDGE('',*,*,#18296,.F.) ;
#25210 = ORIENTED_EDGE('',*,*,#18301,.T.) ;
#25211 = ORIENTED_EDGE('',*,*,#18302,.T.) ;
#25212 = ORIENTED_EDGE('',*,*,#18303,.T.) ;
#25213 = ORIENTED_EDGE('',*,*,#18299,.F.) ;
#25214 = ORIENTED_EDGE('',*,*,#18304,.T.) ;
#25215 = ORIENTED_EDGE('',*,*,#18305,.T.) ;
#25216 = ORIENTED_EDGE('',*,*,#18306,.T.) ;
#25217 = ORIENTED_EDGE('',*,*,#18302,.F.) ;
#25218 = ORIENTED_EDGE('',*,*,#18307,.T.) ;
#25219 = ORIENTED_EDGE('',*,*,#18286,.F.) ;
#25220 = ORIENTED_EDGE('',*,*,#18308,.T.) ;
#25221 = ORIENTED_EDGE('',*,*,#18305,.F.) ;
#25222 = ORIENTED_EDGE('',*,*,#18309,.T.) ;
#25223 = ORIENTED_EDGE('',*,*,#18298,.F.) ;
#25224 = ORIENTED_EDGE('',*,*,#18310,.F.) ;
#25225 = ORIENTED_EDGE('',*,*,#18311,.F.) ;
#25226 = ORIENTED_EDGE('',*,*,#18312,.F.) ;
#25227 = ORIENTED_EDGE('',*,*,#18295,.F.) ;
#25228 = ORIENTED_EDGE('',*,*,#18313,.T.) ;
#25229 = ORIENTED_EDGE('',*,*,#18314,.T.) ;
#25230 = ORIENTED_EDGE('',*,*,#18310,.T.) ;
#25231 = ORIENTED_EDGE('',*,*,#18292,.F.) ;
#25232 = ORIENTED_EDGE('',*,*,#18315,.F.) ;
#25233 = ORIENTED_EDGE('',*,*,#18316,.F.) ;
#25234 = ORIENTED_EDGE('',*,*,#18313,.F.) ;
#25235 = ORIENTED_EDGE('',*,*,#18287,.F.) ;
#25236 = ORIENTED_EDGE('',*,*,#18317,.T.) ;
#25237 = ORIENTED_EDGE('',*,*,#18318,.T.) ;
#25238 = ORIENTED_EDGE('',*,*,#18315,.T.) ;
#25239 = ORIENTED_EDGE('',*,*,#18319,.T.) ;
#25240 = ORIENTED_EDGE('',*,*,#18320,.F.) ;
#25241 = ORIENTED_EDGE('',*,*,#18321,.T.) ;
#25242 = ORIENTED_EDGE('',*,*,#18322,.F.) ;
#25243 = ORIENTED_EDGE('',*,*,#18323,.F.) ;
#25244 = ORIENTED_EDGE('',*,*,#18324,.F.) ;
#25245 = ORIENTED_EDGE('',*,*,#18325,.F.) ;
#25246 = ORIENTED_EDGE('',*,*,#18326,.F.) ;
#25247 = ORIENTED_EDGE('',*,*,#18327,.F.) ;
#25248 = ORIENTED_EDGE('',*,*,#18328,.F.) ;
#25249 = ORIENTED_EDGE('',*,*,#18329,.F.) ;
#25250 = ORIENTED_EDGE('',*,*,#18330,.F.) ;
#25251 = ORIENTED_EDGE('',*,*,#18331,.T.) ;
#25252 = ORIENTED_EDGE('',*,*,#18289,.F.) ;
#25253 = ORIENTED_EDGE('',*,*,#18291,.F.) ;
#25254 = ORIENTED_EDGE('',*,*,#18294,.F.) ;
#25255 = ORIENTED_EDGE('',*,*,#18297,.F.) ;
#25256 = ORIENTED_EDGE('',*,*,#18300,.F.) ;
#25257 = ORIENTED_EDGE('',*,*,#18303,.F.) ;
#25258 = ORIENTED_EDGE('',*,*,#18306,.F.) ;
#25259 = ORIENTED_EDGE('',*,*,#18308,.F.) ;
#25260 = ORIENTED_EDGE('',*,*,#18332,.T.) ;
#25261 = ORIENTED_EDGE('',*,*,#18333,.T.) ;
#25262 = ORIENTED_EDGE('',*,*,#18334,.T.) ;
#25263 = ORIENTED_EDGE('',*,*,#18323,.T.) ;
#25264 = ORIENTED_EDGE('',*,*,#18335,.T.) ;
#25265 = ORIENTED_EDGE('',*,*,#18324,.T.) ;
#25266 = ORIENTED_EDGE('',*,*,#18334,.F.) ;
#25267 = ORIENTED_EDGE('',*,*,#18336,.T.) ;
#25268 = ORIENTED_EDGE('',*,*,#18337,.T.) ;
#25269 = ORIENTED_EDGE('',*,*,#18325,.T.) ;
#25270 = ORIENTED_EDGE('',*,*,#18335,.F.) ;
#25271 = ORIENTED_EDGE('',*,*,#18338,.T.) ;
#25272 = ORIENTED_EDGE('',*,*,#18339,.T.) ;
#25273 = ORIENTED_EDGE('',*,*,#18326,.T.) ;
#25274 = ORIENTED_EDGE('',*,*,#18337,.F.) ;
#25275 = ORIENTED_EDGE('',*,*,#18340,.T.) ;
#25276 = ORIENTED_EDGE('',*,*,#18341,.T.) ;
#25277 = ORIENTED_EDGE('',*,*,#18327,.T.) ;
#25278 = ORIENTED_EDGE('',*,*,#18339,.F.) ;
#25279 = ORIENTED_EDGE('',*,*,#18342,.T.) ;
#25280 = ORIENTED_EDGE('',*,*,#18343,.T.) ;
#25281 = ORIENTED_EDGE('',*,*,#18328,.T.) ;
#25282 = ORIENTED_EDGE('',*,*,#18341,.F.) ;
#25283 = ORIENTED_EDGE('',*,*,#18344,.T.) ;
#25284 = ORIENTED_EDGE('',*,*,#18345,.T.) ;
#25285 = ORIENTED_EDGE('',*,*,#18329,.T.) ;
#25286 = ORIENTED_EDGE('',*,*,#18343,.F.) ;
#25287 = ORIENTED_EDGE('',*,*,#17714,.T.) ;
#25288 = ORIENTED_EDGE('',*,*,#18332,.F.) ;
#25289 = ORIENTED_EDGE('',*,*,#18330,.T.) ;
#25290 = ORIENTED_EDGE('',*,*,#18345,.F.) ;
#25291 = ORIENTED_EDGE('',*,*,#18346,.T.) ;
#25292 = ORIENTED_EDGE('',*,*,#18340,.F.) ;
#25293 = ORIENTED_EDGE('',*,*,#18347,.F.) ;
#25294 = ORIENTED_EDGE('',*,*,#18348,.T.) ;
#25295 = ORIENTED_EDGE('',*,*,#18349,.T.) ;
#25296 = ORIENTED_EDGE('',*,*,#18338,.F.) ;
#25297 = ORIENTED_EDGE('',*,*,#18350,.T.) ;
#25298 = ORIENTED_EDGE('',*,*,#18351,.T.) ;
#25299 = ORIENTED_EDGE('',*,*,#18352,.T.) ;
#25300 = ORIENTED_EDGE('',*,*,#18353,.T.) ;
#25301 = ORIENTED_EDGE('',*,*,#17709,.F.) ;
#25302 = ORIENTED_EDGE('',*,*,#18354,.T.) ;
#25303 = ORIENTED_EDGE('',*,*,#18355,.T.) ;
#25304 = ORIENTED_EDGE('',*,*,#18356,.T.) ;
#25305 = ORIENTED_EDGE('',*,*,#18347,.T.) ;
#25306 = ORIENTED_EDGE('',*,*,#18336,.F.) ;
#25307 = ORIENTED_EDGE('',*,*,#18357,.T.) ;
#25308 = ORIENTED_EDGE('',*,*,#18358,.T.) ;
#25309 = ORIENTED_EDGE('',*,*,#18350,.F.) ;
#25310 = ORIENTED_EDGE('',*,*,#18333,.F.) ;
#25311 = ORIENTED_EDGE('',*,*,#18359,.T.) ;
#25312 = ORIENTED_EDGE('',*,*,#18360,.T.) ;
#25313 = ORIENTED_EDGE('',*,*,#18357,.F.) ;
#25314 = ORIENTED_EDGE('',*,*,#18342,.F.) ;
#25315 = ORIENTED_EDGE('',*,*,#18349,.F.) ;
#25316 = ORIENTED_EDGE('',*,*,#18361,.T.) ;
#25317 = ORIENTED_EDGE('',*,*,#18362,.T.) ;
#25318 = ORIENTED_EDGE('',*,*,#18344,.F.) ;
#25319 = ORIENTED_EDGE('',*,*,#18362,.F.) ;
#25320 = ORIENTED_EDGE('',*,*,#18363,.T.) ;
#25321 = ORIENTED_EDGE('',*,*,#17715,.F.) ;
#25322 = ORIENTED_EDGE('',*,*,#18346,.F.) ;
#25323 = ORIENTED_EDGE('',*,*,#17721,.F.) ;
#25324 = ORIENTED_EDGE('',*,*,#18364,.T.) ;
#25325 = ORIENTED_EDGE('',*,*,#18359,.F.) ;
#25326 = ORIENTED_EDGE('',*,*,#18301,.F.) ;
#25327 = ORIENTED_EDGE('',*,*,#18312,.T.) ;
#25328 = ORIENTED_EDGE('',*,*,#18365,.T.) ;
#25329 = ORIENTED_EDGE('',*,*,#18366,.T.) ;
#25330 = ORIENTED_EDGE('',*,*,#18304,.F.) ;
#25331 = ORIENTED_EDGE('',*,*,#18366,.F.) ;
#25332 = ORIENTED_EDGE('',*,*,#18367,.T.) ;
#25333 = ORIENTED_EDGE('',*,*,#18368,.F.) ;
#25334 = ORIENTED_EDGE('',*,*,#18309,.F.) ;
#25335 = ORIENTED_EDGE('',*,*,#18369,.F.) ;
#25336 = ORIENTED_EDGE('',*,*,#18370,.T.) ;
#25337 = ORIENTED_EDGE('',*,*,#18317,.F.) ;
#25338 = ORIENTED_EDGE('',*,*,#18307,.F.) ;
#25339 = ORIENTED_EDGE('',*,*,#18368,.T.) ;
#25340 = ORIENTED_EDGE('',*,*,#18371,.T.) ;
#25341 = ORIENTED_EDGE('',*,*,#18369,.T.) ;
#25342 = ORIENTED_EDGE('',*,*,#18372,.T.) ;
#25343 = ORIENTED_EDGE('',*,*,#17437,.T.) ;
#25344 = ORIENTED_EDGE('',*,*,#17710,.F.) ;
#25345 = ORIENTED_EDGE('',*,*,#18353,.F.) ;
#25346 = ORIENTED_EDGE('',*,*,#18373,.F.) ;
#25347 = ORIENTED_EDGE('',*,*,#17724,.F.) ;
#25348 = ORIENTED_EDGE('',*,*,#18374,.F.) ;
#25349 = ORIENTED_EDGE('',*,*,#18361,.F.) ;
#25350 = ORIENTED_EDGE('',*,*,#18375,.F.) ;
#25351 = ORIENTED_EDGE('',*,*,#18376,.F.) ;
#25352 = ORIENTED_EDGE('',*,*,#18377,.T.) ;
#25353 = ORIENTED_EDGE('',*,*,#18373,.T.) ;
#25354 = ORIENTED_EDGE('',*,*,#18352,.F.) ;
#25355 = ORIENTED_EDGE('',*,*,#18378,.T.) ;
#25356 = ORIENTED_EDGE('',*,*,#18379,.F.) ;
#25357 = ORIENTED_EDGE('',*,*,#18380,.F.) ;
#25358 = ORIENTED_EDGE('',*,*,#18378,.F.) ;
#25359 = ORIENTED_EDGE('',*,*,#18351,.F.) ;
#25360 = ORIENTED_EDGE('',*,*,#18381,.T.) ;
#25361 = ORIENTED_EDGE('',*,*,#18382,.T.) ;
#25362 = ORIENTED_EDGE('',*,*,#17719,.F.) ;
#25363 = ORIENTED_EDGE('',*,*,#17723,.T.) ;
#25364 = ORIENTED_EDGE('',*,*,#18383,.T.) ;
#25365 = ORIENTED_EDGE('',*,*,#18384,.T.) ;
#25366 = ORIENTED_EDGE('',*,*,#18355,.F.) ;
#25367 = ORIENTED_EDGE('',*,*,#18385,.T.) ;
#25368 = ORIENTED_EDGE('',*,*,#17707,.F.) ;
#25369 = ORIENTED_EDGE('',*,*,#18386,.F.) ;
#25370 = ORIENTED_EDGE('',*,*,#18385,.F.) ;
#25371 = ORIENTED_EDGE('',*,*,#18354,.F.) ;
#25372 = ORIENTED_EDGE('',*,*,#18387,.F.) ;
#25373 = ORIENTED_EDGE('',*,*,#18356,.F.) ;
#25374 = ORIENTED_EDGE('',*,*,#18384,.F.) ;
#25375 = ORIENTED_EDGE('',*,*,#18388,.F.) ;
#25376 = ORIENTED_EDGE('',*,*,#18389,.T.) ;
#25377 = ORIENTED_EDGE('',*,*,#17712,.T.) ;
#25378 = ORIENTED_EDGE('',*,*,#17717,.F.) ;
#25379 = ORIENTED_EDGE('',*,*,#18390,.T.) ;
#25380 = ORIENTED_EDGE('',*,*,#18391,.F.) ;
#25381 = ORIENTED_EDGE('',*,*,#18392,.F.) ;
#25382 = ORIENTED_EDGE('',*,*,#18390,.F.) ;
#25383 = ORIENTED_EDGE('',*,*,#17716,.F.) ;
#25384 = ORIENTED_EDGE('',*,*,#18389,.F.) ;
#25385 = ORIENTED_EDGE('',*,*,#18393,.F.) ;
#25386 = ORIENTED_EDGE('',*,*,#18383,.F.) ;
#25387 = ORIENTED_EDGE('',*,*,#18394,.F.) ;
#25388 = ORIENTED_EDGE('',*,*,#18395,.F.) ;
#25389 = ORIENTED_EDGE('',*,*,#17720,.F.) ;
#25390 = ORIENTED_EDGE('',*,*,#18382,.F.) ;
#25391 = ORIENTED_EDGE('',*,*,#18396,.F.) ;
#25392 = ORIENTED_EDGE('',*,*,#18377,.F.) ;
#25393 = ORIENTED_EDGE('',*,*,#18397,.F.) ;
#25394 = ORIENTED_EDGE('',*,*,#18381,.F.) ;
#25395 = ORIENTED_EDGE('',*,*,#17725,.F.) ;
#25396 = ORIENTED_EDGE('',*,*,#18391,.T.) ;
#25397 = ORIENTED_EDGE('',*,*,#18363,.F.) ;
#25398 = ORIENTED_EDGE('',*,*,#18374,.T.) ;
#25399 = ORIENTED_EDGE('',*,*,#18375,.T.) ;
#25400 = ORIENTED_EDGE('',*,*,#18348,.F.) ;
#25401 = ORIENTED_EDGE('',*,*,#18387,.T.) ;
#25402 = ORIENTED_EDGE('',*,*,#18398,.F.) ;
#25403 = ORIENTED_EDGE('',*,*,#18399,.F.) ;
#25404 = ORIENTED_EDGE('',*,*,#18400,.F.) ;
#25405 = ORIENTED_EDGE('',*,*,#18360,.F.) ;
#25406 = ORIENTED_EDGE('',*,*,#18398,.T.) ;
#25407 = ORIENTED_EDGE('',*,*,#18364,.F.) ;
#25408 = ORIENTED_EDGE('',*,*,#18395,.T.) ;
#25409 = ORIENTED_EDGE('',*,*,#18379,.T.) ;
#25410 = ORIENTED_EDGE('',*,*,#18358,.F.) ;
#25411 = ORIENTED_EDGE('',*,*,#18400,.T.) ;
#25412 = ORIENTED_EDGE('',*,*,#17705,.F.) ;
#25413 = ORIENTED_EDGE('',*,*,#17713,.T.) ;
#25414 = ORIENTED_EDGE('',*,*,#18394,.T.) ;
#25415 = ORIENTED_EDGE('',*,*,#18386,.T.) ;
#25416 = ORIENTED_EDGE('',*,*,#18376,.T.) ;
#25417 = ORIENTED_EDGE('',*,*,#18388,.T.) ;
#25418 = ORIENTED_EDGE('',*,*,#18393,.T.) ;
#25419 = ORIENTED_EDGE('',*,*,#18392,.T.) ;
#25420 = ORIENTED_EDGE('',*,*,#18396,.T.) ;
#25421 = ORIENTED_EDGE('',*,*,#18397,.T.) ;
#25422 = ORIENTED_EDGE('',*,*,#18380,.T.) ;
#25423 = ORIENTED_EDGE('',*,*,#18399,.T.) ;
#25424 = ORIENTED_EDGE('',*,*,#18401,.T.) ;
#25425 = ORIENTED_EDGE('',*,*,#18402,.T.) ;
#25426 = ORIENTED_EDGE('',*,*,#18403,.T.) ;
#25427 = ORIENTED_EDGE('',*,*,#18404,.T.) ;
#25428 = ORIENTED_EDGE('',*,*,#18405,.T.) ;
#25429 = ORIENTED_EDGE('',*,*,#18406,.T.) ;
#25430 = ORIENTED_EDGE('',*,*,#18367,.F.) ;
#25431 = ORIENTED_EDGE('',*,*,#18407,.T.) ;
#25432 = ORIENTED_EDGE('',*,*,#18408,.T.) ;
#25433 = ORIENTED_EDGE('',*,*,#18370,.F.) ;
#25434 = ORIENTED_EDGE('',*,*,#18371,.F.) ;
#25435 = ORIENTED_EDGE('',*,*,#18406,.F.) ;
#25436 = ORIENTED_EDGE('',*,*,#18401,.F.) ;
#25437 = ORIENTED_EDGE('',*,*,#18407,.F.) ;
#25438 = ORIENTED_EDGE('',*,*,#18408,.F.) ;
#25439 = ORIENTED_EDGE('',*,*,#18404,.F.) ;
#25440 = ORIENTED_EDGE('',*,*,#18409,.F.) ;
#25441 = ORIENTED_EDGE('',*,*,#18318,.F.) ;
#25442 = ORIENTED_EDGE('',*,*,#18405,.F.) ;
#25443 = ORIENTED_EDGE('',*,*,#18365,.F.) ;
#25444 = ORIENTED_EDGE('',*,*,#18410,.F.) ;
#25445 = ORIENTED_EDGE('',*,*,#18402,.F.) ;
#25446 = ORIENTED_EDGE('',*,*,#18403,.F.) ;
#25447 = ORIENTED_EDGE('',*,*,#18411,.F.) ;
#25448 = ORIENTED_EDGE('',*,*,#18314,.F.) ;
#25449 = ORIENTED_EDGE('',*,*,#18412,.F.) ;
#25450 = ORIENTED_EDGE('',*,*,#18410,.T.) ;
#25451 = ORIENTED_EDGE('',*,*,#18311,.T.) ;
#25452 = ORIENTED_EDGE('',*,*,#18411,.T.) ;
#25453 = ORIENTED_EDGE('',*,*,#18316,.T.) ;
#25454 = ORIENTED_EDGE('',*,*,#18409,.T.) ;
#25455 = ORIENTED_EDGE('',*,*,#18412,.T.) ;
#25456 = ORIENTED_EDGE('',*,*,#17679,.F.) ;
#25457 = ORIENTED_EDGE('',*,*,#18281,.F.) ;
#25458 = ORIENTED_EDGE('',*,*,#18413,.F.) ;
#25459 = ORIENTED_EDGE('',*,*,#17693,.F.) ;
#25460 = ORIENTED_EDGE('',*,*,#18414,.F.) ;
#25461 = ORIENTED_EDGE('',*,*,#18415,.F.) ;
#25462 = ORIENTED_EDGE('',*,*,#18416,.F.) ;
#25463 = ORIENTED_EDGE('',*,*,#18417,.F.) ;
#25464 = ORIENTED_EDGE('',*,*,#18418,.T.) ;
#25465 = ORIENTED_EDGE('',*,*,#18413,.T.) ;
#25466 = ORIENTED_EDGE('',*,*,#18280,.F.) ;
#25467 = ORIENTED_EDGE('',*,*,#18419,.T.) ;
#25468 = ORIENTED_EDGE('',*,*,#18420,.F.) ;
#25469 = ORIENTED_EDGE('',*,*,#18421,.F.) ;
#25470 = ORIENTED_EDGE('',*,*,#18419,.F.) ;
#25471 = ORIENTED_EDGE('',*,*,#18279,.F.) ;
#25472 = ORIENTED_EDGE('',*,*,#18422,.T.) ;
#25473 = ORIENTED_EDGE('',*,*,#18423,.T.) ;
#25474 = ORIENTED_EDGE('',*,*,#17684,.F.) ;
#25475 = ORIENTED_EDGE('',*,*,#17692,.T.) ;
#25476 = ORIENTED_EDGE('',*,*,#18424,.T.) ;
#25477 = ORIENTED_EDGE('',*,*,#18425,.T.) ;
#25478 = ORIENTED_EDGE('',*,*,#18276,.F.) ;
#25479 = ORIENTED_EDGE('',*,*,#18426,.T.) ;
#25480 = ORIENTED_EDGE('',*,*,#17676,.T.) ;
#25481 = ORIENTED_EDGE('',*,*,#18427,.F.) ;
#25482 = ORIENTED_EDGE('',*,*,#18426,.F.) ;
#25483 = ORIENTED_EDGE('',*,*,#18275,.F.) ;
#25484 = ORIENTED_EDGE('',*,*,#18428,.F.) ;
#25485 = ORIENTED_EDGE('',*,*,#18277,.F.) ;
#25486 = ORIENTED_EDGE('',*,*,#18425,.F.) ;
#25487 = ORIENTED_EDGE('',*,*,#18429,.F.) ;
#25488 = ORIENTED_EDGE('',*,*,#18430,.T.) ;
#25489 = ORIENTED_EDGE('',*,*,#17681,.T.) ;
#25490 = ORIENTED_EDGE('',*,*,#17690,.F.) ;
#25491 = ORIENTED_EDGE('',*,*,#18431,.T.) ;
#25492 = ORIENTED_EDGE('',*,*,#18432,.F.) ;
#25493 = ORIENTED_EDGE('',*,*,#18433,.F.) ;
#25494 = ORIENTED_EDGE('',*,*,#18431,.F.) ;
#25495 = ORIENTED_EDGE('',*,*,#17689,.F.) ;
#25496 = ORIENTED_EDGE('',*,*,#18430,.F.) ;
#25497 = ORIENTED_EDGE('',*,*,#18434,.F.) ;
#25498 = ORIENTED_EDGE('',*,*,#18424,.F.) ;
#25499 = ORIENTED_EDGE('',*,*,#18435,.F.) ;
#25500 = ORIENTED_EDGE('',*,*,#18436,.F.) ;
#25501 = ORIENTED_EDGE('',*,*,#17685,.F.) ;
#25502 = ORIENTED_EDGE('',*,*,#18423,.F.) ;
#25503 = ORIENTED_EDGE('',*,*,#18437,.F.) ;
#25504 = ORIENTED_EDGE('',*,*,#18418,.F.) ;
#25505 = ORIENTED_EDGE('',*,*,#18438,.F.) ;
#25506 = ORIENTED_EDGE('',*,*,#18422,.F.) ;
#25507 = ORIENTED_EDGE('',*,*,#17694,.F.) ;
#25508 = ORIENTED_EDGE('',*,*,#18432,.T.) ;
#25509 = ORIENTED_EDGE('',*,*,#18439,.F.) ;
#25510 = ORIENTED_EDGE('',*,*,#18414,.T.) ;
#25511 = ORIENTED_EDGE('',*,*,#18416,.T.) ;
#25512 = ORIENTED_EDGE('',*,*,#18273,.F.) ;
#25513 = ORIENTED_EDGE('',*,*,#18428,.T.) ;
#25514 = ORIENTED_EDGE('',*,*,#18440,.F.) ;
#25515 = ORIENTED_EDGE('',*,*,#18441,.F.) ;
#25516 = ORIENTED_EDGE('',*,*,#18442,.F.) ;
#25517 = ORIENTED_EDGE('',*,*,#18285,.F.) ;
#25518 = ORIENTED_EDGE('',*,*,#18440,.T.) ;
#25519 = ORIENTED_EDGE('',*,*,#18443,.F.) ;
#25520 = ORIENTED_EDGE('',*,*,#18436,.T.) ;
#25521 = ORIENTED_EDGE('',*,*,#18420,.T.) ;
#25522 = ORIENTED_EDGE('',*,*,#18283,.F.) ;
#25523 = ORIENTED_EDGE('',*,*,#18442,.T.) ;
#25524 = ORIENTED_EDGE('',*,*,#17674,.F.) ;
#25525 = ORIENTED_EDGE('',*,*,#17682,.T.) ;
#25526 = ORIENTED_EDGE('',*,*,#18435,.T.) ;
#25527 = ORIENTED_EDGE('',*,*,#18427,.T.) ;
#25528 = ORIENTED_EDGE('',*,*,#18417,.T.) ;
#25529 = ORIENTED_EDGE('',*,*,#18429,.T.) ;
#25530 = ORIENTED_EDGE('',*,*,#18434,.T.) ;
#25531 = ORIENTED_EDGE('',*,*,#18433,.T.) ;
#25532 = ORIENTED_EDGE('',*,*,#18437,.T.) ;
#25533 = ORIENTED_EDGE('',*,*,#18438,.T.) ;
#25534 = ORIENTED_EDGE('',*,*,#18421,.T.) ;
#25535 = ORIENTED_EDGE('',*,*,#18441,.T.) ;
#25536 = ORIENTED_EDGE('',*,*,#18444,.T.) ;
#25537 = ORIENTED_EDGE('',*,*,#18445,.T.) ;
#25538 = ORIENTED_EDGE('',*,*,#18446,.T.) ;
#25539 = ORIENTED_EDGE('',*,*,#18447,.T.) ;
#25540 = ORIENTED_EDGE('',*,*,#18448,.T.) ;
#25541 = ORIENTED_EDGE('',*,*,#18449,.T.) ;
#25542 = ORIENTED_EDGE('',*,*,#18450,.F.) ;
#25543 = ORIENTED_EDGE('',*,*,#18451,.T.) ;
#25544 = ORIENTED_EDGE('',*,*,#18452,.T.) ;
#25545 = ORIENTED_EDGE('',*,*,#18453,.F.) ;
#25546 = ORIENTED_EDGE('',*,*,#18454,.F.) ;
#25547 = ORIENTED_EDGE('',*,*,#18449,.F.) ;
#25548 = ORIENTED_EDGE('',*,*,#18444,.F.) ;
#25549 = ORIENTED_EDGE('',*,*,#18451,.F.) ;
#25550 = ORIENTED_EDGE('',*,*,#18452,.F.) ;
#25551 = ORIENTED_EDGE('',*,*,#18447,.F.) ;
#25552 = ORIENTED_EDGE('',*,*,#18455,.F.) ;
#25553 = ORIENTED_EDGE('',*,*,#17989,.F.) ;
#25554 = ORIENTED_EDGE('',*,*,#18448,.F.) ;
#25555 = ORIENTED_EDGE('',*,*,#18456,.F.) ;
#25556 = ORIENTED_EDGE('',*,*,#18457,.F.) ;
#25557 = ORIENTED_EDGE('',*,*,#18445,.F.) ;
#25558 = ORIENTED_EDGE('',*,*,#18446,.F.) ;
#25559 = ORIENTED_EDGE('',*,*,#18458,.F.) ;
#25560 = ORIENTED_EDGE('',*,*,#17985,.F.) ;
#25561 = ORIENTED_EDGE('',*,*,#18459,.F.) ;
#25562 = ORIENTED_EDGE('',*,*,#18457,.T.) ;
#25563 = ORIENTED_EDGE('',*,*,#17982,.T.) ;
#25564 = ORIENTED_EDGE('',*,*,#18458,.T.) ;
#25565 = ORIENTED_EDGE('',*,*,#17987,.T.) ;
#25566 = ORIENTED_EDGE('',*,*,#18455,.T.) ;
#25567 = ORIENTED_EDGE('',*,*,#18459,.T.) ;
#25568 = ORIENTED_EDGE('',*,*,#17648,.F.) ;
#25569 = ORIENTED_EDGE('',*,*,#18244,.F.) ;
#25570 = ORIENTED_EDGE('',*,*,#18460,.F.) ;
#25571 = ORIENTED_EDGE('',*,*,#17662,.F.) ;
#25572 = ORIENTED_EDGE('',*,*,#18461,.F.) ;
#25573 = ORIENTED_EDGE('',*,*,#18462,.F.) ;
#25574 = ORIENTED_EDGE('',*,*,#18463,.F.) ;
#25575 = ORIENTED_EDGE('',*,*,#18464,.F.) ;
#25576 = ORIENTED_EDGE('',*,*,#18465,.T.) ;
#25577 = ORIENTED_EDGE('',*,*,#18460,.T.) ;
#25578 = ORIENTED_EDGE('',*,*,#18243,.F.) ;
#25579 = ORIENTED_EDGE('',*,*,#18466,.T.) ;
#25580 = ORIENTED_EDGE('',*,*,#18467,.F.) ;
#25581 = ORIENTED_EDGE('',*,*,#18468,.F.) ;
#25582 = ORIENTED_EDGE('',*,*,#18466,.F.) ;
#25583 = ORIENTED_EDGE('',*,*,#18242,.F.) ;
#25584 = ORIENTED_EDGE('',*,*,#18469,.T.) ;
#25585 = ORIENTED_EDGE('',*,*,#18470,.T.) ;
#25586 = ORIENTED_EDGE('',*,*,#17653,.F.) ;
#25587 = ORIENTED_EDGE('',*,*,#17661,.T.) ;
#25588 = ORIENTED_EDGE('',*,*,#18471,.T.) ;
#25589 = ORIENTED_EDGE('',*,*,#18472,.T.) ;
#25590 = ORIENTED_EDGE('',*,*,#18239,.F.) ;
#25591 = ORIENTED_EDGE('',*,*,#18473,.T.) ;
#25592 = ORIENTED_EDGE('',*,*,#17645,.T.) ;
#25593 = ORIENTED_EDGE('',*,*,#18474,.F.) ;
#25594 = ORIENTED_EDGE('',*,*,#18473,.F.) ;
#25595 = ORIENTED_EDGE('',*,*,#18238,.F.) ;
#25596 = ORIENTED_EDGE('',*,*,#18475,.F.) ;
#25597 = ORIENTED_EDGE('',*,*,#18240,.F.) ;
#25598 = ORIENTED_EDGE('',*,*,#18472,.F.) ;
#25599 = ORIENTED_EDGE('',*,*,#18476,.F.) ;
#25600 = ORIENTED_EDGE('',*,*,#18477,.T.) ;
#25601 = ORIENTED_EDGE('',*,*,#17650,.T.) ;
#25602 = ORIENTED_EDGE('',*,*,#17659,.F.) ;
#25603 = ORIENTED_EDGE('',*,*,#18478,.T.) ;
#25604 = ORIENTED_EDGE('',*,*,#18479,.F.) ;
#25605 = ORIENTED_EDGE('',*,*,#18480,.F.) ;
#25606 = ORIENTED_EDGE('',*,*,#18478,.F.) ;
#25607 = ORIENTED_EDGE('',*,*,#17658,.F.) ;
#25608 = ORIENTED_EDGE('',*,*,#18477,.F.) ;
#25609 = ORIENTED_EDGE('',*,*,#18481,.F.) ;
#25610 = ORIENTED_EDGE('',*,*,#18471,.F.) ;
#25611 = ORIENTED_EDGE('',*,*,#18482,.F.) ;
#25612 = ORIENTED_EDGE('',*,*,#18483,.F.) ;
#25613 = ORIENTED_EDGE('',*,*,#17654,.F.) ;
#25614 = ORIENTED_EDGE('',*,*,#18470,.F.) ;
#25615 = ORIENTED_EDGE('',*,*,#18484,.F.) ;
#25616 = ORIENTED_EDGE('',*,*,#18465,.F.) ;
#25617 = ORIENTED_EDGE('',*,*,#18485,.F.) ;
#25618 = ORIENTED_EDGE('',*,*,#18469,.F.) ;
#25619 = ORIENTED_EDGE('',*,*,#17663,.F.) ;
#25620 = ORIENTED_EDGE('',*,*,#18479,.T.) ;
#25621 = ORIENTED_EDGE('',*,*,#18486,.F.) ;
#25622 = ORIENTED_EDGE('',*,*,#18461,.T.) ;
#25623 = ORIENTED_EDGE('',*,*,#18463,.T.) ;
#25624 = ORIENTED_EDGE('',*,*,#18236,.F.) ;
#25625 = ORIENTED_EDGE('',*,*,#18475,.T.) ;
#25626 = ORIENTED_EDGE('',*,*,#18487,.F.) ;
#25627 = ORIENTED_EDGE('',*,*,#18488,.F.) ;
#25628 = ORIENTED_EDGE('',*,*,#18489,.F.) ;
#25629 = ORIENTED_EDGE('',*,*,#18248,.F.) ;
#25630 = ORIENTED_EDGE('',*,*,#18487,.T.) ;
#25631 = ORIENTED_EDGE('',*,*,#18490,.F.) ;
#25632 = ORIENTED_EDGE('',*,*,#18483,.T.) ;
#25633 = ORIENTED_EDGE('',*,*,#18467,.T.) ;
#25634 = ORIENTED_EDGE('',*,*,#18246,.F.) ;
#25635 = ORIENTED_EDGE('',*,*,#18489,.T.) ;
#25636 = ORIENTED_EDGE('',*,*,#17643,.F.) ;
#25637 = ORIENTED_EDGE('',*,*,#17651,.T.) ;
#25638 = ORIENTED_EDGE('',*,*,#18482,.T.) ;
#25639 = ORIENTED_EDGE('',*,*,#18474,.T.) ;
#25640 = ORIENTED_EDGE('',*,*,#18464,.T.) ;
#25641 = ORIENTED_EDGE('',*,*,#18476,.T.) ;
#25642 = ORIENTED_EDGE('',*,*,#18481,.T.) ;
#25643 = ORIENTED_EDGE('',*,*,#18480,.T.) ;
#25644 = ORIENTED_EDGE('',*,*,#18484,.T.) ;
#25645 = ORIENTED_EDGE('',*,*,#18485,.T.) ;
#25646 = ORIENTED_EDGE('',*,*,#18468,.T.) ;
#25647 = ORIENTED_EDGE('',*,*,#18488,.T.) ;
#25648 = ORIENTED_EDGE('',*,*,#18491,.T.) ;
#25649 = ORIENTED_EDGE('',*,*,#18492,.T.) ;
#25650 = ORIENTED_EDGE('',*,*,#18493,.T.) ;
#25651 = ORIENTED_EDGE('',*,*,#18494,.T.) ;
#25652 = ORIENTED_EDGE('',*,*,#18495,.T.) ;
#25653 = ORIENTED_EDGE('',*,*,#18496,.T.) ;
#25654 = ORIENTED_EDGE('',*,*,#18497,.F.) ;
#25655 = ORIENTED_EDGE('',*,*,#18498,.T.) ;
#25656 = ORIENTED_EDGE('',*,*,#18499,.T.) ;
#25657 = ORIENTED_EDGE('',*,*,#18500,.F.) ;
#25658 = ORIENTED_EDGE('',*,*,#18501,.F.) ;
#25659 = ORIENTED_EDGE('',*,*,#18496,.F.) ;
#25660 = ORIENTED_EDGE('',*,*,#18491,.F.) ;
#25661 = ORIENTED_EDGE('',*,*,#18498,.F.) ;
#25662 = ORIENTED_EDGE('',*,*,#18499,.F.) ;
#25663 = ORIENTED_EDGE('',*,*,#18494,.F.) ;
#25664 = ORIENTED_EDGE('',*,*,#18502,.F.) ;
#25665 = ORIENTED_EDGE('',*,*,#17956,.F.) ;
#25666 = ORIENTED_EDGE('',*,*,#18495,.F.) ;
#25667 = ORIENTED_EDGE('',*,*,#18503,.F.) ;
#25668 = ORIENTED_EDGE('',*,*,#18504,.F.) ;
#25669 = ORIENTED_EDGE('',*,*,#18492,.F.) ;
#25670 = ORIENTED_EDGE('',*,*,#18493,.F.) ;
#25671 = ORIENTED_EDGE('',*,*,#18505,.F.) ;
#25672 = ORIENTED_EDGE('',*,*,#17952,.F.) ;
#25673 = ORIENTED_EDGE('',*,*,#18506,.F.) ;
#25674 = ORIENTED_EDGE('',*,*,#18504,.T.) ;
#25675 = ORIENTED_EDGE('',*,*,#17949,.T.) ;
#25676 = ORIENTED_EDGE('',*,*,#18505,.T.) ;
#25677 = ORIENTED_EDGE('',*,*,#17954,.T.) ;
#25678 = ORIENTED_EDGE('',*,*,#18502,.T.) ;
#25679 = ORIENTED_EDGE('',*,*,#18506,.T.) ;
#25680 = ORIENTED_EDGE('',*,*,#17617,.F.) ;
#25681 = ORIENTED_EDGE('',*,*,#18207,.F.) ;
#25682 = ORIENTED_EDGE('',*,*,#18507,.F.) ;
#25683 = ORIENTED_EDGE('',*,*,#17631,.F.) ;
#25684 = ORIENTED_EDGE('',*,*,#18508,.F.) ;
#25685 = ORIENTED_EDGE('',*,*,#18509,.F.) ;
#25686 = ORIENTED_EDGE('',*,*,#18510,.F.) ;
#25687 = ORIENTED_EDGE('',*,*,#18511,.F.) ;
#25688 = ORIENTED_EDGE('',*,*,#18512,.T.) ;
#25689 = ORIENTED_EDGE('',*,*,#18507,.T.) ;
#25690 = ORIENTED_EDGE('',*,*,#18206,.F.) ;
#25691 = ORIENTED_EDGE('',*,*,#18513,.T.) ;
#25692 = ORIENTED_EDGE('',*,*,#18514,.F.) ;
#25693 = ORIENTED_EDGE('',*,*,#18515,.F.) ;
#25694 = ORIENTED_EDGE('',*,*,#18513,.F.) ;
#25695 = ORIENTED_EDGE('',*,*,#18205,.F.) ;
#25696 = ORIENTED_EDGE('',*,*,#18516,.T.) ;
#25697 = ORIENTED_EDGE('',*,*,#18517,.T.) ;
#25698 = ORIENTED_EDGE('',*,*,#17622,.F.) ;
#25699 = ORIENTED_EDGE('',*,*,#17630,.T.) ;
#25700 = ORIENTED_EDGE('',*,*,#18518,.T.) ;
#25701 = ORIENTED_EDGE('',*,*,#18519,.T.) ;
#25702 = ORIENTED_EDGE('',*,*,#18202,.F.) ;
#25703 = ORIENTED_EDGE('',*,*,#18520,.T.) ;
#25704 = ORIENTED_EDGE('',*,*,#17614,.T.) ;
#25705 = ORIENTED_EDGE('',*,*,#18521,.F.) ;
#25706 = ORIENTED_EDGE('',*,*,#18520,.F.) ;
#25707 = ORIENTED_EDGE('',*,*,#18201,.F.) ;
#25708 = ORIENTED_EDGE('',*,*,#18522,.F.) ;
#25709 = ORIENTED_EDGE('',*,*,#18203,.F.) ;
#25710 = ORIENTED_EDGE('',*,*,#18519,.F.) ;
#25711 = ORIENTED_EDGE('',*,*,#18523,.F.) ;
#25712 = ORIENTED_EDGE('',*,*,#18524,.T.) ;
#25713 = ORIENTED_EDGE('',*,*,#17619,.T.) ;
#25714 = ORIENTED_EDGE('',*,*,#17628,.F.) ;
#25715 = ORIENTED_EDGE('',*,*,#18525,.T.) ;
#25716 = ORIENTED_EDGE('',*,*,#18526,.F.) ;
#25717 = ORIENTED_EDGE('',*,*,#18527,.F.) ;
#25718 = ORIENTED_EDGE('',*,*,#18525,.F.) ;
#25719 = ORIENTED_EDGE('',*,*,#17627,.F.) ;
#25720 = ORIENTED_EDGE('',*,*,#18524,.F.) ;
#25721 = ORIENTED_EDGE('',*,*,#18528,.F.) ;
#25722 = ORIENTED_EDGE('',*,*,#18518,.F.) ;
#25723 = ORIENTED_EDGE('',*,*,#18529,.F.) ;
#25724 = ORIENTED_EDGE('',*,*,#18530,.F.) ;
#25725 = ORIENTED_EDGE('',*,*,#17623,.F.) ;
#25726 = ORIENTED_EDGE('',*,*,#18517,.F.) ;
#25727 = ORIENTED_EDGE('',*,*,#18531,.F.) ;
#25728 = ORIENTED_EDGE('',*,*,#18512,.F.) ;
#25729 = ORIENTED_EDGE('',*,*,#18532,.F.) ;
#25730 = ORIENTED_EDGE('',*,*,#18516,.F.) ;
#25731 = ORIENTED_EDGE('',*,*,#17632,.F.) ;
#25732 = ORIENTED_EDGE('',*,*,#18526,.T.) ;
#25733 = ORIENTED_EDGE('',*,*,#18533,.F.) ;
#25734 = ORIENTED_EDGE('',*,*,#18508,.T.) ;
#25735 = ORIENTED_EDGE('',*,*,#18510,.T.) ;
#25736 = ORIENTED_EDGE('',*,*,#18199,.F.) ;
#25737 = ORIENTED_EDGE('',*,*,#18522,.T.) ;
#25738 = ORIENTED_EDGE('',*,*,#18534,.F.) ;
#25739 = ORIENTED_EDGE('',*,*,#18535,.F.) ;
#25740 = ORIENTED_EDGE('',*,*,#18536,.F.) ;
#25741 = ORIENTED_EDGE('',*,*,#18211,.F.) ;
#25742 = ORIENTED_EDGE('',*,*,#18534,.T.) ;
#25743 = ORIENTED_EDGE('',*,*,#18537,.F.) ;
#25744 = ORIENTED_EDGE('',*,*,#18530,.T.) ;
#25745 = ORIENTED_EDGE('',*,*,#18514,.T.) ;
#25746 = ORIENTED_EDGE('',*,*,#18209,.F.) ;
#25747 = ORIENTED_EDGE('',*,*,#18536,.T.) ;
#25748 = ORIENTED_EDGE('',*,*,#17612,.F.) ;
#25749 = ORIENTED_EDGE('',*,*,#17620,.T.) ;
#25750 = ORIENTED_EDGE('',*,*,#18529,.T.) ;
#25751 = ORIENTED_EDGE('',*,*,#18521,.T.) ;
#25752 = ORIENTED_EDGE('',*,*,#18511,.T.) ;
#25753 = ORIENTED_EDGE('',*,*,#18523,.T.) ;
#25754 = ORIENTED_EDGE('',*,*,#18528,.T.) ;
#25755 = ORIENTED_EDGE('',*,*,#18527,.T.) ;
#25756 = ORIENTED_EDGE('',*,*,#18531,.T.) ;
#25757 = ORIENTED_EDGE('',*,*,#18532,.T.) ;
#25758 = ORIENTED_EDGE('',*,*,#18515,.T.) ;
#25759 = ORIENTED_EDGE('',*,*,#18535,.T.) ;
#25760 = ORIENTED_EDGE('',*,*,#18538,.T.) ;
#25761 = ORIENTED_EDGE('',*,*,#18539,.T.) ;
#25762 = ORIENTED_EDGE('',*,*,#18540,.T.) ;
#25763 = ORIENTED_EDGE('',*,*,#18541,.T.) ;
#25764 = ORIENTED_EDGE('',*,*,#18542,.T.) ;
#25765 = ORIENTED_EDGE('',*,*,#18543,.T.) ;
#25766 = ORIENTED_EDGE('',*,*,#18544,.F.) ;
#25767 = ORIENTED_EDGE('',*,*,#18545,.T.) ;
#25768 = ORIENTED_EDGE('',*,*,#18546,.T.) ;
#25769 = ORIENTED_EDGE('',*,*,#18547,.F.) ;
#25770 = ORIENTED_EDGE('',*,*,#18548,.F.) ;
#25771 = ORIENTED_EDGE('',*,*,#18543,.F.) ;
#25772 = ORIENTED_EDGE('',*,*,#18538,.F.) ;
#25773 = ORIENTED_EDGE('',*,*,#18545,.F.) ;
#25774 = ORIENTED_EDGE('',*,*,#18546,.F.) ;
#25775 = ORIENTED_EDGE('',*,*,#18541,.F.) ;
#25776 = ORIENTED_EDGE('',*,*,#18549,.F.) ;
#25777 = ORIENTED_EDGE('',*,*,#17923,.F.) ;
#25778 = ORIENTED_EDGE('',*,*,#18542,.F.) ;
#25779 = ORIENTED_EDGE('',*,*,#18550,.F.) ;
#25780 = ORIENTED_EDGE('',*,*,#18551,.F.) ;
#25781 = ORIENTED_EDGE('',*,*,#18539,.F.) ;
#25782 = ORIENTED_EDGE('',*,*,#18540,.F.) ;
#25783 = ORIENTED_EDGE('',*,*,#18552,.F.) ;
#25784 = ORIENTED_EDGE('',*,*,#17919,.F.) ;
#25785 = ORIENTED_EDGE('',*,*,#18553,.F.) ;
#25786 = ORIENTED_EDGE('',*,*,#18551,.T.) ;
#25787 = ORIENTED_EDGE('',*,*,#17916,.T.) ;
#25788 = ORIENTED_EDGE('',*,*,#18552,.T.) ;
#25789 = ORIENTED_EDGE('',*,*,#17921,.T.) ;
#25790 = ORIENTED_EDGE('',*,*,#18549,.T.) ;
#25791 = ORIENTED_EDGE('',*,*,#18553,.T.) ;
#25792 = ORIENTED_EDGE('',*,*,#17586,.F.) ;
#25793 = ORIENTED_EDGE('',*,*,#18170,.F.) ;
#25794 = ORIENTED_EDGE('',*,*,#18554,.F.) ;
#25795 = ORIENTED_EDGE('',*,*,#17600,.F.) ;
#25796 = ORIENTED_EDGE('',*,*,#18555,.F.) ;
#25797 = ORIENTED_EDGE('',*,*,#18556,.F.) ;
#25798 = ORIENTED_EDGE('',*,*,#18557,.F.) ;
#25799 = ORIENTED_EDGE('',*,*,#18558,.F.) ;
#25800 = ORIENTED_EDGE('',*,*,#18559,.T.) ;
#25801 = ORIENTED_EDGE('',*,*,#18554,.T.) ;
#25802 = ORIENTED_EDGE('',*,*,#18169,.F.) ;
#25803 = ORIENTED_EDGE('',*,*,#18560,.T.) ;
#25804 = ORIENTED_EDGE('',*,*,#18561,.F.) ;
#25805 = ORIENTED_EDGE('',*,*,#18562,.F.) ;
#25806 = ORIENTED_EDGE('',*,*,#18560,.F.) ;
#25807 = ORIENTED_EDGE('',*,*,#18168,.F.) ;
#25808 = ORIENTED_EDGE('',*,*,#18563,.T.) ;
#25809 = ORIENTED_EDGE('',*,*,#18564,.T.) ;
#25810 = ORIENTED_EDGE('',*,*,#17591,.F.) ;
#25811 = ORIENTED_EDGE('',*,*,#17599,.T.) ;
#25812 = ORIENTED_EDGE('',*,*,#18565,.T.) ;
#25813 = ORIENTED_EDGE('',*,*,#18566,.T.) ;
#25814 = ORIENTED_EDGE('',*,*,#18165,.F.) ;
#25815 = ORIENTED_EDGE('',*,*,#18567,.T.) ;
#25816 = ORIENTED_EDGE('',*,*,#17583,.T.) ;
#25817 = ORIENTED_EDGE('',*,*,#18568,.F.) ;
#25818 = ORIENTED_EDGE('',*,*,#18567,.F.) ;
#25819 = ORIENTED_EDGE('',*,*,#18164,.F.) ;
#25820 = ORIENTED_EDGE('',*,*,#18569,.F.) ;
#25821 = ORIENTED_EDGE('',*,*,#18166,.F.) ;
#25822 = ORIENTED_EDGE('',*,*,#18566,.F.) ;
#25823 = ORIENTED_EDGE('',*,*,#18570,.F.) ;
#25824 = ORIENTED_EDGE('',*,*,#18571,.T.) ;
#25825 = ORIENTED_EDGE('',*,*,#17588,.T.) ;
#25826 = ORIENTED_EDGE('',*,*,#17597,.F.) ;
#25827 = ORIENTED_EDGE('',*,*,#18572,.T.) ;
#25828 = ORIENTED_EDGE('',*,*,#18573,.F.) ;
#25829 = ORIENTED_EDGE('',*,*,#18574,.F.) ;
#25830 = ORIENTED_EDGE('',*,*,#18572,.F.) ;
#25831 = ORIENTED_EDGE('',*,*,#17596,.F.) ;
#25832 = ORIENTED_EDGE('',*,*,#18571,.F.) ;
#25833 = ORIENTED_EDGE('',*,*,#18575,.F.) ;
#25834 = ORIENTED_EDGE('',*,*,#18565,.F.) ;
#25835 = ORIENTED_EDGE('',*,*,#18576,.F.) ;
#25836 = ORIENTED_EDGE('',*,*,#18577,.F.) ;
#25837 = ORIENTED_EDGE('',*,*,#17592,.F.) ;
#25838 = ORIENTED_EDGE('',*,*,#18564,.F.) ;
#25839 = ORIENTED_EDGE('',*,*,#18578,.F.) ;
#25840 = ORIENTED_EDGE('',*,*,#18559,.F.) ;
#25841 = ORIENTED_EDGE('',*,*,#18579,.F.) ;
#25842 = ORIENTED_EDGE('',*,*,#18563,.F.) ;
#25843 = ORIENTED_EDGE('',*,*,#17601,.F.) ;
#25844 = ORIENTED_EDGE('',*,*,#18573,.T.) ;
#25845 = ORIENTED_EDGE('',*,*,#18580,.F.) ;
#25846 = ORIENTED_EDGE('',*,*,#18555,.T.) ;
#25847 = ORIENTED_EDGE('',*,*,#18557,.T.) ;
#25848 = ORIENTED_EDGE('',*,*,#18162,.F.) ;
#25849 = ORIENTED_EDGE('',*,*,#18569,.T.) ;
#25850 = ORIENTED_EDGE('',*,*,#18581,.F.) ;
#25851 = ORIENTED_EDGE('',*,*,#18582,.F.) ;
#25852 = ORIENTED_EDGE('',*,*,#18583,.F.) ;
#25853 = ORIENTED_EDGE('',*,*,#18174,.F.) ;
#25854 = ORIENTED_EDGE('',*,*,#18581,.T.) ;
#25855 = ORIENTED_EDGE('',*,*,#18584,.F.) ;
#25856 = ORIENTED_EDGE('',*,*,#18577,.T.) ;
#25857 = ORIENTED_EDGE('',*,*,#18561,.T.) ;
#25858 = ORIENTED_EDGE('',*,*,#18172,.F.) ;
#25859 = ORIENTED_EDGE('',*,*,#18583,.T.) ;
#25860 = ORIENTED_EDGE('',*,*,#17581,.F.) ;
#25861 = ORIENTED_EDGE('',*,*,#17589,.T.) ;
#25862 = ORIENTED_EDGE('',*,*,#18576,.T.) ;
#25863 = ORIENTED_EDGE('',*,*,#18568,.T.) ;
#25864 = ORIENTED_EDGE('',*,*,#18558,.T.) ;
#25865 = ORIENTED_EDGE('',*,*,#18570,.T.) ;
#25866 = ORIENTED_EDGE('',*,*,#18575,.T.) ;
#25867 = ORIENTED_EDGE('',*,*,#18574,.T.) ;
#25868 = ORIENTED_EDGE('',*,*,#18578,.T.) ;
#25869 = ORIENTED_EDGE('',*,*,#18579,.T.) ;
#25870 = ORIENTED_EDGE('',*,*,#18562,.T.) ;
#25871 = ORIENTED_EDGE('',*,*,#18582,.T.) ;
#25872 = ORIENTED_EDGE('',*,*,#18585,.T.) ;
#25873 = ORIENTED_EDGE('',*,*,#18586,.T.) ;
#25874 = ORIENTED_EDGE('',*,*,#18587,.T.) ;
#25875 = ORIENTED_EDGE('',*,*,#18588,.T.) ;
#25876 = ORIENTED_EDGE('',*,*,#18589,.T.) ;
#25877 = ORIENTED_EDGE('',*,*,#18590,.T.) ;
#25878 = ORIENTED_EDGE('',*,*,#18591,.F.) ;
#25879 = ORIENTED_EDGE('',*,*,#18592,.T.) ;
#25880 = ORIENTED_EDGE('',*,*,#18593,.T.) ;
#25881 = ORIENTED_EDGE('',*,*,#18594,.F.) ;
#25882 = ORIENTED_EDGE('',*,*,#18595,.F.) ;
#25883 = ORIENTED_EDGE('',*,*,#18590,.F.) ;
#25884 = ORIENTED_EDGE('',*,*,#18585,.F.) ;
#25885 = ORIENTED_EDGE('',*,*,#18592,.F.) ;
#25886 = ORIENTED_EDGE('',*,*,#18593,.F.) ;
#25887 = ORIENTED_EDGE('',*,*,#18588,.F.) ;
#25888 = ORIENTED_EDGE('',*,*,#18596,.F.) ;
#25889 = ORIENTED_EDGE('',*,*,#17890,.F.) ;
#25890 = ORIENTED_EDGE('',*,*,#18589,.F.) ;
#25891 = ORIENTED_EDGE('',*,*,#18597,.F.) ;
#25892 = ORIENTED_EDGE('',*,*,#18598,.F.) ;
#25893 = ORIENTED_EDGE('',*,*,#18586,.F.) ;
#25894 = ORIENTED_EDGE('',*,*,#18587,.F.) ;
#25895 = ORIENTED_EDGE('',*,*,#18599,.F.) ;
#25896 = ORIENTED_EDGE('',*,*,#17886,.F.) ;
#25897 = ORIENTED_EDGE('',*,*,#18600,.F.) ;
#25898 = ORIENTED_EDGE('',*,*,#18598,.T.) ;
#25899 = ORIENTED_EDGE('',*,*,#17883,.T.) ;
#25900 = ORIENTED_EDGE('',*,*,#18599,.T.) ;
#25901 = ORIENTED_EDGE('',*,*,#17888,.T.) ;
#25902 = ORIENTED_EDGE('',*,*,#18596,.T.) ;
#25903 = ORIENTED_EDGE('',*,*,#18600,.T.) ;
#25904 = ORIENTED_EDGE('',*,*,#17555,.F.) ;
#25905 = ORIENTED_EDGE('',*,*,#18133,.F.) ;
#25906 = ORIENTED_EDGE('',*,*,#18601,.F.) ;
#25907 = ORIENTED_EDGE('',*,*,#17569,.F.) ;
#25908 = ORIENTED_EDGE('',*,*,#18602,.F.) ;
#25909 = ORIENTED_EDGE('',*,*,#18603,.F.) ;
#25910 = ORIENTED_EDGE('',*,*,#18604,.F.) ;
#25911 = ORIENTED_EDGE('',*,*,#18605,.F.) ;
#25912 = ORIENTED_EDGE('',*,*,#18606,.T.) ;
#25913 = ORIENTED_EDGE('',*,*,#18601,.T.) ;
#25914 = ORIENTED_EDGE('',*,*,#18132,.F.) ;
#25915 = ORIENTED_EDGE('',*,*,#18607,.T.) ;
#25916 = ORIENTED_EDGE('',*,*,#18608,.F.) ;
#25917 = ORIENTED_EDGE('',*,*,#18609,.F.) ;
#25918 = ORIENTED_EDGE('',*,*,#18607,.F.) ;
#25919 = ORIENTED_EDGE('',*,*,#18131,.F.) ;
#25920 = ORIENTED_EDGE('',*,*,#18610,.T.) ;
#25921 = ORIENTED_EDGE('',*,*,#18611,.T.) ;
#25922 = ORIENTED_EDGE('',*,*,#17560,.F.) ;
#25923 = ORIENTED_EDGE('',*,*,#17568,.T.) ;
#25924 = ORIENTED_EDGE('',*,*,#18612,.T.) ;
#25925 = ORIENTED_EDGE('',*,*,#18613,.T.) ;
#25926 = ORIENTED_EDGE('',*,*,#18128,.F.) ;
#25927 = ORIENTED_EDGE('',*,*,#18614,.T.) ;
#25928 = ORIENTED_EDGE('',*,*,#17552,.T.) ;
#25929 = ORIENTED_EDGE('',*,*,#18615,.F.) ;
#25930 = ORIENTED_EDGE('',*,*,#18614,.F.) ;
#25931 = ORIENTED_EDGE('',*,*,#18127,.F.) ;
#25932 = ORIENTED_EDGE('',*,*,#18616,.F.) ;
#25933 = ORIENTED_EDGE('',*,*,#18129,.F.) ;
#25934 = ORIENTED_EDGE('',*,*,#18613,.F.) ;
#25935 = ORIENTED_EDGE('',*,*,#18617,.F.) ;
#25936 = ORIENTED_EDGE('',*,*,#18618,.T.) ;
#25937 = ORIENTED_EDGE('',*,*,#17557,.T.) ;
#25938 = ORIENTED_EDGE('',*,*,#17566,.F.) ;
#25939 = ORIENTED_EDGE('',*,*,#18619,.T.) ;
#25940 = ORIENTED_EDGE('',*,*,#18620,.F.) ;
#25941 = ORIENTED_EDGE('',*,*,#18621,.F.) ;
#25942 = ORIENTED_EDGE('',*,*,#18619,.F.) ;
#25943 = ORIENTED_EDGE('',*,*,#17565,.F.) ;
#25944 = ORIENTED_EDGE('',*,*,#18618,.F.) ;
#25945 = ORIENTED_EDGE('',*,*,#18622,.F.) ;
#25946 = ORIENTED_EDGE('',*,*,#18612,.F.) ;
#25947 = ORIENTED_EDGE('',*,*,#18623,.F.) ;
#25948 = ORIENTED_EDGE('',*,*,#18624,.F.) ;
#25949 = ORIENTED_EDGE('',*,*,#17561,.F.) ;
#25950 = ORIENTED_EDGE('',*,*,#18611,.F.) ;
#25951 = ORIENTED_EDGE('',*,*,#18625,.F.) ;
#25952 = ORIENTED_EDGE('',*,*,#18606,.F.) ;
#25953 = ORIENTED_EDGE('',*,*,#18626,.F.) ;
#25954 = ORIENTED_EDGE('',*,*,#18610,.F.) ;
#25955 = ORIENTED_EDGE('',*,*,#17570,.F.) ;
#25956 = ORIENTED_EDGE('',*,*,#18620,.T.) ;
#25957 = ORIENTED_EDGE('',*,*,#18627,.F.) ;
#25958 = ORIENTED_EDGE('',*,*,#18602,.T.) ;
#25959 = ORIENTED_EDGE('',*,*,#18604,.T.) ;
#25960 = ORIENTED_EDGE('',*,*,#18125,.F.) ;
#25961 = ORIENTED_EDGE('',*,*,#18616,.T.) ;
#25962 = ORIENTED_EDGE('',*,*,#18628,.F.) ;
#25963 = ORIENTED_EDGE('',*,*,#18629,.F.) ;
#25964 = ORIENTED_EDGE('',*,*,#18630,.F.) ;
#25965 = ORIENTED_EDGE('',*,*,#18137,.F.) ;
#25966 = ORIENTED_EDGE('',*,*,#18628,.T.) ;
#25967 = ORIENTED_EDGE('',*,*,#18631,.F.) ;
#25968 = ORIENTED_EDGE('',*,*,#18624,.T.) ;
#25969 = ORIENTED_EDGE('',*,*,#18608,.T.) ;
#25970 = ORIENTED_EDGE('',*,*,#18135,.F.) ;
#25971 = ORIENTED_EDGE('',*,*,#18630,.T.) ;
#25972 = ORIENTED_EDGE('',*,*,#17550,.F.) ;
#25973 = ORIENTED_EDGE('',*,*,#17558,.T.) ;
#25974 = ORIENTED_EDGE('',*,*,#18623,.T.) ;
#25975 = ORIENTED_EDGE('',*,*,#18615,.T.) ;
#25976 = ORIENTED_EDGE('',*,*,#18605,.T.) ;
#25977 = ORIENTED_EDGE('',*,*,#18617,.T.) ;
#25978 = ORIENTED_EDGE('',*,*,#18622,.T.) ;
#25979 = ORIENTED_EDGE('',*,*,#18621,.T.) ;
#25980 = ORIENTED_EDGE('',*,*,#18625,.T.) ;
#25981 = ORIENTED_EDGE('',*,*,#18626,.T.) ;
#25982 = ORIENTED_EDGE('',*,*,#18609,.T.) ;
#25983 = ORIENTED_EDGE('',*,*,#18629,.T.) ;
#25984 = ORIENTED_EDGE('',*,*,#18632,.T.) ;
#25985 = ORIENTED_EDGE('',*,*,#18633,.T.) ;
#25986 = ORIENTED_EDGE('',*,*,#18634,.T.) ;
#25987 = ORIENTED_EDGE('',*,*,#18635,.T.) ;
#25988 = ORIENTED_EDGE('',*,*,#18636,.T.) ;
#25989 = ORIENTED_EDGE('',*,*,#18637,.T.) ;
#25990 = ORIENTED_EDGE('',*,*,#18638,.F.) ;
#25991 = ORIENTED_EDGE('',*,*,#18639,.T.) ;
#25992 = ORIENTED_EDGE('',*,*,#18640,.T.) ;
#25993 = ORIENTED_EDGE('',*,*,#18641,.F.) ;
#25994 = ORIENTED_EDGE('',*,*,#18642,.F.) ;
#25995 = ORIENTED_EDGE('',*,*,#18637,.F.) ;
#25996 = ORIENTED_EDGE('',*,*,#18632,.F.) ;
#25997 = ORIENTED_EDGE('',*,*,#18639,.F.) ;
#25998 = ORIENTED_EDGE('',*,*,#18640,.F.) ;
#25999 = ORIENTED_EDGE('',*,*,#18635,.F.) ;
#26000 = ORIENTED_EDGE('',*,*,#18643,.F.) ;
#26001 = ORIENTED_EDGE('',*,*,#17857,.F.) ;
#26002 = ORIENTED_EDGE('',*,*,#18636,.F.) ;
#26003 = ORIENTED_EDGE('',*,*,#18644,.F.) ;
#26004 = ORIENTED_EDGE('',*,*,#18645,.F.) ;
#26005 = ORIENTED_EDGE('',*,*,#18633,.F.) ;
#26006 = ORIENTED_EDGE('',*,*,#18634,.F.) ;
#26007 = ORIENTED_EDGE('',*,*,#18646,.F.) ;
#26008 = ORIENTED_EDGE('',*,*,#17853,.F.) ;
#26009 = ORIENTED_EDGE('',*,*,#18647,.F.) ;
#26010 = ORIENTED_EDGE('',*,*,#18645,.T.) ;
#26011 = ORIENTED_EDGE('',*,*,#17850,.T.) ;
#26012 = ORIENTED_EDGE('',*,*,#18646,.T.) ;
#26013 = ORIENTED_EDGE('',*,*,#17855,.T.) ;
#26014 = ORIENTED_EDGE('',*,*,#18643,.T.) ;
#26015 = ORIENTED_EDGE('',*,*,#18647,.T.) ;
#26016 = ORIENTED_EDGE('',*,*,#17524,.F.) ;
#26017 = ORIENTED_EDGE('',*,*,#18096,.F.) ;
#26018 = ORIENTED_EDGE('',*,*,#18648,.F.) ;
#26019 = ORIENTED_EDGE('',*,*,#17538,.F.) ;
#26020 = ORIENTED_EDGE('',*,*,#18649,.F.) ;
#26021 = ORIENTED_EDGE('',*,*,#18650,.F.) ;
#26022 = ORIENTED_EDGE('',*,*,#18651,.F.) ;
#26023 = ORIENTED_EDGE('',*,*,#18652,.F.) ;
#26024 = ORIENTED_EDGE('',*,*,#18653,.T.) ;
#26025 = ORIENTED_EDGE('',*,*,#18648,.T.) ;
#26026 = ORIENTED_EDGE('',*,*,#18095,.F.) ;
#26027 = ORIENTED_EDGE('',*,*,#18654,.T.) ;
#26028 = ORIENTED_EDGE('',*,*,#18655,.F.) ;
#26029 = ORIENTED_EDGE('',*,*,#18656,.F.) ;
#26030 = ORIENTED_EDGE('',*,*,#18654,.F.) ;
#26031 = ORIENTED_EDGE('',*,*,#18094,.F.) ;
#26032 = ORIENTED_EDGE('',*,*,#18657,.T.) ;
#26033 = ORIENTED_EDGE('',*,*,#18658,.T.) ;
#26034 = ORIENTED_EDGE('',*,*,#17529,.F.) ;
#26035 = ORIENTED_EDGE('',*,*,#17537,.T.) ;
#26036 = ORIENTED_EDGE('',*,*,#18659,.T.) ;
#26037 = ORIENTED_EDGE('',*,*,#18660,.T.) ;
#26038 = ORIENTED_EDGE('',*,*,#18091,.F.) ;
#26039 = ORIENTED_EDGE('',*,*,#18661,.T.) ;
#26040 = ORIENTED_EDGE('',*,*,#17521,.T.) ;
#26041 = ORIENTED_EDGE('',*,*,#18662,.F.) ;
#26042 = ORIENTED_EDGE('',*,*,#18661,.F.) ;
#26043 = ORIENTED_EDGE('',*,*,#18090,.F.) ;
#26044 = ORIENTED_EDGE('',*,*,#18663,.F.) ;
#26045 = ORIENTED_EDGE('',*,*,#18092,.F.) ;
#26046 = ORIENTED_EDGE('',*,*,#18660,.F.) ;
#26047 = ORIENTED_EDGE('',*,*,#18664,.F.) ;
#26048 = ORIENTED_EDGE('',*,*,#18665,.T.) ;
#26049 = ORIENTED_EDGE('',*,*,#17526,.T.) ;
#26050 = ORIENTED_EDGE('',*,*,#17535,.F.) ;
#26051 = ORIENTED_EDGE('',*,*,#18666,.T.) ;
#26052 = ORIENTED_EDGE('',*,*,#18667,.F.) ;
#26053 = ORIENTED_EDGE('',*,*,#18668,.F.) ;
#26054 = ORIENTED_EDGE('',*,*,#18666,.F.) ;
#26055 = ORIENTED_EDGE('',*,*,#17534,.F.) ;
#26056 = ORIENTED_EDGE('',*,*,#18665,.F.) ;
#26057 = ORIENTED_EDGE('',*,*,#18669,.F.) ;
#26058 = ORIENTED_EDGE('',*,*,#18659,.F.) ;
#26059 = ORIENTED_EDGE('',*,*,#18670,.F.) ;
#26060 = ORIENTED_EDGE('',*,*,#18671,.F.) ;
#26061 = ORIENTED_EDGE('',*,*,#17530,.F.) ;
#26062 = ORIENTED_EDGE('',*,*,#18658,.F.) ;
#26063 = ORIENTED_EDGE('',*,*,#18672,.F.) ;
#26064 = ORIENTED_EDGE('',*,*,#18653,.F.) ;
#26065 = ORIENTED_EDGE('',*,*,#18673,.F.) ;
#26066 = ORIENTED_EDGE('',*,*,#18657,.F.) ;
#26067 = ORIENTED_EDGE('',*,*,#17539,.F.) ;
#26068 = ORIENTED_EDGE('',*,*,#18667,.T.) ;
#26069 = ORIENTED_EDGE('',*,*,#18674,.F.) ;
#26070 = ORIENTED_EDGE('',*,*,#18649,.T.) ;
#26071 = ORIENTED_EDGE('',*,*,#18651,.T.) ;
#26072 = ORIENTED_EDGE('',*,*,#18088,.F.) ;
#26073 = ORIENTED_EDGE('',*,*,#18663,.T.) ;
#26074 = ORIENTED_EDGE('',*,*,#18675,.F.) ;
#26075 = ORIENTED_EDGE('',*,*,#18676,.F.) ;
#26076 = ORIENTED_EDGE('',*,*,#18677,.F.) ;
#26077 = ORIENTED_EDGE('',*,*,#18100,.F.) ;
#26078 = ORIENTED_EDGE('',*,*,#18675,.T.) ;
#26079 = ORIENTED_EDGE('',*,*,#18678,.F.) ;
#26080 = ORIENTED_EDGE('',*,*,#18671,.T.) ;
#26081 = ORIENTED_EDGE('',*,*,#18655,.T.) ;
#26082 = ORIENTED_EDGE('',*,*,#18098,.F.) ;
#26083 = ORIENTED_EDGE('',*,*,#18677,.T.) ;
#26084 = ORIENTED_EDGE('',*,*,#17519,.F.) ;
#26085 = ORIENTED_EDGE('',*,*,#17527,.T.) ;
#26086 = ORIENTED_EDGE('',*,*,#18670,.T.) ;
#26087 = ORIENTED_EDGE('',*,*,#18662,.T.) ;
#26088 = ORIENTED_EDGE('',*,*,#18652,.T.) ;
#26089 = ORIENTED_EDGE('',*,*,#18664,.T.) ;
#26090 = ORIENTED_EDGE('',*,*,#18669,.T.) ;
#26091 = ORIENTED_EDGE('',*,*,#18668,.T.) ;
#26092 = ORIENTED_EDGE('',*,*,#18672,.T.) ;
#26093 = ORIENTED_EDGE('',*,*,#18673,.T.) ;
#26094 = ORIENTED_EDGE('',*,*,#18656,.T.) ;
#26095 = ORIENTED_EDGE('',*,*,#18676,.T.) ;
#26096 = ORIENTED_EDGE('',*,*,#18679,.T.) ;
#26097 = ORIENTED_EDGE('',*,*,#18680,.T.) ;
#26098 = ORIENTED_EDGE('',*,*,#18681,.T.) ;
#26099 = ORIENTED_EDGE('',*,*,#18682,.T.) ;
#26100 = ORIENTED_EDGE('',*,*,#18683,.T.) ;
#26101 = ORIENTED_EDGE('',*,*,#18684,.T.) ;
#26102 = ORIENTED_EDGE('',*,*,#18685,.F.) ;
#26103 = ORIENTED_EDGE('',*,*,#18686,.T.) ;
#26104 = ORIENTED_EDGE('',*,*,#18687,.T.) ;
#26105 = ORIENTED_EDGE('',*,*,#18688,.F.) ;
#26106 = ORIENTED_EDGE('',*,*,#18689,.F.) ;
#26107 = ORIENTED_EDGE('',*,*,#18684,.F.) ;
#26108 = ORIENTED_EDGE('',*,*,#18679,.F.) ;
#26109 = ORIENTED_EDGE('',*,*,#18686,.F.) ;
#26110 = ORIENTED_EDGE('',*,*,#18687,.F.) ;
#26111 = ORIENTED_EDGE('',*,*,#18682,.F.) ;
#26112 = ORIENTED_EDGE('',*,*,#18690,.F.) ;
#26113 = ORIENTED_EDGE('',*,*,#17824,.F.) ;
#26114 = ORIENTED_EDGE('',*,*,#18683,.F.) ;
#26115 = ORIENTED_EDGE('',*,*,#18691,.F.) ;
#26116 = ORIENTED_EDGE('',*,*,#18692,.F.) ;
#26117 = ORIENTED_EDGE('',*,*,#18680,.F.) ;
#26118 = ORIENTED_EDGE('',*,*,#18681,.F.) ;
#26119 = ORIENTED_EDGE('',*,*,#18693,.F.) ;
#26120 = ORIENTED_EDGE('',*,*,#17820,.F.) ;
#26121 = ORIENTED_EDGE('',*,*,#18694,.F.) ;
#26122 = ORIENTED_EDGE('',*,*,#18692,.T.) ;
#26123 = ORIENTED_EDGE('',*,*,#17817,.T.) ;
#26124 = ORIENTED_EDGE('',*,*,#18693,.T.) ;
#26125 = ORIENTED_EDGE('',*,*,#17822,.T.) ;
#26126 = ORIENTED_EDGE('',*,*,#18690,.T.) ;
#26127 = ORIENTED_EDGE('',*,*,#18694,.T.) ;
#26128 = ORIENTED_EDGE('',*,*,#17493,.F.) ;
#26129 = ORIENTED_EDGE('',*,*,#18059,.F.) ;
#26130 = ORIENTED_EDGE('',*,*,#18695,.F.) ;
#26131 = ORIENTED_EDGE('',*,*,#17507,.F.) ;
#26132 = ORIENTED_EDGE('',*,*,#18696,.F.) ;
#26133 = ORIENTED_EDGE('',*,*,#18697,.F.) ;
#26134 = ORIENTED_EDGE('',*,*,#18698,.F.) ;
#26135 = ORIENTED_EDGE('',*,*,#18699,.F.) ;
#26136 = ORIENTED_EDGE('',*,*,#18700,.T.) ;
#26137 = ORIENTED_EDGE('',*,*,#18695,.T.) ;
#26138 = ORIENTED_EDGE('',*,*,#18058,.F.) ;
#26139 = ORIENTED_EDGE('',*,*,#18701,.T.) ;
#26140 = ORIENTED_EDGE('',*,*,#18702,.F.) ;
#26141 = ORIENTED_EDGE('',*,*,#18703,.F.) ;
#26142 = ORIENTED_EDGE('',*,*,#18701,.F.) ;
#26143 = ORIENTED_EDGE('',*,*,#18057,.F.) ;
#26144 = ORIENTED_EDGE('',*,*,#18704,.T.) ;
#26145 = ORIENTED_EDGE('',*,*,#18705,.T.) ;
#26146 = ORIENTED_EDGE('',*,*,#17498,.F.) ;
#26147 = ORIENTED_EDGE('',*,*,#17506,.T.) ;
#26148 = ORIENTED_EDGE('',*,*,#18706,.T.) ;
#26149 = ORIENTED_EDGE('',*,*,#18707,.T.) ;
#26150 = ORIENTED_EDGE('',*,*,#18054,.F.) ;
#26151 = ORIENTED_EDGE('',*,*,#18708,.T.) ;
#26152 = ORIENTED_EDGE('',*,*,#17490,.T.) ;
#26153 = ORIENTED_EDGE('',*,*,#18709,.F.) ;
#26154 = ORIENTED_EDGE('',*,*,#18708,.F.) ;
#26155 = ORIENTED_EDGE('',*,*,#18053,.F.) ;
#26156 = ORIENTED_EDGE('',*,*,#18710,.F.) ;
#26157 = ORIENTED_EDGE('',*,*,#18055,.F.) ;
#26158 = ORIENTED_EDGE('',*,*,#18707,.F.) ;
#26159 = ORIENTED_EDGE('',*,*,#18711,.F.) ;
#26160 = ORIENTED_EDGE('',*,*,#18712,.T.) ;
#26161 = ORIENTED_EDGE('',*,*,#17495,.T.) ;
#26162 = ORIENTED_EDGE('',*,*,#17504,.F.) ;
#26163 = ORIENTED_EDGE('',*,*,#18713,.T.) ;
#26164 = ORIENTED_EDGE('',*,*,#18714,.F.) ;
#26165 = ORIENTED_EDGE('',*,*,#18715,.F.) ;
#26166 = ORIENTED_EDGE('',*,*,#18713,.F.) ;
#26167 = ORIENTED_EDGE('',*,*,#17503,.F.) ;
#26168 = ORIENTED_EDGE('',*,*,#18712,.F.) ;
#26169 = ORIENTED_EDGE('',*,*,#18716,.F.) ;
#26170 = ORIENTED_EDGE('',*,*,#18706,.F.) ;
#26171 = ORIENTED_EDGE('',*,*,#18717,.F.) ;
#26172 = ORIENTED_EDGE('',*,*,#18718,.F.) ;
#26173 = ORIENTED_EDGE('',*,*,#17499,.F.) ;
#26174 = ORIENTED_EDGE('',*,*,#18705,.F.) ;
#26175 = ORIENTED_EDGE('',*,*,#18719,.F.) ;
#26176 = ORIENTED_EDGE('',*,*,#18700,.F.) ;
#26177 = ORIENTED_EDGE('',*,*,#18720,.F.) ;
#26178 = ORIENTED_EDGE('',*,*,#18704,.F.) ;
#26179 = ORIENTED_EDGE('',*,*,#17508,.F.) ;
#26180 = ORIENTED_EDGE('',*,*,#18714,.T.) ;
#26181 = ORIENTED_EDGE('',*,*,#18721,.F.) ;
#26182 = ORIENTED_EDGE('',*,*,#18696,.T.) ;
#26183 = ORIENTED_EDGE('',*,*,#18698,.T.) ;
#26184 = ORIENTED_EDGE('',*,*,#18051,.F.) ;
#26185 = ORIENTED_EDGE('',*,*,#18710,.T.) ;
#26186 = ORIENTED_EDGE('',*,*,#18722,.F.) ;
#26187 = ORIENTED_EDGE('',*,*,#18723,.F.) ;
#26188 = ORIENTED_EDGE('',*,*,#18724,.F.) ;
#26189 = ORIENTED_EDGE('',*,*,#18063,.F.) ;
#26190 = ORIENTED_EDGE('',*,*,#18722,.T.) ;
#26191 = ORIENTED_EDGE('',*,*,#18725,.F.) ;
#26192 = ORIENTED_EDGE('',*,*,#18718,.T.) ;
#26193 = ORIENTED_EDGE('',*,*,#18702,.T.) ;
#26194 = ORIENTED_EDGE('',*,*,#18061,.F.) ;
#26195 = ORIENTED_EDGE('',*,*,#18724,.T.) ;
#26196 = ORIENTED_EDGE('',*,*,#17488,.F.) ;
#26197 = ORIENTED_EDGE('',*,*,#17496,.T.) ;
#26198 = ORIENTED_EDGE('',*,*,#18717,.T.) ;
#26199 = ORIENTED_EDGE('',*,*,#18709,.T.) ;
#26200 = ORIENTED_EDGE('',*,*,#18699,.T.) ;
#26201 = ORIENTED_EDGE('',*,*,#18711,.T.) ;
#26202 = ORIENTED_EDGE('',*,*,#18716,.T.) ;
#26203 = ORIENTED_EDGE('',*,*,#18715,.T.) ;
#26204 = ORIENTED_EDGE('',*,*,#18719,.T.) ;
#26205 = ORIENTED_EDGE('',*,*,#18720,.T.) ;
#26206 = ORIENTED_EDGE('',*,*,#18703,.T.) ;
#26207 = ORIENTED_EDGE('',*,*,#18723,.T.) ;
#26208 = ORIENTED_EDGE('',*,*,#18726,.T.) ;
#26209 = ORIENTED_EDGE('',*,*,#18727,.T.) ;
#26210 = ORIENTED_EDGE('',*,*,#18728,.T.) ;
#26211 = ORIENTED_EDGE('',*,*,#18729,.T.) ;
#26212 = ORIENTED_EDGE('',*,*,#18730,.T.) ;
#26213 = ORIENTED_EDGE('',*,*,#18731,.T.) ;
#26214 = ORIENTED_EDGE('',*,*,#18732,.F.) ;
#26215 = ORIENTED_EDGE('',*,*,#18733,.T.) ;
#26216 = ORIENTED_EDGE('',*,*,#18734,.T.) ;
#26217 = ORIENTED_EDGE('',*,*,#18735,.F.) ;
#26218 = ORIENTED_EDGE('',*,*,#18736,.F.) ;
#26219 = ORIENTED_EDGE('',*,*,#18731,.F.) ;
#26220 = ORIENTED_EDGE('',*,*,#18726,.F.) ;
#26221 = ORIENTED_EDGE('',*,*,#18733,.F.) ;
#26222 = ORIENTED_EDGE('',*,*,#18734,.F.) ;
#26223 = ORIENTED_EDGE('',*,*,#18729,.F.) ;
#26224 = ORIENTED_EDGE('',*,*,#18737,.F.) ;
#26225 = ORIENTED_EDGE('',*,*,#17791,.F.) ;
#26226 = ORIENTED_EDGE('',*,*,#18730,.F.) ;
#26227 = ORIENTED_EDGE('',*,*,#18738,.F.) ;
#26228 = ORIENTED_EDGE('',*,*,#18739,.F.) ;
#26229 = ORIENTED_EDGE('',*,*,#18727,.F.) ;
#26230 = ORIENTED_EDGE('',*,*,#18728,.F.) ;
#26231 = ORIENTED_EDGE('',*,*,#18740,.F.) ;
#26232 = ORIENTED_EDGE('',*,*,#17787,.F.) ;
#26233 = ORIENTED_EDGE('',*,*,#18741,.F.) ;
#26234 = ORIENTED_EDGE('',*,*,#18739,.T.) ;
#26235 = ORIENTED_EDGE('',*,*,#17784,.T.) ;
#26236 = ORIENTED_EDGE('',*,*,#18740,.T.) ;
#26237 = ORIENTED_EDGE('',*,*,#17789,.T.) ;
#26238 = ORIENTED_EDGE('',*,*,#18737,.T.) ;
#26239 = ORIENTED_EDGE('',*,*,#18741,.T.) ;
#26240 = ORIENTED_EDGE('',*,*,#17462,.F.) ;
#26241 = ORIENTED_EDGE('',*,*,#18022,.F.) ;
#26242 = ORIENTED_EDGE('',*,*,#18742,.F.) ;
#26243 = ORIENTED_EDGE('',*,*,#17476,.F.) ;
#26244 = ORIENTED_EDGE('',*,*,#18743,.F.) ;
#26245 = ORIENTED_EDGE('',*,*,#18744,.F.) ;
#26246 = ORIENTED_EDGE('',*,*,#18745,.F.) ;
#26247 = ORIENTED_EDGE('',*,*,#18746,.F.) ;
#26248 = ORIENTED_EDGE('',*,*,#18747,.T.) ;
#26249 = ORIENTED_EDGE('',*,*,#18742,.T.) ;
#26250 = ORIENTED_EDGE('',*,*,#18021,.F.) ;
#26251 = ORIENTED_EDGE('',*,*,#18748,.T.) ;
#26252 = ORIENTED_EDGE('',*,*,#18749,.F.) ;
#26253 = ORIENTED_EDGE('',*,*,#18750,.F.) ;
#26254 = ORIENTED_EDGE('',*,*,#18748,.F.) ;
#26255 = ORIENTED_EDGE('',*,*,#18020,.F.) ;
#26256 = ORIENTED_EDGE('',*,*,#18751,.T.) ;
#26257 = ORIENTED_EDGE('',*,*,#18752,.T.) ;
#26258 = ORIENTED_EDGE('',*,*,#17467,.F.) ;
#26259 = ORIENTED_EDGE('',*,*,#17475,.T.) ;
#26260 = ORIENTED_EDGE('',*,*,#18753,.T.) ;
#26261 = ORIENTED_EDGE('',*,*,#18754,.T.) ;
#26262 = ORIENTED_EDGE('',*,*,#18017,.F.) ;
#26263 = ORIENTED_EDGE('',*,*,#18755,.T.) ;
#26264 = ORIENTED_EDGE('',*,*,#17459,.T.) ;
#26265 = ORIENTED_EDGE('',*,*,#18756,.F.) ;
#26266 = ORIENTED_EDGE('',*,*,#18755,.F.) ;
#26267 = ORIENTED_EDGE('',*,*,#18016,.F.) ;
#26268 = ORIENTED_EDGE('',*,*,#18757,.F.) ;
#26269 = ORIENTED_EDGE('',*,*,#18018,.F.) ;
#26270 = ORIENTED_EDGE('',*,*,#18754,.F.) ;
#26271 = ORIENTED_EDGE('',*,*,#18758,.F.) ;
#26272 = ORIENTED_EDGE('',*,*,#18759,.T.) ;
#26273 = ORIENTED_EDGE('',*,*,#17464,.T.) ;
#26274 = ORIENTED_EDGE('',*,*,#17473,.F.) ;
#26275 = ORIENTED_EDGE('',*,*,#18760,.T.) ;
#26276 = ORIENTED_EDGE('',*,*,#18761,.F.) ;
#26277 = ORIENTED_EDGE('',*,*,#18762,.F.) ;
#26278 = ORIENTED_EDGE('',*,*,#18760,.F.) ;
#26279 = ORIENTED_EDGE('',*,*,#17472,.F.) ;
#26280 = ORIENTED_EDGE('',*,*,#18759,.F.) ;
#26281 = ORIENTED_EDGE('',*,*,#18763,.F.) ;
#26282 = ORIENTED_EDGE('',*,*,#18753,.F.) ;
#26283 = ORIENTED_EDGE('',*,*,#18764,.F.) ;
#26284 = ORIENTED_EDGE('',*,*,#18765,.F.) ;
#26285 = ORIENTED_EDGE('',*,*,#17468,.F.) ;
#26286 = ORIENTED_EDGE('',*,*,#18752,.F.) ;
#26287 = ORIENTED_EDGE('',*,*,#18766,.F.) ;
#26288 = ORIENTED_EDGE('',*,*,#18747,.F.) ;
#26289 = ORIENTED_EDGE('',*,*,#18767,.F.) ;
#26290 = ORIENTED_EDGE('',*,*,#18751,.F.) ;
#26291 = ORIENTED_EDGE('',*,*,#17477,.F.) ;
#26292 = ORIENTED_EDGE('',*,*,#18761,.T.) ;
#26293 = ORIENTED_EDGE('',*,*,#18768,.F.) ;
#26294 = ORIENTED_EDGE('',*,*,#18743,.T.) ;
#26295 = ORIENTED_EDGE('',*,*,#18745,.T.) ;
#26296 = ORIENTED_EDGE('',*,*,#18014,.F.) ;
#26297 = ORIENTED_EDGE('',*,*,#18757,.T.) ;
#26298 = ORIENTED_EDGE('',*,*,#18769,.F.) ;
#26299 = ORIENTED_EDGE('',*,*,#18770,.F.) ;
#26300 = ORIENTED_EDGE('',*,*,#18771,.F.) ;
#26301 = ORIENTED_EDGE('',*,*,#18026,.F.) ;
#26302 = ORIENTED_EDGE('',*,*,#18769,.T.) ;
#26303 = ORIENTED_EDGE('',*,*,#18772,.F.) ;
#26304 = ORIENTED_EDGE('',*,*,#18765,.T.) ;
#26305 = ORIENTED_EDGE('',*,*,#18749,.T.) ;
#26306 = ORIENTED_EDGE('',*,*,#18024,.F.) ;
#26307 = ORIENTED_EDGE('',*,*,#18771,.T.) ;
#26308 = ORIENTED_EDGE('',*,*,#17457,.F.) ;
#26309 = ORIENTED_EDGE('',*,*,#17465,.T.) ;
#26310 = ORIENTED_EDGE('',*,*,#18764,.T.) ;
#26311 = ORIENTED_EDGE('',*,*,#18756,.T.) ;
#26312 = ORIENTED_EDGE('',*,*,#18746,.T.) ;
#26313 = ORIENTED_EDGE('',*,*,#18758,.T.) ;
#26314 = ORIENTED_EDGE('',*,*,#18763,.T.) ;
#26315 = ORIENTED_EDGE('',*,*,#18762,.T.) ;
#26316 = ORIENTED_EDGE('',*,*,#18766,.T.) ;
#26317 = ORIENTED_EDGE('',*,*,#18767,.T.) ;
#26318 = ORIENTED_EDGE('',*,*,#18750,.T.) ;
#26319 = ORIENTED_EDGE('',*,*,#18770,.T.) ;
#26320 = ORIENTED_EDGE('',*,*,#18773,.T.) ;
#26321 = ORIENTED_EDGE('',*,*,#18774,.T.) ;
#26322 = ORIENTED_EDGE('',*,*,#18775,.T.) ;
#26323 = ORIENTED_EDGE('',*,*,#18776,.T.) ;
#26324 = ORIENTED_EDGE('',*,*,#18777,.T.) ;
#26325 = ORIENTED_EDGE('',*,*,#18778,.T.) ;
#26326 = ORIENTED_EDGE('',*,*,#18779,.F.) ;
#26327 = ORIENTED_EDGE('',*,*,#18780,.T.) ;
#26328 = ORIENTED_EDGE('',*,*,#18781,.T.) ;
#26329 = ORIENTED_EDGE('',*,*,#18782,.F.) ;
#26330 = ORIENTED_EDGE('',*,*,#18783,.F.) ;
#26331 = ORIENTED_EDGE('',*,*,#18778,.F.) ;
#26332 = ORIENTED_EDGE('',*,*,#18773,.F.) ;
#26333 = ORIENTED_EDGE('',*,*,#18780,.F.) ;
#26334 = ORIENTED_EDGE('',*,*,#18781,.F.) ;
#26335 = ORIENTED_EDGE('',*,*,#18776,.F.) ;
#26336 = ORIENTED_EDGE('',*,*,#18784,.F.) ;
#26337 = ORIENTED_EDGE('',*,*,#17758,.F.) ;
#26338 = ORIENTED_EDGE('',*,*,#18777,.F.) ;
#26339 = ORIENTED_EDGE('',*,*,#18785,.F.) ;
#26340 = ORIENTED_EDGE('',*,*,#18786,.F.) ;
#26341 = ORIENTED_EDGE('',*,*,#18774,.F.) ;
#26342 = ORIENTED_EDGE('',*,*,#18775,.F.) ;
#26343 = ORIENTED_EDGE('',*,*,#18787,.F.) ;
#26344 = ORIENTED_EDGE('',*,*,#17754,.F.) ;
#26345 = ORIENTED_EDGE('',*,*,#18788,.F.) ;
#26346 = ORIENTED_EDGE('',*,*,#18786,.T.) ;
#26347 = ORIENTED_EDGE('',*,*,#17751,.T.) ;
#26348 = ORIENTED_EDGE('',*,*,#18787,.T.) ;
#26349 = ORIENTED_EDGE('',*,*,#17756,.T.) ;
#26350 = ORIENTED_EDGE('',*,*,#18784,.T.) ;
#26351 = ORIENTED_EDGE('',*,*,#18788,.T.) ;
#26352 = ORIENTED_EDGE('',*,*,#18789,.T.) ;
#26353 = ORIENTED_EDGE('',*,*,#17293,.T.) ;
#26354 = ORIENTED_EDGE('',*,*,#18790,.T.) ;
#26355 = ORIENTED_EDGE('',*,*,#17247,.F.) ;
#26356 = ORIENTED_EDGE('',*,*,#18791,.T.) ;
#26357 = ORIENTED_EDGE('',*,*,#17251,.F.) ;
#26358 = ORIENTED_EDGE('',*,*,#18792,.T.) ;
#26359 = ORIENTED_EDGE('',*,*,#17310,.T.) ;
#26360 = ORIENTED_EDGE('',*,*,#18793,.T.) ;
#26361 = ORIENTED_EDGE('',*,*,#17255,.F.) ;
#26362 = ORIENTED_EDGE('',*,*,#18794,.T.) ;
#26363 = ORIENTED_EDGE('',*,*,#17327,.T.) ;
#26364 = ORIENTED_EDGE('',*,*,#18795,.T.) ;
#26365 = ORIENTED_EDGE('',*,*,#17259,.F.) ;
#26366 = ORIENTED_EDGE('',*,*,#18796,.T.) ;
#26367 = ORIENTED_EDGE('',*,*,#17344,.T.) ;
#26368 = ORIENTED_EDGE('',*,*,#18797,.T.) ;
#26369 = ORIENTED_EDGE('',*,*,#17263,.F.) ;
#26370 = ORIENTED_EDGE('',*,*,#18798,.T.) ;
#26371 = ORIENTED_EDGE('',*,*,#17359,.T.) ;
#26372 = ORIENTED_EDGE('',*,*,#18799,.T.) ;
#26373 = ORIENTED_EDGE('',*,*,#17267,.F.) ;
#26374 = ORIENTED_EDGE('',*,*,#18800,.T.) ;
#26375 = ORIENTED_EDGE('',*,*,#17376,.T.) ;
#26376 = ORIENTED_EDGE('',*,*,#18801,.T.) ;
#26377 = ORIENTED_EDGE('',*,*,#17271,.F.) ;
#26378 = ORIENTED_EDGE('',*,*,#18802,.T.) ;
#26379 = ORIENTED_EDGE('',*,*,#17393,.T.) ;
#26380 = ORIENTED_EDGE('',*,*,#18803,.T.) ;
#26381 = ORIENTED_EDGE('',*,*,#17275,.F.) ;
#26382 = ORIENTED_EDGE('',*,*,#18804,.T.) ;
#26383 = ORIENTED_EDGE('',*,*,#17410,.T.) ;
#26384 = ORIENTED_EDGE('',*,*,#18805,.T.) ;
#26385 = ORIENTED_EDGE('',*,*,#17279,.F.) ;
#26386 = ORIENTED_EDGE('',*,*,#18806,.T.) ;
#26387 = ORIENTED_EDGE('',*,*,#17425,.T.) ;
#26388 = ORIENTED_EDGE('',*,*,#17256,.F.) ;
#26389 = ORIENTED_EDGE('',*,*,#18793,.F.) ;
#26390 = ORIENTED_EDGE('',*,*,#17326,.T.) ;
#26391 = ORIENTED_EDGE('',*,*,#18807,.F.) ;
#26392 = ORIENTED_EDGE('',*,*,#17254,.F.) ;
#26393 = ORIENTED_EDGE('',*,*,#18808,.F.) ;
#26394 = ORIENTED_EDGE('',*,*,#17328,.T.) ;
#26395 = ORIENTED_EDGE('',*,*,#18794,.F.) ;
#26396 = ORIENTED_EDGE('',*,*,#17270,.F.) ;
#26397 = ORIENTED_EDGE('',*,*,#18809,.F.) ;
#26398 = ORIENTED_EDGE('',*,*,#17394,.T.) ;
#26399 = ORIENTED_EDGE('',*,*,#18802,.F.) ;
#26400 = ORIENTED_EDGE('',*,*,#17272,.F.) ;
#26401 = ORIENTED_EDGE('',*,*,#18801,.F.) ;
#26402 = ORIENTED_EDGE('',*,*,#17396,.T.) ;
#26403 = ORIENTED_EDGE('',*,*,#18810,.F.) ;
#26404 = ORIENTED_EDGE('',*,*,#17274,.F.) ;
#26405 = ORIENTED_EDGE('',*,*,#18811,.F.) ;
#26406 = ORIENTED_EDGE('',*,*,#17411,.T.) ;
#26407 = ORIENTED_EDGE('',*,*,#18804,.F.) ;
#26408 = ORIENTED_EDGE('',*,*,#17276,.F.) ;
#26409 = ORIENTED_EDGE('',*,*,#18803,.F.) ;
#26410 = ORIENTED_EDGE('',*,*,#17413,.T.) ;
#26411 = ORIENTED_EDGE('',*,*,#18812,.F.) ;
#26412 = ORIENTED_EDGE('',*,*,#17260,.F.) ;
#26413 = ORIENTED_EDGE('',*,*,#18795,.F.) ;
#26414 = ORIENTED_EDGE('',*,*,#17343,.T.) ;
#26415 = ORIENTED_EDGE('',*,*,#18813,.F.) ;
#26416 = ORIENTED_EDGE('',*,*,#17258,.F.) ;
#26417 = ORIENTED_EDGE('',*,*,#18814,.F.) ;
#26418 = ORIENTED_EDGE('',*,*,#17345,.T.) ;
#26419 = ORIENTED_EDGE('',*,*,#18796,.F.) ;
#26420 = ORIENTED_EDGE('',*,*,#17252,.F.) ;
#26421 = ORIENTED_EDGE('',*,*,#18791,.F.) ;
#26422 = ORIENTED_EDGE('',*,*,#17309,.T.) ;
#26423 = ORIENTED_EDGE('',*,*,#18815,.F.) ;
#26424 = ORIENTED_EDGE('',*,*,#17250,.F.) ;
#26425 = ORIENTED_EDGE('',*,*,#18816,.F.) ;
#26426 = ORIENTED_EDGE('',*,*,#17311,.T.) ;
#26427 = ORIENTED_EDGE('',*,*,#18792,.F.) ;
#26428 = ORIENTED_EDGE('',*,*,#17266,.F.) ;
#26429 = ORIENTED_EDGE('',*,*,#18817,.F.) ;
#26430 = ORIENTED_EDGE('',*,*,#17377,.T.) ;
#26431 = ORIENTED_EDGE('',*,*,#18800,.F.) ;
#26432 = ORIENTED_EDGE('',*,*,#17268,.F.) ;
#26433 = ORIENTED_EDGE('',*,*,#18799,.F.) ;
#26434 = ORIENTED_EDGE('',*,*,#17379,.T.) ;
#26435 = ORIENTED_EDGE('',*,*,#18818,.F.) ;
#26436 = ORIENTED_EDGE('',*,*,#17278,.F.) ;
#26437 = ORIENTED_EDGE('',*,*,#18819,.F.) ;
#26438 = ORIENTED_EDGE('',*,*,#17426,.T.) ;
#26439 = ORIENTED_EDGE('',*,*,#18806,.F.) ;
#26440 = ORIENTED_EDGE('',*,*,#17280,.F.) ;
#26441 = ORIENTED_EDGE('',*,*,#18805,.F.) ;
#26442 = ORIENTED_EDGE('',*,*,#17428,.T.) ;
#26443 = ORIENTED_EDGE('',*,*,#18820,.F.) ;
#26444 = ORIENTED_EDGE('',*,*,#17262,.F.) ;
#26445 = ORIENTED_EDGE('',*,*,#18821,.F.) ;
#26446 = ORIENTED_EDGE('',*,*,#17360,.T.) ;
#26447 = ORIENTED_EDGE('',*,*,#18798,.F.) ;
#26448 = ORIENTED_EDGE('',*,*,#17264,.F.) ;
#26449 = ORIENTED_EDGE('',*,*,#18797,.F.) ;
#26450 = ORIENTED_EDGE('',*,*,#17362,.T.) ;
#26451 = ORIENTED_EDGE('',*,*,#18822,.F.) ;
#26452 = ORIENTED_EDGE('',*,*,#17248,.F.) ;
#26453 = ORIENTED_EDGE('',*,*,#18790,.F.) ;
#26454 = ORIENTED_EDGE('',*,*,#17292,.T.) ;
#26455 = ORIENTED_EDGE('',*,*,#18823,.F.) ;
#26456 = ORIENTED_EDGE('',*,*,#17246,.F.) ;
#26457 = ORIENTED_EDGE('',*,*,#18824,.F.) ;
#26458 = ORIENTED_EDGE('',*,*,#17294,.T.) ;
#26459 = ORIENTED_EDGE('',*,*,#18789,.F.) ;
#26460 = ORIENTED_EDGE('',*,*,#18825,.T.) ;
#26461 = ORIENTED_EDGE('',*,*,#18826,.F.) ;
#26462 = ORIENTED_EDGE('',*,*,#18827,.T.) ;
#26463 = ORIENTED_EDGE('',*,*,#18828,.F.) ;
#26464 = ORIENTED_EDGE('',*,*,#18829,.T.) ;
#26465 = ORIENTED_EDGE('',*,*,#18830,.F.) ;
#26466 = ORIENTED_EDGE('',*,*,#18831,.T.) ;
#26467 = ORIENTED_EDGE('',*,*,#18832,.F.) ;
#26468 = ORIENTED_EDGE('',*,*,#18833,.T.) ;
#26469 = ORIENTED_EDGE('',*,*,#18834,.F.) ;
#26470 = ORIENTED_EDGE('',*,*,#18835,.T.) ;
#26471 = ORIENTED_EDGE('',*,*,#18836,.F.) ;
#26472 = ORIENTED_EDGE('',*,*,#18837,.T.) ;
#26473 = ORIENTED_EDGE('',*,*,#18838,.F.) ;
#26474 = ORIENTED_EDGE('',*,*,#18839,.T.) ;
#26475 = ORIENTED_EDGE('',*,*,#18840,.F.) ;
#26476 = ORIENTED_EDGE('',*,*,#18841,.T.) ;
#26477 = ORIENTED_EDGE('',*,*,#18842,.F.) ;
#26478 = ORIENTED_EDGE('',*,*,#18843,.F.) ;
#26479 = ORIENTED_EDGE('',*,*,#18844,.F.) ;
#26480 = ORIENTED_EDGE('',*,*,#18845,.T.) ;
#26481 = ORIENTED_EDGE('',*,*,#18846,.F.) ;
#26482 = ORIENTED_EDGE('',*,*,#18847,.F.) ;
#26483 = ORIENTED_EDGE('',*,*,#18848,.F.) ;
#26484 = ORIENTED_EDGE('',*,*,#18849,.T.) ;
#26485 = ORIENTED_EDGE('',*,*,#18850,.F.) ;
#26486 = ORIENTED_EDGE('',*,*,#18851,.F.) ;
#26487 = ORIENTED_EDGE('',*,*,#18852,.F.) ;
#26488 = ORIENTED_EDGE('',*,*,#18853,.T.) ;
#26489 = ORIENTED_EDGE('',*,*,#18854,.F.) ;
#26490 = ORIENTED_EDGE('',*,*,#18855,.F.) ;
#26491 = ORIENTED_EDGE('',*,*,#18856,.F.) ;
#26492 = ORIENTED_EDGE('',*,*,#18857,.T.) ;
#26493 = ORIENTED_EDGE('',*,*,#18858,.F.) ;
#26494 = ORIENTED_EDGE('',*,*,#18859,.T.) ;
#26495 = ORIENTED_EDGE('',*,*,#18860,.F.) ;
#26496 = ORIENTED_EDGE('',*,*,#18861,.F.) ;
#26497 = ORIENTED_EDGE('',*,*,#18862,.F.) ;
#26498 = ORIENTED_EDGE('',*,*,#18863,.F.) ;
#26499 = ORIENTED_EDGE('',*,*,#18864,.F.) ;
#26500 = ORIENTED_EDGE('',*,*,#18826,.T.) ;
#26501 = ORIENTED_EDGE('',*,*,#18865,.T.) ;
#26502 = ORIENTED_EDGE('',*,*,#18866,.T.) ;
#26503 = ORIENTED_EDGE('',*,*,#18867,.T.) ;
#26504 = ORIENTED_EDGE('',*,*,#18825,.F.) ;
#26505 = ORIENTED_EDGE('',*,*,#18868,.F.) ;
#26506 = ORIENTED_EDGE('',*,*,#18319,.F.) ;
#26507 = ORIENTED_EDGE('',*,*,#18869,.F.) ;
#26508 = ORIENTED_EDGE('',*,*,#18870,.F.) ;
#26509 = ORIENTED_EDGE('',*,*,#18865,.F.) ;
#26510 = ORIENTED_EDGE('',*,*,#18871,.T.) ;
#26511 = ORIENTED_EDGE('',*,*,#18872,.T.) ;
#26512 = ORIENTED_EDGE('',*,*,#18830,.T.) ;
#26513 = ORIENTED_EDGE('',*,*,#18873,.T.) ;
#26514 = ORIENTED_EDGE('',*,*,#18834,.T.) ;
#26515 = ORIENTED_EDGE('',*,*,#18874,.T.) ;
#26516 = ORIENTED_EDGE('',*,*,#18875,.T.) ;
#26517 = ORIENTED_EDGE('',*,*,#18876,.T.) ;
#26518 = ORIENTED_EDGE('',*,*,#18838,.T.) ;
#26519 = ORIENTED_EDGE('',*,*,#18877,.T.) ;
#26520 = ORIENTED_EDGE('',*,*,#18878,.T.) ;
#26521 = ORIENTED_EDGE('',*,*,#18879,.T.) ;
#26522 = ORIENTED_EDGE('',*,*,#18880,.T.) ;
#26523 = ORIENTED_EDGE('',*,*,#18881,.T.) ;
#26524 = ORIENTED_EDGE('',*,*,#18842,.T.) ;
#26525 = ORIENTED_EDGE('',*,*,#18882,.T.) ;
#26526 = ORIENTED_EDGE('',*,*,#18883,.T.) ;
#26527 = ORIENTED_EDGE('',*,*,#18884,.T.) ;
#26528 = ORIENTED_EDGE('',*,*,#18846,.T.) ;
#26529 = ORIENTED_EDGE('',*,*,#18885,.T.) ;
#26530 = ORIENTED_EDGE('',*,*,#18886,.T.) ;
#26531 = ORIENTED_EDGE('',*,*,#18887,.T.) ;
#26532 = ORIENTED_EDGE('',*,*,#18850,.T.) ;
#26533 = ORIENTED_EDGE('',*,*,#18888,.T.) ;
#26534 = ORIENTED_EDGE('',*,*,#18854,.T.) ;
#26535 = ORIENTED_EDGE('',*,*,#18889,.T.) ;
#26536 = ORIENTED_EDGE('',*,*,#18890,.T.) ;
#26537 = ORIENTED_EDGE('',*,*,#18891,.T.) ;
#26538 = ORIENTED_EDGE('',*,*,#18892,.T.) ;
#26539 = ORIENTED_EDGE('',*,*,#18893,.T.) ;
#26540 = ORIENTED_EDGE('',*,*,#18858,.T.) ;
#26541 = ORIENTED_EDGE('',*,*,#18894,.T.) ;
#26542 = ORIENTED_EDGE('',*,*,#18863,.T.) ;
#26543 = ORIENTED_EDGE('',*,*,#18895,.F.) ;
#26544 = ORIENTED_EDGE('',*,*,#18896,.F.) ;
#26545 = ORIENTED_EDGE('',*,*,#18897,.F.) ;
#26546 = ORIENTED_EDGE('',*,*,#18321,.F.) ;
#26547 = ORIENTED_EDGE('',*,*,#18898,.F.) ;
#26548 = ORIENTED_EDGE('',*,*,#18899,.T.) ;
#26549 = ORIENTED_EDGE('',*,*,#18895,.T.) ;
#26550 = ORIENTED_EDGE('',*,*,#18862,.T.) ;
#26551 = ORIENTED_EDGE('',*,*,#18900,.T.) ;
#26552 = ORIENTED_EDGE('',*,*,#18897,.T.) ;
#26553 = ORIENTED_EDGE('',*,*,#18901,.T.) ;
#26554 = ORIENTED_EDGE('',*,*,#18869,.T.) ;
#26555 = ORIENTED_EDGE('',*,*,#18322,.T.) ;
#26556 = ORIENTED_EDGE('',*,*,#18902,.T.) ;
#26557 = ORIENTED_EDGE('',*,*,#18903,.T.) ;
#26558 = ORIENTED_EDGE('',*,*,#18904,.T.) ;
#26559 = ORIENTED_EDGE('',*,*,#18905,.T.) ;
#26560 = ORIENTED_EDGE('',*,*,#18906,.T.) ;
#26561 = ORIENTED_EDGE('',*,*,#18907,.T.) ;
#26562 = ORIENTED_EDGE('',*,*,#18908,.T.) ;
#26563 = ORIENTED_EDGE('',*,*,#18909,.T.) ;
#26564 = ORIENTED_EDGE('',*,*,#18910,.T.) ;
#26565 = ORIENTED_EDGE('',*,*,#18911,.T.) ;
#26566 = ORIENTED_EDGE('',*,*,#18912,.T.) ;
#26567 = ORIENTED_EDGE('',*,*,#18913,.T.) ;
#26568 = ORIENTED_EDGE('',*,*,#18914,.T.) ;
#26569 = ORIENTED_EDGE('',*,*,#18915,.T.) ;
#26570 = ORIENTED_EDGE('',*,*,#18916,.T.) ;
#26571 = ORIENTED_EDGE('',*,*,#18917,.T.) ;
#26572 = ORIENTED_EDGE('',*,*,#18918,.T.) ;
#26573 = ORIENTED_EDGE('',*,*,#18919,.T.) ;
#26574 = ORIENTED_EDGE('',*,*,#18920,.T.) ;
#26575 = ORIENTED_EDGE('',*,*,#18921,.T.) ;
#26576 = ORIENTED_EDGE('',*,*,#18922,.T.) ;
#26577 = ORIENTED_EDGE('',*,*,#18923,.T.) ;
#26578 = ORIENTED_EDGE('',*,*,#18924,.T.) ;
#26579 = ORIENTED_EDGE('',*,*,#18925,.T.) ;
#26580 = ORIENTED_EDGE('',*,*,#18926,.T.) ;
#26581 = ORIENTED_EDGE('',*,*,#18927,.T.) ;
#26582 = ORIENTED_EDGE('',*,*,#18928,.T.) ;
#26583 = ORIENTED_EDGE('',*,*,#18929,.T.) ;
#26584 = ORIENTED_EDGE('',*,*,#18930,.T.) ;
#26585 = ORIENTED_EDGE('',*,*,#18931,.T.) ;
#26586 = ORIENTED_EDGE('',*,*,#18932,.T.) ;
#26587 = ORIENTED_EDGE('',*,*,#18933,.T.) ;
#26588 = ORIENTED_EDGE('',*,*,#18934,.F.) ;
#26589 = ORIENTED_EDGE('',*,*,#18900,.F.) ;
#26590 = ORIENTED_EDGE('',*,*,#18861,.T.) ;
#26591 = ORIENTED_EDGE('',*,*,#18935,.F.) ;
#26592 = ORIENTED_EDGE('',*,*,#17282,.F.) ;
#26593 = ORIENTED_EDGE('',*,*,#18827,.F.) ;
#26594 = ORIENTED_EDGE('',*,*,#18867,.F.) ;
#26595 = ORIENTED_EDGE('',*,*,#18936,.F.) ;
#26596 = ORIENTED_EDGE('',*,*,#18902,.F.) ;
#26597 = ORIENTED_EDGE('',*,*,#18937,.F.) ;
#26598 = ORIENTED_EDGE('',*,*,#18938,.F.) ;
#26599 = ORIENTED_EDGE('',*,*,#18829,.F.) ;
#26600 = ORIENTED_EDGE('',*,*,#18939,.F.) ;
#26601 = ORIENTED_EDGE('',*,*,#18940,.F.) ;
#26602 = ORIENTED_EDGE('',*,*,#18904,.F.) ;
#26603 = ORIENTED_EDGE('',*,*,#18941,.F.) ;
#26604 = ORIENTED_EDGE('',*,*,#18873,.F.) ;
#26605 = ORIENTED_EDGE('',*,*,#18831,.F.) ;
#26606 = ORIENTED_EDGE('',*,*,#18872,.F.) ;
#26607 = ORIENTED_EDGE('',*,*,#18942,.F.) ;
#26608 = ORIENTED_EDGE('',*,*,#18906,.F.) ;
#26609 = ORIENTED_EDGE('',*,*,#18943,.F.) ;
#26610 = ORIENTED_EDGE('',*,*,#18944,.F.) ;
#26611 = ORIENTED_EDGE('',*,*,#18833,.F.) ;
#26612 = ORIENTED_EDGE('',*,*,#18945,.F.) ;
#26613 = ORIENTED_EDGE('',*,*,#18946,.F.) ;
#26614 = ORIENTED_EDGE('',*,*,#18908,.F.) ;
#26615 = ORIENTED_EDGE('',*,*,#18947,.F.) ;
#26616 = ORIENTED_EDGE('',*,*,#18874,.F.) ;
#26617 = ORIENTED_EDGE('',*,*,#18835,.F.) ;
#26618 = ORIENTED_EDGE('',*,*,#18876,.F.) ;
#26619 = ORIENTED_EDGE('',*,*,#18948,.F.) ;
#26620 = ORIENTED_EDGE('',*,*,#18910,.F.) ;
#26621 = ORIENTED_EDGE('',*,*,#18949,.F.) ;
#26622 = ORIENTED_EDGE('',*,*,#18950,.F.) ;
#26623 = ORIENTED_EDGE('',*,*,#18837,.F.) ;
#26624 = ORIENTED_EDGE('',*,*,#18951,.F.) ;
#26625 = ORIENTED_EDGE('',*,*,#18952,.F.) ;
#26626 = ORIENTED_EDGE('',*,*,#18912,.F.) ;
#26627 = ORIENTED_EDGE('',*,*,#18953,.F.) ;
#26628 = ORIENTED_EDGE('',*,*,#18877,.F.) ;
#26629 = ORIENTED_EDGE('',*,*,#18839,.F.) ;
#26630 = ORIENTED_EDGE('',*,*,#18879,.F.) ;
#26631 = ORIENTED_EDGE('',*,*,#18954,.F.) ;
#26632 = ORIENTED_EDGE('',*,*,#18914,.F.) ;
#26633 = ORIENTED_EDGE('',*,*,#18955,.F.) ;
#26634 = ORIENTED_EDGE('',*,*,#18956,.F.) ;
#26635 = ORIENTED_EDGE('',*,*,#18841,.F.) ;
#26636 = ORIENTED_EDGE('',*,*,#18957,.F.) ;
#26637 = ORIENTED_EDGE('',*,*,#18958,.F.) ;
#26638 = ORIENTED_EDGE('',*,*,#18916,.F.) ;
#26639 = ORIENTED_EDGE('',*,*,#18959,.F.) ;
#26640 = ORIENTED_EDGE('',*,*,#18882,.F.) ;
#26641 = ORIENTED_EDGE('',*,*,#18843,.T.) ;
#26642 = ORIENTED_EDGE('',*,*,#18881,.F.) ;
#26643 = ORIENTED_EDGE('',*,*,#18960,.F.) ;
#26644 = ORIENTED_EDGE('',*,*,#18918,.F.) ;
#26645 = ORIENTED_EDGE('',*,*,#18961,.F.) ;
#26646 = ORIENTED_EDGE('',*,*,#18962,.F.) ;
#26647 = ORIENTED_EDGE('',*,*,#18845,.F.) ;
#26648 = ORIENTED_EDGE('',*,*,#18963,.F.) ;
#26649 = ORIENTED_EDGE('',*,*,#18964,.F.) ;
#26650 = ORIENTED_EDGE('',*,*,#18920,.F.) ;
#26651 = ORIENTED_EDGE('',*,*,#18965,.F.) ;
#26652 = ORIENTED_EDGE('',*,*,#18885,.F.) ;
#26653 = ORIENTED_EDGE('',*,*,#18847,.T.) ;
#26654 = ORIENTED_EDGE('',*,*,#18884,.F.) ;
#26655 = ORIENTED_EDGE('',*,*,#18966,.F.) ;
#26656 = ORIENTED_EDGE('',*,*,#18922,.F.) ;
#26657 = ORIENTED_EDGE('',*,*,#18967,.F.) ;
#26658 = ORIENTED_EDGE('',*,*,#18968,.F.) ;
#26659 = ORIENTED_EDGE('',*,*,#18849,.F.) ;
#26660 = ORIENTED_EDGE('',*,*,#18969,.F.) ;
#26661 = ORIENTED_EDGE('',*,*,#18970,.F.) ;
#26662 = ORIENTED_EDGE('',*,*,#18924,.F.) ;
#26663 = ORIENTED_EDGE('',*,*,#18971,.F.) ;
#26664 = ORIENTED_EDGE('',*,*,#18888,.F.) ;
#26665 = ORIENTED_EDGE('',*,*,#18851,.T.) ;
#26666 = ORIENTED_EDGE('',*,*,#18887,.F.) ;
#26667 = ORIENTED_EDGE('',*,*,#18972,.F.) ;
#26668 = ORIENTED_EDGE('',*,*,#18926,.F.) ;
#26669 = ORIENTED_EDGE('',*,*,#18973,.F.) ;
#26670 = ORIENTED_EDGE('',*,*,#18974,.F.) ;
#26671 = ORIENTED_EDGE('',*,*,#18853,.F.) ;
#26672 = ORIENTED_EDGE('',*,*,#18975,.F.) ;
#26673 = ORIENTED_EDGE('',*,*,#18976,.F.) ;
#26674 = ORIENTED_EDGE('',*,*,#18928,.F.) ;
#26675 = ORIENTED_EDGE('',*,*,#18977,.F.) ;
#26676 = ORIENTED_EDGE('',*,*,#18889,.F.) ;
#26677 = ORIENTED_EDGE('',*,*,#18855,.T.) ;
#26678 = ORIENTED_EDGE('',*,*,#18891,.F.) ;
#26679 = ORIENTED_EDGE('',*,*,#18978,.F.) ;
#26680 = ORIENTED_EDGE('',*,*,#18930,.F.) ;
#26681 = ORIENTED_EDGE('',*,*,#18979,.F.) ;
#26682 = ORIENTED_EDGE('',*,*,#18980,.F.) ;
#26683 = ORIENTED_EDGE('',*,*,#18857,.F.) ;
#26684 = ORIENTED_EDGE('',*,*,#18981,.F.) ;
#26685 = ORIENTED_EDGE('',*,*,#18982,.F.) ;
#26686 = ORIENTED_EDGE('',*,*,#18932,.F.) ;
#26687 = ORIENTED_EDGE('',*,*,#18983,.F.) ;
#26688 = ORIENTED_EDGE('',*,*,#18894,.F.) ;
#26689 = ORIENTED_EDGE('',*,*,#18868,.T.) ;
#26690 = ORIENTED_EDGE('',*,*,#18864,.T.) ;
#26691 = ORIENTED_EDGE('',*,*,#18898,.T.) ;
#26692 = ORIENTED_EDGE('',*,*,#18320,.T.) ;
#26693 = ORIENTED_EDGE('',*,*,#17145,.T.) ;
#26694 = ORIENTED_EDGE('',*,*,#17285,.T.) ;
#26695 = ORIENTED_EDGE('',*,*,#17186,.T.) ;
#26696 = ORIENTED_EDGE('',*,*,#17182,.T.) ;
#26697 = ORIENTED_EDGE('',*,*,#17189,.T.) ;
#26698 = ORIENTED_EDGE('',*,*,#17284,.T.) ;
#26699 = ORIENTED_EDGE('',*,*,#17230,.T.) ;
#26700 = ORIENTED_EDGE('',*,*,#17226,.T.) ;
#26701 = ORIENTED_EDGE('',*,*,#17233,.T.) ;
#26702 = ORIENTED_EDGE('',*,*,#17283,.T.) ;
#26703 = ORIENTED_EDGE('',*,*,#18935,.T.) ;
#26704 = ORIENTED_EDGE('',*,*,#18860,.T.) ;
#26705 = ORIENTED_EDGE('',*,*,#18984,.T.) ;
#26706 = ORIENTED_EDGE('',*,*,#17243,.T.) ;
#26707 = ORIENTED_EDGE('',*,*,#17211,.T.) ;
#26708 = ORIENTED_EDGE('',*,*,#17208,.T.) ;
#26709 = ORIENTED_EDGE('',*,*,#17204,.T.) ;
#26710 = ORIENTED_EDGE('',*,*,#17242,.T.) ;
#26711 = ORIENTED_EDGE('',*,*,#17167,.T.) ;
#26712 = ORIENTED_EDGE('',*,*,#17164,.T.) ;
#26713 = ORIENTED_EDGE('',*,*,#17160,.T.) ;
#26714 = ORIENTED_EDGE('',*,*,#17241,.T.) ;
#26715 = ORIENTED_EDGE('',*,*,#17153,.T.) ;
#26716 = ORIENTED_EDGE('',*,*,#17149,.T.) ;
#26717 = ORIENTED_EDGE('',*,*,#17156,.T.) ;
#26718 = ORIENTED_EDGE('',*,*,#17240,.T.) ;
#26719 = ORIENTED_EDGE('',*,*,#17197,.T.) ;
#26720 = ORIENTED_EDGE('',*,*,#17193,.T.) ;
#26721 = ORIENTED_EDGE('',*,*,#17200,.T.) ;
#26722 = ORIENTED_EDGE('',*,*,#17239,.T.) ;
#26723 = ORIENTED_EDGE('',*,*,#17219,.T.) ;
#26724 = ORIENTED_EDGE('',*,*,#17215,.T.) ;
#26725 = ORIENTED_EDGE('',*,*,#17222,.T.) ;
#26726 = ORIENTED_EDGE('',*,*,#17238,.T.) ;
#26727 = ORIENTED_EDGE('',*,*,#17175,.T.) ;
#26728 = ORIENTED_EDGE('',*,*,#17171,.T.) ;
#26729 = ORIENTED_EDGE('',*,*,#17178,.T.) ;
#26730 = ORIENTED_EDGE('',*,*,#17237,.T.) ;
#26731 = ORIENTED_EDGE('',*,*,#17142,.T.) ;
#26732 = ORIENTED_EDGE('',*,*,#17138,.T.) ;
#26733 = ORIENTED_EDGE('',*,*,#18938,.T.) ;
#26734 = ORIENTED_EDGE('',*,*,#18985,.T.) ;
#26735 = ORIENTED_EDGE('',*,*,#18939,.T.) ;
#26736 = ORIENTED_EDGE('',*,*,#18828,.T.) ;
#26737 = ORIENTED_EDGE('',*,*,#18944,.T.) ;
#26738 = ORIENTED_EDGE('',*,*,#18986,.T.) ;
#26739 = ORIENTED_EDGE('',*,*,#18945,.T.) ;
#26740 = ORIENTED_EDGE('',*,*,#18832,.T.) ;
#26741 = ORIENTED_EDGE('',*,*,#18950,.T.) ;
#26742 = ORIENTED_EDGE('',*,*,#18987,.T.) ;
#26743 = ORIENTED_EDGE('',*,*,#18951,.T.) ;
#26744 = ORIENTED_EDGE('',*,*,#18836,.T.) ;
#26745 = ORIENTED_EDGE('',*,*,#18956,.T.) ;
#26746 = ORIENTED_EDGE('',*,*,#18988,.T.) ;
#26747 = ORIENTED_EDGE('',*,*,#18957,.T.) ;
#26748 = ORIENTED_EDGE('',*,*,#18840,.T.) ;
#26749 = ORIENTED_EDGE('',*,*,#18962,.T.) ;
#26750 = ORIENTED_EDGE('',*,*,#18989,.T.) ;
#26751 = ORIENTED_EDGE('',*,*,#18963,.T.) ;
#26752 = ORIENTED_EDGE('',*,*,#18844,.T.) ;
#26753 = ORIENTED_EDGE('',*,*,#18968,.T.) ;
#26754 = ORIENTED_EDGE('',*,*,#18990,.T.) ;
#26755 = ORIENTED_EDGE('',*,*,#18969,.T.) ;
#26756 = ORIENTED_EDGE('',*,*,#18848,.T.) ;
#26757 = ORIENTED_EDGE('',*,*,#18974,.T.) ;
#26758 = ORIENTED_EDGE('',*,*,#18991,.T.) ;
#26759 = ORIENTED_EDGE('',*,*,#18975,.T.) ;
#26760 = ORIENTED_EDGE('',*,*,#18852,.T.) ;
#26761 = ORIENTED_EDGE('',*,*,#18980,.T.) ;
#26762 = ORIENTED_EDGE('',*,*,#18992,.T.) ;
#26763 = ORIENTED_EDGE('',*,*,#18981,.T.) ;
#26764 = ORIENTED_EDGE('',*,*,#18856,.T.) ;
#26765 = ORIENTED_EDGE('',*,*,#18979,.T.) ;
#26766 = ORIENTED_EDGE('',*,*,#18933,.F.) ;
#26767 = ORIENTED_EDGE('',*,*,#18982,.T.) ;
#26768 = ORIENTED_EDGE('',*,*,#18992,.F.) ;
#26769 = ORIENTED_EDGE('',*,*,#17729,.T.) ;
#26770 = ORIENTED_EDGE('',*,*,#17731,.F.) ;
#26771 = ORIENTED_EDGE('',*,*,#17734,.T.) ;
#26772 = ORIENTED_EDGE('',*,*,#17737,.F.) ;
#26773 = ORIENTED_EDGE('',*,*,#17740,.T.) ;
#26774 = ORIENTED_EDGE('',*,*,#17743,.F.) ;
#26775 = ORIENTED_EDGE('',*,*,#17746,.T.) ;
#26776 = ORIENTED_EDGE('',*,*,#17748,.F.) ;
#26777 = ORIENTED_EDGE('',*,*,#17993,.T.) ;
#26778 = ORIENTED_EDGE('',*,*,#17995,.F.) ;
#26779 = ORIENTED_EDGE('',*,*,#17998,.T.) ;
#26780 = ORIENTED_EDGE('',*,*,#18001,.F.) ;
#26781 = ORIENTED_EDGE('',*,*,#18004,.T.) ;
#26782 = ORIENTED_EDGE('',*,*,#18007,.F.) ;
#26783 = ORIENTED_EDGE('',*,*,#18010,.T.) ;
#26784 = ORIENTED_EDGE('',*,*,#18011,.F.) ;
#26785 = ORIENTED_EDGE('',*,*,#18993,.T.) ;
#26786 = ORIENTED_EDGE('',*,*,#18994,.F.) ;
#26787 = ORIENTED_EDGE('',*,*,#18995,.F.) ;
#26788 = ORIENTED_EDGE('',*,*,#18996,.T.) ;
#26789 = ORIENTED_EDGE('',*,*,#18993,.F.) ;
#26790 = ORIENTED_EDGE('',*,*,#18996,.F.) ;
#26791 = ORIENTED_EDGE('',*,*,#18997,.T.) ;
#26792 = ORIENTED_EDGE('',*,*,#18998,.T.) ;
#26793 = ORIENTED_EDGE('',*,*,#18994,.T.) ;
#26794 = ORIENTED_EDGE('',*,*,#18995,.T.) ;
#26795 = ORIENTED_EDGE('',*,*,#18998,.F.) ;
#26796 = ORIENTED_EDGE('',*,*,#18997,.F.) ;
#26797 = ORIENTED_EDGE('',*,*,#18999,.T.) ;
#26798 = ORIENTED_EDGE('',*,*,#17439,.F.) ;
#26799 = ORIENTED_EDGE('',*,*,#18999,.F.) ;
#26800 = ORIENTED_EDGE('',*,*,#18005,.F.) ;
#26801 = ORIENTED_EDGE('',*,*,#18015,.F.) ;
#26802 = ORIENTED_EDGE('',*,*,#18744,.T.) ;
#26803 = ORIENTED_EDGE('',*,*,#19000,.T.) ;
#26804 = ORIENTED_EDGE('',*,*,#18008,.F.) ;
#26805 = ORIENTED_EDGE('',*,*,#19000,.F.) ;
#26806 = ORIENTED_EDGE('',*,*,#18768,.T.) ;
#26807 = ORIENTED_EDGE('',*,*,#17471,.F.) ;
#26808 = ORIENTED_EDGE('',*,*,#18973,.T.) ;
#26809 = ORIENTED_EDGE('',*,*,#18929,.F.) ;
#26810 = ORIENTED_EDGE('',*,*,#18976,.T.) ;
#26811 = ORIENTED_EDGE('',*,*,#18991,.F.) ;
#26812 = ORIENTED_EDGE('',*,*,#17762,.T.) ;
#26813 = ORIENTED_EDGE('',*,*,#17764,.F.) ;
#26814 = ORIENTED_EDGE('',*,*,#17767,.T.) ;
#26815 = ORIENTED_EDGE('',*,*,#17770,.F.) ;
#26816 = ORIENTED_EDGE('',*,*,#17773,.T.) ;
#26817 = ORIENTED_EDGE('',*,*,#17776,.F.) ;
#26818 = ORIENTED_EDGE('',*,*,#17779,.T.) ;
#26819 = ORIENTED_EDGE('',*,*,#17781,.F.) ;
#26820 = ORIENTED_EDGE('',*,*,#18030,.T.) ;
#26821 = ORIENTED_EDGE('',*,*,#18032,.F.) ;
#26822 = ORIENTED_EDGE('',*,*,#18035,.T.) ;
#26823 = ORIENTED_EDGE('',*,*,#18038,.F.) ;
#26824 = ORIENTED_EDGE('',*,*,#18041,.T.) ;
#26825 = ORIENTED_EDGE('',*,*,#18044,.F.) ;
#26826 = ORIENTED_EDGE('',*,*,#18047,.T.) ;
#26827 = ORIENTED_EDGE('',*,*,#18048,.F.) ;
#26828 = ORIENTED_EDGE('',*,*,#19001,.T.) ;
#26829 = ORIENTED_EDGE('',*,*,#19002,.F.) ;
#26830 = ORIENTED_EDGE('',*,*,#19003,.F.) ;
#26831 = ORIENTED_EDGE('',*,*,#19004,.T.) ;
#26832 = ORIENTED_EDGE('',*,*,#19001,.F.) ;
#26833 = ORIENTED_EDGE('',*,*,#19004,.F.) ;
#26834 = ORIENTED_EDGE('',*,*,#19005,.T.) ;
#26835 = ORIENTED_EDGE('',*,*,#19006,.T.) ;
#26836 = ORIENTED_EDGE('',*,*,#19002,.T.) ;
#26837 = ORIENTED_EDGE('',*,*,#19003,.T.) ;
#26838 = ORIENTED_EDGE('',*,*,#19006,.F.) ;
#26839 = ORIENTED_EDGE('',*,*,#19005,.F.) ;
#26840 = ORIENTED_EDGE('',*,*,#19007,.T.) ;
#26841 = ORIENTED_EDGE('',*,*,#17440,.F.) ;
#26842 = ORIENTED_EDGE('',*,*,#19007,.F.) ;
#26843 = ORIENTED_EDGE('',*,*,#18042,.F.) ;
#26844 = ORIENTED_EDGE('',*,*,#18052,.F.) ;
#26845 = ORIENTED_EDGE('',*,*,#18697,.T.) ;
#26846 = ORIENTED_EDGE('',*,*,#19008,.T.) ;
#26847 = ORIENTED_EDGE('',*,*,#18045,.F.) ;
#26848 = ORIENTED_EDGE('',*,*,#19008,.F.) ;
#26849 = ORIENTED_EDGE('',*,*,#18721,.T.) ;
#26850 = ORIENTED_EDGE('',*,*,#17502,.F.) ;
#26851 = ORIENTED_EDGE('',*,*,#18967,.T.) ;
#26852 = ORIENTED_EDGE('',*,*,#18925,.F.) ;
#26853 = ORIENTED_EDGE('',*,*,#18970,.T.) ;
#26854 = ORIENTED_EDGE('',*,*,#18990,.F.) ;
#26855 = ORIENTED_EDGE('',*,*,#17795,.T.) ;
#26856 = ORIENTED_EDGE('',*,*,#17797,.F.) ;
#26857 = ORIENTED_EDGE('',*,*,#17800,.T.) ;
#26858 = ORIENTED_EDGE('',*,*,#17803,.F.) ;
#26859 = ORIENTED_EDGE('',*,*,#17806,.T.) ;
#26860 = ORIENTED_EDGE('',*,*,#17809,.F.) ;
#26861 = ORIENTED_EDGE('',*,*,#17812,.T.) ;
#26862 = ORIENTED_EDGE('',*,*,#17814,.F.) ;
#26863 = ORIENTED_EDGE('',*,*,#18067,.T.) ;
#26864 = ORIENTED_EDGE('',*,*,#18069,.F.) ;
#26865 = ORIENTED_EDGE('',*,*,#18072,.T.) ;
#26866 = ORIENTED_EDGE('',*,*,#18075,.F.) ;
#26867 = ORIENTED_EDGE('',*,*,#18078,.T.) ;
#26868 = ORIENTED_EDGE('',*,*,#18081,.F.) ;
#26869 = ORIENTED_EDGE('',*,*,#18084,.T.) ;
#26870 = ORIENTED_EDGE('',*,*,#18085,.F.) ;
#26871 = ORIENTED_EDGE('',*,*,#19009,.T.) ;
#26872 = ORIENTED_EDGE('',*,*,#19010,.F.) ;
#26873 = ORIENTED_EDGE('',*,*,#19011,.F.) ;
#26874 = ORIENTED_EDGE('',*,*,#19012,.T.) ;
#26875 = ORIENTED_EDGE('',*,*,#19009,.F.) ;
#26876 = ORIENTED_EDGE('',*,*,#19012,.F.) ;
#26877 = ORIENTED_EDGE('',*,*,#19013,.T.) ;
#26878 = ORIENTED_EDGE('',*,*,#19014,.T.) ;
#26879 = ORIENTED_EDGE('',*,*,#19010,.T.) ;
#26880 = ORIENTED_EDGE('',*,*,#19011,.T.) ;
#26881 = ORIENTED_EDGE('',*,*,#19014,.F.) ;
#26882 = ORIENTED_EDGE('',*,*,#19013,.F.) ;
#26883 = ORIENTED_EDGE('',*,*,#19015,.T.) ;
#26884 = ORIENTED_EDGE('',*,*,#17441,.F.) ;
#26885 = ORIENTED_EDGE('',*,*,#19015,.F.) ;
#26886 = ORIENTED_EDGE('',*,*,#18079,.F.) ;
#26887 = ORIENTED_EDGE('',*,*,#18089,.F.) ;
#26888 = ORIENTED_EDGE('',*,*,#18650,.T.) ;
#26889 = ORIENTED_EDGE('',*,*,#19016,.T.) ;
#26890 = ORIENTED_EDGE('',*,*,#18082,.F.) ;
#26891 = ORIENTED_EDGE('',*,*,#19016,.F.) ;
#26892 = ORIENTED_EDGE('',*,*,#18674,.T.) ;
#26893 = ORIENTED_EDGE('',*,*,#17533,.F.) ;
#26894 = ORIENTED_EDGE('',*,*,#18961,.T.) ;
#26895 = ORIENTED_EDGE('',*,*,#18921,.F.) ;
#26896 = ORIENTED_EDGE('',*,*,#18964,.T.) ;
#26897 = ORIENTED_EDGE('',*,*,#18989,.F.) ;
#26898 = ORIENTED_EDGE('',*,*,#17828,.T.) ;
#26899 = ORIENTED_EDGE('',*,*,#17830,.F.) ;
#26900 = ORIENTED_EDGE('',*,*,#17833,.T.) ;
#26901 = ORIENTED_EDGE('',*,*,#17836,.F.) ;
#26902 = ORIENTED_EDGE('',*,*,#17839,.T.) ;
#26903 = ORIENTED_EDGE('',*,*,#17842,.F.) ;
#26904 = ORIENTED_EDGE('',*,*,#17845,.T.) ;
#26905 = ORIENTED_EDGE('',*,*,#17847,.F.) ;
#26906 = ORIENTED_EDGE('',*,*,#18104,.T.) ;
#26907 = ORIENTED_EDGE('',*,*,#18106,.F.) ;
#26908 = ORIENTED_EDGE('',*,*,#18109,.T.) ;
#26909 = ORIENTED_EDGE('',*,*,#18112,.F.) ;
#26910 = ORIENTED_EDGE('',*,*,#18115,.T.) ;
#26911 = ORIENTED_EDGE('',*,*,#18118,.F.) ;
#26912 = ORIENTED_EDGE('',*,*,#18121,.T.) ;
#26913 = ORIENTED_EDGE('',*,*,#18122,.F.) ;
#26914 = ORIENTED_EDGE('',*,*,#19017,.T.) ;
#26915 = ORIENTED_EDGE('',*,*,#19018,.F.) ;
#26916 = ORIENTED_EDGE('',*,*,#19019,.F.) ;
#26917 = ORIENTED_EDGE('',*,*,#19020,.T.) ;
#26918 = ORIENTED_EDGE('',*,*,#19017,.F.) ;
#26919 = ORIENTED_EDGE('',*,*,#19020,.F.) ;
#26920 = ORIENTED_EDGE('',*,*,#19021,.T.) ;
#26921 = ORIENTED_EDGE('',*,*,#19022,.T.) ;
#26922 = ORIENTED_EDGE('',*,*,#19018,.T.) ;
#26923 = ORIENTED_EDGE('',*,*,#19019,.T.) ;
#26924 = ORIENTED_EDGE('',*,*,#19022,.F.) ;
#26925 = ORIENTED_EDGE('',*,*,#19021,.F.) ;
#26926 = ORIENTED_EDGE('',*,*,#19023,.T.) ;
#26927 = ORIENTED_EDGE('',*,*,#17442,.F.) ;
#26928 = ORIENTED_EDGE('',*,*,#19023,.F.) ;
#26929 = ORIENTED_EDGE('',*,*,#18116,.F.) ;
#26930 = ORIENTED_EDGE('',*,*,#18126,.F.) ;
#26931 = ORIENTED_EDGE('',*,*,#18603,.T.) ;
#26932 = ORIENTED_EDGE('',*,*,#19024,.T.) ;
#26933 = ORIENTED_EDGE('',*,*,#18119,.F.) ;
#26934 = ORIENTED_EDGE('',*,*,#19024,.F.) ;
#26935 = ORIENTED_EDGE('',*,*,#18627,.T.) ;
#26936 = ORIENTED_EDGE('',*,*,#17564,.F.) ;
#26937 = ORIENTED_EDGE('',*,*,#18955,.T.) ;
#26938 = ORIENTED_EDGE('',*,*,#18917,.F.) ;
#26939 = ORIENTED_EDGE('',*,*,#18958,.T.) ;
#26940 = ORIENTED_EDGE('',*,*,#18988,.F.) ;
#26941 = ORIENTED_EDGE('',*,*,#17861,.T.) ;
#26942 = ORIENTED_EDGE('',*,*,#17863,.F.) ;
#26943 = ORIENTED_EDGE('',*,*,#17866,.T.) ;
#26944 = ORIENTED_EDGE('',*,*,#17869,.F.) ;
#26945 = ORIENTED_EDGE('',*,*,#17872,.T.) ;
#26946 = ORIENTED_EDGE('',*,*,#17875,.F.) ;
#26947 = ORIENTED_EDGE('',*,*,#17878,.T.) ;
#26948 = ORIENTED_EDGE('',*,*,#17880,.F.) ;
#26949 = ORIENTED_EDGE('',*,*,#18141,.T.) ;
#26950 = ORIENTED_EDGE('',*,*,#18143,.F.) ;
#26951 = ORIENTED_EDGE('',*,*,#18146,.T.) ;
#26952 = ORIENTED_EDGE('',*,*,#18149,.F.) ;
#26953 = ORIENTED_EDGE('',*,*,#18152,.T.) ;
#26954 = ORIENTED_EDGE('',*,*,#18155,.F.) ;
#26955 = ORIENTED_EDGE('',*,*,#18158,.T.) ;
#26956 = ORIENTED_EDGE('',*,*,#18159,.F.) ;
#26957 = ORIENTED_EDGE('',*,*,#19025,.T.) ;
#26958 = ORIENTED_EDGE('',*,*,#19026,.F.) ;
#26959 = ORIENTED_EDGE('',*,*,#19027,.F.) ;
#26960 = ORIENTED_EDGE('',*,*,#19028,.T.) ;
#26961 = ORIENTED_EDGE('',*,*,#19025,.F.) ;
#26962 = ORIENTED_EDGE('',*,*,#19028,.F.) ;
#26963 = ORIENTED_EDGE('',*,*,#19029,.T.) ;
#26964 = ORIENTED_EDGE('',*,*,#19030,.T.) ;
#26965 = ORIENTED_EDGE('',*,*,#19026,.T.) ;
#26966 = ORIENTED_EDGE('',*,*,#19027,.T.) ;
#26967 = ORIENTED_EDGE('',*,*,#19030,.F.) ;
#26968 = ORIENTED_EDGE('',*,*,#19029,.F.) ;
#26969 = ORIENTED_EDGE('',*,*,#19031,.T.) ;
#26970 = ORIENTED_EDGE('',*,*,#17443,.F.) ;
#26971 = ORIENTED_EDGE('',*,*,#19031,.F.) ;
#26972 = ORIENTED_EDGE('',*,*,#18153,.F.) ;
#26973 = ORIENTED_EDGE('',*,*,#18163,.F.) ;
#26974 = ORIENTED_EDGE('',*,*,#18556,.T.) ;
#26975 = ORIENTED_EDGE('',*,*,#19032,.T.) ;
#26976 = ORIENTED_EDGE('',*,*,#18156,.F.) ;
#26977 = ORIENTED_EDGE('',*,*,#19032,.F.) ;
#26978 = ORIENTED_EDGE('',*,*,#18580,.T.) ;
#26979 = ORIENTED_EDGE('',*,*,#17595,.F.) ;
#26980 = ORIENTED_EDGE('',*,*,#18949,.T.) ;
#26981 = ORIENTED_EDGE('',*,*,#18913,.F.) ;
#26982 = ORIENTED_EDGE('',*,*,#18952,.T.) ;
#26983 = ORIENTED_EDGE('',*,*,#18987,.F.) ;
#26984 = ORIENTED_EDGE('',*,*,#17894,.T.) ;
#26985 = ORIENTED_EDGE('',*,*,#17896,.F.) ;
#26986 = ORIENTED_EDGE('',*,*,#17899,.T.) ;
#26987 = ORIENTED_EDGE('',*,*,#17902,.F.) ;
#26988 = ORIENTED_EDGE('',*,*,#17905,.T.) ;
#26989 = ORIENTED_EDGE('',*,*,#17908,.F.) ;
#26990 = ORIENTED_EDGE('',*,*,#17911,.T.) ;
#26991 = ORIENTED_EDGE('',*,*,#17913,.F.) ;
#26992 = ORIENTED_EDGE('',*,*,#18178,.T.) ;
#26993 = ORIENTED_EDGE('',*,*,#18180,.F.) ;
#26994 = ORIENTED_EDGE('',*,*,#18183,.T.) ;
#26995 = ORIENTED_EDGE('',*,*,#18186,.F.) ;
#26996 = ORIENTED_EDGE('',*,*,#18189,.T.) ;
#26997 = ORIENTED_EDGE('',*,*,#18192,.F.) ;
#26998 = ORIENTED_EDGE('',*,*,#18195,.T.) ;
#26999 = ORIENTED_EDGE('',*,*,#18196,.F.) ;
#27000 = ORIENTED_EDGE('',*,*,#19033,.T.) ;
#27001 = ORIENTED_EDGE('',*,*,#19034,.F.) ;
#27002 = ORIENTED_EDGE('',*,*,#19035,.F.) ;
#27003 = ORIENTED_EDGE('',*,*,#19036,.T.) ;
#27004 = ORIENTED_EDGE('',*,*,#19033,.F.) ;
#27005 = ORIENTED_EDGE('',*,*,#19036,.F.) ;
#27006 = ORIENTED_EDGE('',*,*,#19037,.T.) ;
#27007 = ORIENTED_EDGE('',*,*,#19038,.T.) ;
#27008 = ORIENTED_EDGE('',*,*,#19034,.T.) ;
#27009 = ORIENTED_EDGE('',*,*,#19035,.T.) ;
#27010 = ORIENTED_EDGE('',*,*,#19038,.F.) ;
#27011 = ORIENTED_EDGE('',*,*,#19037,.F.) ;
#27012 = ORIENTED_EDGE('',*,*,#19039,.T.) ;
#27013 = ORIENTED_EDGE('',*,*,#17444,.F.) ;
#27014 = ORIENTED_EDGE('',*,*,#19039,.F.) ;
#27015 = ORIENTED_EDGE('',*,*,#18190,.F.) ;
#27016 = ORIENTED_EDGE('',*,*,#18200,.F.) ;
#27017 = ORIENTED_EDGE('',*,*,#18509,.T.) ;
#27018 = ORIENTED_EDGE('',*,*,#19040,.T.) ;
#27019 = ORIENTED_EDGE('',*,*,#18193,.F.) ;
#27020 = ORIENTED_EDGE('',*,*,#19040,.F.) ;
#27021 = ORIENTED_EDGE('',*,*,#18533,.T.) ;
#27022 = ORIENTED_EDGE('',*,*,#17626,.F.) ;
#27023 = ORIENTED_EDGE('',*,*,#18943,.T.) ;
#27024 = ORIENTED_EDGE('',*,*,#18909,.F.) ;
#27025 = ORIENTED_EDGE('',*,*,#18946,.T.) ;
#27026 = ORIENTED_EDGE('',*,*,#18986,.F.) ;
#27027 = ORIENTED_EDGE('',*,*,#17927,.T.) ;
#27028 = ORIENTED_EDGE('',*,*,#17929,.F.) ;
#27029 = ORIENTED_EDGE('',*,*,#17932,.T.) ;
#27030 = ORIENTED_EDGE('',*,*,#17935,.F.) ;
#27031 = ORIENTED_EDGE('',*,*,#17938,.T.) ;
#27032 = ORIENTED_EDGE('',*,*,#17941,.F.) ;
#27033 = ORIENTED_EDGE('',*,*,#17944,.T.) ;
#27034 = ORIENTED_EDGE('',*,*,#17946,.F.) ;
#27035 = ORIENTED_EDGE('',*,*,#18215,.T.) ;
#27036 = ORIENTED_EDGE('',*,*,#18217,.F.) ;
#27037 = ORIENTED_EDGE('',*,*,#18220,.T.) ;
#27038 = ORIENTED_EDGE('',*,*,#18223,.F.) ;
#27039 = ORIENTED_EDGE('',*,*,#18226,.T.) ;
#27040 = ORIENTED_EDGE('',*,*,#18229,.F.) ;
#27041 = ORIENTED_EDGE('',*,*,#18232,.T.) ;
#27042 = ORIENTED_EDGE('',*,*,#18233,.F.) ;
#27043 = ORIENTED_EDGE('',*,*,#19041,.T.) ;
#27044 = ORIENTED_EDGE('',*,*,#19042,.F.) ;
#27045 = ORIENTED_EDGE('',*,*,#19043,.F.) ;
#27046 = ORIENTED_EDGE('',*,*,#19044,.T.) ;
#27047 = ORIENTED_EDGE('',*,*,#19041,.F.) ;
#27048 = ORIENTED_EDGE('',*,*,#19044,.F.) ;
#27049 = ORIENTED_EDGE('',*,*,#19045,.T.) ;
#27050 = ORIENTED_EDGE('',*,*,#19046,.T.) ;
#27051 = ORIENTED_EDGE('',*,*,#19042,.T.) ;
#27052 = ORIENTED_EDGE('',*,*,#19043,.T.) ;
#27053 = ORIENTED_EDGE('',*,*,#19046,.F.) ;
#27054 = ORIENTED_EDGE('',*,*,#19045,.F.) ;
#27055 = ORIENTED_EDGE('',*,*,#19047,.T.) ;
#27056 = ORIENTED_EDGE('',*,*,#17445,.F.) ;
#27057 = ORIENTED_EDGE('',*,*,#19047,.F.) ;
#27058 = ORIENTED_EDGE('',*,*,#18227,.F.) ;
#27059 = ORIENTED_EDGE('',*,*,#18237,.F.) ;
#27060 = ORIENTED_EDGE('',*,*,#18462,.T.) ;
#27061 = ORIENTED_EDGE('',*,*,#19048,.T.) ;
#27062 = ORIENTED_EDGE('',*,*,#18230,.F.) ;
#27063 = ORIENTED_EDGE('',*,*,#19048,.F.) ;
#27064 = ORIENTED_EDGE('',*,*,#18486,.T.) ;
#27065 = ORIENTED_EDGE('',*,*,#17657,.F.) ;
#27066 = ORIENTED_EDGE('',*,*,#18937,.T.) ;
#27067 = ORIENTED_EDGE('',*,*,#18905,.F.) ;
#27068 = ORIENTED_EDGE('',*,*,#18940,.T.) ;
#27069 = ORIENTED_EDGE('',*,*,#18985,.F.) ;
#27070 = ORIENTED_EDGE('',*,*,#17960,.T.) ;
#27071 = ORIENTED_EDGE('',*,*,#17962,.F.) ;
#27072 = ORIENTED_EDGE('',*,*,#17965,.T.) ;
#27073 = ORIENTED_EDGE('',*,*,#17968,.F.) ;
#27074 = ORIENTED_EDGE('',*,*,#17971,.T.) ;
#27075 = ORIENTED_EDGE('',*,*,#17974,.F.) ;
#27076 = ORIENTED_EDGE('',*,*,#17977,.T.) ;
#27077 = ORIENTED_EDGE('',*,*,#17979,.F.) ;
#27078 = ORIENTED_EDGE('',*,*,#18252,.T.) ;
#27079 = ORIENTED_EDGE('',*,*,#18254,.F.) ;
#27080 = ORIENTED_EDGE('',*,*,#18257,.T.) ;
#27081 = ORIENTED_EDGE('',*,*,#18260,.F.) ;
#27082 = ORIENTED_EDGE('',*,*,#18263,.T.) ;
#27083 = ORIENTED_EDGE('',*,*,#18266,.F.) ;
#27084 = ORIENTED_EDGE('',*,*,#18269,.T.) ;
#27085 = ORIENTED_EDGE('',*,*,#18270,.F.) ;
#27086 = ORIENTED_EDGE('',*,*,#19049,.T.) ;
#27087 = ORIENTED_EDGE('',*,*,#19050,.F.) ;
#27088 = ORIENTED_EDGE('',*,*,#19051,.F.) ;
#27089 = ORIENTED_EDGE('',*,*,#19052,.T.) ;
#27090 = ORIENTED_EDGE('',*,*,#19049,.F.) ;
#27091 = ORIENTED_EDGE('',*,*,#19052,.F.) ;
#27092 = ORIENTED_EDGE('',*,*,#19053,.T.) ;
#27093 = ORIENTED_EDGE('',*,*,#19054,.T.) ;
#27094 = ORIENTED_EDGE('',*,*,#19050,.T.) ;
#27095 = ORIENTED_EDGE('',*,*,#19051,.T.) ;
#27096 = ORIENTED_EDGE('',*,*,#19054,.F.) ;
#27097 = ORIENTED_EDGE('',*,*,#19053,.F.) ;
#27098 = ORIENTED_EDGE('',*,*,#19055,.T.) ;
#27099 = ORIENTED_EDGE('',*,*,#17446,.F.) ;
#27100 = ORIENTED_EDGE('',*,*,#19055,.F.) ;
#27101 = ORIENTED_EDGE('',*,*,#18264,.F.) ;
#27102 = ORIENTED_EDGE('',*,*,#18274,.F.) ;
#27103 = ORIENTED_EDGE('',*,*,#18415,.T.) ;
#27104 = ORIENTED_EDGE('',*,*,#19056,.T.) ;
#27105 = ORIENTED_EDGE('',*,*,#18267,.F.) ;
#27106 = ORIENTED_EDGE('',*,*,#19056,.F.) ;
#27107 = ORIENTED_EDGE('',*,*,#18439,.T.) ;
#27108 = ORIENTED_EDGE('',*,*,#17688,.F.) ;
#27109 = ORIENTED_EDGE('',*,*,#19057,.F.) ;
#27110 = ORIENTED_EDGE('',*,*,#19058,.F.) ;
#27111 = ORIENTED_EDGE('',*,*,#19059,.T.) ;
#27112 = ORIENTED_EDGE('',*,*,#18331,.F.) ;
#27113 = ORIENTED_EDGE('',*,*,#19059,.F.) ;
#27114 = ORIENTED_EDGE('',*,*,#19060,.T.) ;
#27115 = ORIENTED_EDGE('',*,*,#19061,.T.) ;
#27116 = ORIENTED_EDGE('',*,*,#19057,.T.) ;
#27117 = ORIENTED_EDGE('',*,*,#19058,.T.) ;
#27118 = ORIENTED_EDGE('',*,*,#19061,.F.) ;
#27119 = ORIENTED_EDGE('',*,*,#19060,.F.) ;
#27120 = ORIENTED_EDGE('',*,*,#19062,.T.) ;
#27121 = ORIENTED_EDGE('',*,*,#18372,.F.) ;
#27122 = ORIENTED_EDGE('',*,*,#19062,.F.) ;
#27123 = ORIENTED_EDGE('',*,*,#18984,.F.) ;
#27124 = ORIENTED_EDGE('',*,*,#18859,.F.) ;
#27125 = ORIENTED_EDGE('',*,*,#18893,.F.) ;
#27126 = ORIENTED_EDGE('',*,*,#19063,.F.) ;
#27127 = ORIENTED_EDGE('',*,*,#17244,.T.) ;
#27128 = ORIENTED_EDGE('',*,*,#19063,.T.) ;
#27129 = ORIENTED_EDGE('',*,*,#18892,.F.) ;
#27130 = ORIENTED_EDGE('',*,*,#18983,.T.) ;
#27131 = ORIENTED_EDGE('',*,*,#18931,.F.) ;
#27132 = ORIENTED_EDGE('',*,*,#18978,.T.) ;
#27133 = ORIENTED_EDGE('',*,*,#18890,.F.) ;
#27134 = ORIENTED_EDGE('',*,*,#18977,.T.) ;
#27135 = ORIENTED_EDGE('',*,*,#18927,.F.) ;
#27136 = ORIENTED_EDGE('',*,*,#18972,.T.) ;
#27137 = ORIENTED_EDGE('',*,*,#18886,.F.) ;
#27138 = ORIENTED_EDGE('',*,*,#18971,.T.) ;
#27139 = ORIENTED_EDGE('',*,*,#18923,.F.) ;
#27140 = ORIENTED_EDGE('',*,*,#18966,.T.) ;
#27141 = ORIENTED_EDGE('',*,*,#18883,.F.) ;
#27142 = ORIENTED_EDGE('',*,*,#18965,.T.) ;
#27143 = ORIENTED_EDGE('',*,*,#18919,.F.) ;
#27144 = ORIENTED_EDGE('',*,*,#18960,.T.) ;
#27145 = ORIENTED_EDGE('',*,*,#18880,.F.) ;
#27146 = ORIENTED_EDGE('',*,*,#18959,.T.) ;
#27147 = ORIENTED_EDGE('',*,*,#18915,.F.) ;
#27148 = ORIENTED_EDGE('',*,*,#18954,.T.) ;
#27149 = ORIENTED_EDGE('',*,*,#18878,.F.) ;
#27150 = ORIENTED_EDGE('',*,*,#18953,.T.) ;
#27151 = ORIENTED_EDGE('',*,*,#18911,.F.) ;
#27152 = ORIENTED_EDGE('',*,*,#18948,.T.) ;
#27153 = ORIENTED_EDGE('',*,*,#18875,.F.) ;
#27154 = ORIENTED_EDGE('',*,*,#18947,.T.) ;
#27155 = ORIENTED_EDGE('',*,*,#18907,.F.) ;
#27156 = ORIENTED_EDGE('',*,*,#18942,.T.) ;
#27157 = ORIENTED_EDGE('',*,*,#18871,.F.) ;
#27158 = ORIENTED_EDGE('',*,*,#18941,.T.) ;
#27159 = ORIENTED_EDGE('',*,*,#18903,.F.) ;
#27160 = ORIENTED_EDGE('',*,*,#18936,.T.) ;
#27161 = ORIENTED_EDGE('',*,*,#18866,.F.) ;
#27162 = ORIENTED_EDGE('',*,*,#18870,.T.) ;
#27163 = ORIENTED_EDGE('',*,*,#18901,.F.) ;
#27164 = ORIENTED_EDGE('',*,*,#18896,.T.) ;
#27165 = ORIENTED_EDGE('',*,*,#18899,.F.) ;
#27166 = ORIENTED_EDGE('',*,*,#18934,.T.) ;
#27167 = ORIENTED_EDGE('',*,*,#17281,.F.) ;
#27168 = ORIENTED_EDGE('',*,*,#18820,.T.) ;
#27169 = ORIENTED_EDGE('',*,*,#17427,.T.) ;
#27170 = ORIENTED_EDGE('',*,*,#18819,.T.) ;
#27171 = ORIENTED_EDGE('',*,*,#17277,.F.) ;
#27172 = ORIENTED_EDGE('',*,*,#18812,.T.) ;
#27173 = ORIENTED_EDGE('',*,*,#17412,.T.) ;
#27174 = ORIENTED_EDGE('',*,*,#18811,.T.) ;
#27175 = ORIENTED_EDGE('',*,*,#17273,.F.) ;
#27176 = ORIENTED_EDGE('',*,*,#18810,.T.) ;
#27177 = ORIENTED_EDGE('',*,*,#17395,.T.) ;
#27178 = ORIENTED_EDGE('',*,*,#18809,.T.) ;
#27179 = ORIENTED_EDGE('',*,*,#17269,.F.) ;
#27180 = ORIENTED_EDGE('',*,*,#18818,.T.) ;
#27181 = ORIENTED_EDGE('',*,*,#17378,.T.) ;
#27182 = ORIENTED_EDGE('',*,*,#18817,.T.) ;
#27183 = ORIENTED_EDGE('',*,*,#17265,.F.) ;
#27184 = ORIENTED_EDGE('',*,*,#18822,.T.) ;
#27185 = ORIENTED_EDGE('',*,*,#17361,.T.) ;
#27186 = ORIENTED_EDGE('',*,*,#18821,.T.) ;
#27187 = ORIENTED_EDGE('',*,*,#17261,.F.) ;
#27188 = ORIENTED_EDGE('',*,*,#18813,.T.) ;
#27189 = ORIENTED_EDGE('',*,*,#17342,.T.) ;
#27190 = ORIENTED_EDGE('',*,*,#18814,.T.) ;
#27191 = ORIENTED_EDGE('',*,*,#17257,.F.) ;
#27192 = ORIENTED_EDGE('',*,*,#18807,.T.) ;
#27193 = ORIENTED_EDGE('',*,*,#17325,.T.) ;
#27194 = ORIENTED_EDGE('',*,*,#18808,.T.) ;
#27195 = ORIENTED_EDGE('',*,*,#17253,.F.) ;
#27196 = ORIENTED_EDGE('',*,*,#18815,.T.) ;
#27197 = ORIENTED_EDGE('',*,*,#17308,.T.) ;
#27198 = ORIENTED_EDGE('',*,*,#18816,.T.) ;
#27199 = ORIENTED_EDGE('',*,*,#17249,.F.) ;
#27200 = ORIENTED_EDGE('',*,*,#18823,.T.) ;
#27201 = ORIENTED_EDGE('',*,*,#17291,.T.) ;
#27202 = ORIENTED_EDGE('',*,*,#18824,.T.) ;
#27203 = ORIENTED_EDGE('',*,*,#17245,.F.) ;
#27204 = ORIENTED_EDGE('',*,*,#17749,.T.) ;
#27205 = ORIENTED_EDGE('',*,*,#19064,.F.) ;
#27206 = ORIENTED_EDGE('',*,*,#18782,.T.) ;
#27207 = ORIENTED_EDGE('',*,*,#17757,.F.) ;
#27208 = ORIENTED_EDGE('',*,*,#17747,.F.) ;
#27209 = ORIENTED_EDGE('',*,*,#19065,.T.) ;
#27210 = ORIENTED_EDGE('',*,*,#18783,.T.) ;
#27211 = ORIENTED_EDGE('',*,*,#19064,.T.) ;
#27212 = ORIENTED_EDGE('',*,*,#17744,.F.) ;
#27213 = ORIENTED_EDGE('',*,*,#19066,.F.) ;
#27214 = ORIENTED_EDGE('',*,*,#18779,.T.) ;
#27215 = ORIENTED_EDGE('',*,*,#19065,.F.) ;
#27216 = ORIENTED_EDGE('',*,*,#17741,.F.) ;
#27217 = ORIENTED_EDGE('',*,*,#17752,.T.) ;
#27218 = ORIENTED_EDGE('',*,*,#18785,.T.) ;
#27219 = ORIENTED_EDGE('',*,*,#19066,.T.) ;
#27220 = ORIENTED_EDGE('',*,*,#18012,.T.) ;
#27221 = ORIENTED_EDGE('',*,*,#17469,.F.) ;
#27222 = ORIENTED_EDGE('',*,*,#18772,.T.) ;
#27223 = ORIENTED_EDGE('',*,*,#18025,.F.) ;
#27224 = ORIENTED_EDGE('',*,*,#17782,.T.) ;
#27225 = ORIENTED_EDGE('',*,*,#19067,.F.) ;
#27226 = ORIENTED_EDGE('',*,*,#18735,.T.) ;
#27227 = ORIENTED_EDGE('',*,*,#17790,.F.) ;
#27228 = ORIENTED_EDGE('',*,*,#17780,.F.) ;
#27229 = ORIENTED_EDGE('',*,*,#19068,.T.) ;
#27230 = ORIENTED_EDGE('',*,*,#18736,.T.) ;
#27231 = ORIENTED_EDGE('',*,*,#19067,.T.) ;
#27232 = ORIENTED_EDGE('',*,*,#17777,.F.) ;
#27233 = ORIENTED_EDGE('',*,*,#19069,.F.) ;
#27234 = ORIENTED_EDGE('',*,*,#18732,.T.) ;
#27235 = ORIENTED_EDGE('',*,*,#19068,.F.) ;
#27236 = ORIENTED_EDGE('',*,*,#17774,.F.) ;
#27237 = ORIENTED_EDGE('',*,*,#17785,.T.) ;
#27238 = ORIENTED_EDGE('',*,*,#18738,.T.) ;
#27239 = ORIENTED_EDGE('',*,*,#19069,.T.) ;
#27240 = ORIENTED_EDGE('',*,*,#18049,.T.) ;
#27241 = ORIENTED_EDGE('',*,*,#17500,.F.) ;
#27242 = ORIENTED_EDGE('',*,*,#18725,.T.) ;
#27243 = ORIENTED_EDGE('',*,*,#18062,.F.) ;
#27244 = ORIENTED_EDGE('',*,*,#17815,.T.) ;
#27245 = ORIENTED_EDGE('',*,*,#19070,.F.) ;
#27246 = ORIENTED_EDGE('',*,*,#18688,.T.) ;
#27247 = ORIENTED_EDGE('',*,*,#17823,.F.) ;
#27248 = ORIENTED_EDGE('',*,*,#17813,.F.) ;
#27249 = ORIENTED_EDGE('',*,*,#19071,.T.) ;
#27250 = ORIENTED_EDGE('',*,*,#18689,.T.) ;
#27251 = ORIENTED_EDGE('',*,*,#19070,.T.) ;
#27252 = ORIENTED_EDGE('',*,*,#17810,.F.) ;
#27253 = ORIENTED_EDGE('',*,*,#19072,.F.) ;
#27254 = ORIENTED_EDGE('',*,*,#18685,.T.) ;
#27255 = ORIENTED_EDGE('',*,*,#19071,.F.) ;
#27256 = ORIENTED_EDGE('',*,*,#17807,.F.) ;
#27257 = ORIENTED_EDGE('',*,*,#17818,.T.) ;
#27258 = ORIENTED_EDGE('',*,*,#18691,.T.) ;
#27259 = ORIENTED_EDGE('',*,*,#19072,.T.) ;
#27260 = ORIENTED_EDGE('',*,*,#18086,.T.) ;
#27261 = ORIENTED_EDGE('',*,*,#17531,.F.) ;
#27262 = ORIENTED_EDGE('',*,*,#18678,.T.) ;
#27263 = ORIENTED_EDGE('',*,*,#18099,.F.) ;
#27264 = ORIENTED_EDGE('',*,*,#17848,.T.) ;
#27265 = ORIENTED_EDGE('',*,*,#19073,.F.) ;
#27266 = ORIENTED_EDGE('',*,*,#18641,.T.) ;
#27267 = ORIENTED_EDGE('',*,*,#17856,.F.) ;
#27268 = ORIENTED_EDGE('',*,*,#17846,.F.) ;
#27269 = ORIENTED_EDGE('',*,*,#19074,.T.) ;
#27270 = ORIENTED_EDGE('',*,*,#18642,.T.) ;
#27271 = ORIENTED_EDGE('',*,*,#19073,.T.) ;
#27272 = ORIENTED_EDGE('',*,*,#17843,.F.) ;
#27273 = ORIENTED_EDGE('',*,*,#19075,.F.) ;
#27274 = ORIENTED_EDGE('',*,*,#18638,.T.) ;
#27275 = ORIENTED_EDGE('',*,*,#19074,.F.) ;
#27276 = ORIENTED_EDGE('',*,*,#17840,.F.) ;
#27277 = ORIENTED_EDGE('',*,*,#17851,.T.) ;
#27278 = ORIENTED_EDGE('',*,*,#18644,.T.) ;
#27279 = ORIENTED_EDGE('',*,*,#19075,.T.) ;
#27280 = ORIENTED_EDGE('',*,*,#18123,.T.) ;
#27281 = ORIENTED_EDGE('',*,*,#17562,.F.) ;
#27282 = ORIENTED_EDGE('',*,*,#18631,.T.) ;
#27283 = ORIENTED_EDGE('',*,*,#18136,.F.) ;
#27284 = ORIENTED_EDGE('',*,*,#17881,.T.) ;
#27285 = ORIENTED_EDGE('',*,*,#19076,.F.) ;
#27286 = ORIENTED_EDGE('',*,*,#18594,.T.) ;
#27287 = ORIENTED_EDGE('',*,*,#17889,.F.) ;
#27288 = ORIENTED_EDGE('',*,*,#17879,.F.) ;
#27289 = ORIENTED_EDGE('',*,*,#19077,.T.) ;
#27290 = ORIENTED_EDGE('',*,*,#18595,.T.) ;
#27291 = ORIENTED_EDGE('',*,*,#19076,.T.) ;
#27292 = ORIENTED_EDGE('',*,*,#17876,.F.) ;
#27293 = ORIENTED_EDGE('',*,*,#19078,.F.) ;
#27294 = ORIENTED_EDGE('',*,*,#18591,.T.) ;
#27295 = ORIENTED_EDGE('',*,*,#19077,.F.) ;
#27296 = ORIENTED_EDGE('',*,*,#17873,.F.) ;
#27297 = ORIENTED_EDGE('',*,*,#17884,.T.) ;
#27298 = ORIENTED_EDGE('',*,*,#18597,.T.) ;
#27299 = ORIENTED_EDGE('',*,*,#19078,.T.) ;
#27300 = ORIENTED_EDGE('',*,*,#18160,.T.) ;
#27301 = ORIENTED_EDGE('',*,*,#17593,.F.) ;
#27302 = ORIENTED_EDGE('',*,*,#18584,.T.) ;
#27303 = ORIENTED_EDGE('',*,*,#18173,.F.) ;
#27304 = ORIENTED_EDGE('',*,*,#17914,.T.) ;
#27305 = ORIENTED_EDGE('',*,*,#19079,.F.) ;
#27306 = ORIENTED_EDGE('',*,*,#18547,.T.) ;
#27307 = ORIENTED_EDGE('',*,*,#17922,.F.) ;
#27308 = ORIENTED_EDGE('',*,*,#17912,.F.) ;
#27309 = ORIENTED_EDGE('',*,*,#19080,.T.) ;
#27310 = ORIENTED_EDGE('',*,*,#18548,.T.) ;
#27311 = ORIENTED_EDGE('',*,*,#19079,.T.) ;
#27312 = ORIENTED_EDGE('',*,*,#17909,.F.) ;
#27313 = ORIENTED_EDGE('',*,*,#19081,.F.) ;
#27314 = ORIENTED_EDGE('',*,*,#18544,.T.) ;
#27315 = ORIENTED_EDGE('',*,*,#19080,.F.) ;
#27316 = ORIENTED_EDGE('',*,*,#17906,.F.) ;
#27317 = ORIENTED_EDGE('',*,*,#17917,.T.) ;
#27318 = ORIENTED_EDGE('',*,*,#18550,.T.) ;
#27319 = ORIENTED_EDGE('',*,*,#19081,.T.) ;
#27320 = ORIENTED_EDGE('',*,*,#18197,.T.) ;
#27321 = ORIENTED_EDGE('',*,*,#17624,.F.) ;
#27322 = ORIENTED_EDGE('',*,*,#18537,.T.) ;
#27323 = ORIENTED_EDGE('',*,*,#18210,.F.) ;
#27324 = ORIENTED_EDGE('',*,*,#17947,.T.) ;
#27325 = ORIENTED_EDGE('',*,*,#19082,.F.) ;
#27326 = ORIENTED_EDGE('',*,*,#18500,.T.) ;
#27327 = ORIENTED_EDGE('',*,*,#17955,.F.) ;
#27328 = ORIENTED_EDGE('',*,*,#17945,.F.) ;
#27329 = ORIENTED_EDGE('',*,*,#19083,.T.) ;
#27330 = ORIENTED_EDGE('',*,*,#18501,.T.) ;
#27331 = ORIENTED_EDGE('',*,*,#19082,.T.) ;
#27332 = ORIENTED_EDGE('',*,*,#17942,.F.) ;
#27333 = ORIENTED_EDGE('',*,*,#19084,.F.) ;
#27334 = ORIENTED_EDGE('',*,*,#18497,.T.) ;
#27335 = ORIENTED_EDGE('',*,*,#19083,.F.) ;
#27336 = ORIENTED_EDGE('',*,*,#17939,.F.) ;
#27337 = ORIENTED_EDGE('',*,*,#17950,.T.) ;
#27338 = ORIENTED_EDGE('',*,*,#18503,.T.) ;
#27339 = ORIENTED_EDGE('',*,*,#19084,.T.) ;
#27340 = ORIENTED_EDGE('',*,*,#18234,.T.) ;
#27341 = ORIENTED_EDGE('',*,*,#17655,.F.) ;
#27342 = ORIENTED_EDGE('',*,*,#18490,.T.) ;
#27343 = ORIENTED_EDGE('',*,*,#18247,.F.) ;
#27344 = ORIENTED_EDGE('',*,*,#17980,.T.) ;
#27345 = ORIENTED_EDGE('',*,*,#19085,.F.) ;
#27346 = ORIENTED_EDGE('',*,*,#18453,.T.) ;
#27347 = ORIENTED_EDGE('',*,*,#17988,.F.) ;
#27348 = ORIENTED_EDGE('',*,*,#17978,.F.) ;
#27349 = ORIENTED_EDGE('',*,*,#19086,.T.) ;
#27350 = ORIENTED_EDGE('',*,*,#18454,.T.) ;
#27351 = ORIENTED_EDGE('',*,*,#19085,.T.) ;
#27352 = ORIENTED_EDGE('',*,*,#17975,.F.) ;
#27353 = ORIENTED_EDGE('',*,*,#19087,.F.) ;
#27354 = ORIENTED_EDGE('',*,*,#18450,.T.) ;
#27355 = ORIENTED_EDGE('',*,*,#19086,.F.) ;
#27356 = ORIENTED_EDGE('',*,*,#17972,.F.) ;
#27357 = ORIENTED_EDGE('',*,*,#17983,.T.) ;
#27358 = ORIENTED_EDGE('',*,*,#18456,.T.) ;
#27359 = ORIENTED_EDGE('',*,*,#19087,.T.) ;
#27360 = ORIENTED_EDGE('',*,*,#18271,.T.) ;
#27361 = ORIENTED_EDGE('',*,*,#17686,.F.) ;
#27362 = ORIENTED_EDGE('',*,*,#18443,.T.) ;
#27363 = ORIENTED_EDGE('',*,*,#18284,.F.) ;
#27364 = ORIENTED_EDGE('',*,*,#19088,.F.) ;
#27365 = ORIENTED_EDGE('',*,*,#19089,.T.) ;
#27366 = ORIENTED_EDGE('',*,*,#19090,.T.) ;
#27367 = ORIENTED_EDGE('',*,*,#19091,.F.) ;
#27368 = ORIENTED_EDGE('',*,*,#19092,.F.) ;
#27369 = ORIENTED_EDGE('',*,*,#19093,.T.) ;
#27370 = ORIENTED_EDGE('',*,*,#19088,.T.) ;
#27371 = ORIENTED_EDGE('',*,*,#19094,.F.) ;
#27372 = ORIENTED_EDGE('',*,*,#19095,.F.) ;
#27373 = ORIENTED_EDGE('',*,*,#19096,.T.) ;
#27374 = ORIENTED_EDGE('',*,*,#19092,.T.) ;
#27375 = ORIENTED_EDGE('',*,*,#19097,.F.) ;
#27376 = ORIENTED_EDGE('',*,*,#19098,.F.) ;
#27377 = ORIENTED_EDGE('',*,*,#19099,.T.) ;
#27378 = ORIENTED_EDGE('',*,*,#19095,.T.) ;
#27379 = ORIENTED_EDGE('',*,*,#19100,.F.) ;
#27380 = ORIENTED_EDGE('',*,*,#19101,.F.) ;
#27381 = ORIENTED_EDGE('',*,*,#19102,.T.) ;
#27382 = ORIENTED_EDGE('',*,*,#19098,.T.) ;
#27383 = ORIENTED_EDGE('',*,*,#19103,.F.) ;
#27384 = ORIENTED_EDGE('',*,*,#19104,.F.) ;
#27385 = ORIENTED_EDGE('',*,*,#19105,.T.) ;
#27386 = ORIENTED_EDGE('',*,*,#19101,.T.) ;
#27387 = ORIENTED_EDGE('',*,*,#19106,.F.) ;
#27388 = ORIENTED_EDGE('',*,*,#19107,.F.) ;
#27389 = ORIENTED_EDGE('',*,*,#19108,.T.) ;
#27390 = ORIENTED_EDGE('',*,*,#19104,.T.) ;
#27391 = ORIENTED_EDGE('',*,*,#19109,.F.) ;
#27392 = ORIENTED_EDGE('',*,*,#19110,.F.) ;
#27393 = ORIENTED_EDGE('',*,*,#19111,.F.) ;
#27394 = ORIENTED_EDGE('',*,*,#19112,.T.) ;
#27395 = ORIENTED_EDGE('',*,*,#19107,.T.) ;
#27396 = ORIENTED_EDGE('',*,*,#19113,.F.) ;
#27397 = ORIENTED_EDGE('',*,*,#19114,.F.) ;
#27398 = ORIENTED_EDGE('',*,*,#19115,.F.) ;
#27399 = ORIENTED_EDGE('',*,*,#19116,.T.) ;
#27400 = ORIENTED_EDGE('',*,*,#19117,.T.) ;
#27401 = ORIENTED_EDGE('',*,*,#19118,.F.) ;
#27402 = ORIENTED_EDGE('',*,*,#19119,.F.) ;
#27403 = ORIENTED_EDGE('',*,*,#19114,.T.) ;
#27404 = ORIENTED_EDGE('',*,*,#19120,.T.) ;
#27405 = ORIENTED_EDGE('',*,*,#19121,.F.) ;
#27406 = ORIENTED_EDGE('',*,*,#19122,.F.) ;
#27407 = ORIENTED_EDGE('',*,*,#19118,.T.) ;
#27408 = ORIENTED_EDGE('',*,*,#19123,.T.) ;
#27409 = ORIENTED_EDGE('',*,*,#19124,.F.) ;
#27410 = ORIENTED_EDGE('',*,*,#19125,.F.) ;
#27411 = ORIENTED_EDGE('',*,*,#19121,.T.) ;
#27412 = ORIENTED_EDGE('',*,*,#19126,.T.) ;
#27413 = ORIENTED_EDGE('',*,*,#19127,.F.) ;
#27414 = ORIENTED_EDGE('',*,*,#19128,.F.) ;
#27415 = ORIENTED_EDGE('',*,*,#19124,.T.) ;
#27416 = ORIENTED_EDGE('',*,*,#19129,.T.) ;
#27417 = ORIENTED_EDGE('',*,*,#19130,.F.) ;
#27418 = ORIENTED_EDGE('',*,*,#19131,.F.) ;
#27419 = ORIENTED_EDGE('',*,*,#19127,.T.) ;
#27420 = ORIENTED_EDGE('',*,*,#19132,.T.) ;
#27421 = ORIENTED_EDGE('',*,*,#19133,.F.) ;
#27422 = ORIENTED_EDGE('',*,*,#19134,.F.) ;
#27423 = ORIENTED_EDGE('',*,*,#19130,.T.) ;
#27424 = ORIENTED_EDGE('',*,*,#19135,.T.) ;
#27425 = ORIENTED_EDGE('',*,*,#19133,.T.) ;
#27426 = ORIENTED_EDGE('',*,*,#19136,.T.) ;
#27427 = ORIENTED_EDGE('',*,*,#19137,.F.) ;
#27428 = ORIENTED_EDGE('',*,*,#19138,.F.) ;
#27429 = ORIENTED_EDGE('',*,*,#19139,.F.) ;
#27430 = ORIENTED_EDGE('',*,*,#19110,.T.) ;
#27431 = ORIENTED_EDGE('',*,*,#19140,.F.) ;
#27432 = ORIENTED_EDGE('',*,*,#19141,.F.) ;
#27433 = ORIENTED_EDGE('',*,*,#19142,.T.) ;
#27434 = ORIENTED_EDGE('',*,*,#19143,.T.) ;
#27435 = ORIENTED_EDGE('',*,*,#19144,.T.) ;
#27436 = ORIENTED_EDGE('',*,*,#19142,.F.) ;
#27437 = ORIENTED_EDGE('',*,*,#19145,.T.) ;
#27438 = ORIENTED_EDGE('',*,*,#19146,.T.) ;
#27439 = ORIENTED_EDGE('',*,*,#19147,.T.) ;
#27440 = ORIENTED_EDGE('',*,*,#19148,.T.) ;
#27441 = ORIENTED_EDGE('',*,*,#19149,.T.) ;
#27442 = ORIENTED_EDGE('',*,*,#19146,.F.) ;
#27443 = ORIENTED_EDGE('',*,*,#19150,.T.) ;
#27444 = ORIENTED_EDGE('',*,*,#19151,.T.) ;
#27445 = ORIENTED_EDGE('',*,*,#19152,.T.) ;
#27446 = ORIENTED_EDGE('',*,*,#19148,.F.) ;
#27447 = ORIENTED_EDGE('',*,*,#19153,.T.) ;
#27448 = ORIENTED_EDGE('',*,*,#19154,.T.) ;
#27449 = ORIENTED_EDGE('',*,*,#19155,.T.) ;
#27450 = ORIENTED_EDGE('',*,*,#19156,.T.) ;
#27451 = ORIENTED_EDGE('',*,*,#19157,.T.) ;
#27452 = ORIENTED_EDGE('',*,*,#19158,.T.) ;
#27453 = ORIENTED_EDGE('',*,*,#19154,.F.) ;
#27454 = ORIENTED_EDGE('',*,*,#19159,.T.) ;
#27455 = ORIENTED_EDGE('',*,*,#19157,.F.) ;
#27456 = ORIENTED_EDGE('',*,*,#19160,.T.) ;
#27457 = ORIENTED_EDGE('',*,*,#19151,.F.) ;
#27458 = ORIENTED_EDGE('',*,*,#19161,.T.) ;
#27459 = ORIENTED_EDGE('',*,*,#19147,.F.) ;
#27460 = ORIENTED_EDGE('',*,*,#19162,.F.) ;
#27461 = ORIENTED_EDGE('',*,*,#19163,.T.) ;
#27462 = ORIENTED_EDGE('',*,*,#19164,.F.) ;
#27463 = ORIENTED_EDGE('',*,*,#19165,.F.) ;
#27464 = ORIENTED_EDGE('',*,*,#19166,.F.) ;
#27465 = ORIENTED_EDGE('',*,*,#19167,.F.) ;
#27466 = ORIENTED_EDGE('',*,*,#19168,.F.) ;
#27467 = ORIENTED_EDGE('',*,*,#19169,.F.) ;
#27468 = ORIENTED_EDGE('',*,*,#19170,.F.) ;
#27469 = ORIENTED_EDGE('',*,*,#19143,.F.) ;
#27470 = ORIENTED_EDGE('',*,*,#19163,.F.) ;
#27471 = ORIENTED_EDGE('',*,*,#19171,.F.) ;
#27472 = ORIENTED_EDGE('',*,*,#19172,.F.) ;
#27473 = ORIENTED_EDGE('',*,*,#19173,.F.) ;
#27474 = ORIENTED_EDGE('',*,*,#19174,.F.) ;
#27475 = ORIENTED_EDGE('',*,*,#19175,.T.) ;
#27476 = ORIENTED_EDGE('',*,*,#19176,.T.) ;
#27477 = ORIENTED_EDGE('',*,*,#19175,.F.) ;
#27478 = ORIENTED_EDGE('',*,*,#19149,.F.) ;
#27479 = ORIENTED_EDGE('',*,*,#19152,.F.) ;
#27480 = ORIENTED_EDGE('',*,*,#19177,.T.) ;
#27481 = ORIENTED_EDGE('',*,*,#19178,.F.) ;
#27482 = ORIENTED_EDGE('',*,*,#19179,.F.) ;
#27483 = ORIENTED_EDGE('',*,*,#19180,.F.) ;
#27484 = ORIENTED_EDGE('',*,*,#19171,.T.) ;
#27485 = ORIENTED_EDGE('',*,*,#19162,.T.) ;
#27486 = ORIENTED_EDGE('',*,*,#19181,.T.) ;
#27487 = ORIENTED_EDGE('',*,*,#19182,.T.) ;
#27488 = ORIENTED_EDGE('',*,*,#19173,.T.) ;
#27489 = ORIENTED_EDGE('',*,*,#19183,.T.) ;
#27490 = ORIENTED_EDGE('',*,*,#19184,.T.) ;
#27491 = ORIENTED_EDGE('',*,*,#19181,.F.) ;
#27492 = ORIENTED_EDGE('',*,*,#19185,.T.) ;
#27493 = ORIENTED_EDGE('',*,*,#19186,.T.) ;
#27494 = ORIENTED_EDGE('',*,*,#19187,.T.) ;
#27495 = ORIENTED_EDGE('',*,*,#19183,.F.) ;
#27496 = ORIENTED_EDGE('',*,*,#19179,.T.) ;
#27497 = ORIENTED_EDGE('',*,*,#19188,.T.) ;
#27498 = ORIENTED_EDGE('',*,*,#19189,.T.) ;
#27499 = ORIENTED_EDGE('',*,*,#19186,.F.) ;
#27500 = ORIENTED_EDGE('',*,*,#19178,.T.) ;
#27501 = ORIENTED_EDGE('',*,*,#19190,.T.) ;
#27502 = ORIENTED_EDGE('',*,*,#19191,.T.) ;
#27503 = ORIENTED_EDGE('',*,*,#19192,.T.) ;
#27504 = ORIENTED_EDGE('',*,*,#19192,.F.) ;
#27505 = ORIENTED_EDGE('',*,*,#19193,.T.) ;
#27506 = ORIENTED_EDGE('',*,*,#19194,.T.) ;
#27507 = ORIENTED_EDGE('',*,*,#19195,.T.) ;
#27508 = ORIENTED_EDGE('',*,*,#19194,.F.) ;
#27509 = ORIENTED_EDGE('',*,*,#19196,.T.) ;
#27510 = ORIENTED_EDGE('',*,*,#19188,.F.) ;
#27511 = ORIENTED_EDGE('',*,*,#19197,.T.) ;
#27512 = ORIENTED_EDGE('',*,*,#19182,.F.) ;
#27513 = ORIENTED_EDGE('',*,*,#19184,.F.) ;
#27514 = ORIENTED_EDGE('',*,*,#19187,.F.) ;
#27515 = ORIENTED_EDGE('',*,*,#19198,.T.) ;
#27516 = ORIENTED_EDGE('',*,*,#19199,.T.) ;
#27517 = ORIENTED_EDGE('',*,*,#19200,.T.) ;
#27518 = ORIENTED_EDGE('',*,*,#19189,.F.) ;
#27519 = ORIENTED_EDGE('',*,*,#19196,.F.) ;
#27520 = ORIENTED_EDGE('',*,*,#19193,.F.) ;
#27521 = ORIENTED_EDGE('',*,*,#19191,.F.) ;
#27522 = ORIENTED_EDGE('',*,*,#19201,.F.) ;
#27523 = ORIENTED_EDGE('',*,*,#19202,.F.) ;
#27524 = ORIENTED_EDGE('',*,*,#19203,.F.) ;
#27525 = ORIENTED_EDGE('',*,*,#19204,.F.) ;
#27526 = ORIENTED_EDGE('',*,*,#19198,.F.) ;
#27527 = ORIENTED_EDGE('',*,*,#19205,.T.) ;
#27528 = ORIENTED_EDGE('',*,*,#19165,.T.) ;
#27529 = ORIENTED_EDGE('',*,*,#19206,.T.) ;
#27530 = ORIENTED_EDGE('',*,*,#19205,.F.) ;
#27531 = ORIENTED_EDGE('',*,*,#19207,.T.) ;
#27532 = ORIENTED_EDGE('',*,*,#19208,.T.) ;
#27533 = ORIENTED_EDGE('',*,*,#19209,.T.) ;
#27534 = ORIENTED_EDGE('',*,*,#19210,.T.) ;
#27535 = ORIENTED_EDGE('',*,*,#19211,.T.) ;
#27536 = ORIENTED_EDGE('',*,*,#19208,.F.) ;
#27537 = ORIENTED_EDGE('',*,*,#19212,.T.) ;
#27538 = ORIENTED_EDGE('',*,*,#19213,.T.) ;
#27539 = ORIENTED_EDGE('',*,*,#19214,.T.) ;
#27540 = ORIENTED_EDGE('',*,*,#19210,.F.) ;
#27541 = ORIENTED_EDGE('',*,*,#19215,.T.) ;
#27542 = ORIENTED_EDGE('',*,*,#19216,.T.) ;
#27543 = ORIENTED_EDGE('',*,*,#19217,.T.) ;
#27544 = ORIENTED_EDGE('',*,*,#19218,.T.) ;
#27545 = ORIENTED_EDGE('',*,*,#19219,.T.) ;
#27546 = ORIENTED_EDGE('',*,*,#19220,.T.) ;
#27547 = ORIENTED_EDGE('',*,*,#19216,.F.) ;
#27548 = ORIENTED_EDGE('',*,*,#19221,.T.) ;
#27549 = ORIENTED_EDGE('',*,*,#19219,.F.) ;
#27550 = ORIENTED_EDGE('',*,*,#19222,.T.) ;
#27551 = ORIENTED_EDGE('',*,*,#19213,.F.) ;
#27552 = ORIENTED_EDGE('',*,*,#19223,.T.) ;
#27553 = ORIENTED_EDGE('',*,*,#19209,.F.) ;
#27554 = ORIENTED_EDGE('',*,*,#19224,.F.) ;
#27555 = ORIENTED_EDGE('',*,*,#19166,.T.) ;
#27556 = ORIENTED_EDGE('',*,*,#19211,.F.) ;
#27557 = ORIENTED_EDGE('',*,*,#19214,.F.) ;
#27558 = ORIENTED_EDGE('',*,*,#19225,.T.) ;
#27559 = ORIENTED_EDGE('',*,*,#19226,.F.) ;
#27560 = ORIENTED_EDGE('',*,*,#19227,.F.) ;
#27561 = ORIENTED_EDGE('',*,*,#19228,.F.) ;
#27562 = ORIENTED_EDGE('',*,*,#19167,.T.) ;
#27563 = ORIENTED_EDGE('',*,*,#19224,.T.) ;
#27564 = ORIENTED_EDGE('',*,*,#19229,.T.) ;
#27565 = ORIENTED_EDGE('',*,*,#19230,.T.) ;
#27566 = ORIENTED_EDGE('',*,*,#19169,.T.) ;
#27567 = ORIENTED_EDGE('',*,*,#19231,.T.) ;
#27568 = ORIENTED_EDGE('',*,*,#19232,.T.) ;
#27569 = ORIENTED_EDGE('',*,*,#19229,.F.) ;
#27570 = ORIENTED_EDGE('',*,*,#19233,.T.) ;
#27571 = ORIENTED_EDGE('',*,*,#19234,.T.) ;
#27572 = ORIENTED_EDGE('',*,*,#19235,.T.) ;
#27573 = ORIENTED_EDGE('',*,*,#19231,.F.) ;
#27574 = ORIENTED_EDGE('',*,*,#19227,.T.) ;
#27575 = ORIENTED_EDGE('',*,*,#19236,.T.) ;
#27576 = ORIENTED_EDGE('',*,*,#19237,.T.) ;
#27577 = ORIENTED_EDGE('',*,*,#19234,.F.) ;
#27578 = ORIENTED_EDGE('',*,*,#19226,.T.) ;
#27579 = ORIENTED_EDGE('',*,*,#19238,.T.) ;
#27580 = ORIENTED_EDGE('',*,*,#19239,.T.) ;
#27581 = ORIENTED_EDGE('',*,*,#19240,.T.) ;
#27582 = ORIENTED_EDGE('',*,*,#19240,.F.) ;
#27583 = ORIENTED_EDGE('',*,*,#19241,.T.) ;
#27584 = ORIENTED_EDGE('',*,*,#19242,.T.) ;
#27585 = ORIENTED_EDGE('',*,*,#19243,.T.) ;
#27586 = ORIENTED_EDGE('',*,*,#19242,.F.) ;
#27587 = ORIENTED_EDGE('',*,*,#19244,.T.) ;
#27588 = ORIENTED_EDGE('',*,*,#19236,.F.) ;
#27589 = ORIENTED_EDGE('',*,*,#19245,.T.) ;
#27590 = ORIENTED_EDGE('',*,*,#19230,.F.) ;
#27591 = ORIENTED_EDGE('',*,*,#19232,.F.) ;
#27592 = ORIENTED_EDGE('',*,*,#19235,.F.) ;
#27593 = ORIENTED_EDGE('',*,*,#19246,.T.) ;
#27594 = ORIENTED_EDGE('',*,*,#19247,.F.) ;
#27595 = ORIENTED_EDGE('',*,*,#19248,.T.) ;
#27596 = ORIENTED_EDGE('',*,*,#19237,.F.) ;
#27597 = ORIENTED_EDGE('',*,*,#19244,.F.) ;
#27598 = ORIENTED_EDGE('',*,*,#19241,.F.) ;
#27599 = ORIENTED_EDGE('',*,*,#19239,.F.) ;
#27600 = ORIENTED_EDGE('',*,*,#19249,.F.) ;
#27601 = ORIENTED_EDGE('',*,*,#19250,.F.) ;
#27602 = ORIENTED_EDGE('',*,*,#19251,.F.) ;
#27603 = ORIENTED_EDGE('',*,*,#19252,.F.) ;
#27604 = ORIENTED_EDGE('',*,*,#19246,.F.) ;
#27605 = ORIENTED_EDGE('',*,*,#19253,.T.) ;
#27606 = ORIENTED_EDGE('',*,*,#19254,.T.) ;
#27607 = ORIENTED_EDGE('',*,*,#19255,.T.) ;
#27608 = ORIENTED_EDGE('',*,*,#19253,.F.) ;
#27609 = ORIENTED_EDGE('',*,*,#19256,.T.) ;
#27610 = ORIENTED_EDGE('',*,*,#19257,.T.) ;
#27611 = ORIENTED_EDGE('',*,*,#19258,.T.) ;
#27612 = ORIENTED_EDGE('',*,*,#19257,.F.) ;
#27613 = ORIENTED_EDGE('',*,*,#19259,.T.) ;
#27614 = ORIENTED_EDGE('',*,*,#19260,.T.) ;
#27615 = ORIENTED_EDGE('',*,*,#19259,.F.) ;
#27616 = ORIENTED_EDGE('',*,*,#19261,.T.) ;
#27617 = ORIENTED_EDGE('',*,*,#19262,.F.) ;
#27618 = ORIENTED_EDGE('',*,*,#19263,.T.) ;
#27619 = ORIENTED_EDGE('',*,*,#19256,.F.) ;
#27620 = ORIENTED_EDGE('',*,*,#19264,.F.) ;
#27621 = ORIENTED_EDGE('',*,*,#19265,.F.) ;
#27622 = ORIENTED_EDGE('',*,*,#19266,.F.) ;
#27623 = ORIENTED_EDGE('',*,*,#19261,.F.) ;
#27624 = ORIENTED_EDGE('',*,*,#19255,.F.) ;
#27625 = ORIENTED_EDGE('',*,*,#19267,.T.) ;
#27626 = ORIENTED_EDGE('',*,*,#19268,.F.) ;
#27627 = ORIENTED_EDGE('',*,*,#19264,.T.) ;
#27628 = ORIENTED_EDGE('',*,*,#19269,.T.) ;
#27629 = ORIENTED_EDGE('',*,*,#19262,.T.) ;
#27630 = ORIENTED_EDGE('',*,*,#19270,.T.) ;
#27631 = ORIENTED_EDGE('',*,*,#19271,.T.) ;
#27632 = ORIENTED_EDGE('',*,*,#19272,.T.) ;
#27633 = ORIENTED_EDGE('',*,*,#19270,.F.) ;
#27634 = ORIENTED_EDGE('',*,*,#19266,.T.) ;
#27635 = ORIENTED_EDGE('',*,*,#19271,.F.) ;
#27636 = ORIENTED_EDGE('',*,*,#19265,.T.) ;
#27637 = ORIENTED_EDGE('',*,*,#19273,.T.) ;
#27638 = ORIENTED_EDGE('',*,*,#19274,.T.) ;
#27639 = ORIENTED_EDGE('',*,*,#19273,.F.) ;
#27640 = ORIENTED_EDGE('',*,*,#19268,.T.) ;
#27641 = ORIENTED_EDGE('',*,*,#19275,.T.) ;
#27642 = ORIENTED_EDGE('',*,*,#19276,.T.) ;
#27643 = ORIENTED_EDGE('',*,*,#19277,.T.) ;
#27644 = ORIENTED_EDGE('',*,*,#19278,.T.) ;
#27645 = ORIENTED_EDGE('',*,*,#19279,.T.) ;
#27646 = ORIENTED_EDGE('',*,*,#19280,.T.) ;
#27647 = ORIENTED_EDGE('',*,*,#19276,.F.) ;
#27648 = ORIENTED_EDGE('',*,*,#19281,.T.) ;
#27649 = ORIENTED_EDGE('',*,*,#19282,.T.) ;
#27650 = ORIENTED_EDGE('',*,*,#19283,.T.) ;
#27651 = ORIENTED_EDGE('',*,*,#19279,.F.) ;
#27652 = ORIENTED_EDGE('',*,*,#19284,.T.) ;
#27653 = ORIENTED_EDGE('',*,*,#19285,.T.) ;
#27654 = ORIENTED_EDGE('',*,*,#19286,.T.) ;
#27655 = ORIENTED_EDGE('',*,*,#19282,.F.) ;
#27656 = ORIENTED_EDGE('',*,*,#19285,.F.) ;
#27657 = ORIENTED_EDGE('',*,*,#19287,.T.) ;
#27658 = ORIENTED_EDGE('',*,*,#19288,.F.) ;
#27659 = ORIENTED_EDGE('',*,*,#19289,.T.) ;
#27660 = ORIENTED_EDGE('',*,*,#19284,.F.) ;
#27661 = ORIENTED_EDGE('',*,*,#19281,.F.) ;
#27662 = ORIENTED_EDGE('',*,*,#19290,.F.) ;
#27663 = ORIENTED_EDGE('',*,*,#19291,.F.) ;
#27664 = ORIENTED_EDGE('',*,*,#19287,.F.) ;
#27665 = ORIENTED_EDGE('',*,*,#19278,.F.) ;
#27666 = ORIENTED_EDGE('',*,*,#19292,.T.) ;
#27667 = ORIENTED_EDGE('',*,*,#19293,.F.) ;
#27668 = ORIENTED_EDGE('',*,*,#19290,.T.) ;
#27669 = ORIENTED_EDGE('',*,*,#19294,.T.) ;
#27670 = ORIENTED_EDGE('',*,*,#19293,.T.) ;
#27671 = ORIENTED_EDGE('',*,*,#19295,.T.) ;
#27672 = ORIENTED_EDGE('',*,*,#19294,.F.) ;
#27673 = ORIENTED_EDGE('',*,*,#19296,.T.) ;
#27674 = ORIENTED_EDGE('',*,*,#19297,.T.) ;
#27675 = ORIENTED_EDGE('',*,*,#19291,.T.) ;
#27676 = ORIENTED_EDGE('',*,*,#19297,.F.) ;
#27677 = ORIENTED_EDGE('',*,*,#19298,.T.) ;
#27678 = ORIENTED_EDGE('',*,*,#19288,.T.) ;
#27679 = ORIENTED_EDGE('',*,*,#19296,.F.) ;
#27680 = ORIENTED_EDGE('',*,*,#19299,.F.) ;
#27681 = ORIENTED_EDGE('',*,*,#19300,.F.) ;
#27682 = ORIENTED_EDGE('',*,*,#19301,.F.) ;
#27683 = ORIENTED_EDGE('',*,*,#19302,.F.) ;
#27684 = ORIENTED_EDGE('',*,*,#19303,.F.) ;
#27685 = ORIENTED_EDGE('',*,*,#19295,.F.) ;
#27686 = ORIENTED_EDGE('',*,*,#19304,.T.) ;
#27687 = ORIENTED_EDGE('',*,*,#19305,.F.) ;
#27688 = ORIENTED_EDGE('',*,*,#19299,.T.) ;
#27689 = ORIENTED_EDGE('',*,*,#19306,.T.) ;
#27690 = ORIENTED_EDGE('',*,*,#19307,.T.) ;
#27691 = ORIENTED_EDGE('',*,*,#19308,.T.) ;
#27692 = ORIENTED_EDGE('',*,*,#19309,.T.) ;
#27693 = ORIENTED_EDGE('',*,*,#19310,.T.) ;
#27694 = ORIENTED_EDGE('',*,*,#19306,.F.) ;
#27695 = ORIENTED_EDGE('',*,*,#19311,.T.) ;
#27696 = ORIENTED_EDGE('',*,*,#19309,.F.) ;
#27697 = ORIENTED_EDGE('',*,*,#19312,.T.) ;
#27698 = ORIENTED_EDGE('',*,*,#19313,.T.) ;
#27699 = ORIENTED_EDGE('',*,*,#19314,.T.) ;
#27700 = ORIENTED_EDGE('',*,*,#19315,.T.) ;
#27701 = ORIENTED_EDGE('',*,*,#19316,.T.) ;
#27702 = ORIENTED_EDGE('',*,*,#19313,.F.) ;
#27703 = ORIENTED_EDGE('',*,*,#19315,.F.) ;
#27704 = ORIENTED_EDGE('',*,*,#19312,.F.) ;
#27705 = ORIENTED_EDGE('',*,*,#19317,.T.) ;
#27706 = ORIENTED_EDGE('',*,*,#19318,.F.) ;
#27707 = ORIENTED_EDGE('',*,*,#19319,.F.) ;
#27708 = ORIENTED_EDGE('',*,*,#19320,.T.) ;
#27709 = ORIENTED_EDGE('',*,*,#19311,.F.) ;
#27710 = ORIENTED_EDGE('',*,*,#19321,.F.) ;
#27711 = ORIENTED_EDGE('',*,*,#19322,.F.) ;
#27712 = ORIENTED_EDGE('',*,*,#19317,.F.) ;
#27713 = ORIENTED_EDGE('',*,*,#19308,.F.) ;
#27714 = ORIENTED_EDGE('',*,*,#19323,.T.) ;
#27715 = ORIENTED_EDGE('',*,*,#19324,.F.) ;
#27716 = ORIENTED_EDGE('',*,*,#19321,.T.) ;
#27717 = ORIENTED_EDGE('',*,*,#19307,.F.) ;
#27718 = ORIENTED_EDGE('',*,*,#19325,.T.) ;
#27719 = ORIENTED_EDGE('',*,*,#19326,.F.) ;
#27720 = ORIENTED_EDGE('',*,*,#19327,.T.) ;
#27721 = ORIENTED_EDGE('',*,*,#19328,.T.) ;
#27722 = ORIENTED_EDGE('',*,*,#19324,.T.) ;
#27723 = ORIENTED_EDGE('',*,*,#19329,.T.) ;
#27724 = ORIENTED_EDGE('',*,*,#19330,.T.) ;
#27725 = ORIENTED_EDGE('',*,*,#19322,.T.) ;
#27726 = ORIENTED_EDGE('',*,*,#19328,.F.) ;
#27727 = ORIENTED_EDGE('',*,*,#19331,.T.) ;
#27728 = ORIENTED_EDGE('',*,*,#19332,.T.) ;
#27729 = ORIENTED_EDGE('',*,*,#19318,.T.) ;
#27730 = ORIENTED_EDGE('',*,*,#19330,.F.) ;
#27731 = ORIENTED_EDGE('',*,*,#19333,.T.) ;
#27732 = ORIENTED_EDGE('',*,*,#19334,.T.) ;
#27733 = ORIENTED_EDGE('',*,*,#19319,.T.) ;
#27734 = ORIENTED_EDGE('',*,*,#19332,.F.) ;
#27735 = ORIENTED_EDGE('',*,*,#19334,.F.) ;
#27736 = ORIENTED_EDGE('',*,*,#19335,.T.) ;
#27737 = ORIENTED_EDGE('',*,*,#19336,.F.) ;
#27738 = ORIENTED_EDGE('',*,*,#19337,.T.) ;
#27739 = ORIENTED_EDGE('',*,*,#19333,.F.) ;
#27740 = ORIENTED_EDGE('',*,*,#19331,.F.) ;
#27741 = ORIENTED_EDGE('',*,*,#19338,.F.) ;
#27742 = ORIENTED_EDGE('',*,*,#19339,.F.) ;
#27743 = ORIENTED_EDGE('',*,*,#19335,.F.) ;
#27744 = ORIENTED_EDGE('',*,*,#19329,.F.) ;
#27745 = ORIENTED_EDGE('',*,*,#19340,.T.) ;
#27746 = ORIENTED_EDGE('',*,*,#19341,.F.) ;
#27747 = ORIENTED_EDGE('',*,*,#19338,.T.) ;
#27748 = ORIENTED_EDGE('',*,*,#19342,.T.) ;
#27749 = ORIENTED_EDGE('',*,*,#19341,.T.) ;
#27750 = ORIENTED_EDGE('',*,*,#19343,.T.) ;
#27751 = ORIENTED_EDGE('',*,*,#19342,.F.) ;
#27752 = ORIENTED_EDGE('',*,*,#19344,.T.) ;
#27753 = ORIENTED_EDGE('',*,*,#19345,.T.) ;
#27754 = ORIENTED_EDGE('',*,*,#19339,.T.) ;
#27755 = ORIENTED_EDGE('',*,*,#19345,.F.) ;
#27756 = ORIENTED_EDGE('',*,*,#19346,.T.) ;
#27757 = ORIENTED_EDGE('',*,*,#19336,.T.) ;
#27758 = ORIENTED_EDGE('',*,*,#19344,.F.) ;
#27759 = ORIENTED_EDGE('',*,*,#19347,.F.) ;
#27760 = ORIENTED_EDGE('',*,*,#19348,.F.) ;
#27761 = ORIENTED_EDGE('',*,*,#19349,.F.) ;
#27762 = ORIENTED_EDGE('',*,*,#19350,.F.) ;
#27763 = ORIENTED_EDGE('',*,*,#19351,.F.) ;
#27764 = ORIENTED_EDGE('',*,*,#19343,.F.) ;
#27765 = ORIENTED_EDGE('',*,*,#19352,.T.) ;
#27766 = ORIENTED_EDGE('',*,*,#19353,.F.) ;
#27767 = ORIENTED_EDGE('',*,*,#19347,.T.) ;
#27768 = ORIENTED_EDGE('',*,*,#19354,.T.) ;
#27769 = ORIENTED_EDGE('',*,*,#19355,.T.) ;
#27770 = ORIENTED_EDGE('',*,*,#19326,.T.) ;
#27771 = ORIENTED_EDGE('',*,*,#19354,.F.) ;
#27772 = ORIENTED_EDGE('',*,*,#19356,.T.) ;
#27773 = ORIENTED_EDGE('',*,*,#19357,.T.) ;
#27774 = ORIENTED_EDGE('',*,*,#19358,.T.) ;
#27775 = ORIENTED_EDGE('',*,*,#19357,.F.) ;
#27776 = ORIENTED_EDGE('',*,*,#19359,.T.) ;
#27777 = ORIENTED_EDGE('',*,*,#19360,.T.) ;
#27778 = ORIENTED_EDGE('',*,*,#19314,.F.) ;
#27779 = ORIENTED_EDGE('',*,*,#19361,.F.) ;
#27780 = ORIENTED_EDGE('',*,*,#19356,.F.) ;
#27781 = ORIENTED_EDGE('',*,*,#19325,.F.) ;
#27782 = ORIENTED_EDGE('',*,*,#19310,.F.) ;
#27783 = ORIENTED_EDGE('',*,*,#19355,.F.) ;
#27784 = ORIENTED_EDGE('',*,*,#19362,.T.) ;
#27785 = ORIENTED_EDGE('',*,*,#19363,.F.) ;
#27786 = ORIENTED_EDGE('',*,*,#19364,.T.) ;
#27787 = ORIENTED_EDGE('',*,*,#19365,.F.) ;
#27788 = ORIENTED_EDGE('',*,*,#19366,.T.) ;
#27789 = ORIENTED_EDGE('',*,*,#19367,.T.) ;
#27790 = ORIENTED_EDGE('',*,*,#19368,.T.) ;
#27791 = ORIENTED_EDGE('',*,*,#19369,.T.) ;
#27792 = ORIENTED_EDGE('',*,*,#19370,.T.) ;
#27793 = ORIENTED_EDGE('',*,*,#19371,.T.) ;
#27794 = ORIENTED_EDGE('',*,*,#19372,.T.) ;
#27795 = ORIENTED_EDGE('',*,*,#19137,.T.) ;
#27796 = ORIENTED_EDGE('',*,*,#19373,.T.) ;
#27797 = ORIENTED_EDGE('',*,*,#19367,.F.) ;
#27798 = ORIENTED_EDGE('',*,*,#19374,.T.) ;
#27799 = ORIENTED_EDGE('',*,*,#19375,.T.) ;
#27800 = ORIENTED_EDGE('',*,*,#19365,.T.) ;
#27801 = ORIENTED_EDGE('',*,*,#19376,.F.) ;
#27802 = ORIENTED_EDGE('',*,*,#19090,.F.) ;
#27803 = ORIENTED_EDGE('',*,*,#19377,.T.) ;
#27804 = ORIENTED_EDGE('',*,*,#19378,.T.) ;
#27805 = ORIENTED_EDGE('',*,*,#19379,.T.) ;
#27806 = ORIENTED_EDGE('',*,*,#19380,.T.) ;
#27807 = ORIENTED_EDGE('',*,*,#19138,.T.) ;
#27808 = ORIENTED_EDGE('',*,*,#19375,.F.) ;
#27809 = ORIENTED_EDGE('',*,*,#19381,.T.) ;
#27810 = ORIENTED_EDGE('',*,*,#19376,.T.) ;
#27811 = ORIENTED_EDGE('',*,*,#19372,.F.) ;
#27812 = ORIENTED_EDGE('',*,*,#19371,.F.) ;
#27813 = ORIENTED_EDGE('',*,*,#19370,.F.) ;
#27814 = ORIENTED_EDGE('',*,*,#19369,.F.) ;
#27815 = ORIENTED_EDGE('',*,*,#19368,.F.) ;
#27816 = ORIENTED_EDGE('',*,*,#19373,.F.) ;
#27817 = ORIENTED_EDGE('',*,*,#19136,.F.) ;
#27818 = ORIENTED_EDGE('',*,*,#19135,.F.) ;
#27819 = ORIENTED_EDGE('',*,*,#19132,.F.) ;
#27820 = ORIENTED_EDGE('',*,*,#19129,.F.) ;
#27821 = ORIENTED_EDGE('',*,*,#19126,.F.) ;
#27822 = ORIENTED_EDGE('',*,*,#19123,.F.) ;
#27823 = ORIENTED_EDGE('',*,*,#19120,.F.) ;
#27824 = ORIENTED_EDGE('',*,*,#19117,.F.) ;
#27825 = ORIENTED_EDGE('',*,*,#19382,.F.) ;
#27826 = ORIENTED_EDGE('',*,*,#19140,.T.) ;
#27827 = ORIENTED_EDGE('',*,*,#19113,.T.) ;
#27828 = ORIENTED_EDGE('',*,*,#19109,.T.) ;
#27829 = ORIENTED_EDGE('',*,*,#19106,.T.) ;
#27830 = ORIENTED_EDGE('',*,*,#19103,.T.) ;
#27831 = ORIENTED_EDGE('',*,*,#19100,.T.) ;
#27832 = ORIENTED_EDGE('',*,*,#19097,.T.) ;
#27833 = ORIENTED_EDGE('',*,*,#19094,.T.) ;
#27834 = ORIENTED_EDGE('',*,*,#19091,.T.) ;
#27835 = ORIENTED_EDGE('',*,*,#19176,.F.) ;
#27836 = ORIENTED_EDGE('',*,*,#19366,.F.) ;
#27837 = ORIENTED_EDGE('',*,*,#19381,.F.) ;
#27838 = ORIENTED_EDGE('',*,*,#19374,.F.) ;
#27839 = ORIENTED_EDGE('',*,*,#19383,.T.) ;
#27840 = ORIENTED_EDGE('',*,*,#19384,.T.) ;
#27841 = ORIENTED_EDGE('',*,*,#19385,.T.) ;
#27842 = ORIENTED_EDGE('',*,*,#19386,.T.) ;
#27843 = ORIENTED_EDGE('',*,*,#19387,.T.) ;
#27844 = ORIENTED_EDGE('',*,*,#19388,.T.) ;
#27845 = ORIENTED_EDGE('',*,*,#19389,.T.) ;
#27846 = ORIENTED_EDGE('',*,*,#19390,.T.) ;
#27847 = ORIENTED_EDGE('',*,*,#19391,.T.) ;
#27848 = ORIENTED_EDGE('',*,*,#19392,.T.) ;
#27849 = ORIENTED_EDGE('',*,*,#19393,.T.) ;
#27850 = ORIENTED_EDGE('',*,*,#19383,.F.) ;
#27851 = ORIENTED_EDGE('',*,*,#19394,.T.) ;
#27852 = ORIENTED_EDGE('',*,*,#19392,.F.) ;
#27853 = ORIENTED_EDGE('',*,*,#19395,.T.) ;
#27854 = ORIENTED_EDGE('',*,*,#19396,.T.) ;
#27855 = ORIENTED_EDGE('',*,*,#19397,.T.) ;
#27856 = ORIENTED_EDGE('',*,*,#19396,.F.) ;
#27857 = ORIENTED_EDGE('',*,*,#19398,.T.) ;
#27858 = ORIENTED_EDGE('',*,*,#19399,.T.) ;
#27859 = ORIENTED_EDGE('',*,*,#19395,.F.) ;
#27860 = ORIENTED_EDGE('',*,*,#19400,.F.) ;
#27861 = ORIENTED_EDGE('',*,*,#19401,.F.) ;
#27862 = ORIENTED_EDGE('',*,*,#19402,.F.) ;
#27863 = ORIENTED_EDGE('',*,*,#19394,.F.) ;
#27864 = ORIENTED_EDGE('',*,*,#19391,.F.) ;
#27865 = ORIENTED_EDGE('',*,*,#19390,.F.) ;
#27866 = ORIENTED_EDGE('',*,*,#19389,.F.) ;
#27867 = ORIENTED_EDGE('',*,*,#19388,.F.) ;
#27868 = ORIENTED_EDGE('',*,*,#19403,.T.) ;
#27869 = ORIENTED_EDGE('',*,*,#19404,.T.) ;
#27870 = ORIENTED_EDGE('',*,*,#19400,.T.) ;
#27871 = ORIENTED_EDGE('',*,*,#19384,.F.) ;
#27872 = ORIENTED_EDGE('',*,*,#19405,.T.) ;
#27873 = ORIENTED_EDGE('',*,*,#19406,.F.) ;
#27874 = ORIENTED_EDGE('',*,*,#19407,.F.) ;
#27875 = ORIENTED_EDGE('',*,*,#19408,.T.) ;
#27876 = ORIENTED_EDGE('',*,*,#19387,.F.) ;
#27877 = ORIENTED_EDGE('',*,*,#19386,.F.) ;
#27878 = ORIENTED_EDGE('',*,*,#19385,.F.) ;
#27879 = ORIENTED_EDGE('',*,*,#19409,.T.) ;
#27880 = ORIENTED_EDGE('',*,*,#19410,.T.) ;
#27881 = ORIENTED_EDGE('',*,*,#19411,.T.) ;
#27882 = ORIENTED_EDGE('',*,*,#19412,.T.) ;
#27883 = ORIENTED_EDGE('',*,*,#19413,.T.) ;
#27884 = ORIENTED_EDGE('',*,*,#19409,.F.) ;
#27885 = ORIENTED_EDGE('',*,*,#19414,.T.) ;
#27886 = ORIENTED_EDGE('',*,*,#19412,.F.) ;
#27887 = ORIENTED_EDGE('',*,*,#19415,.T.) ;
#27888 = ORIENTED_EDGE('',*,*,#19416,.T.) ;
#27889 = ORIENTED_EDGE('',*,*,#19417,.T.) ;
#27890 = ORIENTED_EDGE('',*,*,#19418,.T.) ;
#27891 = ORIENTED_EDGE('',*,*,#19419,.T.) ;
#27892 = ORIENTED_EDGE('',*,*,#19407,.T.) ;
#27893 = ORIENTED_EDGE('',*,*,#19406,.T.) ;
#27894 = ORIENTED_EDGE('',*,*,#19416,.F.) ;
#27895 = ORIENTED_EDGE('',*,*,#19418,.F.) ;
#27896 = ORIENTED_EDGE('',*,*,#19415,.F.) ;
#27897 = ORIENTED_EDGE('',*,*,#19420,.T.) ;
#27898 = ORIENTED_EDGE('',*,*,#19421,.T.) ;
#27899 = ORIENTED_EDGE('',*,*,#19422,.T.) ;
#27900 = ORIENTED_EDGE('',*,*,#19419,.F.) ;
#27901 = ORIENTED_EDGE('',*,*,#19414,.F.) ;
#27902 = ORIENTED_EDGE('',*,*,#19423,.F.) ;
#27903 = ORIENTED_EDGE('',*,*,#19424,.F.) ;
#27904 = ORIENTED_EDGE('',*,*,#19420,.F.) ;
#27905 = ORIENTED_EDGE('',*,*,#19411,.F.) ;
#27906 = ORIENTED_EDGE('',*,*,#19425,.T.) ;
#27907 = ORIENTED_EDGE('',*,*,#19426,.F.) ;
#27908 = ORIENTED_EDGE('',*,*,#19423,.T.) ;
#27909 = ORIENTED_EDGE('',*,*,#19403,.F.) ;
#27910 = ORIENTED_EDGE('',*,*,#19408,.F.) ;
#27911 = ORIENTED_EDGE('',*,*,#19422,.F.) ;
#27912 = ORIENTED_EDGE('',*,*,#19427,.F.) ;
#27913 = ORIENTED_EDGE('',*,*,#19428,.F.) ;
#27914 = ORIENTED_EDGE('',*,*,#19177,.F.) ;
#27915 = ORIENTED_EDGE('',*,*,#19429,.F.) ;
#27916 = ORIENTED_EDGE('',*,*,#19430,.F.) ;
#27917 = ORIENTED_EDGE('',*,*,#19431,.T.) ;
#27918 = ORIENTED_EDGE('',*,*,#19432,.T.) ;
#27919 = ORIENTED_EDGE('',*,*,#19363,.T.) ;
#27920 = ORIENTED_EDGE('',*,*,#19433,.T.) ;
#27921 = ORIENTED_EDGE('',*,*,#19434,.T.) ;
#27922 = ORIENTED_EDGE('',*,*,#19431,.F.) ;
#27923 = ORIENTED_EDGE('',*,*,#19435,.T.) ;
#27924 = ORIENTED_EDGE('',*,*,#19436,.T.) ;
#27925 = ORIENTED_EDGE('',*,*,#19437,.T.) ;
#27926 = ORIENTED_EDGE('',*,*,#19438,.T.) ;
#27927 = ORIENTED_EDGE('',*,*,#19439,.T.) ;
#27928 = ORIENTED_EDGE('',*,*,#19440,.T.) ;
#27929 = ORIENTED_EDGE('',*,*,#19202,.T.) ;
#27930 = ORIENTED_EDGE('',*,*,#19438,.F.) ;
#27931 = ORIENTED_EDGE('',*,*,#19441,.T.) ;
#27932 = ORIENTED_EDGE('',*,*,#19440,.F.) ;
#27933 = ORIENTED_EDGE('',*,*,#19442,.T.) ;
#27934 = ORIENTED_EDGE('',*,*,#19443,.T.) ;
#27935 = ORIENTED_EDGE('',*,*,#19436,.F.) ;
#27936 = ORIENTED_EDGE('',*,*,#19444,.T.) ;
#27937 = ORIENTED_EDGE('',*,*,#19433,.F.) ;
#27938 = ORIENTED_EDGE('',*,*,#19432,.F.) ;
#27939 = ORIENTED_EDGE('',*,*,#19445,.T.) ;
#27940 = ORIENTED_EDGE('',*,*,#19446,.F.) ;
#27941 = ORIENTED_EDGE('',*,*,#19447,.T.) ;
#27942 = ORIENTED_EDGE('',*,*,#19448,.F.) ;
#27943 = ORIENTED_EDGE('',*,*,#19449,.F.) ;
#27944 = ORIENTED_EDGE('',*,*,#19445,.F.) ;
#27945 = ORIENTED_EDGE('',*,*,#19434,.F.) ;
#27946 = ORIENTED_EDGE('',*,*,#19439,.F.) ;
#27947 = ORIENTED_EDGE('',*,*,#19201,.T.) ;
#27948 = ORIENTED_EDGE('',*,*,#19190,.F.) ;
#27949 = ORIENTED_EDGE('',*,*,#19195,.F.) ;
#27950 = ORIENTED_EDGE('',*,*,#19197,.F.) ;
#27951 = ORIENTED_EDGE('',*,*,#19428,.T.) ;
#27952 = ORIENTED_EDGE('',*,*,#19450,.F.) ;
#27953 = ORIENTED_EDGE('',*,*,#19451,.F.) ;
#27954 = ORIENTED_EDGE('',*,*,#19421,.F.) ;
#27955 = ORIENTED_EDGE('',*,*,#19444,.F.) ;
#27956 = ORIENTED_EDGE('',*,*,#19427,.T.) ;
#27957 = ORIENTED_EDGE('',*,*,#19451,.T.) ;
#27958 = ORIENTED_EDGE('',*,*,#19448,.T.) ;
#27959 = ORIENTED_EDGE('',*,*,#19452,.T.) ;
#27960 = ORIENTED_EDGE('',*,*,#19449,.T.) ;
#27961 = ORIENTED_EDGE('',*,*,#19450,.T.) ;
#27962 = ORIENTED_EDGE('',*,*,#19424,.T.) ;
#27963 = ORIENTED_EDGE('',*,*,#19452,.F.) ;
#27964 = ORIENTED_EDGE('',*,*,#19426,.T.) ;
#27965 = ORIENTED_EDGE('',*,*,#19446,.T.) ;
#27966 = ORIENTED_EDGE('',*,*,#19453,.T.) ;
#27967 = ORIENTED_EDGE('',*,*,#19301,.T.) ;
#27968 = ORIENTED_EDGE('',*,*,#19454,.T.) ;
#27969 = ORIENTED_EDGE('',*,*,#19455,.T.) ;
#27970 = ORIENTED_EDGE('',*,*,#19456,.T.) ;
#27971 = ORIENTED_EDGE('',*,*,#19302,.T.) ;
#27972 = ORIENTED_EDGE('',*,*,#19453,.F.) ;
#27973 = ORIENTED_EDGE('',*,*,#19457,.T.) ;
#27974 = ORIENTED_EDGE('',*,*,#19456,.F.) ;
#27975 = ORIENTED_EDGE('',*,*,#19458,.T.) ;
#27976 = ORIENTED_EDGE('',*,*,#19459,.T.) ;
#27977 = ORIENTED_EDGE('',*,*,#19460,.T.) ;
#27978 = ORIENTED_EDGE('',*,*,#19300,.T.) ;
#27979 = ORIENTED_EDGE('',*,*,#19461,.T.) ;
#27980 = ORIENTED_EDGE('',*,*,#19462,.T.) ;
#27981 = ORIENTED_EDGE('',*,*,#19461,.F.) ;
#27982 = ORIENTED_EDGE('',*,*,#19305,.T.) ;
#27983 = ORIENTED_EDGE('',*,*,#19463,.T.) ;
#27984 = ORIENTED_EDGE('',*,*,#19460,.F.) ;
#27985 = ORIENTED_EDGE('',*,*,#19464,.T.) ;
#27986 = ORIENTED_EDGE('',*,*,#19454,.F.) ;
#27987 = ORIENTED_EDGE('',*,*,#19298,.F.) ;
#27988 = ORIENTED_EDGE('',*,*,#19303,.T.) ;
#27989 = ORIENTED_EDGE('',*,*,#19459,.F.) ;
#27990 = ORIENTED_EDGE('',*,*,#19465,.T.) ;
#27991 = ORIENTED_EDGE('',*,*,#19458,.F.) ;
#27992 = ORIENTED_EDGE('',*,*,#19466,.T.) ;
#27993 = ORIENTED_EDGE('',*,*,#19467,.F.) ;
#27994 = ORIENTED_EDGE('',*,*,#19468,.T.) ;
#27995 = ORIENTED_EDGE('',*,*,#19153,.F.) ;
#27996 = ORIENTED_EDGE('',*,*,#19469,.F.) ;
#27997 = ORIENTED_EDGE('',*,*,#19470,.F.) ;
#27998 = ORIENTED_EDGE('',*,*,#19466,.F.) ;
#27999 = ORIENTED_EDGE('',*,*,#19457,.F.) ;
#28000 = ORIENTED_EDGE('',*,*,#19471,.F.) ;
#28001 = ORIENTED_EDGE('',*,*,#19155,.F.) ;
#28002 = ORIENTED_EDGE('',*,*,#19158,.F.) ;
#28003 = ORIENTED_EDGE('',*,*,#19161,.F.) ;
#28004 = ORIENTED_EDGE('',*,*,#19429,.T.) ;
#28005 = ORIENTED_EDGE('',*,*,#19160,.F.) ;
#28006 = ORIENTED_EDGE('',*,*,#19159,.F.) ;
#28007 = ORIENTED_EDGE('',*,*,#19156,.F.) ;
#28008 = ORIENTED_EDGE('',*,*,#19471,.T.) ;
#28009 = ORIENTED_EDGE('',*,*,#19455,.F.) ;
#28010 = ORIENTED_EDGE('',*,*,#19462,.F.) ;
#28011 = ORIENTED_EDGE('',*,*,#19472,.F.) ;
#28012 = ORIENTED_EDGE('',*,*,#19473,.F.) ;
#28013 = ORIENTED_EDGE('',*,*,#19474,.F.) ;
#28014 = ORIENTED_EDGE('',*,*,#19475,.F.) ;
#28015 = ORIENTED_EDGE('',*,*,#19404,.F.) ;
#28016 = ORIENTED_EDGE('',*,*,#19476,.F.) ;
#28017 = ORIENTED_EDGE('',*,*,#19464,.F.) ;
#28018 = ORIENTED_EDGE('',*,*,#19474,.T.) ;
#28019 = ORIENTED_EDGE('',*,*,#19476,.T.) ;
#28020 = ORIENTED_EDGE('',*,*,#19430,.T.) ;
#28021 = ORIENTED_EDGE('',*,*,#19477,.T.) ;
#28022 = ORIENTED_EDGE('',*,*,#19401,.T.) ;
#28023 = ORIENTED_EDGE('',*,*,#19475,.T.) ;
#28024 = ORIENTED_EDGE('',*,*,#19473,.T.) ;
#28025 = ORIENTED_EDGE('',*,*,#19477,.F.) ;
#28026 = ORIENTED_EDGE('',*,*,#19478,.T.) ;
#28027 = ORIENTED_EDGE('',*,*,#19479,.T.) ;
#28028 = ORIENTED_EDGE('',*,*,#19398,.F.) ;
#28029 = ORIENTED_EDGE('',*,*,#19402,.T.) ;
#28030 = ORIENTED_EDGE('',*,*,#19479,.F.) ;
#28031 = ORIENTED_EDGE('',*,*,#19480,.T.) ;
#28032 = ORIENTED_EDGE('',*,*,#19463,.F.) ;
#28033 = ORIENTED_EDGE('',*,*,#19481,.T.) ;
#28034 = ORIENTED_EDGE('',*,*,#19478,.F.) ;
#28035 = ORIENTED_EDGE('',*,*,#19472,.T.) ;
#28036 = ORIENTED_EDGE('',*,*,#19185,.F.) ;
#28037 = ORIENTED_EDGE('',*,*,#19172,.T.) ;
#28038 = ORIENTED_EDGE('',*,*,#19180,.T.) ;
#28039 = ORIENTED_EDGE('',*,*,#19233,.F.) ;
#28040 = ORIENTED_EDGE('',*,*,#19168,.T.) ;
#28041 = ORIENTED_EDGE('',*,*,#19228,.T.) ;
#28042 = ORIENTED_EDGE('',*,*,#19482,.T.) ;
#28043 = ORIENTED_EDGE('',*,*,#19222,.F.) ;
#28044 = ORIENTED_EDGE('',*,*,#19221,.F.) ;
#28045 = ORIENTED_EDGE('',*,*,#19218,.F.) ;
#28046 = ORIENTED_EDGE('',*,*,#19483,.T.) ;
#28047 = ORIENTED_EDGE('',*,*,#19484,.F.) ;
#28048 = ORIENTED_EDGE('',*,*,#19485,.T.) ;
#28049 = ORIENTED_EDGE('',*,*,#19486,.T.) ;
#28050 = ORIENTED_EDGE('',*,*,#19487,.T.) ;
#28051 = ORIENTED_EDGE('',*,*,#19488,.T.) ;
#28052 = ORIENTED_EDGE('',*,*,#19489,.T.) ;
#28053 = ORIENTED_EDGE('',*,*,#19490,.T.) ;
#28054 = ORIENTED_EDGE('',*,*,#19491,.T.) ;
#28055 = ORIENTED_EDGE('',*,*,#19492,.T.) ;
#28056 = ORIENTED_EDGE('',*,*,#19493,.T.) ;
#28057 = ORIENTED_EDGE('',*,*,#19494,.T.) ;
#28058 = ORIENTED_EDGE('',*,*,#19495,.T.) ;
#28059 = ORIENTED_EDGE('',*,*,#19485,.F.) ;
#28060 = ORIENTED_EDGE('',*,*,#19496,.T.) ;
#28061 = ORIENTED_EDGE('',*,*,#19494,.F.) ;
#28062 = ORIENTED_EDGE('',*,*,#19497,.T.) ;
#28063 = ORIENTED_EDGE('',*,*,#19498,.T.) ;
#28064 = ORIENTED_EDGE('',*,*,#19499,.T.) ;
#28065 = ORIENTED_EDGE('',*,*,#19498,.F.) ;
#28066 = ORIENTED_EDGE('',*,*,#19500,.T.) ;
#28067 = ORIENTED_EDGE('',*,*,#19501,.T.) ;
#28068 = ORIENTED_EDGE('',*,*,#19497,.F.) ;
#28069 = ORIENTED_EDGE('',*,*,#19502,.F.) ;
#28070 = ORIENTED_EDGE('',*,*,#19503,.F.) ;
#28071 = ORIENTED_EDGE('',*,*,#19504,.F.) ;
#28072 = ORIENTED_EDGE('',*,*,#19496,.F.) ;
#28073 = ORIENTED_EDGE('',*,*,#19493,.F.) ;
#28074 = ORIENTED_EDGE('',*,*,#19492,.F.) ;
#28075 = ORIENTED_EDGE('',*,*,#19491,.F.) ;
#28076 = ORIENTED_EDGE('',*,*,#19490,.F.) ;
#28077 = ORIENTED_EDGE('',*,*,#19505,.T.) ;
#28078 = ORIENTED_EDGE('',*,*,#19506,.T.) ;
#28079 = ORIENTED_EDGE('',*,*,#19502,.T.) ;
#28080 = ORIENTED_EDGE('',*,*,#19486,.F.) ;
#28081 = ORIENTED_EDGE('',*,*,#19507,.T.) ;
#28082 = ORIENTED_EDGE('',*,*,#19508,.F.) ;
#28083 = ORIENTED_EDGE('',*,*,#19509,.F.) ;
#28084 = ORIENTED_EDGE('',*,*,#19510,.T.) ;
#28085 = ORIENTED_EDGE('',*,*,#19489,.F.) ;
#28086 = ORIENTED_EDGE('',*,*,#19488,.F.) ;
#28087 = ORIENTED_EDGE('',*,*,#19487,.F.) ;
#28088 = ORIENTED_EDGE('',*,*,#19511,.T.) ;
#28089 = ORIENTED_EDGE('',*,*,#19512,.T.) ;
#28090 = ORIENTED_EDGE('',*,*,#19513,.T.) ;
#28091 = ORIENTED_EDGE('',*,*,#19514,.T.) ;
#28092 = ORIENTED_EDGE('',*,*,#19515,.T.) ;
#28093 = ORIENTED_EDGE('',*,*,#19511,.F.) ;
#28094 = ORIENTED_EDGE('',*,*,#19516,.T.) ;
#28095 = ORIENTED_EDGE('',*,*,#19514,.F.) ;
#28096 = ORIENTED_EDGE('',*,*,#19517,.T.) ;
#28097 = ORIENTED_EDGE('',*,*,#19518,.T.) ;
#28098 = ORIENTED_EDGE('',*,*,#19519,.T.) ;
#28099 = ORIENTED_EDGE('',*,*,#19520,.T.) ;
#28100 = ORIENTED_EDGE('',*,*,#19521,.T.) ;
#28101 = ORIENTED_EDGE('',*,*,#19509,.T.) ;
#28102 = ORIENTED_EDGE('',*,*,#19508,.T.) ;
#28103 = ORIENTED_EDGE('',*,*,#19518,.F.) ;
#28104 = ORIENTED_EDGE('',*,*,#19520,.F.) ;
#28105 = ORIENTED_EDGE('',*,*,#19517,.F.) ;
#28106 = ORIENTED_EDGE('',*,*,#19522,.T.) ;
#28107 = ORIENTED_EDGE('',*,*,#19523,.T.) ;
#28108 = ORIENTED_EDGE('',*,*,#19524,.T.) ;
#28109 = ORIENTED_EDGE('',*,*,#19521,.F.) ;
#28110 = ORIENTED_EDGE('',*,*,#19516,.F.) ;
#28111 = ORIENTED_EDGE('',*,*,#19525,.F.) ;
#28112 = ORIENTED_EDGE('',*,*,#19526,.F.) ;
#28113 = ORIENTED_EDGE('',*,*,#19522,.F.) ;
#28114 = ORIENTED_EDGE('',*,*,#19513,.F.) ;
#28115 = ORIENTED_EDGE('',*,*,#19527,.T.) ;
#28116 = ORIENTED_EDGE('',*,*,#19528,.F.) ;
#28117 = ORIENTED_EDGE('',*,*,#19525,.T.) ;
#28118 = ORIENTED_EDGE('',*,*,#19225,.F.) ;
#28119 = ORIENTED_EDGE('',*,*,#19482,.F.) ;
#28120 = ORIENTED_EDGE('',*,*,#19529,.F.) ;
#28121 = ORIENTED_EDGE('',*,*,#19505,.F.) ;
#28122 = ORIENTED_EDGE('',*,*,#19510,.F.) ;
#28123 = ORIENTED_EDGE('',*,*,#19524,.F.) ;
#28124 = ORIENTED_EDGE('',*,*,#19530,.F.) ;
#28125 = ORIENTED_EDGE('',*,*,#19531,.F.) ;
#28126 = ORIENTED_EDGE('',*,*,#19532,.T.) ;
#28127 = ORIENTED_EDGE('',*,*,#19533,.T.) ;
#28128 = ORIENTED_EDGE('',*,*,#19534,.T.) ;
#28129 = ORIENTED_EDGE('',*,*,#19535,.T.) ;
#28130 = ORIENTED_EDGE('',*,*,#19534,.F.) ;
#28131 = ORIENTED_EDGE('',*,*,#19536,.T.) ;
#28132 = ORIENTED_EDGE('',*,*,#19537,.T.) ;
#28133 = ORIENTED_EDGE('',*,*,#19538,.T.) ;
#28134 = ORIENTED_EDGE('',*,*,#19539,.T.) ;
#28135 = ORIENTED_EDGE('',*,*,#19540,.T.) ;
#28136 = ORIENTED_EDGE('',*,*,#19541,.T.) ;
#28137 = ORIENTED_EDGE('',*,*,#19542,.T.) ;
#28138 = ORIENTED_EDGE('',*,*,#19250,.T.) ;
#28139 = ORIENTED_EDGE('',*,*,#19540,.F.) ;
#28140 = ORIENTED_EDGE('',*,*,#19543,.T.) ;
#28141 = ORIENTED_EDGE('',*,*,#19542,.F.) ;
#28142 = ORIENTED_EDGE('',*,*,#19544,.T.) ;
#28143 = ORIENTED_EDGE('',*,*,#19545,.T.) ;
#28144 = ORIENTED_EDGE('',*,*,#19538,.F.) ;
#28145 = ORIENTED_EDGE('',*,*,#19546,.T.) ;
#28146 = ORIENTED_EDGE('',*,*,#19532,.F.) ;
#28147 = ORIENTED_EDGE('',*,*,#19254,.F.) ;
#28148 = ORIENTED_EDGE('',*,*,#19547,.T.) ;
#28149 = ORIENTED_EDGE('',*,*,#19537,.F.) ;
#28150 = ORIENTED_EDGE('',*,*,#19548,.T.) ;
#28151 = ORIENTED_EDGE('',*,*,#19536,.F.) ;
#28152 = ORIENTED_EDGE('',*,*,#19549,.T.) ;
#28153 = ORIENTED_EDGE('',*,*,#19550,.F.) ;
#28154 = ORIENTED_EDGE('',*,*,#19551,.T.) ;
#28155 = ORIENTED_EDGE('',*,*,#19552,.F.) ;
#28156 = ORIENTED_EDGE('',*,*,#19553,.F.) ;
#28157 = ORIENTED_EDGE('',*,*,#19549,.F.) ;
#28158 = ORIENTED_EDGE('',*,*,#19533,.F.) ;
#28159 = ORIENTED_EDGE('',*,*,#19541,.F.) ;
#28160 = ORIENTED_EDGE('',*,*,#19249,.T.) ;
#28161 = ORIENTED_EDGE('',*,*,#19238,.F.) ;
#28162 = ORIENTED_EDGE('',*,*,#19243,.F.) ;
#28163 = ORIENTED_EDGE('',*,*,#19245,.F.) ;
#28164 = ORIENTED_EDGE('',*,*,#19531,.T.) ;
#28165 = ORIENTED_EDGE('',*,*,#19554,.F.) ;
#28166 = ORIENTED_EDGE('',*,*,#19555,.F.) ;
#28167 = ORIENTED_EDGE('',*,*,#19523,.F.) ;
#28168 = ORIENTED_EDGE('',*,*,#19546,.F.) ;
#28169 = ORIENTED_EDGE('',*,*,#19530,.T.) ;
#28170 = ORIENTED_EDGE('',*,*,#19555,.T.) ;
#28171 = ORIENTED_EDGE('',*,*,#19552,.T.) ;
#28172 = ORIENTED_EDGE('',*,*,#19556,.T.) ;
#28173 = ORIENTED_EDGE('',*,*,#19528,.T.) ;
#28174 = ORIENTED_EDGE('',*,*,#19550,.T.) ;
#28175 = ORIENTED_EDGE('',*,*,#19556,.F.) ;
#28176 = ORIENTED_EDGE('',*,*,#19553,.T.) ;
#28177 = ORIENTED_EDGE('',*,*,#19554,.T.) ;
#28178 = ORIENTED_EDGE('',*,*,#19526,.T.) ;
#28179 = ORIENTED_EDGE('',*,*,#19258,.F.) ;
#28180 = ORIENTED_EDGE('',*,*,#19557,.F.) ;
#28181 = ORIENTED_EDGE('',*,*,#19543,.F.) ;
#28182 = ORIENTED_EDGE('',*,*,#19539,.F.) ;
#28183 = ORIENTED_EDGE('',*,*,#19535,.F.) ;
#28184 = ORIENTED_EDGE('',*,*,#19547,.F.) ;
#28185 = ORIENTED_EDGE('',*,*,#19558,.T.) ;
#28186 = ORIENTED_EDGE('',*,*,#19349,.T.) ;
#28187 = ORIENTED_EDGE('',*,*,#19559,.T.) ;
#28188 = ORIENTED_EDGE('',*,*,#19484,.T.) ;
#28189 = ORIENTED_EDGE('',*,*,#19560,.T.) ;
#28190 = ORIENTED_EDGE('',*,*,#19350,.T.) ;
#28191 = ORIENTED_EDGE('',*,*,#19558,.F.) ;
#28192 = ORIENTED_EDGE('',*,*,#19561,.T.) ;
#28193 = ORIENTED_EDGE('',*,*,#19560,.F.) ;
#28194 = ORIENTED_EDGE('',*,*,#19562,.T.) ;
#28195 = ORIENTED_EDGE('',*,*,#19563,.T.) ;
#28196 = ORIENTED_EDGE('',*,*,#19564,.T.) ;
#28197 = ORIENTED_EDGE('',*,*,#19348,.T.) ;
#28198 = ORIENTED_EDGE('',*,*,#19565,.T.) ;
#28199 = ORIENTED_EDGE('',*,*,#19566,.T.) ;
#28200 = ORIENTED_EDGE('',*,*,#19565,.F.) ;
#28201 = ORIENTED_EDGE('',*,*,#19353,.T.) ;
#28202 = ORIENTED_EDGE('',*,*,#19567,.T.) ;
#28203 = ORIENTED_EDGE('',*,*,#19564,.F.) ;
#28204 = ORIENTED_EDGE('',*,*,#19568,.T.) ;
#28205 = ORIENTED_EDGE('',*,*,#19559,.F.) ;
#28206 = ORIENTED_EDGE('',*,*,#19346,.F.) ;
#28207 = ORIENTED_EDGE('',*,*,#19351,.T.) ;
#28208 = ORIENTED_EDGE('',*,*,#19563,.F.) ;
#28209 = ORIENTED_EDGE('',*,*,#19569,.T.) ;
#28210 = ORIENTED_EDGE('',*,*,#19562,.F.) ;
#28211 = ORIENTED_EDGE('',*,*,#19570,.T.) ;
#28212 = ORIENTED_EDGE('',*,*,#19571,.T.) ;
#28213 = ORIENTED_EDGE('',*,*,#19572,.T.) ;
#28214 = ORIENTED_EDGE('',*,*,#19215,.F.) ;
#28215 = ORIENTED_EDGE('',*,*,#19573,.F.) ;
#28216 = ORIENTED_EDGE('',*,*,#19574,.F.) ;
#28217 = ORIENTED_EDGE('',*,*,#19570,.F.) ;
#28218 = ORIENTED_EDGE('',*,*,#19561,.F.) ;
#28219 = ORIENTED_EDGE('',*,*,#19483,.F.) ;
#28220 = ORIENTED_EDGE('',*,*,#19217,.F.) ;
#28221 = ORIENTED_EDGE('',*,*,#19220,.F.) ;
#28222 = ORIENTED_EDGE('',*,*,#19223,.F.) ;
#28223 = ORIENTED_EDGE('',*,*,#19566,.F.) ;
#28224 = ORIENTED_EDGE('',*,*,#19575,.F.) ;
#28225 = ORIENTED_EDGE('',*,*,#19576,.F.) ;
#28226 = ORIENTED_EDGE('',*,*,#19577,.F.) ;
#28227 = ORIENTED_EDGE('',*,*,#19578,.F.) ;
#28228 = ORIENTED_EDGE('',*,*,#19506,.F.) ;
#28229 = ORIENTED_EDGE('',*,*,#19579,.F.) ;
#28230 = ORIENTED_EDGE('',*,*,#19568,.F.) ;
#28231 = ORIENTED_EDGE('',*,*,#19577,.T.) ;
#28232 = ORIENTED_EDGE('',*,*,#19579,.T.) ;
#28233 = ORIENTED_EDGE('',*,*,#19529,.T.) ;
#28234 = ORIENTED_EDGE('',*,*,#19580,.T.) ;
#28235 = ORIENTED_EDGE('',*,*,#19503,.T.) ;
#28236 = ORIENTED_EDGE('',*,*,#19578,.T.) ;
#28237 = ORIENTED_EDGE('',*,*,#19576,.T.) ;
#28238 = ORIENTED_EDGE('',*,*,#19580,.F.) ;
#28239 = ORIENTED_EDGE('',*,*,#19581,.T.) ;
#28240 = ORIENTED_EDGE('',*,*,#19582,.T.) ;
#28241 = ORIENTED_EDGE('',*,*,#19500,.F.) ;
#28242 = ORIENTED_EDGE('',*,*,#19504,.T.) ;
#28243 = ORIENTED_EDGE('',*,*,#19582,.F.) ;
#28244 = ORIENTED_EDGE('',*,*,#19583,.T.) ;
#28245 = ORIENTED_EDGE('',*,*,#19567,.F.) ;
#28246 = ORIENTED_EDGE('',*,*,#19584,.T.) ;
#28247 = ORIENTED_EDGE('',*,*,#19581,.F.) ;
#28248 = ORIENTED_EDGE('',*,*,#19575,.T.) ;
#28249 = ORIENTED_EDGE('',*,*,#19399,.F.) ;
#28250 = ORIENTED_EDGE('',*,*,#19585,.T.) ;
#28251 = ORIENTED_EDGE('',*,*,#19410,.F.) ;
#28252 = ORIENTED_EDGE('',*,*,#19586,.T.) ;
#28253 = ORIENTED_EDGE('',*,*,#19275,.F.) ;
#28254 = ORIENTED_EDGE('',*,*,#19587,.T.) ;
#28255 = ORIENTED_EDGE('',*,*,#19277,.F.) ;
#28256 = ORIENTED_EDGE('',*,*,#19588,.T.) ;
#28257 = ORIENTED_EDGE('',*,*,#19501,.F.) ;
#28258 = ORIENTED_EDGE('',*,*,#19589,.T.) ;
#28259 = ORIENTED_EDGE('',*,*,#19512,.F.) ;
#28260 = ORIENTED_EDGE('',*,*,#19590,.T.) ;
#28261 = ORIENTED_EDGE('',*,*,#19358,.F.) ;
#28262 = ORIENTED_EDGE('',*,*,#19591,.F.) ;
#28263 = ORIENTED_EDGE('',*,*,#19441,.F.) ;
#28264 = ORIENTED_EDGE('',*,*,#19437,.F.) ;
#28265 = ORIENTED_EDGE('',*,*,#19435,.F.) ;
#28266 = ORIENTED_EDGE('',*,*,#19362,.F.) ;
#28267 = ORIENTED_EDGE('',*,*,#19499,.F.) ;
#28268 = ORIENTED_EDGE('',*,*,#19590,.F.) ;
#28269 = ORIENTED_EDGE('',*,*,#19515,.F.) ;
#28270 = ORIENTED_EDGE('',*,*,#19519,.F.) ;
#28271 = ORIENTED_EDGE('',*,*,#19507,.F.) ;
#28272 = ORIENTED_EDGE('',*,*,#19495,.F.) ;
#28273 = ORIENTED_EDGE('',*,*,#19589,.F.) ;
#28274 = ORIENTED_EDGE('',*,*,#19583,.F.) ;
#28275 = ORIENTED_EDGE('',*,*,#19584,.F.) ;
#28276 = ORIENTED_EDGE('',*,*,#19352,.F.) ;
#28277 = ORIENTED_EDGE('',*,*,#19340,.F.) ;
#28278 = ORIENTED_EDGE('',*,*,#19323,.F.) ;
#28279 = ORIENTED_EDGE('',*,*,#19327,.F.) ;
#28280 = ORIENTED_EDGE('',*,*,#19364,.F.) ;
#28281 = ORIENTED_EDGE('',*,*,#19447,.F.) ;
#28282 = ORIENTED_EDGE('',*,*,#19425,.F.) ;
#28283 = ORIENTED_EDGE('',*,*,#19585,.F.) ;
#28284 = ORIENTED_EDGE('',*,*,#19480,.F.) ;
#28285 = ORIENTED_EDGE('',*,*,#19481,.F.) ;
#28286 = ORIENTED_EDGE('',*,*,#19304,.F.) ;
#28287 = ORIENTED_EDGE('',*,*,#19292,.F.) ;
#28288 = ORIENTED_EDGE('',*,*,#19587,.F.) ;
#28289 = ORIENTED_EDGE('',*,*,#19267,.F.) ;
#28290 = ORIENTED_EDGE('',*,*,#19548,.F.) ;
#28291 = ORIENTED_EDGE('',*,*,#19551,.F.) ;
#28292 = ORIENTED_EDGE('',*,*,#19527,.F.) ;
#28293 = ORIENTED_EDGE('',*,*,#19545,.F.) ;
#28294 = ORIENTED_EDGE('',*,*,#19592,.T.) ;
#28295 = ORIENTED_EDGE('',*,*,#19593,.T.) ;
#28296 = ORIENTED_EDGE('',*,*,#19251,.T.) ;
#28297 = ORIENTED_EDGE('',*,*,#19247,.T.) ;
#28298 = ORIENTED_EDGE('',*,*,#19252,.T.) ;
#28299 = ORIENTED_EDGE('',*,*,#19593,.F.) ;
#28300 = ORIENTED_EDGE('',*,*,#19594,.T.) ;
#28301 = ORIENTED_EDGE('',*,*,#19260,.F.) ;
#28302 = ORIENTED_EDGE('',*,*,#19595,.T.) ;
#28303 = ORIENTED_EDGE('',*,*,#19544,.F.) ;
#28304 = ORIENTED_EDGE('',*,*,#19557,.T.) ;
#28305 = ORIENTED_EDGE('',*,*,#19272,.F.) ;
#28306 = ORIENTED_EDGE('',*,*,#19596,.T.) ;
#28307 = ORIENTED_EDGE('',*,*,#19283,.F.) ;
#28308 = ORIENTED_EDGE('',*,*,#19286,.F.) ;
#28309 = ORIENTED_EDGE('',*,*,#19597,.T.) ;
#28310 = ORIENTED_EDGE('',*,*,#19269,.F.) ;
#28311 = ORIENTED_EDGE('',*,*,#19144,.F.) ;
#28312 = ORIENTED_EDGE('',*,*,#19598,.T.) ;
#28313 = ORIENTED_EDGE('',*,*,#19599,.T.) ;
#28314 = ORIENTED_EDGE('',*,*,#19469,.T.) ;
#28315 = ORIENTED_EDGE('',*,*,#19150,.F.) ;
#28316 = ORIENTED_EDGE('',*,*,#19145,.F.) ;
#28317 = ORIENTED_EDGE('',*,*,#19467,.T.) ;
#28318 = ORIENTED_EDGE('',*,*,#19470,.T.) ;
#28319 = ORIENTED_EDGE('',*,*,#19599,.F.) ;
#28320 = ORIENTED_EDGE('',*,*,#19600,.T.) ;
#28321 = ORIENTED_EDGE('',*,*,#19592,.F.) ;
#28322 = ORIENTED_EDGE('',*,*,#19595,.F.) ;
#28323 = ORIENTED_EDGE('',*,*,#19263,.F.) ;
#28324 = ORIENTED_EDGE('',*,*,#19597,.F.) ;
#28325 = ORIENTED_EDGE('',*,*,#19289,.F.) ;
#28326 = ORIENTED_EDGE('',*,*,#19465,.F.) ;
#28327 = ORIENTED_EDGE('',*,*,#19468,.F.) ;
#28328 = ORIENTED_EDGE('',*,*,#19601,.T.) ;
#28329 = ORIENTED_EDGE('',*,*,#19594,.F.) ;
#28330 = ORIENTED_EDGE('',*,*,#19601,.F.) ;
#28331 = ORIENTED_EDGE('',*,*,#19600,.F.) ;
#28332 = ORIENTED_EDGE('',*,*,#19602,.T.) ;
#28333 = ORIENTED_EDGE('',*,*,#19248,.F.) ;
#28334 = ORIENTED_EDGE('',*,*,#19602,.F.) ;
#28335 = ORIENTED_EDGE('',*,*,#19598,.F.) ;
#28336 = ORIENTED_EDGE('',*,*,#19170,.T.) ;
#28337 = ORIENTED_EDGE('',*,*,#19603,.T.) ;
#28338 = ORIENTED_EDGE('',*,*,#19604,.T.) ;
#28339 = ORIENTED_EDGE('',*,*,#19199,.F.) ;
#28340 = ORIENTED_EDGE('',*,*,#19204,.T.) ;
#28341 = ORIENTED_EDGE('',*,*,#19443,.F.) ;
#28342 = ORIENTED_EDGE('',*,*,#19605,.T.) ;
#28343 = ORIENTED_EDGE('',*,*,#19603,.F.) ;
#28344 = ORIENTED_EDGE('',*,*,#19203,.T.) ;
#28345 = ORIENTED_EDGE('',*,*,#19360,.F.) ;
#28346 = ORIENTED_EDGE('',*,*,#19606,.T.) ;
#28347 = ORIENTED_EDGE('',*,*,#19442,.F.) ;
#28348 = ORIENTED_EDGE('',*,*,#19591,.T.) ;
#28349 = ORIENTED_EDGE('',*,*,#19316,.F.) ;
#28350 = ORIENTED_EDGE('',*,*,#19607,.T.) ;
#28351 = ORIENTED_EDGE('',*,*,#19359,.F.) ;
#28352 = ORIENTED_EDGE('',*,*,#19361,.T.) ;
#28353 = ORIENTED_EDGE('',*,*,#19608,.T.) ;
#28354 = ORIENTED_EDGE('',*,*,#19609,.T.) ;
#28355 = ORIENTED_EDGE('',*,*,#19571,.F.) ;
#28356 = ORIENTED_EDGE('',*,*,#19574,.T.) ;
#28357 = ORIENTED_EDGE('',*,*,#19206,.F.) ;
#28358 = ORIENTED_EDGE('',*,*,#19610,.T.) ;
#28359 = ORIENTED_EDGE('',*,*,#19608,.F.) ;
#28360 = ORIENTED_EDGE('',*,*,#19573,.T.) ;
#28361 = ORIENTED_EDGE('',*,*,#19212,.F.) ;
#28362 = ORIENTED_EDGE('',*,*,#19207,.F.) ;
#28363 = ORIENTED_EDGE('',*,*,#19605,.F.) ;
#28364 = ORIENTED_EDGE('',*,*,#19606,.F.) ;
#28365 = ORIENTED_EDGE('',*,*,#19607,.F.) ;
#28366 = ORIENTED_EDGE('',*,*,#19320,.F.) ;
#28367 = ORIENTED_EDGE('',*,*,#19337,.F.) ;
#28368 = ORIENTED_EDGE('',*,*,#19569,.F.) ;
#28369 = ORIENTED_EDGE('',*,*,#19572,.F.) ;
#28370 = ORIENTED_EDGE('',*,*,#19611,.T.) ;
#28371 = ORIENTED_EDGE('',*,*,#19604,.F.) ;
#28372 = ORIENTED_EDGE('',*,*,#19611,.F.) ;
#28373 = ORIENTED_EDGE('',*,*,#19609,.F.) ;
#28374 = ORIENTED_EDGE('',*,*,#19612,.T.) ;
#28375 = ORIENTED_EDGE('',*,*,#19200,.F.) ;
#28376 = ORIENTED_EDGE('',*,*,#19612,.F.) ;
#28377 = ORIENTED_EDGE('',*,*,#19610,.F.) ;
#28378 = ORIENTED_EDGE('',*,*,#19164,.T.) ;
#28379 = ORIENTED_EDGE('',*,*,#19174,.T.) ;
#28380 = ORIENTED_EDGE('',*,*,#19613,.T.) ;
#28381 = ORIENTED_EDGE('',*,*,#19614,.T.) ;
#28382 = ORIENTED_EDGE('',*,*,#19615,.F.) ;
#28383 = ORIENTED_EDGE('',*,*,#19614,.F.) ;
#28384 = ORIENTED_EDGE('',*,*,#19616,.T.) ;
#28385 = ORIENTED_EDGE('',*,*,#19111,.T.) ;
#28386 = ORIENTED_EDGE('',*,*,#19141,.T.) ;
#28387 = ORIENTED_EDGE('',*,*,#19382,.T.) ;
#28388 = ORIENTED_EDGE('',*,*,#19116,.F.) ;
#28389 = ORIENTED_EDGE('',*,*,#19274,.F.) ;
#28390 = ORIENTED_EDGE('',*,*,#19588,.F.) ;
#28391 = ORIENTED_EDGE('',*,*,#19280,.F.) ;
#28392 = ORIENTED_EDGE('',*,*,#19596,.F.) ;
#28393 = ORIENTED_EDGE('',*,*,#19397,.F.) ;
#28394 = ORIENTED_EDGE('',*,*,#19586,.F.) ;
#28395 = ORIENTED_EDGE('',*,*,#19413,.F.) ;
#28396 = ORIENTED_EDGE('',*,*,#19417,.F.) ;
#28397 = ORIENTED_EDGE('',*,*,#19405,.F.) ;
#28398 = ORIENTED_EDGE('',*,*,#19393,.F.) ;
#28399 = ORIENTED_EDGE('',*,*,#19615,.T.) ;
#28400 = ORIENTED_EDGE('',*,*,#19380,.F.) ;
#28401 = ORIENTED_EDGE('',*,*,#19379,.F.) ;
#28402 = ORIENTED_EDGE('',*,*,#19378,.F.) ;
#28403 = ORIENTED_EDGE('',*,*,#19377,.F.) ;
#28404 = ORIENTED_EDGE('',*,*,#19089,.F.) ;
#28405 = ORIENTED_EDGE('',*,*,#19093,.F.) ;
#28406 = ORIENTED_EDGE('',*,*,#19096,.F.) ;
#28407 = ORIENTED_EDGE('',*,*,#19099,.F.) ;
#28408 = ORIENTED_EDGE('',*,*,#19102,.F.) ;
#28409 = ORIENTED_EDGE('',*,*,#19105,.F.) ;
#28410 = ORIENTED_EDGE('',*,*,#19108,.F.) ;
#28411 = ORIENTED_EDGE('',*,*,#19112,.F.) ;
#28412 = ORIENTED_EDGE('',*,*,#19616,.F.) ;
#28413 = ORIENTED_EDGE('',*,*,#19613,.F.) ;
#28414 = ORIENTED_EDGE('',*,*,#19115,.T.) ;
#28415 = ORIENTED_EDGE('',*,*,#19119,.T.) ;
#28416 = ORIENTED_EDGE('',*,*,#19122,.T.) ;
#28417 = ORIENTED_EDGE('',*,*,#19125,.T.) ;
#28418 = ORIENTED_EDGE('',*,*,#19128,.T.) ;
#28419 = ORIENTED_EDGE('',*,*,#19131,.T.) ;
#28420 = ORIENTED_EDGE('',*,*,#19134,.T.) ;
#28421 = ORIENTED_EDGE('',*,*,#19139,.T.) ;
#28422 = ORIENTED_EDGE('',*,*,#19617,.T.) ;
#28423 = ORIENTED_EDGE('',*,*,#19618,.T.) ;
#28424 = ORIENTED_EDGE('',*,*,#19619,.F.) ;
#28425 = ORIENTED_EDGE('',*,*,#19620,.F.) ;
#28426 = ORIENTED_EDGE('',*,*,#19621,.T.) ;
#28427 = ORIENTED_EDGE('',*,*,#19622,.T.) ;
#28428 = ORIENTED_EDGE('',*,*,#19617,.F.) ;
#28429 = ORIENTED_EDGE('',*,*,#19623,.F.) ;
#28430 = ORIENTED_EDGE('',*,*,#19624,.T.) ;
#28431 = ORIENTED_EDGE('',*,*,#19625,.T.) ;
#28432 = ORIENTED_EDGE('',*,*,#19621,.F.) ;
#28433 = ORIENTED_EDGE('',*,*,#19626,.F.) ;
#28434 = ORIENTED_EDGE('',*,*,#19627,.F.) ;
#28435 = ORIENTED_EDGE('',*,*,#19628,.F.) ;
#28436 = ORIENTED_EDGE('',*,*,#19629,.F.) ;
#28437 = ORIENTED_EDGE('',*,*,#19630,.T.) ;
#28438 = ORIENTED_EDGE('',*,*,#19631,.T.) ;
#28439 = ORIENTED_EDGE('',*,*,#19632,.T.) ;
#28440 = ORIENTED_EDGE('',*,*,#19633,.F.) ;
#28441 = ORIENTED_EDGE('',*,*,#19634,.T.) ;
#28442 = ORIENTED_EDGE('',*,*,#19635,.T.) ;
#28443 = ORIENTED_EDGE('',*,*,#19636,.T.) ;
#28444 = ORIENTED_EDGE('',*,*,#19631,.F.) ;
#28445 = ORIENTED_EDGE('',*,*,#19637,.T.) ;
#28446 = ORIENTED_EDGE('',*,*,#19638,.T.) ;
#28447 = ORIENTED_EDGE('',*,*,#19639,.T.) ;
#28448 = ORIENTED_EDGE('',*,*,#19635,.F.) ;
#28449 = ORIENTED_EDGE('',*,*,#19640,.T.) ;
#28450 = ORIENTED_EDGE('',*,*,#19641,.F.) ;
#28451 = ORIENTED_EDGE('',*,*,#19642,.T.) ;
#28452 = ORIENTED_EDGE('',*,*,#19643,.F.) ;
#28453 = ORIENTED_EDGE('',*,*,#19644,.T.) ;
#28454 = ORIENTED_EDGE('',*,*,#19641,.T.) ;
#28455 = ORIENTED_EDGE('',*,*,#19645,.T.) ;
#28456 = ORIENTED_EDGE('',*,*,#19638,.F.) ;
#28457 = ORIENTED_EDGE('',*,*,#19646,.T.) ;
#28458 = ORIENTED_EDGE('',*,*,#19627,.T.) ;
#28459 = ORIENTED_EDGE('',*,*,#19647,.T.) ;
#28460 = ORIENTED_EDGE('',*,*,#19624,.F.) ;
#28461 = ORIENTED_EDGE('',*,*,#19648,.F.) ;
#28462 = ORIENTED_EDGE('',*,*,#19649,.T.) ;
#28463 = ORIENTED_EDGE('',*,*,#19650,.T.) ;
#28464 = ORIENTED_EDGE('',*,*,#19651,.T.) ;
#28465 = ORIENTED_EDGE('',*,*,#19652,.T.) ;
#28466 = ORIENTED_EDGE('',*,*,#19653,.F.) ;
#28467 = ORIENTED_EDGE('',*,*,#19654,.F.) ;
#28468 = ORIENTED_EDGE('',*,*,#19655,.T.) ;
#28469 = ORIENTED_EDGE('',*,*,#19656,.F.) ;
#28470 = ORIENTED_EDGE('',*,*,#19657,.T.) ;
#28471 = ORIENTED_EDGE('',*,*,#19658,.T.) ;
#28472 = ORIENTED_EDGE('',*,*,#19654,.T.) ;
#28473 = ORIENTED_EDGE('',*,*,#19659,.T.) ;
#28474 = ORIENTED_EDGE('',*,*,#19660,.F.) ;
#28475 = ORIENTED_EDGE('',*,*,#19661,.F.) ;
#28476 = ORIENTED_EDGE('',*,*,#19662,.T.) ;
#28477 = ORIENTED_EDGE('',*,*,#19663,.F.) ;
#28478 = ORIENTED_EDGE('',*,*,#19664,.F.) ;
#28479 = ORIENTED_EDGE('',*,*,#19665,.F.) ;
#28480 = ORIENTED_EDGE('',*,*,#19666,.T.) ;
#28481 = ORIENTED_EDGE('',*,*,#19667,.F.) ;
#28482 = ORIENTED_EDGE('',*,*,#19668,.T.) ;
#28483 = ORIENTED_EDGE('',*,*,#19669,.T.) ;
#28484 = ORIENTED_EDGE('',*,*,#19665,.T.) ;
#28485 = ORIENTED_EDGE('',*,*,#19670,.T.) ;
#28486 = ORIENTED_EDGE('',*,*,#19671,.T.) ;
#28487 = ORIENTED_EDGE('',*,*,#19672,.T.) ;
#28488 = ORIENTED_EDGE('',*,*,#19668,.F.) ;
#28489 = ORIENTED_EDGE('',*,*,#19673,.T.) ;
#28490 = ORIENTED_EDGE('',*,*,#19656,.T.) ;
#28491 = ORIENTED_EDGE('',*,*,#19674,.T.) ;
#28492 = ORIENTED_EDGE('',*,*,#19671,.F.) ;
#28493 = ORIENTED_EDGE('',*,*,#19675,.T.) ;
#28494 = ORIENTED_EDGE('',*,*,#19676,.T.) ;
#28495 = ORIENTED_EDGE('',*,*,#19677,.T.) ;
#28496 = ORIENTED_EDGE('',*,*,#19667,.T.) ;
#28497 = ORIENTED_EDGE('',*,*,#19678,.T.) ;
#28498 = ORIENTED_EDGE('',*,*,#19679,.F.) ;
#28499 = ORIENTED_EDGE('',*,*,#19680,.F.) ;
#28500 = ORIENTED_EDGE('',*,*,#19681,.T.) ;
#28501 = ORIENTED_EDGE('',*,*,#19682,.F.) ;
#28502 = ORIENTED_EDGE('',*,*,#19683,.T.) ;
#28503 = ORIENTED_EDGE('',*,*,#19684,.T.) ;
#28504 = ORIENTED_EDGE('',*,*,#19680,.T.) ;
#28505 = ORIENTED_EDGE('',*,*,#19685,.T.) ;
#28506 = ORIENTED_EDGE('',*,*,#19686,.T.) ;
#28507 = ORIENTED_EDGE('',*,*,#19687,.T.) ;
#28508 = ORIENTED_EDGE('',*,*,#19661,.T.) ;
#28509 = ORIENTED_EDGE('',*,*,#19688,.T.) ;
#28510 = ORIENTED_EDGE('',*,*,#19689,.T.) ;
#28511 = ORIENTED_EDGE('',*,*,#19690,.T.) ;
#28512 = ORIENTED_EDGE('',*,*,#19686,.F.) ;
#28513 = ORIENTED_EDGE('',*,*,#19691,.T.) ;
#28514 = ORIENTED_EDGE('',*,*,#19682,.T.) ;
#28515 = ORIENTED_EDGE('',*,*,#19692,.T.) ;
#28516 = ORIENTED_EDGE('',*,*,#19689,.F.) ;
#28517 = ORIENTED_EDGE('',*,*,#19693,.T.) ;
#28518 = ORIENTED_EDGE('',*,*,#19679,.T.) ;
#28519 = ORIENTED_EDGE('',*,*,#19694,.T.) ;
#28520 = ORIENTED_EDGE('',*,*,#19664,.T.) ;
#28521 = ORIENTED_EDGE('',*,*,#19695,.T.) ;
#28522 = ORIENTED_EDGE('',*,*,#19696,.T.) ;
#28523 = ORIENTED_EDGE('',*,*,#19697,.T.) ;
#28524 = ORIENTED_EDGE('',*,*,#19663,.T.) ;
#28525 = ORIENTED_EDGE('',*,*,#19698,.T.) ;
#28526 = ORIENTED_EDGE('',*,*,#19653,.T.) ;
#28527 = ORIENTED_EDGE('',*,*,#19699,.T.) ;
#28528 = ORIENTED_EDGE('',*,*,#19660,.T.) ;
#28529 = ORIENTED_EDGE('',*,*,#19700,.T.) ;
#28530 = ORIENTED_EDGE('',*,*,#19683,.F.) ;
#28531 = ORIENTED_EDGE('',*,*,#19649,.F.) ;
#28532 = ORIENTED_EDGE('',*,*,#19701,.T.) ;
#28533 = ORIENTED_EDGE('',*,*,#19651,.F.) ;
#28534 = ORIENTED_EDGE('',*,*,#19676,.F.) ;
#28535 = ORIENTED_EDGE('',*,*,#19702,.T.) ;
#28536 = ORIENTED_EDGE('',*,*,#19703,.T.) ;
#28537 = ORIENTED_EDGE('',*,*,#19704,.T.) ;
#28538 = ORIENTED_EDGE('',*,*,#19705,.T.) ;
#28539 = ORIENTED_EDGE('',*,*,#19706,.T.) ;
#28540 = ORIENTED_EDGE('',*,*,#19703,.F.) ;
#28541 = ORIENTED_EDGE('',*,*,#19696,.F.) ;
#28542 = ORIENTED_EDGE('',*,*,#19707,.T.) ;
#28543 = ORIENTED_EDGE('',*,*,#19657,.F.) ;
#28544 = ORIENTED_EDGE('',*,*,#19705,.F.) ;
#28545 = ORIENTED_EDGE('',*,*,#19708,.T.) ;
#28546 = ORIENTED_EDGE('',*,*,#19670,.F.) ;
#28547 = ORIENTED_EDGE('',*,*,#19694,.F.) ;
#28548 = ORIENTED_EDGE('',*,*,#19693,.F.) ;
#28549 = ORIENTED_EDGE('',*,*,#19709,.T.) ;
#28550 = ORIENTED_EDGE('',*,*,#19702,.F.) ;
#28551 = ORIENTED_EDGE('',*,*,#19710,.T.) ;
#28552 = ORIENTED_EDGE('',*,*,#19711,.F.) ;
#28553 = ORIENTED_EDGE('',*,*,#19712,.F.) ;
#28554 = ORIENTED_EDGE('',*,*,#19678,.F.) ;
#28555 = ORIENTED_EDGE('',*,*,#19666,.F.) ;
#28556 = ORIENTED_EDGE('',*,*,#19669,.F.) ;
#28557 = ORIENTED_EDGE('',*,*,#19672,.F.) ;
#28558 = ORIENTED_EDGE('',*,*,#19674,.F.) ;
#28559 = ORIENTED_EDGE('',*,*,#19655,.F.) ;
#28560 = ORIENTED_EDGE('',*,*,#19658,.F.) ;
#28561 = ORIENTED_EDGE('',*,*,#19713,.F.) ;
#28562 = ORIENTED_EDGE('',*,*,#19714,.T.) ;
#28563 = ORIENTED_EDGE('',*,*,#19715,.F.) ;
#28564 = ORIENTED_EDGE('',*,*,#19716,.T.) ;
#28565 = ORIENTED_EDGE('',*,*,#19710,.F.) ;
#28566 = ORIENTED_EDGE('',*,*,#19708,.F.) ;
#28567 = ORIENTED_EDGE('',*,*,#19717,.T.) ;
#28568 = ORIENTED_EDGE('',*,*,#19718,.F.) ;
#28569 = ORIENTED_EDGE('',*,*,#19713,.T.) ;
#28570 = ORIENTED_EDGE('',*,*,#19704,.F.) ;
#28571 = ORIENTED_EDGE('',*,*,#19719,.F.) ;
#28572 = ORIENTED_EDGE('',*,*,#19720,.F.) ;
#28573 = ORIENTED_EDGE('',*,*,#19717,.F.) ;
#28574 = ORIENTED_EDGE('',*,*,#19650,.F.) ;
#28575 = ORIENTED_EDGE('',*,*,#19685,.F.) ;
#28576 = ORIENTED_EDGE('',*,*,#19695,.F.) ;
#28577 = ORIENTED_EDGE('',*,*,#19677,.F.) ;
#28578 = ORIENTED_EDGE('',*,*,#19697,.F.) ;
#28579 = ORIENTED_EDGE('',*,*,#19706,.F.) ;
#28580 = ORIENTED_EDGE('',*,*,#19659,.F.) ;
#28581 = ORIENTED_EDGE('',*,*,#19700,.F.) ;
#28582 = ORIENTED_EDGE('',*,*,#19675,.F.) ;
#28583 = ORIENTED_EDGE('',*,*,#19721,.F.) ;
#28584 = ORIENTED_EDGE('',*,*,#19688,.F.) ;
#28585 = ORIENTED_EDGE('',*,*,#19699,.F.) ;
#28586 = ORIENTED_EDGE('',*,*,#19673,.F.) ;
#28587 = ORIENTED_EDGE('',*,*,#19709,.F.) ;
#28588 = ORIENTED_EDGE('',*,*,#19691,.F.) ;
#28589 = ORIENTED_EDGE('',*,*,#19721,.T.) ;
#28590 = ORIENTED_EDGE('',*,*,#19707,.F.) ;
#28591 = ORIENTED_EDGE('',*,*,#19722,.T.) ;
#28592 = ORIENTED_EDGE('',*,*,#19723,.T.) ;
#28593 = ORIENTED_EDGE('',*,*,#19719,.T.) ;
#28594 = ORIENTED_EDGE('',*,*,#19701,.F.) ;
#28595 = ORIENTED_EDGE('',*,*,#19724,.T.) ;
#28596 = ORIENTED_EDGE('',*,*,#19725,.T.) ;
#28597 = ORIENTED_EDGE('',*,*,#19726,.T.) ;
#28598 = ORIENTED_EDGE('',*,*,#19684,.F.) ;
#28599 = ORIENTED_EDGE('',*,*,#19726,.F.) ;
#28600 = ORIENTED_EDGE('',*,*,#19727,.F.) ;
#28601 = ORIENTED_EDGE('',*,*,#19728,.F.) ;
#28602 = ORIENTED_EDGE('',*,*,#19729,.F.) ;
#28603 = ORIENTED_EDGE('',*,*,#19730,.T.) ;
#28604 = ORIENTED_EDGE('',*,*,#19731,.F.) ;
#28605 = ORIENTED_EDGE('',*,*,#19732,.F.) ;
#28606 = ORIENTED_EDGE('',*,*,#19733,.F.) ;
#28607 = ORIENTED_EDGE('',*,*,#19722,.F.) ;
#28608 = ORIENTED_EDGE('',*,*,#19698,.F.) ;
#28609 = ORIENTED_EDGE('',*,*,#19662,.F.) ;
#28610 = ORIENTED_EDGE('',*,*,#19687,.F.) ;
#28611 = ORIENTED_EDGE('',*,*,#19690,.F.) ;
#28612 = ORIENTED_EDGE('',*,*,#19692,.F.) ;
#28613 = ORIENTED_EDGE('',*,*,#19681,.F.) ;
#28614 = ORIENTED_EDGE('',*,*,#19652,.F.) ;
#28615 = ORIENTED_EDGE('',*,*,#19712,.T.) ;
#28616 = ORIENTED_EDGE('',*,*,#19734,.F.) ;
#28617 = ORIENTED_EDGE('',*,*,#19724,.F.) ;
#28618 = ORIENTED_EDGE('',*,*,#19735,.F.) ;
#28619 = ORIENTED_EDGE('',*,*,#19736,.F.) ;
#28620 = ORIENTED_EDGE('',*,*,#19737,.T.) ;
#28621 = ORIENTED_EDGE('',*,*,#19738,.T.) ;
#28622 = ORIENTED_EDGE('',*,*,#19739,.T.) ;
#28623 = ORIENTED_EDGE('',*,*,#19740,.F.) ;
#28624 = ORIENTED_EDGE('',*,*,#19741,.F.) ;
#28625 = ORIENTED_EDGE('',*,*,#19742,.F.) ;
#28626 = ORIENTED_EDGE('',*,*,#19743,.F.) ;
#28627 = ORIENTED_EDGE('',*,*,#19744,.F.) ;
#28628 = ORIENTED_EDGE('',*,*,#19745,.F.) ;
#28629 = ORIENTED_EDGE('',*,*,#19746,.F.) ;
#28630 = ORIENTED_EDGE('',*,*,#19747,.F.) ;
#28631 = ORIENTED_EDGE('',*,*,#19748,.F.) ;
#28632 = ORIENTED_EDGE('',*,*,#19749,.F.) ;
#28633 = ORIENTED_EDGE('',*,*,#19750,.F.) ;
#28634 = ORIENTED_EDGE('',*,*,#19751,.F.) ;
#28635 = ORIENTED_EDGE('',*,*,#19752,.F.) ;
#28636 = ORIENTED_EDGE('',*,*,#19753,.F.) ;
#28637 = ORIENTED_EDGE('',*,*,#19754,.F.) ;
#28638 = ORIENTED_EDGE('',*,*,#19755,.F.) ;
#28639 = ORIENTED_EDGE('',*,*,#19756,.T.) ;
#28640 = ORIENTED_EDGE('',*,*,#19757,.F.) ;
#28641 = ORIENTED_EDGE('',*,*,#19758,.F.) ;
#28642 = ORIENTED_EDGE('',*,*,#19759,.T.) ;
#28643 = ORIENTED_EDGE('',*,*,#19633,.T.) ;
#28644 = ORIENTED_EDGE('',*,*,#19760,.T.) ;
#28645 = ORIENTED_EDGE('',*,*,#19619,.T.) ;
#28646 = ORIENTED_EDGE('',*,*,#19761,.F.) ;
#28647 = ORIENTED_EDGE('',*,*,#19750,.T.) ;
#28648 = ORIENTED_EDGE('',*,*,#19762,.F.) ;
#28649 = ORIENTED_EDGE('',*,*,#19756,.F.) ;
#28650 = ORIENTED_EDGE('',*,*,#19763,.F.) ;
#28651 = ORIENTED_EDGE('',*,*,#19758,.T.) ;
#28652 = ORIENTED_EDGE('',*,*,#19764,.F.) ;
#28653 = ORIENTED_EDGE('',*,*,#19730,.F.) ;
#28654 = ORIENTED_EDGE('',*,*,#19765,.T.) ;
#28655 = ORIENTED_EDGE('',*,*,#19738,.F.) ;
#28656 = ORIENTED_EDGE('',*,*,#19766,.T.) ;
#28657 = ORIENTED_EDGE('',*,*,#19767,.F.) ;
#28658 = ORIENTED_EDGE('',*,*,#19768,.T.) ;
#28659 = ORIENTED_EDGE('',*,*,#19769,.T.) ;
#28660 = ORIENTED_EDGE('',*,*,#19770,.T.) ;
#28661 = ORIENTED_EDGE('',*,*,#19715,.T.) ;
#28662 = ORIENTED_EDGE('',*,*,#19771,.F.) ;
#28663 = ORIENTED_EDGE('',*,*,#19772,.F.) ;
#28664 = ORIENTED_EDGE('',*,*,#19773,.F.) ;
#28665 = ORIENTED_EDGE('',*,*,#19774,.F.) ;
#28666 = ORIENTED_EDGE('',*,*,#19775,.F.) ;
#28667 = ORIENTED_EDGE('',*,*,#19740,.T.) ;
#28668 = ORIENTED_EDGE('',*,*,#19776,.F.) ;
#28669 = ORIENTED_EDGE('',*,*,#19772,.T.) ;
#28670 = ORIENTED_EDGE('',*,*,#19777,.F.) ;
#28671 = ORIENTED_EDGE('',*,*,#19778,.F.) ;
#28672 = ORIENTED_EDGE('',*,*,#19779,.F.) ;
#28673 = ORIENTED_EDGE('',*,*,#19780,.F.) ;
#28674 = ORIENTED_EDGE('',*,*,#19781,.F.) ;
#28675 = ORIENTED_EDGE('',*,*,#19782,.F.) ;
#28676 = ORIENTED_EDGE('',*,*,#19783,.F.) ;
#28677 = ORIENTED_EDGE('',*,*,#19784,.F.) ;
#28678 = ORIENTED_EDGE('',*,*,#19785,.F.) ;
#28679 = ORIENTED_EDGE('',*,*,#19786,.F.) ;
#28680 = ORIENTED_EDGE('',*,*,#19787,.F.) ;
#28681 = ORIENTED_EDGE('',*,*,#19788,.F.) ;
#28682 = ORIENTED_EDGE('',*,*,#19789,.F.) ;
#28683 = ORIENTED_EDGE('',*,*,#19790,.T.) ;
#28684 = ORIENTED_EDGE('',*,*,#19791,.F.) ;
#28685 = ORIENTED_EDGE('',*,*,#19736,.T.) ;
#28686 = ORIENTED_EDGE('',*,*,#19792,.F.) ;
#28687 = ORIENTED_EDGE('',*,*,#19793,.F.) ;
#28688 = ORIENTED_EDGE('',*,*,#19794,.F.) ;
#28689 = ORIENTED_EDGE('',*,*,#19790,.F.) ;
#28690 = ORIENTED_EDGE('',*,*,#19714,.F.) ;
#28691 = ORIENTED_EDGE('',*,*,#19718,.T.) ;
#28692 = ORIENTED_EDGE('',*,*,#19795,.F.) ;
#28693 = ORIENTED_EDGE('',*,*,#19796,.T.) ;
#28694 = ORIENTED_EDGE('',*,*,#19768,.F.) ;
#28695 = ORIENTED_EDGE('',*,*,#19770,.F.) ;
#28696 = ORIENTED_EDGE('',*,*,#19797,.T.) ;
#28697 = ORIENTED_EDGE('',*,*,#19798,.F.) ;
#28698 = ORIENTED_EDGE('',*,*,#19711,.T.) ;
#28699 = ORIENTED_EDGE('',*,*,#19716,.F.) ;
#28700 = ORIENTED_EDGE('',*,*,#19765,.F.) ;
#28701 = ORIENTED_EDGE('',*,*,#19799,.T.) ;
#28702 = ORIENTED_EDGE('',*,*,#19800,.F.) ;
#28703 = ORIENTED_EDGE('',*,*,#19776,.T.) ;
#28704 = ORIENTED_EDGE('',*,*,#19739,.F.) ;
#28705 = ORIENTED_EDGE('',*,*,#19801,.F.) ;
#28706 = ORIENTED_EDGE('',*,*,#19789,.T.) ;
#28707 = ORIENTED_EDGE('',*,*,#19802,.F.) ;
#28708 = ORIENTED_EDGE('',*,*,#19737,.F.) ;
#28709 = ORIENTED_EDGE('',*,*,#19791,.T.) ;
#28710 = ORIENTED_EDGE('',*,*,#19803,.F.) ;
#28711 = ORIENTED_EDGE('',*,*,#19804,.T.) ;
#28712 = ORIENTED_EDGE('',*,*,#19766,.F.) ;
#28713 = ORIENTED_EDGE('',*,*,#19805,.F.) ;
#28714 = ORIENTED_EDGE('',*,*,#19775,.T.) ;
#28715 = ORIENTED_EDGE('',*,*,#19806,.F.) ;
#28716 = ORIENTED_EDGE('',*,*,#19735,.T.) ;
#28717 = ORIENTED_EDGE('',*,*,#19805,.T.) ;
#28718 = ORIENTED_EDGE('',*,*,#19741,.T.) ;
#28719 = ORIENTED_EDGE('',*,*,#19802,.T.) ;
#28720 = ORIENTED_EDGE('',*,*,#19795,.T.) ;
#28721 = ORIENTED_EDGE('',*,*,#19720,.T.) ;
#28722 = ORIENTED_EDGE('',*,*,#19807,.T.) ;
#28723 = ORIENTED_EDGE('',*,*,#19808,.T.) ;
#28724 = ORIENTED_EDGE('',*,*,#19798,.T.) ;
#28725 = ORIENTED_EDGE('',*,*,#19809,.T.) ;
#28726 = ORIENTED_EDGE('',*,*,#19810,.T.) ;
#28727 = ORIENTED_EDGE('',*,*,#19734,.T.) ;
#28728 = ORIENTED_EDGE('',*,*,#19811,.T.) ;
#28729 = ORIENTED_EDGE('',*,*,#19812,.T.) ;
#28730 = ORIENTED_EDGE('',*,*,#19813,.T.) ;
#28731 = ORIENTED_EDGE('',*,*,#19732,.T.) ;
#28732 = ORIENTED_EDGE('',*,*,#19814,.T.) ;
#28733 = ORIENTED_EDGE('',*,*,#19815,.T.) ;
#28734 = ORIENTED_EDGE('',*,*,#19816,.T.) ;
#28735 = ORIENTED_EDGE('',*,*,#19728,.T.) ;
#28736 = ORIENTED_EDGE('',*,*,#19817,.T.) ;
#28737 = ORIENTED_EDGE('',*,*,#19782,.T.) ;
#28738 = ORIENTED_EDGE('',*,*,#19818,.F.) ;
#28739 = ORIENTED_EDGE('',*,*,#19749,.T.) ;
#28740 = ORIENTED_EDGE('',*,*,#19818,.T.) ;
#28741 = ORIENTED_EDGE('',*,*,#19781,.T.) ;
#28742 = ORIENTED_EDGE('',*,*,#19819,.F.) ;
#28743 = ORIENTED_EDGE('',*,*,#19762,.T.) ;
#28744 = ORIENTED_EDGE('',*,*,#19819,.T.) ;
#28745 = ORIENTED_EDGE('',*,*,#19780,.T.) ;
#28746 = ORIENTED_EDGE('',*,*,#19820,.F.) ;
#28747 = ORIENTED_EDGE('',*,*,#19757,.T.) ;
#28748 = ORIENTED_EDGE('',*,*,#19820,.T.) ;
#28749 = ORIENTED_EDGE('',*,*,#19779,.T.) ;
#28750 = ORIENTED_EDGE('',*,*,#19821,.F.) ;
#28751 = ORIENTED_EDGE('',*,*,#19764,.T.) ;
#28752 = ORIENTED_EDGE('',*,*,#19821,.T.) ;
#28753 = ORIENTED_EDGE('',*,*,#19778,.T.) ;
#28754 = ORIENTED_EDGE('',*,*,#19822,.T.) ;
#28755 = ORIENTED_EDGE('',*,*,#19731,.T.) ;
#28756 = ORIENTED_EDGE('',*,*,#19823,.T.) ;
#28757 = ORIENTED_EDGE('',*,*,#19824,.T.) ;
#28758 = ORIENTED_EDGE('',*,*,#19825,.T.) ;
#28759 = ORIENTED_EDGE('',*,*,#19777,.T.) ;
#28760 = ORIENTED_EDGE('',*,*,#19826,.T.) ;
#28761 = ORIENTED_EDGE('',*,*,#19827,.T.) ;
#28762 = ORIENTED_EDGE('',*,*,#19828,.T.) ;
#28763 = ORIENTED_EDGE('',*,*,#19788,.T.) ;
#28764 = ORIENTED_EDGE('',*,*,#19829,.T.) ;
#28765 = ORIENTED_EDGE('',*,*,#19787,.T.) ;
#28766 = ORIENTED_EDGE('',*,*,#19830,.F.) ;
#28767 = ORIENTED_EDGE('',*,*,#19729,.T.) ;
#28768 = ORIENTED_EDGE('',*,*,#19830,.T.) ;
#28769 = ORIENTED_EDGE('',*,*,#19786,.T.) ;
#28770 = ORIENTED_EDGE('',*,*,#19831,.F.) ;
#28771 = ORIENTED_EDGE('',*,*,#19763,.T.) ;
#28772 = ORIENTED_EDGE('',*,*,#19831,.T.) ;
#28773 = ORIENTED_EDGE('',*,*,#19785,.T.) ;
#28774 = ORIENTED_EDGE('',*,*,#19832,.F.) ;
#28775 = ORIENTED_EDGE('',*,*,#19755,.T.) ;
#28776 = ORIENTED_EDGE('',*,*,#19832,.T.) ;
#28777 = ORIENTED_EDGE('',*,*,#19784,.T.) ;
#28778 = ORIENTED_EDGE('',*,*,#19833,.F.) ;
#28779 = ORIENTED_EDGE('',*,*,#19761,.T.) ;
#28780 = ORIENTED_EDGE('',*,*,#19833,.T.) ;
#28781 = ORIENTED_EDGE('',*,*,#19783,.T.) ;
#28782 = ORIENTED_EDGE('',*,*,#19834,.T.) ;
#28783 = ORIENTED_EDGE('',*,*,#19751,.T.) ;
#28784 = ORIENTED_EDGE('',*,*,#19800,.T.) ;
#28785 = ORIENTED_EDGE('',*,*,#19835,.T.) ;
#28786 = ORIENTED_EDGE('',*,*,#19836,.T.) ;
#28787 = ORIENTED_EDGE('',*,*,#19773,.T.) ;
#28788 = ORIENTED_EDGE('',*,*,#19837,.T.) ;
#28789 = ORIENTED_EDGE('',*,*,#19774,.T.) ;
#28790 = ORIENTED_EDGE('',*,*,#19838,.T.) ;
#28791 = ORIENTED_EDGE('',*,*,#19746,.T.) ;
#28792 = ORIENTED_EDGE('',*,*,#19806,.T.) ;
#28793 = ORIENTED_EDGE('',*,*,#19771,.T.) ;
#28794 = ORIENTED_EDGE('',*,*,#19839,.T.) ;
#28795 = ORIENTED_EDGE('',*,*,#19742,.T.) ;
#28796 = ORIENTED_EDGE('',*,*,#19801,.T.) ;
#28797 = ORIENTED_EDGE('',*,*,#19744,.T.) ;
#28798 = ORIENTED_EDGE('',*,*,#19840,.T.) ;
#28799 = ORIENTED_EDGE('',*,*,#19792,.T.) ;
#28800 = ORIENTED_EDGE('',*,*,#19841,.T.) ;
#28801 = ORIENTED_EDGE('',*,*,#19793,.T.) ;
#28802 = ORIENTED_EDGE('',*,*,#19842,.T.) ;
#28803 = ORIENTED_EDGE('',*,*,#19754,.T.) ;
#28804 = ORIENTED_EDGE('',*,*,#19743,.T.) ;
#28805 = ORIENTED_EDGE('',*,*,#19843,.T.) ;
#28806 = ORIENTED_EDGE('',*,*,#19745,.T.) ;
#28807 = ORIENTED_EDGE('',*,*,#19844,.T.) ;
#28808 = ORIENTED_EDGE('',*,*,#19840,.F.) ;
#28809 = ORIENTED_EDGE('',*,*,#19844,.F.) ;
#28810 = ORIENTED_EDGE('',*,*,#19842,.F.) ;
#28811 = ORIENTED_EDGE('',*,*,#19837,.F.) ;
#28812 = ORIENTED_EDGE('',*,*,#19843,.F.) ;
#28813 = ORIENTED_EDGE('',*,*,#19839,.F.) ;
#28814 = ORIENTED_EDGE('',*,*,#19803,.T.) ;
#28815 = ORIENTED_EDGE('',*,*,#19794,.T.) ;
#28816 = ORIENTED_EDGE('',*,*,#19845,.T.) ;
#28817 = ORIENTED_EDGE('',*,*,#19846,.T.) ;
#28818 = ORIENTED_EDGE('',*,*,#19847,.T.) ;
#28819 = ORIENTED_EDGE('',*,*,#19848,.T.) ;
#28820 = ORIENTED_EDGE('',*,*,#19849,.T.) ;
#28821 = ORIENTED_EDGE('',*,*,#19752,.T.) ;
#28822 = ORIENTED_EDGE('',*,*,#19753,.T.) ;
#28823 = ORIENTED_EDGE('',*,*,#19849,.F.) ;
#28824 = ORIENTED_EDGE('',*,*,#19845,.F.) ;
#28825 = ORIENTED_EDGE('',*,*,#19841,.F.) ;
#28826 = ORIENTED_EDGE('',*,*,#19850,.T.) ;
#28827 = ORIENTED_EDGE('',*,*,#19851,.T.) ;
#28828 = ORIENTED_EDGE('',*,*,#19852,.T.) ;
#28829 = ORIENTED_EDGE('',*,*,#19748,.T.) ;
#28830 = ORIENTED_EDGE('',*,*,#19836,.F.) ;
#28831 = ORIENTED_EDGE('',*,*,#19850,.F.) ;
#28832 = ORIENTED_EDGE('',*,*,#19747,.T.) ;
#28833 = ORIENTED_EDGE('',*,*,#19838,.F.) ;
#28834 = ORIENTED_EDGE('',*,*,#19828,.F.) ;
#28835 = ORIENTED_EDGE('',*,*,#19847,.F.) ;
#28836 = ORIENTED_EDGE('',*,*,#19834,.F.) ;
#28837 = ORIENTED_EDGE('',*,*,#19817,.F.) ;
#28838 = ORIENTED_EDGE('',*,*,#19852,.F.) ;
#28839 = ORIENTED_EDGE('',*,*,#19823,.F.) ;
#28840 = ORIENTED_EDGE('',*,*,#19816,.F.) ;
#28841 = ORIENTED_EDGE('',*,*,#19826,.F.) ;
#28842 = ORIENTED_EDGE('',*,*,#19829,.F.) ;
#28843 = ORIENTED_EDGE('',*,*,#19822,.F.) ;
#28844 = ORIENTED_EDGE('',*,*,#19825,.F.) ;
#28845 = ORIENTED_EDGE('',*,*,#19811,.F.) ;
#28846 = ORIENTED_EDGE('',*,*,#19810,.F.) ;
#28847 = ORIENTED_EDGE('',*,*,#19814,.F.) ;
#28848 = ORIENTED_EDGE('',*,*,#19727,.T.) ;
#28849 = ORIENTED_EDGE('',*,*,#19725,.F.) ;
#28850 = ORIENTED_EDGE('',*,*,#19733,.T.) ;
#28851 = ORIENTED_EDGE('',*,*,#19813,.F.) ;
#28852 = ORIENTED_EDGE('',*,*,#19807,.F.) ;
#28853 = ORIENTED_EDGE('',*,*,#19723,.F.) ;
#28854 = ORIENTED_EDGE('',*,*,#19853,.T.) ;
#28855 = ORIENTED_EDGE('',*,*,#19854,.T.) ;
#28856 = ORIENTED_EDGE('',*,*,#19855,.T.) ;
#28857 = ORIENTED_EDGE('',*,*,#19854,.F.) ;
#28858 = ORIENTED_EDGE('',*,*,#19799,.F.) ;
#28859 = ORIENTED_EDGE('',*,*,#19767,.T.) ;
#28860 = ORIENTED_EDGE('',*,*,#19804,.F.) ;
#28861 = ORIENTED_EDGE('',*,*,#19846,.F.) ;
#28862 = ORIENTED_EDGE('',*,*,#19848,.F.) ;
#28863 = ORIENTED_EDGE('',*,*,#19827,.F.) ;
#28864 = ORIENTED_EDGE('',*,*,#19815,.F.) ;
#28865 = ORIENTED_EDGE('',*,*,#19809,.F.) ;
#28866 = ORIENTED_EDGE('',*,*,#19797,.F.) ;
#28867 = ORIENTED_EDGE('',*,*,#19769,.F.) ;
#28868 = ORIENTED_EDGE('',*,*,#19796,.F.) ;
#28869 = ORIENTED_EDGE('',*,*,#19808,.F.) ;
#28870 = ORIENTED_EDGE('',*,*,#19812,.F.) ;
#28871 = ORIENTED_EDGE('',*,*,#19824,.F.) ;
#28872 = ORIENTED_EDGE('',*,*,#19851,.F.) ;
#28873 = ORIENTED_EDGE('',*,*,#19835,.F.) ;
#28874 = ORIENTED_EDGE('',*,*,#19856,.F.) ;
#28875 = ORIENTED_EDGE('',*,*,#19857,.F.) ;
#28876 = ORIENTED_EDGE('',*,*,#19858,.F.) ;
#28877 = ORIENTED_EDGE('',*,*,#19859,.T.) ;
#28878 = ORIENTED_EDGE('',*,*,#19855,.F.) ;
#28879 = ORIENTED_EDGE('',*,*,#19859,.F.) ;
#28880 = ORIENTED_EDGE('',*,*,#19856,.T.) ;
#28881 = ORIENTED_EDGE('',*,*,#19860,.T.) ;
#28882 = ORIENTED_EDGE('',*,*,#19857,.T.) ;
#28883 = ORIENTED_EDGE('',*,*,#19858,.T.) ;
#28884 = ORIENTED_EDGE('',*,*,#19860,.F.) ;
#28885 = ORIENTED_EDGE('',*,*,#19853,.F.) ;
#28886 = ORIENTED_EDGE('',*,*,#19861,.T.) ;
#28887 = ORIENTED_EDGE('',*,*,#19629,.T.) ;
#28888 = ORIENTED_EDGE('',*,*,#19862,.T.) ;
#28889 = ORIENTED_EDGE('',*,*,#19643,.T.) ;
#28890 = ORIENTED_EDGE('',*,*,#19760,.F.) ;
#28891 = ORIENTED_EDGE('',*,*,#19632,.F.) ;
#28892 = ORIENTED_EDGE('',*,*,#19636,.F.) ;
#28893 = ORIENTED_EDGE('',*,*,#19639,.F.) ;
#28894 = ORIENTED_EDGE('',*,*,#19645,.F.) ;
#28895 = ORIENTED_EDGE('',*,*,#19644,.F.) ;
#28896 = ORIENTED_EDGE('',*,*,#19862,.F.) ;
#28897 = ORIENTED_EDGE('',*,*,#19628,.T.) ;
#28898 = ORIENTED_EDGE('',*,*,#19648,.T.) ;
#28899 = ORIENTED_EDGE('',*,*,#19626,.T.) ;
#28900 = ORIENTED_EDGE('',*,*,#19623,.T.) ;
#28901 = ORIENTED_EDGE('',*,*,#19620,.T.) ;
#28902 = ORIENTED_EDGE('',*,*,#19759,.F.) ;
#28903 = ORIENTED_EDGE('',*,*,#19618,.F.) ;
#28904 = ORIENTED_EDGE('',*,*,#19622,.F.) ;
#28905 = ORIENTED_EDGE('',*,*,#19625,.F.) ;
#28906 = ORIENTED_EDGE('',*,*,#19647,.F.) ;
#28907 = ORIENTED_EDGE('',*,*,#19630,.F.) ;
#28908 = ORIENTED_EDGE('',*,*,#19861,.F.) ;
#28909 = ORIENTED_EDGE('',*,*,#19642,.F.) ;
#28910 = ORIENTED_EDGE('',*,*,#19646,.F.) ;
#28911 = ORIENTED_EDGE('',*,*,#19640,.F.) ;
#28912 = ORIENTED_EDGE('',*,*,#19637,.F.) ;
#28913 = ORIENTED_EDGE('',*,*,#19634,.F.) ;
#28914 = ORIENTED_EDGE('',*,*,#19863,.F.) ;
#28915 = ORIENTED_EDGE('',*,*,#19864,.F.) ;
#28916 = ORIENTED_EDGE('',*,*,#19865,.F.) ;
#28917 = ORIENTED_EDGE('',*,*,#19866,.F.) ;
#28918 = ORIENTED_EDGE('',*,*,#19867,.F.) ;
#28919 = ORIENTED_EDGE('',*,*,#19868,.F.) ;
#28920 = ORIENTED_EDGE('',*,*,#19869,.F.) ;
#28921 = ORIENTED_EDGE('',*,*,#19870,.F.) ;
#28922 = ORIENTED_EDGE('',*,*,#19865,.T.) ;
#28923 = ORIENTED_EDGE('',*,*,#19871,.F.) ;
#28924 = ORIENTED_EDGE('',*,*,#19872,.F.) ;
#28925 = ORIENTED_EDGE('',*,*,#19873,.F.) ;
#28926 = ORIENTED_EDGE('',*,*,#19874,.F.) ;
#28927 = ORIENTED_EDGE('',*,*,#19875,.F.) ;
#28928 = ORIENTED_EDGE('',*,*,#19876,.F.) ;
#28929 = ORIENTED_EDGE('',*,*,#19877,.F.) ;
#28930 = ORIENTED_EDGE('',*,*,#19878,.F.) ;
#28931 = ORIENTED_EDGE('',*,*,#19879,.F.) ;
#28932 = ORIENTED_EDGE('',*,*,#19880,.F.) ;
#28933 = ORIENTED_EDGE('',*,*,#19881,.F.) ;
#28934 = ORIENTED_EDGE('',*,*,#19882,.F.) ;
#28935 = ORIENTED_EDGE('',*,*,#19883,.T.) ;
#28936 = ORIENTED_EDGE('',*,*,#19884,.T.) ;
#28937 = ORIENTED_EDGE('',*,*,#19883,.F.) ;
#28938 = ORIENTED_EDGE('',*,*,#19868,.T.) ;
#28939 = ORIENTED_EDGE('',*,*,#19885,.F.) ;
#28940 = ORIENTED_EDGE('',*,*,#19886,.T.) ;
#28941 = ORIENTED_EDGE('',*,*,#19887,.F.) ;
#28942 = ORIENTED_EDGE('',*,*,#19888,.T.) ;
#28943 = ORIENTED_EDGE('',*,*,#19889,.F.) ;
#28944 = ORIENTED_EDGE('',*,*,#19875,.T.) ;
#28945 = ORIENTED_EDGE('',*,*,#19890,.F.) ;
#28946 = ORIENTED_EDGE('',*,*,#19891,.T.) ;
#28947 = ORIENTED_EDGE('',*,*,#19892,.F.) ;
#28948 = ORIENTED_EDGE('',*,*,#19893,.T.) ;
#28949 = ORIENTED_EDGE('',*,*,#19894,.F.) ;
#28950 = ORIENTED_EDGE('',*,*,#19871,.T.) ;
#28951 = ORIENTED_EDGE('',*,*,#19864,.T.) ;
#28952 = ORIENTED_EDGE('',*,*,#19895,.F.) ;
#28953 = ORIENTED_EDGE('',*,*,#19896,.T.) ;
#28954 = ORIENTED_EDGE('',*,*,#19897,.F.) ;
#28955 = ORIENTED_EDGE('',*,*,#19898,.T.) ;
#28956 = ORIENTED_EDGE('',*,*,#19899,.F.) ;
#28957 = ORIENTED_EDGE('',*,*,#19879,.T.) ;
#28958 = ORIENTED_EDGE('',*,*,#19900,.F.) ;
#28959 = ORIENTED_EDGE('',*,*,#19901,.T.) ;
#28960 = ORIENTED_EDGE('',*,*,#19902,.F.) ;
#28961 = ORIENTED_EDGE('',*,*,#19903,.T.) ;
#28962 = ORIENTED_EDGE('',*,*,#19904,.F.) ;
#28963 = ORIENTED_EDGE('',*,*,#19882,.T.) ;
#28964 = ORIENTED_EDGE('',*,*,#19905,.F.) ;
#28965 = ORIENTED_EDGE('',*,*,#19906,.F.) ;
#28966 = ORIENTED_EDGE('',*,*,#19907,.F.) ;
#28967 = ORIENTED_EDGE('',*,*,#19908,.F.) ;
#28968 = ORIENTED_EDGE('',*,*,#19909,.F.) ;
#28969 = ORIENTED_EDGE('',*,*,#19910,.F.) ;
#28970 = ORIENTED_EDGE('',*,*,#19911,.F.) ;
#28971 = ORIENTED_EDGE('',*,*,#19912,.F.) ;
#28972 = ORIENTED_EDGE('',*,*,#19913,.F.) ;
#28973 = ORIENTED_EDGE('',*,*,#19914,.F.) ;
#28974 = ORIENTED_EDGE('',*,*,#19915,.F.) ;
#28975 = ORIENTED_EDGE('',*,*,#19916,.F.) ;
#28976 = ORIENTED_EDGE('',*,*,#19917,.F.) ;
#28977 = ORIENTED_EDGE('',*,*,#19918,.F.) ;
#28978 = ORIENTED_EDGE('',*,*,#19919,.F.) ;
#28979 = ORIENTED_EDGE('',*,*,#19920,.F.) ;
#28980 = ORIENTED_EDGE('',*,*,#19921,.F.) ;
#28981 = ORIENTED_EDGE('',*,*,#19897,.T.) ;
#28982 = ORIENTED_EDGE('',*,*,#19922,.T.) ;
#28983 = ORIENTED_EDGE('',*,*,#19923,.F.) ;
#28984 = ORIENTED_EDGE('',*,*,#19921,.T.) ;
#28985 = ORIENTED_EDGE('',*,*,#19924,.T.) ;
#28986 = ORIENTED_EDGE('',*,*,#19925,.F.) ;
#28987 = ORIENTED_EDGE('',*,*,#19898,.F.) ;
#28988 = ORIENTED_EDGE('',*,*,#19926,.F.) ;
#28989 = ORIENTED_EDGE('',*,*,#19927,.T.) ;
#28990 = ORIENTED_EDGE('',*,*,#19922,.F.) ;
#28991 = ORIENTED_EDGE('',*,*,#19896,.F.) ;
#28992 = ORIENTED_EDGE('',*,*,#19928,.T.) ;
#28993 = ORIENTED_EDGE('',*,*,#19902,.T.) ;
#28994 = ORIENTED_EDGE('',*,*,#19929,.T.) ;
#28995 = ORIENTED_EDGE('',*,*,#19930,.F.) ;
#28996 = ORIENTED_EDGE('',*,*,#19928,.F.) ;
#28997 = ORIENTED_EDGE('',*,*,#19931,.T.) ;
#28998 = ORIENTED_EDGE('',*,*,#19932,.F.) ;
#28999 = ORIENTED_EDGE('',*,*,#19903,.F.) ;
#29000 = ORIENTED_EDGE('',*,*,#19933,.F.) ;
#29001 = ORIENTED_EDGE('',*,*,#19934,.T.) ;
#29002 = ORIENTED_EDGE('',*,*,#19929,.F.) ;
#29003 = ORIENTED_EDGE('',*,*,#19901,.F.) ;
#29004 = ORIENTED_EDGE('',*,*,#19935,.F.) ;
#29005 = ORIENTED_EDGE('',*,*,#19887,.T.) ;
#29006 = ORIENTED_EDGE('',*,*,#19936,.T.) ;
#29007 = ORIENTED_EDGE('',*,*,#19937,.F.) ;
#29008 = ORIENTED_EDGE('',*,*,#19935,.T.) ;
#29009 = ORIENTED_EDGE('',*,*,#19938,.T.) ;
#29010 = ORIENTED_EDGE('',*,*,#19939,.F.) ;
#29011 = ORIENTED_EDGE('',*,*,#19888,.F.) ;
#29012 = ORIENTED_EDGE('',*,*,#19940,.F.) ;
#29013 = ORIENTED_EDGE('',*,*,#19941,.T.) ;
#29014 = ORIENTED_EDGE('',*,*,#19936,.F.) ;
#29015 = ORIENTED_EDGE('',*,*,#19886,.F.) ;
#29016 = ORIENTED_EDGE('',*,*,#19942,.T.) ;
#29017 = ORIENTED_EDGE('',*,*,#19943,.F.) ;
#29018 = ORIENTED_EDGE('',*,*,#19938,.F.) ;
#29019 = ORIENTED_EDGE('',*,*,#19944,.T.) ;
#29020 = ORIENTED_EDGE('',*,*,#19945,.T.) ;
#29021 = ORIENTED_EDGE('',*,*,#19946,.F.) ;
#29022 = ORIENTED_EDGE('',*,*,#19941,.F.) ;
#29023 = ORIENTED_EDGE('',*,*,#19947,.T.) ;
#29024 = ORIENTED_EDGE('',*,*,#19948,.T.) ;
#29025 = ORIENTED_EDGE('',*,*,#19944,.F.) ;
#29026 = ORIENTED_EDGE('',*,*,#19937,.T.) ;
#29027 = ORIENTED_EDGE('',*,*,#19946,.T.) ;
#29028 = ORIENTED_EDGE('',*,*,#19949,.F.) ;
#29029 = ORIENTED_EDGE('',*,*,#19915,.T.) ;
#29030 = ORIENTED_EDGE('',*,*,#19950,.F.) ;
#29031 = ORIENTED_EDGE('',*,*,#19942,.F.) ;
#29032 = ORIENTED_EDGE('',*,*,#19951,.F.) ;
#29033 = ORIENTED_EDGE('',*,*,#19913,.T.) ;
#29034 = ORIENTED_EDGE('',*,*,#19952,.T.) ;
#29035 = ORIENTED_EDGE('',*,*,#19945,.F.) ;
#29036 = ORIENTED_EDGE('',*,*,#19952,.F.) ;
#29037 = ORIENTED_EDGE('',*,*,#19916,.T.) ;
#29038 = ORIENTED_EDGE('',*,*,#19949,.T.) ;
#29039 = ORIENTED_EDGE('',*,*,#19948,.F.) ;
#29040 = ORIENTED_EDGE('',*,*,#19953,.T.) ;
#29041 = ORIENTED_EDGE('',*,*,#19954,.T.) ;
#29042 = ORIENTED_EDGE('',*,*,#19955,.F.) ;
#29043 = ORIENTED_EDGE('',*,*,#19956,.F.) ;
#29044 = ORIENTED_EDGE('',*,*,#19957,.T.) ;
#29045 = ORIENTED_EDGE('',*,*,#19958,.T.) ;
#29046 = ORIENTED_EDGE('',*,*,#19959,.F.) ;
#29047 = ORIENTED_EDGE('',*,*,#19960,.F.) ;
#29048 = ORIENTED_EDGE('',*,*,#19961,.T.) ;
#29049 = ORIENTED_EDGE('',*,*,#19911,.T.) ;
#29050 = ORIENTED_EDGE('',*,*,#19962,.T.) ;
#29051 = ORIENTED_EDGE('',*,*,#19963,.F.) ;
#29052 = ORIENTED_EDGE('',*,*,#19962,.F.) ;
#29053 = ORIENTED_EDGE('',*,*,#19910,.T.) ;
#29054 = ORIENTED_EDGE('',*,*,#19964,.F.) ;
#29055 = ORIENTED_EDGE('',*,*,#19954,.F.) ;
#29056 = ORIENTED_EDGE('',*,*,#19965,.F.) ;
#29057 = ORIENTED_EDGE('',*,*,#19912,.T.) ;
#29058 = ORIENTED_EDGE('',*,*,#19961,.F.) ;
#29059 = ORIENTED_EDGE('',*,*,#19958,.F.) ;
#29060 = ORIENTED_EDGE('',*,*,#19966,.T.) ;
#29061 = ORIENTED_EDGE('',*,*,#19967,.F.) ;
#29062 = ORIENTED_EDGE('',*,*,#19924,.F.) ;
#29063 = ORIENTED_EDGE('',*,*,#19968,.T.) ;
#29064 = ORIENTED_EDGE('',*,*,#19969,.T.) ;
#29065 = ORIENTED_EDGE('',*,*,#19970,.F.) ;
#29066 = ORIENTED_EDGE('',*,*,#19927,.F.) ;
#29067 = ORIENTED_EDGE('',*,*,#19971,.T.) ;
#29068 = ORIENTED_EDGE('',*,*,#19972,.T.) ;
#29069 = ORIENTED_EDGE('',*,*,#19968,.F.) ;
#29070 = ORIENTED_EDGE('',*,*,#19923,.T.) ;
#29071 = ORIENTED_EDGE('',*,*,#19970,.T.) ;
#29072 = ORIENTED_EDGE('',*,*,#19973,.T.) ;
#29073 = ORIENTED_EDGE('',*,*,#19919,.T.) ;
#29074 = ORIENTED_EDGE('',*,*,#19974,.T.) ;
#29075 = ORIENTED_EDGE('',*,*,#19972,.F.) ;
#29076 = ORIENTED_EDGE('',*,*,#19974,.F.) ;
#29077 = ORIENTED_EDGE('',*,*,#19918,.T.) ;
#29078 = ORIENTED_EDGE('',*,*,#19975,.F.) ;
#29079 = ORIENTED_EDGE('',*,*,#19966,.F.) ;
#29080 = ORIENTED_EDGE('',*,*,#19976,.F.) ;
#29081 = ORIENTED_EDGE('',*,*,#19920,.T.) ;
#29082 = ORIENTED_EDGE('',*,*,#19973,.F.) ;
#29083 = ORIENTED_EDGE('',*,*,#19969,.F.) ;
#29084 = ORIENTED_EDGE('',*,*,#19977,.T.) ;
#29085 = ORIENTED_EDGE('',*,*,#19978,.F.) ;
#29086 = ORIENTED_EDGE('',*,*,#19931,.F.) ;
#29087 = ORIENTED_EDGE('',*,*,#19979,.T.) ;
#29088 = ORIENTED_EDGE('',*,*,#19980,.T.) ;
#29089 = ORIENTED_EDGE('',*,*,#19981,.F.) ;
#29090 = ORIENTED_EDGE('',*,*,#19934,.F.) ;
#29091 = ORIENTED_EDGE('',*,*,#19982,.T.) ;
#29092 = ORIENTED_EDGE('',*,*,#19983,.T.) ;
#29093 = ORIENTED_EDGE('',*,*,#19979,.F.) ;
#29094 = ORIENTED_EDGE('',*,*,#19930,.T.) ;
#29095 = ORIENTED_EDGE('',*,*,#19981,.T.) ;
#29096 = ORIENTED_EDGE('',*,*,#19984,.F.) ;
#29097 = ORIENTED_EDGE('',*,*,#19907,.T.) ;
#29098 = ORIENTED_EDGE('',*,*,#19985,.F.) ;
#29099 = ORIENTED_EDGE('',*,*,#19977,.F.) ;
#29100 = ORIENTED_EDGE('',*,*,#19986,.F.) ;
#29101 = ORIENTED_EDGE('',*,*,#19905,.T.) ;
#29102 = ORIENTED_EDGE('',*,*,#19987,.T.) ;
#29103 = ORIENTED_EDGE('',*,*,#19980,.F.) ;
#29104 = ORIENTED_EDGE('',*,*,#19987,.F.) ;
#29105 = ORIENTED_EDGE('',*,*,#19908,.T.) ;
#29106 = ORIENTED_EDGE('',*,*,#19984,.T.) ;
#29107 = ORIENTED_EDGE('',*,*,#19983,.F.) ;
#29108 = ORIENTED_EDGE('',*,*,#19988,.T.) ;
#29109 = ORIENTED_EDGE('',*,*,#19959,.T.) ;
#29110 = ORIENTED_EDGE('',*,*,#19963,.T.) ;
#29111 = ORIENTED_EDGE('',*,*,#19953,.F.) ;
#29112 = ORIENTED_EDGE('',*,*,#19989,.T.) ;
#29113 = ORIENTED_EDGE('',*,*,#19892,.T.) ;
#29114 = ORIENTED_EDGE('',*,*,#19990,.T.) ;
#29115 = ORIENTED_EDGE('',*,*,#19988,.F.) ;
#29116 = ORIENTED_EDGE('',*,*,#19989,.F.) ;
#29117 = ORIENTED_EDGE('',*,*,#19956,.T.) ;
#29118 = ORIENTED_EDGE('',*,*,#19991,.F.) ;
#29119 = ORIENTED_EDGE('',*,*,#19893,.F.) ;
#29120 = ORIENTED_EDGE('',*,*,#19992,.F.) ;
#29121 = ORIENTED_EDGE('',*,*,#19960,.T.) ;
#29122 = ORIENTED_EDGE('',*,*,#19990,.F.) ;
#29123 = ORIENTED_EDGE('',*,*,#19891,.F.) ;
#29124 = ORIENTED_EDGE('',*,*,#19993,.T.) ;
#29125 = ORIENTED_EDGE('',*,*,#19994,.T.) ;
#29126 = ORIENTED_EDGE('',*,*,#19995,.T.) ;
#29127 = ORIENTED_EDGE('',*,*,#19996,.T.) ;
#29128 = ORIENTED_EDGE('',*,*,#19997,.T.) ;
#29129 = ORIENTED_EDGE('',*,*,#19998,.T.) ;
#29130 = ORIENTED_EDGE('',*,*,#19999,.F.) ;
#29131 = ORIENTED_EDGE('',*,*,#20000,.F.) ;
#29132 = ORIENTED_EDGE('',*,*,#20001,.T.) ;
#29133 = ORIENTED_EDGE('',*,*,#20002,.T.) ;
#29134 = ORIENTED_EDGE('',*,*,#20003,.F.) ;
#29135 = ORIENTED_EDGE('',*,*,#20002,.F.) ;
#29136 = ORIENTED_EDGE('',*,*,#20004,.T.) ;
#29137 = ORIENTED_EDGE('',*,*,#20005,.F.) ;
#29138 = ORIENTED_EDGE('',*,*,#19999,.T.) ;
#29139 = ORIENTED_EDGE('',*,*,#20006,.F.) ;
#29140 = ORIENTED_EDGE('',*,*,#19994,.F.) ;
#29141 = ORIENTED_EDGE('',*,*,#20007,.F.) ;
#29142 = ORIENTED_EDGE('',*,*,#20003,.T.) ;
#29143 = ORIENTED_EDGE('',*,*,#20008,.T.) ;
#29144 = ORIENTED_EDGE('',*,*,#19996,.F.) ;
#29145 = ORIENTED_EDGE('',*,*,#20009,.F.) ;
#29146 = ORIENTED_EDGE('',*,*,#20005,.T.) ;
#29147 = ORIENTED_EDGE('',*,*,#20007,.T.) ;
#29148 = ORIENTED_EDGE('',*,*,#19993,.F.) ;
#29149 = ORIENTED_EDGE('',*,*,#20008,.F.) ;
#29150 = ORIENTED_EDGE('',*,*,#20010,.T.) ;
#29151 = ORIENTED_EDGE('',*,*,#20011,.T.) ;
#29152 = ORIENTED_EDGE('',*,*,#20012,.T.) ;
#29153 = ORIENTED_EDGE('',*,*,#20013,.T.) ;
#29154 = ORIENTED_EDGE('',*,*,#20014,.T.) ;
#29155 = ORIENTED_EDGE('',*,*,#20015,.T.) ;
#29156 = ORIENTED_EDGE('',*,*,#20016,.F.) ;
#29157 = ORIENTED_EDGE('',*,*,#20017,.F.) ;
#29158 = ORIENTED_EDGE('',*,*,#20018,.T.) ;
#29159 = ORIENTED_EDGE('',*,*,#20019,.T.) ;
#29160 = ORIENTED_EDGE('',*,*,#20020,.F.) ;
#29161 = ORIENTED_EDGE('',*,*,#20019,.F.) ;
#29162 = ORIENTED_EDGE('',*,*,#20021,.T.) ;
#29163 = ORIENTED_EDGE('',*,*,#20022,.F.) ;
#29164 = ORIENTED_EDGE('',*,*,#20016,.T.) ;
#29165 = ORIENTED_EDGE('',*,*,#20023,.F.) ;
#29166 = ORIENTED_EDGE('',*,*,#20011,.F.) ;
#29167 = ORIENTED_EDGE('',*,*,#20024,.F.) ;
#29168 = ORIENTED_EDGE('',*,*,#20020,.T.) ;
#29169 = ORIENTED_EDGE('',*,*,#20025,.T.) ;
#29170 = ORIENTED_EDGE('',*,*,#20013,.F.) ;
#29171 = ORIENTED_EDGE('',*,*,#20026,.F.) ;
#29172 = ORIENTED_EDGE('',*,*,#20022,.T.) ;
#29173 = ORIENTED_EDGE('',*,*,#20024,.T.) ;
#29174 = ORIENTED_EDGE('',*,*,#20010,.F.) ;
#29175 = ORIENTED_EDGE('',*,*,#20025,.F.) ;
#29176 = ORIENTED_EDGE('',*,*,#20027,.F.) ;
#29177 = ORIENTED_EDGE('',*,*,#20028,.F.) ;
#29178 = ORIENTED_EDGE('',*,*,#20029,.F.) ;
#29179 = ORIENTED_EDGE('',*,*,#20030,.F.) ;
#29180 = ORIENTED_EDGE('',*,*,#20031,.T.) ;
#29181 = ORIENTED_EDGE('',*,*,#20032,.F.) ;
#29182 = ORIENTED_EDGE('',*,*,#20033,.T.) ;
#29183 = ORIENTED_EDGE('',*,*,#20034,.T.) ;
#29184 = ORIENTED_EDGE('',*,*,#20035,.F.) ;
#29185 = ORIENTED_EDGE('',*,*,#20036,.T.) ;
#29186 = ORIENTED_EDGE('',*,*,#20037,.T.) ;
#29187 = ORIENTED_EDGE('',*,*,#20038,.T.) ;
#29188 = ORIENTED_EDGE('',*,*,#20039,.T.) ;
#29189 = ORIENTED_EDGE('',*,*,#20035,.T.) ;
#29190 = ORIENTED_EDGE('',*,*,#20040,.T.) ;
#29191 = ORIENTED_EDGE('',*,*,#20029,.T.) ;
#29192 = ORIENTED_EDGE('',*,*,#20041,.T.) ;
#29193 = ORIENTED_EDGE('',*,*,#20031,.F.) ;
#29194 = ORIENTED_EDGE('',*,*,#20042,.T.) ;
#29195 = ORIENTED_EDGE('',*,*,#20027,.T.) ;
#29196 = ORIENTED_EDGE('',*,*,#20043,.F.) ;
#29197 = ORIENTED_EDGE('',*,*,#20034,.F.) ;
#29198 = ORIENTED_EDGE('',*,*,#20043,.T.) ;
#29199 = ORIENTED_EDGE('',*,*,#20030,.T.) ;
#29200 = ORIENTED_EDGE('',*,*,#20040,.F.) ;
#29201 = ORIENTED_EDGE('',*,*,#20038,.F.) ;
#29202 = ORIENTED_EDGE('',*,*,#20044,.F.) ;
#29203 = ORIENTED_EDGE('',*,*,#20045,.F.) ;
#29204 = ORIENTED_EDGE('',*,*,#20046,.F.) ;
#29205 = ORIENTED_EDGE('',*,*,#20047,.F.) ;
#29206 = ORIENTED_EDGE('',*,*,#20048,.T.) ;
#29207 = ORIENTED_EDGE('',*,*,#20049,.F.) ;
#29208 = ORIENTED_EDGE('',*,*,#20050,.T.) ;
#29209 = ORIENTED_EDGE('',*,*,#20051,.T.) ;
#29210 = ORIENTED_EDGE('',*,*,#20052,.F.) ;
#29211 = ORIENTED_EDGE('',*,*,#20053,.T.) ;
#29212 = ORIENTED_EDGE('',*,*,#20054,.T.) ;
#29213 = ORIENTED_EDGE('',*,*,#20055,.T.) ;
#29214 = ORIENTED_EDGE('',*,*,#20056,.T.) ;
#29215 = ORIENTED_EDGE('',*,*,#20052,.T.) ;
#29216 = ORIENTED_EDGE('',*,*,#20057,.T.) ;
#29217 = ORIENTED_EDGE('',*,*,#20046,.T.) ;
#29218 = ORIENTED_EDGE('',*,*,#20058,.T.) ;
#29219 = ORIENTED_EDGE('',*,*,#20048,.F.) ;
#29220 = ORIENTED_EDGE('',*,*,#20059,.T.) ;
#29221 = ORIENTED_EDGE('',*,*,#20044,.T.) ;
#29222 = ORIENTED_EDGE('',*,*,#20060,.F.) ;
#29223 = ORIENTED_EDGE('',*,*,#20051,.F.) ;
#29224 = ORIENTED_EDGE('',*,*,#20060,.T.) ;
#29225 = ORIENTED_EDGE('',*,*,#20047,.T.) ;
#29226 = ORIENTED_EDGE('',*,*,#20057,.F.) ;
#29227 = ORIENTED_EDGE('',*,*,#20055,.F.) ;
#29228 = ORIENTED_EDGE('',*,*,#20061,.T.) ;
#29229 = ORIENTED_EDGE('',*,*,#19869,.T.) ;
#29230 = ORIENTED_EDGE('',*,*,#19904,.T.) ;
#29231 = ORIENTED_EDGE('',*,*,#19932,.T.) ;
#29232 = ORIENTED_EDGE('',*,*,#19978,.T.) ;
#29233 = ORIENTED_EDGE('',*,*,#19985,.T.) ;
#29234 = ORIENTED_EDGE('',*,*,#19906,.T.) ;
#29235 = ORIENTED_EDGE('',*,*,#19986,.T.) ;
#29236 = ORIENTED_EDGE('',*,*,#19982,.F.) ;
#29237 = ORIENTED_EDGE('',*,*,#19933,.T.) ;
#29238 = ORIENTED_EDGE('',*,*,#19900,.T.) ;
#29239 = ORIENTED_EDGE('',*,*,#19878,.T.) ;
#29240 = ORIENTED_EDGE('',*,*,#20062,.T.) ;
#29241 = ORIENTED_EDGE('',*,*,#20063,.F.) ;
#29242 = ORIENTED_EDGE('',*,*,#20064,.F.) ;
#29243 = ORIENTED_EDGE('',*,*,#20000,.T.) ;
#29244 = ORIENTED_EDGE('',*,*,#20009,.T.) ;
#29245 = ORIENTED_EDGE('',*,*,#19995,.F.) ;
#29246 = ORIENTED_EDGE('',*,*,#20006,.T.) ;
#29247 = ORIENTED_EDGE('',*,*,#19998,.F.) ;
#29248 = ORIENTED_EDGE('',*,*,#20065,.F.) ;
#29249 = ORIENTED_EDGE('',*,*,#20066,.F.) ;
#29250 = ORIENTED_EDGE('',*,*,#20067,.T.) ;
#29251 = ORIENTED_EDGE('',*,*,#19872,.T.) ;
#29252 = ORIENTED_EDGE('',*,*,#19894,.T.) ;
#29253 = ORIENTED_EDGE('',*,*,#19991,.T.) ;
#29254 = ORIENTED_EDGE('',*,*,#19955,.T.) ;
#29255 = ORIENTED_EDGE('',*,*,#19964,.T.) ;
#29256 = ORIENTED_EDGE('',*,*,#19909,.T.) ;
#29257 = ORIENTED_EDGE('',*,*,#19965,.T.) ;
#29258 = ORIENTED_EDGE('',*,*,#19957,.F.) ;
#29259 = ORIENTED_EDGE('',*,*,#19992,.T.) ;
#29260 = ORIENTED_EDGE('',*,*,#19890,.T.) ;
#29261 = ORIENTED_EDGE('',*,*,#19874,.T.) ;
#29262 = ORIENTED_EDGE('',*,*,#20068,.T.) ;
#29263 = ORIENTED_EDGE('',*,*,#20069,.F.) ;
#29264 = ORIENTED_EDGE('',*,*,#20070,.F.) ;
#29265 = ORIENTED_EDGE('',*,*,#20049,.T.) ;
#29266 = ORIENTED_EDGE('',*,*,#20058,.F.) ;
#29267 = ORIENTED_EDGE('',*,*,#20045,.T.) ;
#29268 = ORIENTED_EDGE('',*,*,#20059,.F.) ;
#29269 = ORIENTED_EDGE('',*,*,#20054,.F.) ;
#29270 = ORIENTED_EDGE('',*,*,#20071,.F.) ;
#29271 = ORIENTED_EDGE('',*,*,#20072,.F.) ;
#29272 = ORIENTED_EDGE('',*,*,#20073,.T.) ;
#29273 = ORIENTED_EDGE('',*,*,#19876,.T.) ;
#29274 = ORIENTED_EDGE('',*,*,#19889,.T.) ;
#29275 = ORIENTED_EDGE('',*,*,#19939,.T.) ;
#29276 = ORIENTED_EDGE('',*,*,#19943,.T.) ;
#29277 = ORIENTED_EDGE('',*,*,#19950,.T.) ;
#29278 = ORIENTED_EDGE('',*,*,#19914,.T.) ;
#29279 = ORIENTED_EDGE('',*,*,#19951,.T.) ;
#29280 = ORIENTED_EDGE('',*,*,#19947,.F.) ;
#29281 = ORIENTED_EDGE('',*,*,#19940,.T.) ;
#29282 = ORIENTED_EDGE('',*,*,#19885,.T.) ;
#29283 = ORIENTED_EDGE('',*,*,#19867,.T.) ;
#29284 = ORIENTED_EDGE('',*,*,#20074,.T.) ;
#29285 = ORIENTED_EDGE('',*,*,#20075,.F.) ;
#29286 = ORIENTED_EDGE('',*,*,#20076,.F.) ;
#29287 = ORIENTED_EDGE('',*,*,#20017,.T.) ;
#29288 = ORIENTED_EDGE('',*,*,#20026,.T.) ;
#29289 = ORIENTED_EDGE('',*,*,#20012,.F.) ;
#29290 = ORIENTED_EDGE('',*,*,#20023,.T.) ;
#29291 = ORIENTED_EDGE('',*,*,#20015,.F.) ;
#29292 = ORIENTED_EDGE('',*,*,#20077,.F.) ;
#29293 = ORIENTED_EDGE('',*,*,#20078,.F.) ;
#29294 = ORIENTED_EDGE('',*,*,#20079,.T.) ;
#29295 = ORIENTED_EDGE('',*,*,#19880,.T.) ;
#29296 = ORIENTED_EDGE('',*,*,#19899,.T.) ;
#29297 = ORIENTED_EDGE('',*,*,#19925,.T.) ;
#29298 = ORIENTED_EDGE('',*,*,#19967,.T.) ;
#29299 = ORIENTED_EDGE('',*,*,#19975,.T.) ;
#29300 = ORIENTED_EDGE('',*,*,#19917,.T.) ;
#29301 = ORIENTED_EDGE('',*,*,#19976,.T.) ;
#29302 = ORIENTED_EDGE('',*,*,#19971,.F.) ;
#29303 = ORIENTED_EDGE('',*,*,#19926,.T.) ;
#29304 = ORIENTED_EDGE('',*,*,#19895,.T.) ;
#29305 = ORIENTED_EDGE('',*,*,#19863,.T.) ;
#29306 = ORIENTED_EDGE('',*,*,#20080,.T.) ;
#29307 = ORIENTED_EDGE('',*,*,#20081,.F.) ;
#29308 = ORIENTED_EDGE('',*,*,#20082,.F.) ;
#29309 = ORIENTED_EDGE('',*,*,#20032,.T.) ;
#29310 = ORIENTED_EDGE('',*,*,#20041,.F.) ;
#29311 = ORIENTED_EDGE('',*,*,#20028,.T.) ;
#29312 = ORIENTED_EDGE('',*,*,#20042,.F.) ;
#29313 = ORIENTED_EDGE('',*,*,#20037,.F.) ;
#29314 = ORIENTED_EDGE('',*,*,#20083,.F.) ;
#29315 = ORIENTED_EDGE('',*,*,#20084,.F.) ;
#29316 = ORIENTED_EDGE('',*,*,#20065,.T.) ;
#29317 = ORIENTED_EDGE('',*,*,#19997,.F.) ;
#29318 = ORIENTED_EDGE('',*,*,#20004,.F.) ;
#29319 = ORIENTED_EDGE('',*,*,#20001,.F.) ;
#29320 = ORIENTED_EDGE('',*,*,#20064,.T.) ;
#29321 = ORIENTED_EDGE('',*,*,#20085,.F.) ;
#29322 = ORIENTED_EDGE('',*,*,#20083,.T.) ;
#29323 = ORIENTED_EDGE('',*,*,#20036,.F.) ;
#29324 = ORIENTED_EDGE('',*,*,#20039,.F.) ;
#29325 = ORIENTED_EDGE('',*,*,#20033,.F.) ;
#29326 = ORIENTED_EDGE('',*,*,#20082,.T.) ;
#29327 = ORIENTED_EDGE('',*,*,#20086,.F.) ;
#29328 = ORIENTED_EDGE('',*,*,#20087,.F.) ;
#29329 = ORIENTED_EDGE('',*,*,#20071,.T.) ;
#29330 = ORIENTED_EDGE('',*,*,#20053,.F.) ;
#29331 = ORIENTED_EDGE('',*,*,#20056,.F.) ;
#29332 = ORIENTED_EDGE('',*,*,#20050,.F.) ;
#29333 = ORIENTED_EDGE('',*,*,#20070,.T.) ;
#29334 = ORIENTED_EDGE('',*,*,#20088,.F.) ;
#29335 = ORIENTED_EDGE('',*,*,#20077,.T.) ;
#29336 = ORIENTED_EDGE('',*,*,#20014,.F.) ;
#29337 = ORIENTED_EDGE('',*,*,#20021,.F.) ;
#29338 = ORIENTED_EDGE('',*,*,#20018,.F.) ;
#29339 = ORIENTED_EDGE('',*,*,#20076,.T.) ;
#29340 = ORIENTED_EDGE('',*,*,#20089,.F.) ;
#29341 = ORIENTED_EDGE('',*,*,#19884,.F.) ;
#29342 = ORIENTED_EDGE('',*,*,#20090,.T.) ;
#29343 = ORIENTED_EDGE('',*,*,#20091,.T.) ;
#29344 = ORIENTED_EDGE('',*,*,#20089,.T.) ;
#29345 = ORIENTED_EDGE('',*,*,#20092,.T.) ;
#29346 = ORIENTED_EDGE('',*,*,#20093,.T.) ;
#29347 = ORIENTED_EDGE('',*,*,#20066,.T.) ;
#29348 = ORIENTED_EDGE('',*,*,#20091,.F.) ;
#29349 = ORIENTED_EDGE('',*,*,#20094,.T.) ;
#29350 = ORIENTED_EDGE('',*,*,#20092,.F.) ;
#29351 = ORIENTED_EDGE('',*,*,#20075,.T.) ;
#29352 = ORIENTED_EDGE('',*,*,#20095,.T.) ;
#29353 = ORIENTED_EDGE('',*,*,#20096,.T.) ;
#29354 = ORIENTED_EDGE('',*,*,#20088,.T.) ;
#29355 = ORIENTED_EDGE('',*,*,#20097,.T.) ;
#29356 = ORIENTED_EDGE('',*,*,#20098,.T.) ;
#29357 = ORIENTED_EDGE('',*,*,#20097,.F.) ;
#29358 = ORIENTED_EDGE('',*,*,#20069,.T.) ;
#29359 = ORIENTED_EDGE('',*,*,#20099,.T.) ;
#29360 = ORIENTED_EDGE('',*,*,#20078,.T.) ;
#29361 = ORIENTED_EDGE('',*,*,#20096,.F.) ;
#29362 = ORIENTED_EDGE('',*,*,#20100,.T.) ;
#29363 = ORIENTED_EDGE('',*,*,#20101,.T.) ;
#29364 = ORIENTED_EDGE('',*,*,#20087,.T.) ;
#29365 = ORIENTED_EDGE('',*,*,#20102,.F.) ;
#29366 = ORIENTED_EDGE('',*,*,#20103,.T.) ;
#29367 = ORIENTED_EDGE('',*,*,#20102,.T.) ;
#29368 = ORIENTED_EDGE('',*,*,#20086,.T.) ;
#29369 = ORIENTED_EDGE('',*,*,#20104,.T.) ;
#29370 = ORIENTED_EDGE('',*,*,#20105,.T.) ;
#29371 = ORIENTED_EDGE('',*,*,#20072,.T.) ;
#29372 = ORIENTED_EDGE('',*,*,#20101,.F.) ;
#29373 = ORIENTED_EDGE('',*,*,#20106,.T.) ;
#29374 = ORIENTED_EDGE('',*,*,#20104,.F.) ;
#29375 = ORIENTED_EDGE('',*,*,#20081,.T.) ;
#29376 = ORIENTED_EDGE('',*,*,#20107,.T.) ;
#29377 = ORIENTED_EDGE('',*,*,#20108,.T.) ;
#29378 = ORIENTED_EDGE('',*,*,#20085,.T.) ;
#29379 = ORIENTED_EDGE('',*,*,#20109,.T.) ;
#29380 = ORIENTED_EDGE('',*,*,#20110,.T.) ;
#29381 = ORIENTED_EDGE('',*,*,#20109,.F.) ;
#29382 = ORIENTED_EDGE('',*,*,#20063,.T.) ;
#29383 = ORIENTED_EDGE('',*,*,#20111,.T.) ;
#29384 = ORIENTED_EDGE('',*,*,#20084,.T.) ;
#29385 = ORIENTED_EDGE('',*,*,#20108,.F.) ;
#29386 = ORIENTED_EDGE('',*,*,#20100,.F.) ;
#29387 = ORIENTED_EDGE('',*,*,#20103,.F.) ;
#29388 = ORIENTED_EDGE('',*,*,#20106,.F.) ;
#29389 = ORIENTED_EDGE('',*,*,#20080,.F.) ;
#29390 = ORIENTED_EDGE('',*,*,#19866,.T.) ;
#29391 = ORIENTED_EDGE('',*,*,#19873,.T.) ;
#29392 = ORIENTED_EDGE('',*,*,#20067,.F.) ;
#29393 = ORIENTED_EDGE('',*,*,#20105,.F.) ;
#29394 = ORIENTED_EDGE('',*,*,#20074,.F.) ;
#29395 = ORIENTED_EDGE('',*,*,#19870,.T.) ;
#29396 = ORIENTED_EDGE('',*,*,#20061,.F.) ;
#29397 = ORIENTED_EDGE('',*,*,#20093,.F.) ;
#29398 = ORIENTED_EDGE('',*,*,#20090,.F.) ;
#29399 = ORIENTED_EDGE('',*,*,#20094,.F.) ;
#29400 = ORIENTED_EDGE('',*,*,#20095,.F.) ;
#29401 = ORIENTED_EDGE('',*,*,#20098,.F.) ;
#29402 = ORIENTED_EDGE('',*,*,#20068,.F.) ;
#29403 = ORIENTED_EDGE('',*,*,#19877,.T.) ;
#29404 = ORIENTED_EDGE('',*,*,#20073,.F.) ;
#29405 = ORIENTED_EDGE('',*,*,#20099,.F.) ;
#29406 = ORIENTED_EDGE('',*,*,#20107,.F.) ;
#29407 = ORIENTED_EDGE('',*,*,#20110,.F.) ;
#29408 = ORIENTED_EDGE('',*,*,#20062,.F.) ;
#29409 = ORIENTED_EDGE('',*,*,#19881,.T.) ;
#29410 = ORIENTED_EDGE('',*,*,#20079,.F.) ;
#29411 = ORIENTED_EDGE('',*,*,#20111,.F.) ;
#29412 = ORIENTED_EDGE('',*,*,#20112,.T.) ;
#29413 = ORIENTED_EDGE('',*,*,#20113,.T.) ;
#29414 = ORIENTED_EDGE('',*,*,#20114,.T.) ;
#29415 = ORIENTED_EDGE('',*,*,#20115,.T.) ;
#29416 = ORIENTED_EDGE('',*,*,#20116,.T.) ;
#29417 = ORIENTED_EDGE('',*,*,#20117,.T.) ;
#29418 = ORIENTED_EDGE('',*,*,#20115,.F.) ;
#29419 = ORIENTED_EDGE('',*,*,#20118,.F.) ;
#29420 = ORIENTED_EDGE('',*,*,#20119,.T.) ;
#29421 = ORIENTED_EDGE('',*,*,#20120,.F.) ;
#29422 = ORIENTED_EDGE('',*,*,#20121,.F.) ;
#29423 = ORIENTED_EDGE('',*,*,#20122,.T.) ;
#29424 = ORIENTED_EDGE('',*,*,#20114,.F.) ;
#29425 = ORIENTED_EDGE('',*,*,#20123,.T.) ;
#29426 = ORIENTED_EDGE('',*,*,#20124,.F.) ;
#29427 = ORIENTED_EDGE('',*,*,#20125,.T.) ;
#29428 = ORIENTED_EDGE('',*,*,#20126,.T.) ;
#29429 = ORIENTED_EDGE('',*,*,#20118,.T.) ;
#29430 = ORIENTED_EDGE('',*,*,#20113,.F.) ;
#29431 = ORIENTED_EDGE('',*,*,#20127,.F.) ;
#29432 = ORIENTED_EDGE('',*,*,#20128,.F.) ;
#29433 = ORIENTED_EDGE('',*,*,#20123,.F.) ;
#29434 = ORIENTED_EDGE('',*,*,#20129,.T.) ;
#29435 = ORIENTED_EDGE('',*,*,#20130,.T.) ;
#29436 = ORIENTED_EDGE('',*,*,#20131,.T.) ;
#29437 = ORIENTED_EDGE('',*,*,#20124,.T.) ;
#29438 = ORIENTED_EDGE('',*,*,#20128,.T.) ;
#29439 = ORIENTED_EDGE('',*,*,#20132,.T.) ;
#29440 = ORIENTED_EDGE('',*,*,#20131,.F.) ;
#29441 = ORIENTED_EDGE('',*,*,#20133,.T.) ;
#29442 = ORIENTED_EDGE('',*,*,#20134,.F.) ;
#29443 = ORIENTED_EDGE('',*,*,#20135,.F.) ;
#29444 = ORIENTED_EDGE('',*,*,#20136,.T.) ;
#29445 = ORIENTED_EDGE('',*,*,#20125,.F.) ;
#29446 = ORIENTED_EDGE('',*,*,#20137,.T.) ;
#29447 = ORIENTED_EDGE('',*,*,#20138,.T.) ;
#29448 = ORIENTED_EDGE('',*,*,#20139,.T.) ;
#29449 = ORIENTED_EDGE('',*,*,#20134,.T.) ;
#29450 = ORIENTED_EDGE('',*,*,#20140,.T.) ;
#29451 = ORIENTED_EDGE('',*,*,#20141,.T.) ;
#29452 = ORIENTED_EDGE('',*,*,#20139,.F.) ;
#29453 = ORIENTED_EDGE('',*,*,#20142,.T.) ;
#29454 = ORIENTED_EDGE('',*,*,#20143,.F.) ;
#29455 = ORIENTED_EDGE('',*,*,#20120,.T.) ;
#29456 = ORIENTED_EDGE('',*,*,#20144,.T.) ;
#29457 = ORIENTED_EDGE('',*,*,#20135,.T.) ;
#29458 = ORIENTED_EDGE('',*,*,#20138,.F.) ;
#29459 = ORIENTED_EDGE('',*,*,#20145,.F.) ;
#29460 = ORIENTED_EDGE('',*,*,#20146,.F.) ;
#29461 = ORIENTED_EDGE('',*,*,#20142,.F.) ;
#29462 = ORIENTED_EDGE('',*,*,#20137,.F.) ;
#29463 = ORIENTED_EDGE('',*,*,#20147,.F.) ;
#29464 = ORIENTED_EDGE('',*,*,#20148,.T.) ;
#29465 = ORIENTED_EDGE('',*,*,#20149,.F.) ;
#29466 = ORIENTED_EDGE('',*,*,#20150,.F.) ;
#29467 = ORIENTED_EDGE('',*,*,#20145,.T.) ;
#29468 = ORIENTED_EDGE('',*,*,#20143,.T.) ;
#29469 = ORIENTED_EDGE('',*,*,#20146,.T.) ;
#29470 = ORIENTED_EDGE('',*,*,#20150,.T.) ;
#29471 = ORIENTED_EDGE('',*,*,#20151,.T.) ;
#29472 = ORIENTED_EDGE('',*,*,#20152,.T.) ;
#29473 = ORIENTED_EDGE('',*,*,#20121,.T.) ;
#29474 = ORIENTED_EDGE('',*,*,#20144,.F.) ;
#29475 = ORIENTED_EDGE('',*,*,#20119,.F.) ;
#29476 = ORIENTED_EDGE('',*,*,#20126,.F.) ;
#29477 = ORIENTED_EDGE('',*,*,#20136,.F.) ;
#29478 = ORIENTED_EDGE('',*,*,#20130,.F.) ;
#29479 = ORIENTED_EDGE('',*,*,#20153,.F.) ;
#29480 = ORIENTED_EDGE('',*,*,#20140,.F.) ;
#29481 = ORIENTED_EDGE('',*,*,#20133,.F.) ;
#29482 = ORIENTED_EDGE('',*,*,#20154,.F.) ;
#29483 = ORIENTED_EDGE('',*,*,#20155,.F.) ;
#29484 = ORIENTED_EDGE('',*,*,#20156,.F.) ;
#29485 = ORIENTED_EDGE('',*,*,#20157,.F.) ;
#29486 = ORIENTED_EDGE('',*,*,#20158,.F.) ;
#29487 = ORIENTED_EDGE('',*,*,#20116,.F.) ;
#29488 = ORIENTED_EDGE('',*,*,#20122,.F.) ;
#29489 = ORIENTED_EDGE('',*,*,#20152,.F.) ;
#29490 = ORIENTED_EDGE('',*,*,#20159,.F.) ;
#29491 = ORIENTED_EDGE('',*,*,#20160,.F.) ;
#29492 = ORIENTED_EDGE('',*,*,#20161,.F.) ;
#29493 = ORIENTED_EDGE('',*,*,#20162,.F.) ;
#29494 = ORIENTED_EDGE('',*,*,#20163,.F.) ;
#29495 = ORIENTED_EDGE('',*,*,#20164,.F.) ;
#29496 = ORIENTED_EDGE('',*,*,#20129,.F.) ;
#29497 = ORIENTED_EDGE('',*,*,#20165,.T.) ;
#29498 = ORIENTED_EDGE('',*,*,#20166,.T.) ;
#29499 = ORIENTED_EDGE('',*,*,#20147,.T.) ;
#29500 = ORIENTED_EDGE('',*,*,#20141,.F.) ;
#29501 = ORIENTED_EDGE('',*,*,#20153,.T.) ;
#29502 = ORIENTED_EDGE('',*,*,#20166,.F.) ;
#29503 = ORIENTED_EDGE('',*,*,#20167,.F.) ;
#29504 = ORIENTED_EDGE('',*,*,#20168,.F.) ;
#29505 = ORIENTED_EDGE('',*,*,#20148,.F.) ;
#29506 = ORIENTED_EDGE('',*,*,#20117,.F.) ;
#29507 = ORIENTED_EDGE('',*,*,#20159,.T.) ;
#29508 = ORIENTED_EDGE('',*,*,#20151,.F.) ;
#29509 = ORIENTED_EDGE('',*,*,#20149,.T.) ;
#29510 = ORIENTED_EDGE('',*,*,#20168,.T.) ;
#29511 = ORIENTED_EDGE('',*,*,#20169,.T.) ;
#29512 = ORIENTED_EDGE('',*,*,#20112,.F.) ;
#29513 = ORIENTED_EDGE('',*,*,#20169,.F.) ;
#29514 = ORIENTED_EDGE('',*,*,#20167,.T.) ;
#29515 = ORIENTED_EDGE('',*,*,#20165,.F.) ;
#29516 = ORIENTED_EDGE('',*,*,#20132,.F.) ;
#29517 = ORIENTED_EDGE('',*,*,#20127,.T.) ;
#29518 = ORIENTED_EDGE('',*,*,#20158,.T.) ;
#29519 = ORIENTED_EDGE('',*,*,#20170,.T.) ;
#29520 = ORIENTED_EDGE('',*,*,#20164,.T.) ;
#29521 = ORIENTED_EDGE('',*,*,#20170,.F.) ;
#29522 = ORIENTED_EDGE('',*,*,#20157,.T.) ;
#29523 = ORIENTED_EDGE('',*,*,#20171,.T.) ;
#29524 = ORIENTED_EDGE('',*,*,#20163,.T.) ;
#29525 = ORIENTED_EDGE('',*,*,#20171,.F.) ;
#29526 = ORIENTED_EDGE('',*,*,#20156,.T.) ;
#29527 = ORIENTED_EDGE('',*,*,#20172,.T.) ;
#29528 = ORIENTED_EDGE('',*,*,#20162,.T.) ;
#29529 = ORIENTED_EDGE('',*,*,#20172,.F.) ;
#29530 = ORIENTED_EDGE('',*,*,#20155,.T.) ;
#29531 = ORIENTED_EDGE('',*,*,#20173,.T.) ;
#29532 = ORIENTED_EDGE('',*,*,#20161,.T.) ;
#29533 = ORIENTED_EDGE('',*,*,#20173,.F.) ;
#29534 = ORIENTED_EDGE('',*,*,#20154,.T.) ;
#29535 = ORIENTED_EDGE('',*,*,#20174,.T.) ;
#29536 = ORIENTED_EDGE('',*,*,#20160,.T.) ;
#29537 = ORIENTED_EDGE('',*,*,#20174,.F.) ;
#29538 = ORIENTED_EDGE('',*,*,#20175,.F.) ;
#29539 = ORIENTED_EDGE('',*,*,#20176,.F.) ;
#29540 = ORIENTED_EDGE('',*,*,#20177,.F.) ;
#29541 = ORIENTED_EDGE('',*,*,#20178,.T.) ;
#29542 = ORIENTED_EDGE('',*,*,#20179,.F.) ;
#29543 = ORIENTED_EDGE('',*,*,#20180,.F.) ;
#29544 = ORIENTED_EDGE('',*,*,#20175,.T.) ;
#29545 = ORIENTED_EDGE('',*,*,#20181,.T.) ;
#29546 = ORIENTED_EDGE('',*,*,#20182,.F.) ;
#29547 = ORIENTED_EDGE('',*,*,#20183,.F.) ;
#29548 = ORIENTED_EDGE('',*,*,#20179,.T.) ;
#29549 = ORIENTED_EDGE('',*,*,#20184,.T.) ;
#29550 = ORIENTED_EDGE('',*,*,#20185,.F.) ;
#29551 = ORIENTED_EDGE('',*,*,#20186,.F.) ;
#29552 = ORIENTED_EDGE('',*,*,#20182,.T.) ;
#29553 = ORIENTED_EDGE('',*,*,#20187,.T.) ;
#29554 = ORIENTED_EDGE('',*,*,#20188,.F.) ;
#29555 = ORIENTED_EDGE('',*,*,#20189,.F.) ;
#29556 = ORIENTED_EDGE('',*,*,#20185,.T.) ;
#29557 = ORIENTED_EDGE('',*,*,#20190,.T.) ;
#29558 = ORIENTED_EDGE('',*,*,#20191,.F.) ;
#29559 = ORIENTED_EDGE('',*,*,#20192,.F.) ;
#29560 = ORIENTED_EDGE('',*,*,#20188,.T.) ;
#29561 = ORIENTED_EDGE('',*,*,#20193,.T.) ;
#29562 = ORIENTED_EDGE('',*,*,#20194,.F.) ;
#29563 = ORIENTED_EDGE('',*,*,#20195,.F.) ;
#29564 = ORIENTED_EDGE('',*,*,#20191,.T.) ;
#29565 = ORIENTED_EDGE('',*,*,#20196,.T.) ;
#29566 = ORIENTED_EDGE('',*,*,#20197,.F.) ;
#29567 = ORIENTED_EDGE('',*,*,#20198,.F.) ;
#29568 = ORIENTED_EDGE('',*,*,#20194,.T.) ;
#29569 = ORIENTED_EDGE('',*,*,#20199,.T.) ;
#29570 = ORIENTED_EDGE('',*,*,#20200,.F.) ;
#29571 = ORIENTED_EDGE('',*,*,#20201,.F.) ;
#29572 = ORIENTED_EDGE('',*,*,#20197,.T.) ;
#29573 = ORIENTED_EDGE('',*,*,#20202,.T.) ;
#29574 = ORIENTED_EDGE('',*,*,#20203,.F.) ;
#29575 = ORIENTED_EDGE('',*,*,#20204,.F.) ;
#29576 = ORIENTED_EDGE('',*,*,#20200,.T.) ;
#29577 = ORIENTED_EDGE('',*,*,#20205,.T.) ;
#29578 = ORIENTED_EDGE('',*,*,#20206,.F.) ;
#29579 = ORIENTED_EDGE('',*,*,#20207,.F.) ;
#29580 = ORIENTED_EDGE('',*,*,#20203,.T.) ;
#29581 = ORIENTED_EDGE('',*,*,#20208,.T.) ;
#29582 = ORIENTED_EDGE('',*,*,#20209,.F.) ;
#29583 = ORIENTED_EDGE('',*,*,#20210,.F.) ;
#29584 = ORIENTED_EDGE('',*,*,#20206,.T.) ;
#29585 = ORIENTED_EDGE('',*,*,#20211,.T.) ;
#29586 = ORIENTED_EDGE('',*,*,#20212,.F.) ;
#29587 = ORIENTED_EDGE('',*,*,#20213,.F.) ;
#29588 = ORIENTED_EDGE('',*,*,#20209,.T.) ;
#29589 = ORIENTED_EDGE('',*,*,#20214,.T.) ;
#29590 = ORIENTED_EDGE('',*,*,#20215,.F.) ;
#29591 = ORIENTED_EDGE('',*,*,#20216,.F.) ;
#29592 = ORIENTED_EDGE('',*,*,#20212,.T.) ;
#29593 = ORIENTED_EDGE('',*,*,#20217,.T.) ;
#29594 = ORIENTED_EDGE('',*,*,#20218,.F.) ;
#29595 = ORIENTED_EDGE('',*,*,#20219,.F.) ;
#29596 = ORIENTED_EDGE('',*,*,#20215,.T.) ;
#29597 = ORIENTED_EDGE('',*,*,#20220,.T.) ;
#29598 = ORIENTED_EDGE('',*,*,#20221,.F.) ;
#29599 = ORIENTED_EDGE('',*,*,#20222,.F.) ;
#29600 = ORIENTED_EDGE('',*,*,#20223,.T.) ;
#29601 = ORIENTED_EDGE('',*,*,#20224,.F.) ;
#29602 = ORIENTED_EDGE('',*,*,#20225,.T.) ;
#29603 = ORIENTED_EDGE('',*,*,#20226,.F.) ;
#29604 = ORIENTED_EDGE('',*,*,#20227,.F.) ;
#29605 = ORIENTED_EDGE('',*,*,#20221,.T.) ;
#29606 = ORIENTED_EDGE('',*,*,#20228,.T.) ;
#29607 = ORIENTED_EDGE('',*,*,#20229,.F.) ;
#29608 = ORIENTED_EDGE('',*,*,#20230,.F.) ;
#29609 = ORIENTED_EDGE('',*,*,#20226,.T.) ;
#29610 = ORIENTED_EDGE('',*,*,#20231,.T.) ;
#29611 = ORIENTED_EDGE('',*,*,#20232,.F.) ;
#29612 = ORIENTED_EDGE('',*,*,#20233,.F.) ;
#29613 = ORIENTED_EDGE('',*,*,#20229,.T.) ;
#29614 = ORIENTED_EDGE('',*,*,#20234,.T.) ;
#29615 = ORIENTED_EDGE('',*,*,#20235,.F.) ;
#29616 = ORIENTED_EDGE('',*,*,#20236,.F.) ;
#29617 = ORIENTED_EDGE('',*,*,#20232,.T.) ;
#29618 = ORIENTED_EDGE('',*,*,#20237,.T.) ;
#29619 = ORIENTED_EDGE('',*,*,#20238,.F.) ;
#29620 = ORIENTED_EDGE('',*,*,#20239,.F.) ;
#29621 = ORIENTED_EDGE('',*,*,#20235,.T.) ;
#29622 = ORIENTED_EDGE('',*,*,#20240,.T.) ;
#29623 = ORIENTED_EDGE('',*,*,#20241,.F.) ;
#29624 = ORIENTED_EDGE('',*,*,#20242,.F.) ;
#29625 = ORIENTED_EDGE('',*,*,#20238,.T.) ;
#29626 = ORIENTED_EDGE('',*,*,#20243,.T.) ;
#29627 = ORIENTED_EDGE('',*,*,#20244,.F.) ;
#29628 = ORIENTED_EDGE('',*,*,#20245,.F.) ;
#29629 = ORIENTED_EDGE('',*,*,#20241,.T.) ;
#29630 = ORIENTED_EDGE('',*,*,#20246,.T.) ;
#29631 = ORIENTED_EDGE('',*,*,#20247,.F.) ;
#29632 = ORIENTED_EDGE('',*,*,#20248,.F.) ;
#29633 = ORIENTED_EDGE('',*,*,#20244,.T.) ;
#29634 = ORIENTED_EDGE('',*,*,#20249,.T.) ;
#29635 = ORIENTED_EDGE('',*,*,#20250,.F.) ;
#29636 = ORIENTED_EDGE('',*,*,#20251,.F.) ;
#29637 = ORIENTED_EDGE('',*,*,#20247,.T.) ;
#29638 = ORIENTED_EDGE('',*,*,#20252,.T.) ;
#29639 = ORIENTED_EDGE('',*,*,#20253,.F.) ;
#29640 = ORIENTED_EDGE('',*,*,#20254,.F.) ;
#29641 = ORIENTED_EDGE('',*,*,#20250,.T.) ;
#29642 = ORIENTED_EDGE('',*,*,#20255,.T.) ;
#29643 = ORIENTED_EDGE('',*,*,#20256,.F.) ;
#29644 = ORIENTED_EDGE('',*,*,#20257,.F.) ;
#29645 = ORIENTED_EDGE('',*,*,#20253,.T.) ;
#29646 = ORIENTED_EDGE('',*,*,#20258,.T.) ;
#29647 = ORIENTED_EDGE('',*,*,#20259,.F.) ;
#29648 = ORIENTED_EDGE('',*,*,#20260,.F.) ;
#29649 = ORIENTED_EDGE('',*,*,#20256,.T.) ;
#29650 = ORIENTED_EDGE('',*,*,#20261,.T.) ;
#29651 = ORIENTED_EDGE('',*,*,#20262,.F.) ;
#29652 = ORIENTED_EDGE('',*,*,#20263,.F.) ;
#29653 = ORIENTED_EDGE('',*,*,#20259,.T.) ;
#29654 = ORIENTED_EDGE('',*,*,#20264,.T.) ;
#29655 = ORIENTED_EDGE('',*,*,#20265,.F.) ;
#29656 = ORIENTED_EDGE('',*,*,#20266,.F.) ;
#29657 = ORIENTED_EDGE('',*,*,#20262,.T.) ;
#29658 = ORIENTED_EDGE('',*,*,#20267,.T.) ;
#29659 = ORIENTED_EDGE('',*,*,#20268,.F.) ;
#29660 = ORIENTED_EDGE('',*,*,#20269,.F.) ;
#29661 = ORIENTED_EDGE('',*,*,#20265,.T.) ;
#29662 = ORIENTED_EDGE('',*,*,#20270,.T.) ;
#29663 = ORIENTED_EDGE('',*,*,#20271,.F.) ;
#29664 = ORIENTED_EDGE('',*,*,#20272,.T.) ;
#29665 = ORIENTED_EDGE('',*,*,#20273,.F.) ;
#29666 = ORIENTED_EDGE('',*,*,#20274,.T.) ;
#29667 = ORIENTED_EDGE('',*,*,#20271,.T.) ;
#29668 = ORIENTED_EDGE('',*,*,#20275,.T.) ;
#29669 = ORIENTED_EDGE('',*,*,#20276,.T.) ;
#29670 = ORIENTED_EDGE('',*,*,#20177,.T.) ;
#29671 = ORIENTED_EDGE('',*,*,#20277,.T.) ;
#29672 = ORIENTED_EDGE('',*,*,#20268,.T.) ;
#29673 = ORIENTED_EDGE('',*,*,#20278,.T.) ;
#29674 = ORIENTED_EDGE('',*,*,#20279,.F.) ;
#29675 = ORIENTED_EDGE('',*,*,#20280,.F.) ;
#29676 = ORIENTED_EDGE('',*,*,#20218,.T.) ;
#29677 = ORIENTED_EDGE('',*,*,#20281,.T.) ;
#29678 = ORIENTED_EDGE('',*,*,#20282,.F.) ;
#29679 = ORIENTED_EDGE('',*,*,#20283,.F.) ;
#29680 = ORIENTED_EDGE('',*,*,#20284,.F.) ;
#29681 = ORIENTED_EDGE('',*,*,#20285,.T.) ;
#29682 = ORIENTED_EDGE('',*,*,#20286,.T.) ;
#29683 = ORIENTED_EDGE('',*,*,#20287,.F.) ;
#29684 = ORIENTED_EDGE('',*,*,#20288,.F.) ;
#29685 = ORIENTED_EDGE('',*,*,#20289,.T.) ;
#29686 = ORIENTED_EDGE('',*,*,#20290,.T.) ;
#29687 = ORIENTED_EDGE('',*,*,#20291,.F.) ;
#29688 = ORIENTED_EDGE('',*,*,#20292,.F.) ;
#29689 = ORIENTED_EDGE('',*,*,#20293,.T.) ;
#29690 = ORIENTED_EDGE('',*,*,#20294,.T.) ;
#29691 = ORIENTED_EDGE('',*,*,#20295,.T.) ;
#29692 = ORIENTED_EDGE('',*,*,#20293,.F.) ;
#29693 = ORIENTED_EDGE('',*,*,#20292,.T.) ;
#29694 = ORIENTED_EDGE('',*,*,#20296,.F.) ;
#29695 = ORIENTED_EDGE('',*,*,#20297,.F.) ;
#29696 = ORIENTED_EDGE('',*,*,#20298,.F.) ;
#29697 = ORIENTED_EDGE('',*,*,#20299,.F.) ;
#29698 = ORIENTED_EDGE('',*,*,#20300,.F.) ;
#29699 = ORIENTED_EDGE('',*,*,#20290,.F.) ;
#29700 = ORIENTED_EDGE('',*,*,#20301,.F.) ;
#29701 = ORIENTED_EDGE('',*,*,#20302,.F.) ;
#29702 = ORIENTED_EDGE('',*,*,#20303,.F.) ;
#29703 = ORIENTED_EDGE('',*,*,#20304,.F.) ;
#29704 = ORIENTED_EDGE('',*,*,#20286,.F.) ;
#29705 = ORIENTED_EDGE('',*,*,#20305,.F.) ;
#29706 = ORIENTED_EDGE('',*,*,#20306,.F.) ;
#29707 = ORIENTED_EDGE('',*,*,#20307,.F.) ;
#29708 = ORIENTED_EDGE('',*,*,#20308,.F.) ;
#29709 = ORIENTED_EDGE('',*,*,#20309,.F.) ;
#29710 = ORIENTED_EDGE('',*,*,#20310,.F.) ;
#29711 = ORIENTED_EDGE('',*,*,#20311,.F.) ;
#29712 = ORIENTED_EDGE('',*,*,#20312,.F.) ;
#29713 = ORIENTED_EDGE('',*,*,#20313,.F.) ;
#29714 = ORIENTED_EDGE('',*,*,#20314,.T.) ;
#29715 = ORIENTED_EDGE('',*,*,#20315,.T.) ;
#29716 = ORIENTED_EDGE('',*,*,#20294,.F.) ;
#29717 = ORIENTED_EDGE('',*,*,#20295,.F.) ;
#29718 = ORIENTED_EDGE('',*,*,#20315,.F.) ;
#29719 = ORIENTED_EDGE('',*,*,#20316,.T.) ;
#29720 = ORIENTED_EDGE('',*,*,#20314,.F.) ;
#29721 = ORIENTED_EDGE('',*,*,#20317,.T.) ;
#29722 = ORIENTED_EDGE('',*,*,#20318,.T.) ;
#29723 = ORIENTED_EDGE('',*,*,#20317,.F.) ;
#29724 = ORIENTED_EDGE('',*,*,#20316,.F.) ;
#29725 = ORIENTED_EDGE('',*,*,#20318,.F.) ;
#29726 = ORIENTED_EDGE('',*,*,#20282,.T.) ;
#29727 = ORIENTED_EDGE('',*,*,#20319,.T.) ;
#29728 = ORIENTED_EDGE('',*,*,#20279,.T.) ;
#29729 = ORIENTED_EDGE('',*,*,#20320,.T.) ;
#29730 = ORIENTED_EDGE('',*,*,#20320,.F.) ;
#29731 = ORIENTED_EDGE('',*,*,#20278,.F.) ;
#29732 = ORIENTED_EDGE('',*,*,#20270,.F.) ;
#29733 = ORIENTED_EDGE('',*,*,#20267,.F.) ;
#29734 = ORIENTED_EDGE('',*,*,#20264,.F.) ;
#29735 = ORIENTED_EDGE('',*,*,#20261,.F.) ;
#29736 = ORIENTED_EDGE('',*,*,#20258,.F.) ;
#29737 = ORIENTED_EDGE('',*,*,#20255,.F.) ;
#29738 = ORIENTED_EDGE('',*,*,#20252,.F.) ;
#29739 = ORIENTED_EDGE('',*,*,#20249,.F.) ;
#29740 = ORIENTED_EDGE('',*,*,#20246,.F.) ;
#29741 = ORIENTED_EDGE('',*,*,#20243,.F.) ;
#29742 = ORIENTED_EDGE('',*,*,#20240,.F.) ;
#29743 = ORIENTED_EDGE('',*,*,#20237,.F.) ;
#29744 = ORIENTED_EDGE('',*,*,#20234,.F.) ;
#29745 = ORIENTED_EDGE('',*,*,#20231,.F.) ;
#29746 = ORIENTED_EDGE('',*,*,#20228,.F.) ;
#29747 = ORIENTED_EDGE('',*,*,#20225,.F.) ;
#29748 = ORIENTED_EDGE('',*,*,#20321,.F.) ;
#29749 = ORIENTED_EDGE('',*,*,#20272,.F.) ;
#29750 = ORIENTED_EDGE('',*,*,#20277,.F.) ;
#29751 = ORIENTED_EDGE('',*,*,#20176,.T.) ;
#29752 = ORIENTED_EDGE('',*,*,#20180,.T.) ;
#29753 = ORIENTED_EDGE('',*,*,#20183,.T.) ;
#29754 = ORIENTED_EDGE('',*,*,#20186,.T.) ;
#29755 = ORIENTED_EDGE('',*,*,#20189,.T.) ;
#29756 = ORIENTED_EDGE('',*,*,#20192,.T.) ;
#29757 = ORIENTED_EDGE('',*,*,#20195,.T.) ;
#29758 = ORIENTED_EDGE('',*,*,#20198,.T.) ;
#29759 = ORIENTED_EDGE('',*,*,#20201,.T.) ;
#29760 = ORIENTED_EDGE('',*,*,#20204,.T.) ;
#29761 = ORIENTED_EDGE('',*,*,#20207,.T.) ;
#29762 = ORIENTED_EDGE('',*,*,#20210,.T.) ;
#29763 = ORIENTED_EDGE('',*,*,#20213,.T.) ;
#29764 = ORIENTED_EDGE('',*,*,#20216,.T.) ;
#29765 = ORIENTED_EDGE('',*,*,#20219,.T.) ;
#29766 = ORIENTED_EDGE('',*,*,#20283,.T.) ;
#29767 = ORIENTED_EDGE('',*,*,#20319,.F.) ;
#29768 = ORIENTED_EDGE('',*,*,#20281,.F.) ;
#29769 = ORIENTED_EDGE('',*,*,#20220,.F.) ;
#29770 = ORIENTED_EDGE('',*,*,#20217,.F.) ;
#29771 = ORIENTED_EDGE('',*,*,#20214,.F.) ;
#29772 = ORIENTED_EDGE('',*,*,#20211,.F.) ;
#29773 = ORIENTED_EDGE('',*,*,#20208,.F.) ;
#29774 = ORIENTED_EDGE('',*,*,#20205,.F.) ;
#29775 = ORIENTED_EDGE('',*,*,#20202,.F.) ;
#29776 = ORIENTED_EDGE('',*,*,#20199,.F.) ;
#29777 = ORIENTED_EDGE('',*,*,#20196,.F.) ;
#29778 = ORIENTED_EDGE('',*,*,#20193,.F.) ;
#29779 = ORIENTED_EDGE('',*,*,#20190,.F.) ;
#29780 = ORIENTED_EDGE('',*,*,#20187,.F.) ;
#29781 = ORIENTED_EDGE('',*,*,#20184,.F.) ;
#29782 = ORIENTED_EDGE('',*,*,#20181,.F.) ;
#29783 = ORIENTED_EDGE('',*,*,#20178,.F.) ;
#29784 = ORIENTED_EDGE('',*,*,#20276,.F.) ;
#29785 = ORIENTED_EDGE('',*,*,#20222,.T.) ;
#29786 = ORIENTED_EDGE('',*,*,#20227,.T.) ;
#29787 = ORIENTED_EDGE('',*,*,#20230,.T.) ;
#29788 = ORIENTED_EDGE('',*,*,#20233,.T.) ;
#29789 = ORIENTED_EDGE('',*,*,#20236,.T.) ;
#29790 = ORIENTED_EDGE('',*,*,#20239,.T.) ;
#29791 = ORIENTED_EDGE('',*,*,#20242,.T.) ;
#29792 = ORIENTED_EDGE('',*,*,#20245,.T.) ;
#29793 = ORIENTED_EDGE('',*,*,#20248,.T.) ;
#29794 = ORIENTED_EDGE('',*,*,#20251,.T.) ;
#29795 = ORIENTED_EDGE('',*,*,#20254,.T.) ;
#29796 = ORIENTED_EDGE('',*,*,#20257,.T.) ;
#29797 = ORIENTED_EDGE('',*,*,#20260,.T.) ;
#29798 = ORIENTED_EDGE('',*,*,#20263,.T.) ;
#29799 = ORIENTED_EDGE('',*,*,#20266,.T.) ;
#29800 = ORIENTED_EDGE('',*,*,#20269,.T.) ;
#29801 = ORIENTED_EDGE('',*,*,#20280,.T.) ;
#29802 = ORIENTED_EDGE('',*,*,#20224,.T.) ;
#29803 = ORIENTED_EDGE('',*,*,#20273,.T.) ;
#29804 = ORIENTED_EDGE('',*,*,#20321,.T.) ;
#29805 = ORIENTED_EDGE('',*,*,#20274,.F.) ;
#29806 = ORIENTED_EDGE('',*,*,#20223,.F.) ;
#29807 = ORIENTED_EDGE('',*,*,#20275,.F.) ;
#29808 = ORIENTED_EDGE('',*,*,#20296,.T.) ;
#29809 = ORIENTED_EDGE('',*,*,#20322,.F.) ;
#29810 = ORIENTED_EDGE('',*,*,#20323,.F.) ;
#29811 = ORIENTED_EDGE('',*,*,#20324,.T.) ;
#29812 = ORIENTED_EDGE('',*,*,#20297,.T.) ;
#29813 = ORIENTED_EDGE('',*,*,#20324,.F.) ;
#29814 = ORIENTED_EDGE('',*,*,#20325,.F.) ;
#29815 = ORIENTED_EDGE('',*,*,#20326,.T.) ;
#29816 = ORIENTED_EDGE('',*,*,#20298,.T.) ;
#29817 = ORIENTED_EDGE('',*,*,#20326,.F.) ;
#29818 = ORIENTED_EDGE('',*,*,#20327,.F.) ;
#29819 = ORIENTED_EDGE('',*,*,#20328,.T.) ;
#29820 = ORIENTED_EDGE('',*,*,#20299,.T.) ;
#29821 = ORIENTED_EDGE('',*,*,#20328,.F.) ;
#29822 = ORIENTED_EDGE('',*,*,#20329,.F.) ;
#29823 = ORIENTED_EDGE('',*,*,#20330,.T.) ;
#29824 = ORIENTED_EDGE('',*,*,#20300,.T.) ;
#29825 = ORIENTED_EDGE('',*,*,#20330,.F.) ;
#29826 = ORIENTED_EDGE('',*,*,#20331,.F.) ;
#29827 = ORIENTED_EDGE('',*,*,#20291,.T.) ;
#29828 = ORIENTED_EDGE('',*,*,#20332,.T.) ;
#29829 = ORIENTED_EDGE('',*,*,#20288,.T.) ;
#29830 = ORIENTED_EDGE('',*,*,#20331,.T.) ;
#29831 = ORIENTED_EDGE('',*,*,#20329,.T.) ;
#29832 = ORIENTED_EDGE('',*,*,#20327,.T.) ;
#29833 = ORIENTED_EDGE('',*,*,#20325,.T.) ;
#29834 = ORIENTED_EDGE('',*,*,#20323,.T.) ;
#29835 = ORIENTED_EDGE('',*,*,#20333,.T.) ;
#29836 = ORIENTED_EDGE('',*,*,#20334,.T.) ;
#29837 = ORIENTED_EDGE('',*,*,#20335,.T.) ;
#29838 = ORIENTED_EDGE('',*,*,#20336,.T.) ;
#29839 = ORIENTED_EDGE('',*,*,#20337,.T.) ;
#29840 = ORIENTED_EDGE('',*,*,#20338,.T.) ;
#29841 = ORIENTED_EDGE('',*,*,#20339,.T.) ;
#29842 = ORIENTED_EDGE('',*,*,#20340,.T.) ;
#29843 = ORIENTED_EDGE('',*,*,#20341,.T.) ;
#29844 = ORIENTED_EDGE('',*,*,#20284,.T.) ;
#29845 = ORIENTED_EDGE('',*,*,#20342,.T.) ;
#29846 = ORIENTED_EDGE('',*,*,#20343,.T.) ;
#29847 = ORIENTED_EDGE('',*,*,#20344,.T.) ;
#29848 = ORIENTED_EDGE('',*,*,#20301,.T.) ;
#29849 = ORIENTED_EDGE('',*,*,#20289,.F.) ;
#29850 = ORIENTED_EDGE('',*,*,#20332,.F.) ;
#29851 = ORIENTED_EDGE('',*,*,#20345,.T.) ;
#29852 = ORIENTED_EDGE('',*,*,#20302,.T.) ;
#29853 = ORIENTED_EDGE('',*,*,#20345,.F.) ;
#29854 = ORIENTED_EDGE('',*,*,#20344,.F.) ;
#29855 = ORIENTED_EDGE('',*,*,#20346,.T.) ;
#29856 = ORIENTED_EDGE('',*,*,#20303,.T.) ;
#29857 = ORIENTED_EDGE('',*,*,#20346,.F.) ;
#29858 = ORIENTED_EDGE('',*,*,#20343,.F.) ;
#29859 = ORIENTED_EDGE('',*,*,#20347,.T.) ;
#29860 = ORIENTED_EDGE('',*,*,#20304,.T.) ;
#29861 = ORIENTED_EDGE('',*,*,#20347,.F.) ;
#29862 = ORIENTED_EDGE('',*,*,#20342,.F.) ;
#29863 = ORIENTED_EDGE('',*,*,#20287,.T.) ;
#29864 = ORIENTED_EDGE('',*,*,#20305,.T.) ;
#29865 = ORIENTED_EDGE('',*,*,#20285,.F.) ;
#29866 = ORIENTED_EDGE('',*,*,#20341,.F.) ;
#29867 = ORIENTED_EDGE('',*,*,#20348,.T.) ;
#29868 = ORIENTED_EDGE('',*,*,#20306,.T.) ;
#29869 = ORIENTED_EDGE('',*,*,#20348,.F.) ;
#29870 = ORIENTED_EDGE('',*,*,#20340,.F.) ;
#29871 = ORIENTED_EDGE('',*,*,#20349,.T.) ;
#29872 = ORIENTED_EDGE('',*,*,#20307,.T.) ;
#29873 = ORIENTED_EDGE('',*,*,#20349,.F.) ;
#29874 = ORIENTED_EDGE('',*,*,#20339,.F.) ;
#29875 = ORIENTED_EDGE('',*,*,#20350,.T.) ;
#29876 = ORIENTED_EDGE('',*,*,#20308,.T.) ;
#29877 = ORIENTED_EDGE('',*,*,#20350,.F.) ;
#29878 = ORIENTED_EDGE('',*,*,#20338,.F.) ;
#29879 = ORIENTED_EDGE('',*,*,#20351,.T.) ;
#29880 = ORIENTED_EDGE('',*,*,#20309,.T.) ;
#29881 = ORIENTED_EDGE('',*,*,#20351,.F.) ;
#29882 = ORIENTED_EDGE('',*,*,#20337,.F.) ;
#29883 = ORIENTED_EDGE('',*,*,#20352,.T.) ;
#29884 = ORIENTED_EDGE('',*,*,#20310,.T.) ;
#29885 = ORIENTED_EDGE('',*,*,#20352,.F.) ;
#29886 = ORIENTED_EDGE('',*,*,#20336,.F.) ;
#29887 = ORIENTED_EDGE('',*,*,#20353,.T.) ;
#29888 = ORIENTED_EDGE('',*,*,#20311,.T.) ;
#29889 = ORIENTED_EDGE('',*,*,#20353,.F.) ;
#29890 = ORIENTED_EDGE('',*,*,#20335,.F.) ;
#29891 = ORIENTED_EDGE('',*,*,#20354,.T.) ;
#29892 = ORIENTED_EDGE('',*,*,#20312,.T.) ;
#29893 = ORIENTED_EDGE('',*,*,#20354,.F.) ;
#29894 = ORIENTED_EDGE('',*,*,#20334,.F.) ;
#29895 = ORIENTED_EDGE('',*,*,#20355,.T.) ;
#29896 = ORIENTED_EDGE('',*,*,#20313,.T.) ;
#29897 = ORIENTED_EDGE('',*,*,#20355,.F.) ;
#29898 = ORIENTED_EDGE('',*,*,#20333,.F.) ;
#29899 = ORIENTED_EDGE('',*,*,#20322,.T.) ;
#29900 = ORIENTED_EDGE('',*,*,#20356,.T.) ;
#29901 = ORIENTED_EDGE('',*,*,#20357,.T.) ;
#29902 = ORIENTED_EDGE('',*,*,#20358,.T.) ;
#29903 = ORIENTED_EDGE('',*,*,#20359,.T.) ;
#29904 = ORIENTED_EDGE('',*,*,#20360,.T.) ;
#29905 = ORIENTED_EDGE('',*,*,#20361,.T.) ;
#29906 = ORIENTED_EDGE('',*,*,#20362,.T.) ;
#29907 = ORIENTED_EDGE('',*,*,#20363,.T.) ;
#29908 = ORIENTED_EDGE('',*,*,#20356,.F.) ;
#29909 = ORIENTED_EDGE('',*,*,#20364,.T.) ;
#29910 = ORIENTED_EDGE('',*,*,#20360,.F.) ;
#29911 = ORIENTED_EDGE('',*,*,#20365,.F.) ;
#29912 = ORIENTED_EDGE('',*,*,#20359,.F.) ;
#29913 = ORIENTED_EDGE('',*,*,#20366,.T.) ;
#29914 = ORIENTED_EDGE('',*,*,#20361,.F.) ;
#29915 = ORIENTED_EDGE('',*,*,#20364,.F.) ;
#29916 = ORIENTED_EDGE('',*,*,#20358,.F.) ;
#29917 = ORIENTED_EDGE('',*,*,#20367,.T.) ;
#29918 = ORIENTED_EDGE('',*,*,#20362,.F.) ;
#29919 = ORIENTED_EDGE('',*,*,#20366,.F.) ;
#29920 = ORIENTED_EDGE('',*,*,#20357,.F.) ;
#29921 = ORIENTED_EDGE('',*,*,#20365,.T.) ;
#29922 = ORIENTED_EDGE('',*,*,#20363,.F.) ;
#29923 = ORIENTED_EDGE('',*,*,#20367,.F.) ;
#29924 = ORIENTED_EDGE('',*,*,#20368,.T.) ;
#29925 = ORIENTED_EDGE('',*,*,#20369,.T.) ;
#29926 = ORIENTED_EDGE('',*,*,#20370,.T.) ;
#29927 = ORIENTED_EDGE('',*,*,#20371,.T.) ;
#29928 = ORIENTED_EDGE('',*,*,#20369,.F.) ;
#29929 = ORIENTED_EDGE('',*,*,#20372,.F.) ;
#29930 = ORIENTED_EDGE('',*,*,#20373,.F.) ;
#29931 = ORIENTED_EDGE('',*,*,#20374,.T.) ;
#29932 = ORIENTED_EDGE('',*,*,#20370,.F.) ;
#29933 = ORIENTED_EDGE('',*,*,#20371,.F.) ;
#29934 = ORIENTED_EDGE('',*,*,#20374,.F.) ;
#29935 = ORIENTED_EDGE('',*,*,#20368,.F.) ;
#29936 = ORIENTED_EDGE('',*,*,#20375,.F.) ;
#29937 = ORIENTED_EDGE('',*,*,#20372,.T.) ;
#29938 = ORIENTED_EDGE('',*,*,#20373,.T.) ;
#29939 = ORIENTED_EDGE('',*,*,#20376,.T.) ;
#29940 = ORIENTED_EDGE('',*,*,#20377,.T.) ;
#29941 = ORIENTED_EDGE('',*,*,#20376,.F.) ;
#29942 = ORIENTED_EDGE('',*,*,#20377,.F.) ;
#29943 = ORIENTED_EDGE('',*,*,#20378,.T.) ;
#29944 = ORIENTED_EDGE('',*,*,#20375,.T.) ;
#29945 = ORIENTED_EDGE('',*,*,#20379,.T.) ;
#29946 = ORIENTED_EDGE('',*,*,#20378,.F.) ;
#29947 = ORIENTED_EDGE('',*,*,#20379,.F.) ;
#29948 = CYLINDRICAL_SURFACE('',#32774,0.25) ;
#29949 = CYLINDRICAL_SURFACE('',#32826,0.25) ;
#29950 = CYLINDRICAL_SURFACE('',#32829,0.25) ;
#29951 = CYLINDRICAL_SURFACE('',#32843,0.75) ;
#29952 = CYLINDRICAL_SURFACE('',#32858,0.75) ;
#29953 = CYLINDRICAL_SURFACE('',#32873,1.) ;
#29954 = CYLINDRICAL_SURFACE('',#32876,1.) ;
#29955 = CYLINDRICAL_SURFACE('',#32878,0.75) ;
#29956 = CYLINDRICAL_SURFACE('',#32944,2.4999999999) ;
#29957 = CYLINDRICAL_SURFACE('',#32945,28.5) ;
#29958 = CYLINDRICAL_SURFACE('',#32946,2.4999999999) ;
#29959 = CYLINDRICAL_SURFACE('',#32947,28.5) ;
#29960 = CYLINDRICAL_SURFACE('',#32948,2.4999999999) ;
#29961 = CYLINDRICAL_SURFACE('',#32949,28.5) ;
#29962 = CYLINDRICAL_SURFACE('',#32950,2.4999999999) ;
#29963 = CYLINDRICAL_SURFACE('',#32951,28.5) ;
#29964 = CYLINDRICAL_SURFACE('',#32952,2.4999999999) ;
#29965 = CYLINDRICAL_SURFACE('',#32953,2.4999999999) ;
#29966 = CYLINDRICAL_SURFACE('',#32954,0.5) ;
#29967 = CYLINDRICAL_SURFACE('',#32957,0.5) ;
#29968 = CYLINDRICAL_SURFACE('',#32960,0.5) ;
#29969 = CYLINDRICAL_SURFACE('',#32961,0.5) ;
#29970 = CYLINDRICAL_SURFACE('',#32967,0.5) ;
#29971 = CYLINDRICAL_SURFACE('',#32972,0.5) ;
#29972 = CYLINDRICAL_SURFACE('',#32974,1.) ;
#29973 = CYLINDRICAL_SURFACE('',#32976,1.) ;
#29974 = CYLINDRICAL_SURFACE('',#32978,1.) ;
#29975 = CYLINDRICAL_SURFACE('',#32979,1.) ;
#29976 = CYLINDRICAL_SURFACE('',#32981,1.) ;
#29977 = CYLINDRICAL_SURFACE('',#32983,1.) ;
#29978 = CYLINDRICAL_SURFACE('',#32984,1.) ;
#29979 = CYLINDRICAL_SURFACE('',#32986,1.) ;
#29980 = CYLINDRICAL_SURFACE('',#32988,1.) ;
#29981 = CYLINDRICAL_SURFACE('',#32989,1.) ;
#29982 = CYLINDRICAL_SURFACE('',#32991,1.) ;
#29983 = CYLINDRICAL_SURFACE('',#32993,1.) ;
#29984 = CYLINDRICAL_SURFACE('',#32995,0.25) ;
#29985 = CYLINDRICAL_SURFACE('',#33001,1.25) ;
#29986 = CYLINDRICAL_SURFACE('',#33002,1.25) ;
#29987 = CYLINDRICAL_SURFACE('',#33004,1.25) ;
#29988 = CYLINDRICAL_SURFACE('',#33005,3.) ;
#29989 = CYLINDRICAL_SURFACE('',#33006,3.) ;
#29990 = CYLINDRICAL_SURFACE('',#33007,15.5) ;
#29991 = CYLINDRICAL_SURFACE('',#33008,21.5) ;
#29992 = CYLINDRICAL_SURFACE('',#33009,23.5) ;
#29993 = CYLINDRICAL_SURFACE('',#33014,2.) ;
#29994 = CYLINDRICAL_SURFACE('',#33015,2.) ;
#29995 = CYLINDRICAL_SURFACE('',#33016,2.) ;
#29996 = CYLINDRICAL_SURFACE('',#33017,2.) ;
#29997 = CYLINDRICAL_SURFACE('',#33018,1.5) ;
#29998 = CYLINDRICAL_SURFACE('',#33020,1.5) ;
#29999 = CYLINDRICAL_SURFACE('',#33022,1.5) ;
#30000 = CYLINDRICAL_SURFACE('',#33024,1.5) ;
#30001 = CYLINDRICAL_SURFACE('',#33026,1.5) ;
#30002 = CYLINDRICAL_SURFACE('',#33028,1.5) ;
#30003 = CYLINDRICAL_SURFACE('',#33030,1.5) ;
#30004 = CYLINDRICAL_SURFACE('',#33032,1.5) ;
#30005 = CYLINDRICAL_SURFACE('',#33034,1.5) ;
#30006 = CYLINDRICAL_SURFACE('',#33036,1.5) ;
#30007 = CYLINDRICAL_SURFACE('',#33038,1.5) ;
#30008 = CYLINDRICAL_SURFACE('',#33040,1.5) ;
#30009 = CYLINDRICAL_SURFACE('',#33042,0.75) ;
#30010 = CYLINDRICAL_SURFACE('',#33044,1.25) ;
#30011 = CYLINDRICAL_SURFACE('',#33045,23.5) ;
#30012 = CYLINDRICAL_SURFACE('',#33046,23.5) ;
#30013 = CYLINDRICAL_SURFACE('',#33047,23.5) ;
#30014 = CYLINDRICAL_SURFACE('',#33048,3.) ;
#30015 = CYLINDRICAL_SURFACE('',#33049,3.) ;
#30016 = CYLINDRICAL_SURFACE('',#33050,15.5) ;
#30017 = CYLINDRICAL_SURFACE('',#33051,21.5) ;
#30018 = CYLINDRICAL_SURFACE('',#33052,3.) ;
#30019 = CYLINDRICAL_SURFACE('',#33053,3.) ;
#30020 = CYLINDRICAL_SURFACE('',#33054,15.5) ;
#30021 = CYLINDRICAL_SURFACE('',#33055,21.5) ;
#30022 = CYLINDRICAL_SURFACE('',#33056,3.) ;
#30023 = CYLINDRICAL_SURFACE('',#33057,3.) ;
#30024 = CYLINDRICAL_SURFACE('',#33058,15.5) ;
#30025 = CYLINDRICAL_SURFACE('',#33059,21.5) ;
#30026 = CYLINDRICAL_SURFACE('',#33063,1.17524047358083) ;
#30027 = CYLINDRICAL_SURFACE('',#33065,1.17524047358083) ;
#30028 = CYLINDRICAL_SURFACE('',#33066,1.17524047358083) ;
#30029 = CYLINDRICAL_SURFACE('',#33067,1.17524047358083) ;
#30030 = CYLINDRICAL_SURFACE('',#33068,1.17524047358083) ;
#30031 = CYLINDRICAL_SURFACE('',#33070,1.5) ;
#30032 = CYLINDRICAL_SURFACE('',#33072,1.5) ;
#30033 = CYLINDRICAL_SURFACE('',#33073,1.5) ;
#30034 = CYLINDRICAL_SURFACE('',#33074,1.5) ;
#30035 = CYLINDRICAL_SURFACE('',#33075,1.5) ;
#30036 = CYLINDRICAL_SURFACE('',#33076,1.5) ;
#30037 = CYLINDRICAL_SURFACE('',#33084,1.5) ;
#30038 = CYLINDRICAL_SURFACE('',#33085,1.17524047358083) ;
#30039 = CYLINDRICAL_SURFACE('',#33125,1.00995540144767) ;
#30040 = CYLINDRICAL_SURFACE('',#33127,1.00995540144767) ;
#30041 = CYLINDRICAL_SURFACE('',#33129,1.00995540144767) ;
#30042 = CYLINDRICAL_SURFACE('',#33130,1.00995540144767) ;
#30043 = CYLINDRICAL_SURFACE('',#33131,1.00995540144767) ;
#30044 = CYLINDRICAL_SURFACE('',#33132,1.00995540144767) ;
#30045 = CYLINDRICAL_SURFACE('',#33133,1.4224) ;
#30046 = CYLINDRICAL_SURFACE('',#33138,1.4224) ;
#30047 = CYLINDRICAL_SURFACE('',#33139,1.4224) ;
#30048 = CYLINDRICAL_SURFACE('',#33140,1.4224) ;
#30049 = CYLINDRICAL_SURFACE('',#33141,1.4224) ;
#30050 = CYLINDRICAL_SURFACE('',#33142,1.4224) ;
#30051 = CYLINDRICAL_SURFACE('',#33144,1.00995540144767) ;
#30052 = CYLINDRICAL_SURFACE('',#33165,1.7907) ;
#30053 = CYLINDRICAL_SURFACE('',#33168,1.7907) ;
#30054 = CYLINDRICAL_SURFACE('',#33171,1.7907) ;
#30055 = CYLINDRICAL_SURFACE('',#33186,1.7907) ;
#30056 = CYLINDRICAL_SURFACE('',#33201,2.05475) ;
#30057 = CYLINDRICAL_SURFACE('',#33203,2.05475) ;
#30058 = CYLINDRICAL_SURFACE('',#33204,2.05475) ;
#30059 = CYLINDRICAL_SURFACE('',#33206,2.05475000000001) ;
#30060 = CYLINDRICAL_SURFACE('',#33208,2.05475000000001) ;
#30061 = CYLINDRICAL_SURFACE('',#33209,2.05475000000001) ;
#30062 = CYLINDRICAL_SURFACE('',#33211,2.05475000000001) ;
#30063 = CYLINDRICAL_SURFACE('',#33213,2.05475000000001) ;
#30064 = CYLINDRICAL_SURFACE('',#33214,2.05475000000001) ;
#30065 = CYLINDRICAL_SURFACE('',#33216,2.05474999999993) ;
#30066 = CYLINDRICAL_SURFACE('',#33218,2.05474999999993) ;
#30067 = CYLINDRICAL_SURFACE('',#33219,2.05474999999993) ;
#30068 = CYLINDRICAL_SURFACE('',#33221,1.66599999999999) ;
#30069 = CYLINDRICAL_SURFACE('',#33223,1.66599999999999) ;
#30070 = CYLINDRICAL_SURFACE('',#33225,1.66599999999999) ;
#30071 = CYLINDRICAL_SURFACE('',#33227,1.66599999999999) ;
#30072 = CYLINDRICAL_SURFACE('',#33229,1.66599999999999) ;
#30073 = CYLINDRICAL_SURFACE('',#33231,1.66599999999999) ;
#30074 = CYLINDRICAL_SURFACE('',#33233,1.66599999999999) ;
#30075 = CYLINDRICAL_SURFACE('',#33235,1.66599999999999) ;
#30076 = CYLINDRICAL_SURFACE('',#33237,1.66599999999999) ;
#30077 = CYLINDRICAL_SURFACE('',#33239,1.66599999999998) ;
#30078 = CYLINDRICAL_SURFACE('',#33241,1.66599999999998) ;
#30079 = CYLINDRICAL_SURFACE('',#33243,1.66599999999998) ;
#30080 = CYLINDRICAL_SURFACE('',#33245,2.05475) ;
#30081 = CYLINDRICAL_SURFACE('',#33247,2.05475) ;
#30082 = CYLINDRICAL_SURFACE('',#33248,2.05475) ;
#30083 = CYLINDRICAL_SURFACE('',#33250,2.05475) ;
#30084 = CYLINDRICAL_SURFACE('',#33252,2.05475) ;
#30085 = CYLINDRICAL_SURFACE('',#33253,2.05475) ;
#30086 = CYLINDRICAL_SURFACE('',#33255,1.666) ;
#30087 = CYLINDRICAL_SURFACE('',#33257,1.666) ;
#30088 = CYLINDRICAL_SURFACE('',#33259,1.666) ;
#30089 = CYLINDRICAL_SURFACE('',#33261,1.666) ;
#30090 = CYLINDRICAL_SURFACE('',#33263,1.666) ;
#30091 = CYLINDRICAL_SURFACE('',#33265,1.666) ;
#30092 = CYLINDRICAL_SURFACE('',#33267,2.05475) ;
#30093 = CYLINDRICAL_SURFACE('',#33269,2.05475) ;
#30094 = CYLINDRICAL_SURFACE('',#33270,2.05475) ;
#30095 = CYLINDRICAL_SURFACE('',#33272,2.05475) ;
#30096 = CYLINDRICAL_SURFACE('',#33274,2.05475) ;
#30097 = CYLINDRICAL_SURFACE('',#33275,2.05475) ;
#30098 = CYLINDRICAL_SURFACE('',#33277,1.66600000000001) ;
#30099 = CYLINDRICAL_SURFACE('',#33279,1.66600000000001) ;
#30100 = CYLINDRICAL_SURFACE('',#33281,1.66600000000001) ;
#30101 = CYLINDRICAL_SURFACE('',#33283,1.66600000000001) ;
#30102 = CYLINDRICAL_SURFACE('',#33285,1.66600000000001) ;
#30103 = CYLINDRICAL_SURFACE('',#33287,1.66600000000001) ;
#30104 = CYLINDRICAL_SURFACE('',#33289,1.66600000000001) ;
#30105 = CYLINDRICAL_SURFACE('',#33290,1.66600000000001) ;
#30106 = CYLINDRICAL_SURFACE('',#33291,2.05475) ;
#30107 = CYLINDRICAL_SURFACE('',#33292,2.05475) ;
#30108 = CYLINDRICAL_SURFACE('',#33293,1.666) ;
#30109 = CYLINDRICAL_SURFACE('',#33294,1.666) ;
#30110 = CYLINDRICAL_SURFACE('',#33295,2.05475) ;
#30111 = CYLINDRICAL_SURFACE('',#33296,2.05475) ;
#30112 = CYLINDRICAL_SURFACE('',#33297,1.66599999999998) ;
#30113 = CYLINDRICAL_SURFACE('',#33298,1.66599999999999) ;
#30114 = CYLINDRICAL_SURFACE('',#33299,1.66599999999999) ;
#30115 = CYLINDRICAL_SURFACE('',#33300,1.66599999999999) ;
#30116 = CYLINDRICAL_SURFACE('',#33301,2.05474999999993) ;
#30117 = CYLINDRICAL_SURFACE('',#33302,2.05475000000001) ;
#30118 = CYLINDRICAL_SURFACE('',#33303,2.05475000000001) ;
#30119 = CYLINDRICAL_SURFACE('',#33304,2.05475) ;
#30120 = CYLINDRICAL_SURFACE('',#33305,0.5) ;
#30121 = CYLINDRICAL_SURFACE('',#33308,2.) ;
#30122 = CYLINDRICAL_SURFACE('',#33311,2.) ;
#30123 = CYLINDRICAL_SURFACE('',#33314,2.) ;
#30124 = CYLINDRICAL_SURFACE('',#33317,2.) ;
#30125 = CYLINDRICAL_SURFACE('',#33324,2.) ;
#30126 = CYLINDRICAL_SURFACE('',#33327,1.) ;
#30127 = CYLINDRICAL_SURFACE('',#33337,0.5) ;
#30128 = CYLINDRICAL_SURFACE('',#33376,2.) ;
#30129 = CYLINDRICAL_SURFACE('',#33378,2.) ;
#30130 = CYLINDRICAL_SURFACE('',#33380,2.) ;
#30131 = CYLINDRICAL_SURFACE('',#33382,0.5) ;
#30132 = CYLINDRICAL_SURFACE('',#33396,1.) ;
#30133 = CYLINDRICAL_SURFACE('',#33400,1.) ;
#30134 = CYLINDRICAL_SURFACE('',#33406,1.) ;
#30135 = CYLINDRICAL_SURFACE('',#33411,1.) ;
#30136 = CYLINDRICAL_SURFACE('',#33414,4.) ;
#30137 = CYLINDRICAL_SURFACE('',#33417,4.) ;
#30138 = CYLINDRICAL_SURFACE('',#33420,1.) ;
#30139 = CYLINDRICAL_SURFACE('',#33426,1.) ;
#30140 = CYLINDRICAL_SURFACE('',#33431,1.) ;
#30141 = CYLINDRICAL_SURFACE('',#33434,4.) ;
#30142 = CYLINDRICAL_SURFACE('',#33437,4.) ;
#30143 = CYLINDRICAL_SURFACE('',#33454,0.5) ;
#30144 = CYLINDRICAL_SURFACE('',#33457,0.5) ;
#30145 = CYLINDRICAL_SURFACE('',#33460,0.5) ;
#30146 = CYLINDRICAL_SURFACE('',#33462,0.5) ;
#30147 = CYLINDRICAL_SURFACE('',#33465,0.5) ;
#30148 = CYLINDRICAL_SURFACE('',#33471,1.65) ;
#30149 = CYLINDRICAL_SURFACE('',#33474,1.65) ;
#30150 = CYLINDRICAL_SURFACE('',#33477,1.65) ;
#30151 = CYLINDRICAL_SURFACE('',#33482,1.75) ;
#30152 = CYLINDRICAL_SURFACE('',#33488,2.) ;
#30153 = CYLINDRICAL_SURFACE('',#33491,2.) ;
#30154 = CYLINDRICAL_SURFACE('',#33494,2.) ;
#30155 = CYLINDRICAL_SURFACE('',#33497,2.) ;
#30156 = CYLINDRICAL_SURFACE('',#33500,2.) ;
#30157 = CYLINDRICAL_SURFACE('',#33503,2.) ;
#30158 = CYLINDRICAL_SURFACE('',#33510,3.25) ;
#30159 = CYLINDRICAL_SURFACE('',#33512,2.) ;
#30160 = CYLINDRICAL_SURFACE('',#33513,2.) ;
#30161 = CYLINDRICAL_SURFACE('',#33514,2.) ;
#30162 = CYLINDRICAL_SURFACE('',#33516,2.) ;
#30163 = CYLINDRICAL_SURFACE('',#33539,2.) ;
#30164 = CYLINDRICAL_SURFACE('',#33541,2.) ;
#30165 = CYLINDRICAL_SURFACE('',#33545,2.) ;
#30166 = CYLINDRICAL_SURFACE('',#33547,3.25) ;
#30167 = CYLINDRICAL_SURFACE('',#33552,3.25) ;
#30168 = CYLINDRICAL_SURFACE('',#33567,1.75) ;
#30169 = CYLINDRICAL_SURFACE('',#33572,1.75) ;
#30170 = CYLINDRICAL_SURFACE('',#33577,1.75) ;
#30171 = CYLINDRICAL_SURFACE('',#33582,1.75) ;
#30172 = CYLINDRICAL_SURFACE('',#33600,2.) ;
#30173 = CYLINDRICAL_SURFACE('',#33601,2.) ;
#30174 = CYLINDRICAL_SURFACE('',#33617,3.25) ;
#30175 = CYLINDRICAL_SURFACE('',#33621,2.) ;
#30176 = CYLINDRICAL_SURFACE('',#33624,2.) ;
#30177 = CYLINDRICAL_SURFACE('',#33627,3.25) ;
#30178 = CYLINDRICAL_SURFACE('',#33630,3.25) ;
#30179 = CYLINDRICAL_SURFACE('',#33632,1.65) ;
#30180 = CYLINDRICAL_SURFACE('',#33640,0.125) ;
#30181 = CYLINDRICAL_SURFACE('',#33642,0.125) ;
#30182 = CYLINDRICAL_SURFACE('',#33644,0.125) ;
#30183 = CYLINDRICAL_SURFACE('',#33647,0.125) ;
#30184 = CYLINDRICAL_SURFACE('',#33649,0.125) ;
#30185 = CYLINDRICAL_SURFACE('',#33652,0.125) ;
#30186 = CYLINDRICAL_SURFACE('',#33654,0.125) ;
#30187 = CYLINDRICAL_SURFACE('',#33658,0.125) ;
#30188 = CYLINDRICAL_SURFACE('',#33669,2.) ;
#30189 = CYLINDRICAL_SURFACE('',#33673,2.) ;
#30190 = CYLINDRICAL_SURFACE('',#33674,2.) ;
#30191 = CYLINDRICAL_SURFACE('',#33676,2.) ;
#30192 = CYLINDRICAL_SURFACE('',#33682,2.) ;
#30193 = CYLINDRICAL_SURFACE('',#33687,2.) ;
#30194 = CYLINDRICAL_SURFACE('',#33690,2.) ;
#30195 = CYLINDRICAL_SURFACE('',#33760,1.5) ;
#30196 = CYLINDRICAL_SURFACE('',#33771,1.5) ;
#30197 = CYLINDRICAL_SURFACE('',#33782,1.5) ;
#30198 = CYLINDRICAL_SURFACE('',#33793,1.5) ;
#30199 = CYLINDRICAL_SURFACE('',#33804,1.5) ;
#30200 = CYLINDRICAL_SURFACE('',#33815,1.5) ;
#30201 = CYLINDRICAL_SURFACE('',#33826,1.5) ;
#30202 = CYLINDRICAL_SURFACE('',#33837,1.5) ;
#30203 = CYLINDRICAL_SURFACE('',#33853,1.5) ;
#30204 = CYLINDRICAL_SURFACE('',#33871,0.25) ;
#30205 = CYLINDRICAL_SURFACE('',#33877,0.25) ;
#30206 = CYLINDRICAL_SURFACE('',#33882,0.25) ;
#30207 = CYLINDRICAL_SURFACE('',#33887,0.25) ;
#30208 = CYLINDRICAL_SURFACE('',#33891,0.125) ;
#30209 = CYLINDRICAL_SURFACE('',#33896,0.125) ;
#30210 = CYLINDRICAL_SURFACE('',#33899,0.25) ;
#30211 = CYLINDRICAL_SURFACE('',#33905,0.25) ;
#30212 = CYLINDRICAL_SURFACE('',#33910,0.25) ;
#30213 = CYLINDRICAL_SURFACE('',#33915,0.25) ;
#30214 = CYLINDRICAL_SURFACE('',#33919,0.125) ;
#30215 = CYLINDRICAL_SURFACE('',#33924,0.125) ;
#30216 = CYLINDRICAL_SURFACE('',#33927,0.25) ;
#30217 = CYLINDRICAL_SURFACE('',#33933,0.25) ;
#30218 = CYLINDRICAL_SURFACE('',#33938,0.25) ;
#30219 = CYLINDRICAL_SURFACE('',#33943,0.25) ;
#30220 = CYLINDRICAL_SURFACE('',#33947,0.125) ;
#30221 = CYLINDRICAL_SURFACE('',#33952,0.125) ;
#30222 = CYLINDRICAL_SURFACE('',#33955,0.25) ;
#30223 = CYLINDRICAL_SURFACE('',#33961,0.25) ;
#30224 = CYLINDRICAL_SURFACE('',#33966,0.25) ;
#30225 = CYLINDRICAL_SURFACE('',#33971,0.25) ;
#30226 = CYLINDRICAL_SURFACE('',#33975,0.125) ;
#30227 = CYLINDRICAL_SURFACE('',#33980,0.125) ;
#30228 = CYLINDRICAL_SURFACE('',#33983,0.25) ;
#30229 = CYLINDRICAL_SURFACE('',#33989,0.25) ;
#30230 = CYLINDRICAL_SURFACE('',#33994,0.25) ;
#30231 = CYLINDRICAL_SURFACE('',#33999,0.25) ;
#30232 = CYLINDRICAL_SURFACE('',#34003,0.125) ;
#30233 = CYLINDRICAL_SURFACE('',#34008,0.125) ;
#30234 = CYLINDRICAL_SURFACE('',#34011,0.25) ;
#30235 = CYLINDRICAL_SURFACE('',#34017,0.25) ;
#30236 = CYLINDRICAL_SURFACE('',#34022,0.25) ;
#30237 = CYLINDRICAL_SURFACE('',#34027,0.25) ;
#30238 = CYLINDRICAL_SURFACE('',#34031,0.125) ;
#30239 = CYLINDRICAL_SURFACE('',#34036,0.125) ;
#30240 = CYLINDRICAL_SURFACE('',#34039,0.25) ;
#30241 = CYLINDRICAL_SURFACE('',#34045,0.25) ;
#30242 = CYLINDRICAL_SURFACE('',#34050,0.25) ;
#30243 = CYLINDRICAL_SURFACE('',#34055,0.25) ;
#30244 = CYLINDRICAL_SURFACE('',#34059,0.125) ;
#30245 = CYLINDRICAL_SURFACE('',#34064,0.125) ;
#30246 = CYLINDRICAL_SURFACE('',#34067,0.25) ;
#30247 = CYLINDRICAL_SURFACE('',#34073,0.25) ;
#30248 = CYLINDRICAL_SURFACE('',#34078,0.25) ;
#30249 = CYLINDRICAL_SURFACE('',#34083,0.25) ;
#30250 = CYLINDRICAL_SURFACE('',#34087,0.125) ;
#30251 = CYLINDRICAL_SURFACE('',#34092,0.125) ;
#30252 = CYLINDRICAL_SURFACE('',#34095,0.25) ;
#30253 = CYLINDRICAL_SURFACE('',#34101,0.25) ;
#30254 = CYLINDRICAL_SURFACE('',#34106,0.25) ;
#30255 = CYLINDRICAL_SURFACE('',#34111,0.25) ;
#30256 = CYLINDRICAL_SURFACE('',#34115,0.125) ;
#30257 = CYLINDRICAL_SURFACE('',#34120,0.125) ;
#30258 = CYLINDRICAL_SURFACE('',#34123,0.25) ;
#30259 = CYLINDRICAL_SURFACE('',#34130,0.25) ;
#30260 = CYLINDRICAL_SURFACE('',#34136,0.25) ;
#30261 = CYLINDRICAL_SURFACE('',#34142,0.25) ;
#30262 = CYLINDRICAL_SURFACE('',#34147,0.125) ;
#30263 = CYLINDRICAL_SURFACE('',#34150,0.125) ;
#30264 = CYLINDRICAL_SURFACE('',#34153,0.25) ;
#30265 = CYLINDRICAL_SURFACE('',#34160,0.25) ;
#30266 = CYLINDRICAL_SURFACE('',#34166,0.25) ;
#30267 = CYLINDRICAL_SURFACE('',#34172,0.25) ;
#30268 = CYLINDRICAL_SURFACE('',#34177,0.125) ;
#30269 = CYLINDRICAL_SURFACE('',#34180,0.125) ;
#30270 = CYLINDRICAL_SURFACE('',#34183,0.25) ;
#30271 = CYLINDRICAL_SURFACE('',#34190,0.25) ;
#30272 = CYLINDRICAL_SURFACE('',#34196,0.25) ;
#30273 = CYLINDRICAL_SURFACE('',#34202,0.25) ;
#30274 = CYLINDRICAL_SURFACE('',#34207,0.125) ;
#30275 = CYLINDRICAL_SURFACE('',#34210,0.125) ;
#30276 = CYLINDRICAL_SURFACE('',#34213,0.25) ;
#30277 = CYLINDRICAL_SURFACE('',#34220,0.25) ;
#30278 = CYLINDRICAL_SURFACE('',#34226,0.25) ;
#30279 = CYLINDRICAL_SURFACE('',#34232,0.25) ;
#30280 = CYLINDRICAL_SURFACE('',#34237,0.125) ;
#30281 = CYLINDRICAL_SURFACE('',#34240,0.125) ;
#30282 = CYLINDRICAL_SURFACE('',#34243,0.25) ;
#30283 = CYLINDRICAL_SURFACE('',#34250,0.25) ;
#30284 = CYLINDRICAL_SURFACE('',#34256,0.25) ;
#30285 = CYLINDRICAL_SURFACE('',#34262,0.25) ;
#30286 = CYLINDRICAL_SURFACE('',#34267,0.125) ;
#30287 = CYLINDRICAL_SURFACE('',#34270,0.125) ;
#30288 = CYLINDRICAL_SURFACE('',#34273,0.25) ;
#30289 = CYLINDRICAL_SURFACE('',#34280,0.25) ;
#30290 = CYLINDRICAL_SURFACE('',#34286,0.25) ;
#30291 = CYLINDRICAL_SURFACE('',#34292,0.25) ;
#30292 = CYLINDRICAL_SURFACE('',#34297,0.125) ;
#30293 = CYLINDRICAL_SURFACE('',#34300,0.125) ;
#30294 = CYLINDRICAL_SURFACE('',#34303,0.25) ;
#30295 = CYLINDRICAL_SURFACE('',#34310,0.25) ;
#30296 = CYLINDRICAL_SURFACE('',#34316,0.25) ;
#30297 = CYLINDRICAL_SURFACE('',#34322,0.25) ;
#30298 = CYLINDRICAL_SURFACE('',#34327,0.125) ;
#30299 = CYLINDRICAL_SURFACE('',#34330,0.125) ;
#30300 = CYLINDRICAL_SURFACE('',#34333,0.25) ;
#30301 = CYLINDRICAL_SURFACE('',#34340,0.25) ;
#30302 = CYLINDRICAL_SURFACE('',#34346,0.25) ;
#30303 = CYLINDRICAL_SURFACE('',#34352,0.25) ;
#30304 = CYLINDRICAL_SURFACE('',#34357,0.125) ;
#30305 = CYLINDRICAL_SURFACE('',#34360,0.125) ;
#30306 = CYLINDRICAL_SURFACE('',#34363,0.25) ;
#30307 = CYLINDRICAL_SURFACE('',#34370,0.25) ;
#30308 = CYLINDRICAL_SURFACE('',#34376,0.25) ;
#30309 = CYLINDRICAL_SURFACE('',#34382,0.25) ;
#30310 = CYLINDRICAL_SURFACE('',#34387,0.125) ;
#30311 = CYLINDRICAL_SURFACE('',#34392,0.125) ;
#30312 = CYLINDRICAL_SURFACE('',#34395,0.25) ;
#30313 = CYLINDRICAL_SURFACE('',#34402,0.25) ;
#30314 = CYLINDRICAL_SURFACE('',#34408,0.25) ;
#30315 = CYLINDRICAL_SURFACE('',#34414,0.25) ;
#30316 = CYLINDRICAL_SURFACE('',#34419,0.125) ;
#30317 = CYLINDRICAL_SURFACE('',#34424,0.125) ;
#30318 = CYLINDRICAL_SURFACE('',#34427,0.25) ;
#30319 = CYLINDRICAL_SURFACE('',#34434,0.25) ;
#30320 = CYLINDRICAL_SURFACE('',#34440,0.25) ;
#30321 = CYLINDRICAL_SURFACE('',#34446,0.25) ;
#30322 = CYLINDRICAL_SURFACE('',#34451,0.125) ;
#30323 = CYLINDRICAL_SURFACE('',#34456,0.125) ;
#30324 = CYLINDRICAL_SURFACE('',#34459,0.25) ;
#30325 = CYLINDRICAL_SURFACE('',#34466,0.25) ;
#30326 = CYLINDRICAL_SURFACE('',#34472,0.25) ;
#30327 = CYLINDRICAL_SURFACE('',#34478,0.25) ;
#30328 = CYLINDRICAL_SURFACE('',#34483,0.125) ;
#30329 = CYLINDRICAL_SURFACE('',#34488,0.125) ;
#30330 = CYLINDRICAL_SURFACE('',#34491,0.25) ;
#30331 = CYLINDRICAL_SURFACE('',#34498,0.25) ;
#30332 = CYLINDRICAL_SURFACE('',#34504,0.25) ;
#30333 = CYLINDRICAL_SURFACE('',#34510,0.25) ;
#30334 = CYLINDRICAL_SURFACE('',#34515,0.125) ;
#30335 = CYLINDRICAL_SURFACE('',#34520,0.125) ;
#30336 = CYLINDRICAL_SURFACE('',#34523,0.25) ;
#30337 = CYLINDRICAL_SURFACE('',#34530,0.25) ;
#30338 = CYLINDRICAL_SURFACE('',#34536,0.25) ;
#30339 = CYLINDRICAL_SURFACE('',#34542,0.25) ;
#30340 = CYLINDRICAL_SURFACE('',#34547,0.125) ;
#30341 = CYLINDRICAL_SURFACE('',#34552,0.125) ;
#30342 = CYLINDRICAL_SURFACE('',#34555,0.25) ;
#30343 = CYLINDRICAL_SURFACE('',#34562,0.25) ;
#30344 = CYLINDRICAL_SURFACE('',#34568,0.25) ;
#30345 = CYLINDRICAL_SURFACE('',#34574,0.25) ;
#30346 = CYLINDRICAL_SURFACE('',#34579,0.125) ;
#30347 = CYLINDRICAL_SURFACE('',#34584,0.125) ;
#30348 = CYLINDRICAL_SURFACE('',#34587,0.25) ;
#30349 = CYLINDRICAL_SURFACE('',#34594,0.25) ;
#30350 = CYLINDRICAL_SURFACE('',#34600,0.25) ;
#30351 = CYLINDRICAL_SURFACE('',#34606,0.25) ;
#30352 = CYLINDRICAL_SURFACE('',#34611,0.125) ;
#30353 = CYLINDRICAL_SURFACE('',#34616,0.125) ;
#30354 = CYLINDRICAL_SURFACE('',#34619,0.25) ;
#30355 = CYLINDRICAL_SURFACE('',#34626,0.25) ;
#30356 = CYLINDRICAL_SURFACE('',#34632,0.25) ;
#30357 = CYLINDRICAL_SURFACE('',#34638,0.25) ;
#30358 = CYLINDRICAL_SURFACE('',#34643,0.125) ;
#30359 = CYLINDRICAL_SURFACE('',#34646,0.125) ;
#30360 = CYLINDRICAL_SURFACE('',#34655,0.25) ;
#30361 = CYLINDRICAL_SURFACE('',#34661,0.25) ;
#30362 = CYLINDRICAL_SURFACE('',#34666,0.25) ;
#30363 = CYLINDRICAL_SURFACE('',#34671,0.25) ;
#30364 = CYLINDRICAL_SURFACE('',#34675,0.125) ;
#30365 = CYLINDRICAL_SURFACE('',#34680,0.125) ;
#30366 = CYLINDRICAL_SURFACE('',#34684,0.125) ;
#30367 = CYLINDRICAL_SURFACE('',#34686,0.125) ;
#30368 = CYLINDRICAL_SURFACE('',#34689,0.125) ;
#30369 = CYLINDRICAL_SURFACE('',#34691,0.125) ;
#30370 = CYLINDRICAL_SURFACE('',#34696,0.125) ;
#30371 = CYLINDRICAL_SURFACE('',#34698,0.125) ;
#30372 = CYLINDRICAL_SURFACE('',#34704,0.125) ;
#30373 = CYLINDRICAL_SURFACE('',#34713,0.125) ;
#30374 = CYLINDRICAL_SURFACE('',#34714,0.125) ;
#30375 = CYLINDRICAL_SURFACE('',#34719,0.125) ;
#30376 = CYLINDRICAL_SURFACE('',#34721,0.0635000000000012) ;
#30377 = CYLINDRICAL_SURFACE('',#34722,0.125) ;
#30378 = CYLINDRICAL_SURFACE('',#34724,0.0634999999999974) ;
#30379 = CYLINDRICAL_SURFACE('',#34727,0.125) ;
#30380 = CYLINDRICAL_SURFACE('',#34742,0.125) ;
#30381 = CYLINDRICAL_SURFACE('',#34743,0.125) ;
#30382 = CYLINDRICAL_SURFACE('',#34745,0.125) ;
#30383 = CYLINDRICAL_SURFACE('',#34747,0.125) ;
#30384 = CYLINDRICAL_SURFACE('',#34752,0.125) ;
#30385 = CYLINDRICAL_SURFACE('',#34754,0.125) ;
#30386 = CYLINDRICAL_SURFACE('',#34760,0.125) ;
#30387 = CYLINDRICAL_SURFACE('',#34769,0.125) ;
#30388 = CYLINDRICAL_SURFACE('',#34770,0.125) ;
#30389 = CYLINDRICAL_SURFACE('',#34775,0.125) ;
#30390 = CYLINDRICAL_SURFACE('',#34777,0.0635000000000012) ;
#30391 = CYLINDRICAL_SURFACE('',#34778,0.125) ;
#30392 = CYLINDRICAL_SURFACE('',#34780,0.0634999999999974) ;
#30393 = CYLINDRICAL_SURFACE('',#34784,0.125) ;
#30394 = CYLINDRICAL_SURFACE('',#34802,0.125) ;
#30395 = CYLINDRICAL_SURFACE('',#34803,0.125) ;
#30396 = CYLINDRICAL_SURFACE('',#34805,0.125) ;
#30397 = CYLINDRICAL_SURFACE('',#34807,0.125) ;
#30398 = CYLINDRICAL_SURFACE('',#34812,0.125) ;
#30399 = CYLINDRICAL_SURFACE('',#34814,0.125) ;
#30400 = CYLINDRICAL_SURFACE('',#34820,0.125) ;
#30401 = CYLINDRICAL_SURFACE('',#34829,0.125) ;
#30402 = CYLINDRICAL_SURFACE('',#34830,0.125) ;
#30403 = CYLINDRICAL_SURFACE('',#34835,0.125) ;
#30404 = CYLINDRICAL_SURFACE('',#34837,0.0635000000000012) ;
#30405 = CYLINDRICAL_SURFACE('',#34838,0.125) ;
#30406 = CYLINDRICAL_SURFACE('',#34840,0.0634999999999974) ;
#30407 = CYLINDRICAL_SURFACE('',#34844,0.125) ;
#30408 = CYLINDRICAL_SURFACE('',#34862,0.125) ;
#30409 = CYLINDRICAL_SURFACE('',#34863,0.125) ;
#30410 = CYLINDRICAL_SURFACE('',#34865,0.125) ;
#30411 = CYLINDRICAL_SURFACE('',#34867,0.125) ;
#30412 = CYLINDRICAL_SURFACE('',#34872,0.125) ;
#30413 = CYLINDRICAL_SURFACE('',#34874,0.125) ;
#30414 = CYLINDRICAL_SURFACE('',#34880,0.125) ;
#30415 = CYLINDRICAL_SURFACE('',#34889,0.125) ;
#30416 = CYLINDRICAL_SURFACE('',#34890,0.125) ;
#30417 = CYLINDRICAL_SURFACE('',#34895,0.125) ;
#30418 = CYLINDRICAL_SURFACE('',#34897,0.0635000000000012) ;
#30419 = CYLINDRICAL_SURFACE('',#34898,0.125) ;
#30420 = CYLINDRICAL_SURFACE('',#34900,0.0634999999999974) ;
#30421 = CYLINDRICAL_SURFACE('',#34904,0.125) ;
#30422 = CYLINDRICAL_SURFACE('',#34922,0.125) ;
#30423 = CYLINDRICAL_SURFACE('',#34923,0.125) ;
#30424 = CYLINDRICAL_SURFACE('',#34925,0.125) ;
#30425 = CYLINDRICAL_SURFACE('',#34927,0.125) ;
#30426 = CYLINDRICAL_SURFACE('',#34932,0.125) ;
#30427 = CYLINDRICAL_SURFACE('',#34934,0.125) ;
#30428 = CYLINDRICAL_SURFACE('',#34940,0.125) ;
#30429 = CYLINDRICAL_SURFACE('',#34949,0.125) ;
#30430 = CYLINDRICAL_SURFACE('',#34950,0.125) ;
#30431 = CYLINDRICAL_SURFACE('',#34955,0.125) ;
#30432 = CYLINDRICAL_SURFACE('',#34957,0.0635000000000012) ;
#30433 = CYLINDRICAL_SURFACE('',#34958,0.125) ;
#30434 = CYLINDRICAL_SURFACE('',#34960,0.0634999999999974) ;
#30435 = CYLINDRICAL_SURFACE('',#34964,0.125) ;
#30436 = CYLINDRICAL_SURFACE('',#34982,0.125) ;
#30437 = CYLINDRICAL_SURFACE('',#34983,0.125) ;
#30438 = CYLINDRICAL_SURFACE('',#34985,0.125) ;
#30439 = CYLINDRICAL_SURFACE('',#34987,0.125) ;
#30440 = CYLINDRICAL_SURFACE('',#34992,0.125) ;
#30441 = CYLINDRICAL_SURFACE('',#34994,0.125) ;
#30442 = CYLINDRICAL_SURFACE('',#35000,0.125) ;
#30443 = CYLINDRICAL_SURFACE('',#35009,0.125) ;
#30444 = CYLINDRICAL_SURFACE('',#35010,0.125) ;
#30445 = CYLINDRICAL_SURFACE('',#35015,0.125) ;
#30446 = CYLINDRICAL_SURFACE('',#35017,0.0635000000000012) ;
#30447 = CYLINDRICAL_SURFACE('',#35018,0.125) ;
#30448 = CYLINDRICAL_SURFACE('',#35020,0.0634999999999974) ;
#30449 = CYLINDRICAL_SURFACE('',#35024,0.125) ;
#30450 = CYLINDRICAL_SURFACE('',#35042,0.125) ;
#30451 = CYLINDRICAL_SURFACE('',#35043,0.125) ;
#30452 = CYLINDRICAL_SURFACE('',#35045,0.125) ;
#30453 = CYLINDRICAL_SURFACE('',#35047,0.125) ;
#30454 = CYLINDRICAL_SURFACE('',#35052,0.125) ;
#30455 = CYLINDRICAL_SURFACE('',#35054,0.125) ;
#30456 = CYLINDRICAL_SURFACE('',#35060,0.125) ;
#30457 = CYLINDRICAL_SURFACE('',#35069,0.125) ;
#30458 = CYLINDRICAL_SURFACE('',#35070,0.125) ;
#30459 = CYLINDRICAL_SURFACE('',#35075,0.125) ;
#30460 = CYLINDRICAL_SURFACE('',#35077,0.0635000000000012) ;
#30461 = CYLINDRICAL_SURFACE('',#35078,0.125) ;
#30462 = CYLINDRICAL_SURFACE('',#35080,0.0634999999999974) ;
#30463 = CYLINDRICAL_SURFACE('',#35084,0.125) ;
#30464 = CYLINDRICAL_SURFACE('',#35102,0.125) ;
#30465 = CYLINDRICAL_SURFACE('',#35103,0.125) ;
#30466 = CYLINDRICAL_SURFACE('',#35105,0.125) ;
#30467 = CYLINDRICAL_SURFACE('',#35107,0.125) ;
#30468 = CYLINDRICAL_SURFACE('',#35112,0.125) ;
#30469 = CYLINDRICAL_SURFACE('',#35114,0.125) ;
#30470 = CYLINDRICAL_SURFACE('',#35120,0.125) ;
#30471 = CYLINDRICAL_SURFACE('',#35129,0.125) ;
#30472 = CYLINDRICAL_SURFACE('',#35130,0.125) ;
#30473 = CYLINDRICAL_SURFACE('',#35135,0.125) ;
#30474 = CYLINDRICAL_SURFACE('',#35137,0.0635000000000012) ;
#30475 = CYLINDRICAL_SURFACE('',#35138,0.125) ;
#30476 = CYLINDRICAL_SURFACE('',#35140,0.0634999999999974) ;
#30477 = CYLINDRICAL_SURFACE('',#35144,0.125) ;
#30478 = CYLINDRICAL_SURFACE('',#35162,0.125) ;
#30479 = CYLINDRICAL_SURFACE('',#35163,0.125) ;
#30480 = CYLINDRICAL_SURFACE('',#35165,0.125) ;
#30481 = CYLINDRICAL_SURFACE('',#35167,0.125) ;
#30482 = CYLINDRICAL_SURFACE('',#35172,0.125) ;
#30483 = CYLINDRICAL_SURFACE('',#35174,0.125) ;
#30484 = CYLINDRICAL_SURFACE('',#35180,0.125) ;
#30485 = CYLINDRICAL_SURFACE('',#35189,0.125) ;
#30486 = CYLINDRICAL_SURFACE('',#35190,0.125) ;
#30487 = CYLINDRICAL_SURFACE('',#35195,0.125) ;
#30488 = CYLINDRICAL_SURFACE('',#35197,0.0635000000000012) ;
#30489 = CYLINDRICAL_SURFACE('',#35198,0.125) ;
#30490 = CYLINDRICAL_SURFACE('',#35200,0.0634999999999974) ;
#30491 = CYLINDRICAL_SURFACE('',#35204,0.125) ;
#30492 = CYLINDRICAL_SURFACE('',#35222,0.125) ;
#30493 = CYLINDRICAL_SURFACE('',#35223,0.125) ;
#30494 = CYLINDRICAL_SURFACE('',#35225,0.125) ;
#30495 = CYLINDRICAL_SURFACE('',#35227,0.125) ;
#30496 = CYLINDRICAL_SURFACE('',#35260,0.75) ;
#30497 = CYLINDRICAL_SURFACE('',#35264,0.75) ;
#30498 = CYLINDRICAL_SURFACE('',#35267,0.75) ;
#30499 = CYLINDRICAL_SURFACE('',#35270,0.75) ;
#30500 = CYLINDRICAL_SURFACE('',#35273,0.75) ;
#30501 = CYLINDRICAL_SURFACE('',#35276,0.75) ;
#30502 = CYLINDRICAL_SURFACE('',#35279,0.75) ;
#30503 = CYLINDRICAL_SURFACE('',#35282,0.75) ;
#30504 = CYLINDRICAL_SURFACE('',#35285,0.75) ;
#30505 = CYLINDRICAL_SURFACE('',#35290,0.75) ;
#30506 = CYLINDRICAL_SURFACE('',#35334,2.8575) ;
#30507 = CYLINDRICAL_SURFACE('',#35339,0.125) ;
#30508 = CYLINDRICAL_SURFACE('',#35346,2.8575) ;
#30509 = CYLINDRICAL_SURFACE('',#35351,0.125) ;
#30510 = CYLINDRICAL_SURFACE('',#35358,2.8575) ;
#30511 = CYLINDRICAL_SURFACE('',#35363,0.125) ;
#30512 = CYLINDRICAL_SURFACE('',#35370,2.8575) ;
#30513 = CYLINDRICAL_SURFACE('',#35375,0.125) ;
#30514 = CYLINDRICAL_SURFACE('',#35382,2.8575) ;
#30515 = CYLINDRICAL_SURFACE('',#35387,0.125) ;
#30516 = CYLINDRICAL_SURFACE('',#35394,2.8575) ;
#30517 = CYLINDRICAL_SURFACE('',#35399,0.125) ;
#30518 = CYLINDRICAL_SURFACE('',#35406,2.8575) ;
#30519 = CYLINDRICAL_SURFACE('',#35411,0.125) ;
#30520 = CYLINDRICAL_SURFACE('',#35418,2.8575) ;
#30521 = CYLINDRICAL_SURFACE('',#35423,0.125) ;
#30522 = CYLINDRICAL_SURFACE('',#35428,2.8575) ;
#30523 = CYLINDRICAL_SURFACE('',#35434,0.125) ;
#30524 = CYLINDRICAL_SURFACE('',#35436,0.125) ;
#30525 = CYLINDRICAL_SURFACE('',#35438,0.125) ;
#30526 = CYLINDRICAL_SURFACE('',#35439,0.125) ;
#30527 = CYLINDRICAL_SURFACE('',#35441,0.125) ;
#30528 = CYLINDRICAL_SURFACE('',#35443,0.125) ;
#30529 = CYLINDRICAL_SURFACE('',#35444,0.125) ;
#30530 = CYLINDRICAL_SURFACE('',#35446,0.125) ;
#30531 = CYLINDRICAL_SURFACE('',#35448,0.125) ;
#30532 = CYLINDRICAL_SURFACE('',#35449,0.125) ;
#30533 = CYLINDRICAL_SURFACE('',#35451,0.125) ;
#30534 = CYLINDRICAL_SURFACE('',#35453,0.125) ;
#30535 = CYLINDRICAL_SURFACE('',#35454,0.125) ;
#30536 = CYLINDRICAL_SURFACE('',#35456,0.125) ;
#30537 = CYLINDRICAL_SURFACE('',#35458,0.125) ;
#30538 = CYLINDRICAL_SURFACE('',#35459,0.125) ;
#30539 = CYLINDRICAL_SURFACE('',#35461,0.125) ;
#30540 = CYLINDRICAL_SURFACE('',#35463,0.125) ;
#30541 = CYLINDRICAL_SURFACE('',#35464,0.125) ;
#30542 = CYLINDRICAL_SURFACE('',#35466,0.125) ;
#30543 = CYLINDRICAL_SURFACE('',#35468,0.125) ;
#30544 = CYLINDRICAL_SURFACE('',#35469,0.125) ;
#30545 = CYLINDRICAL_SURFACE('',#35471,0.125) ;
#30546 = CYLINDRICAL_SURFACE('',#35473,0.125) ;
#30547 = CYLINDRICAL_SURFACE('',#35476,1.2370442518096) ;
#30548 = CYLINDRICAL_SURFACE('',#35477,1.2370442518096) ;
#30549 = CYLINDRICAL_SURFACE('',#35478,1.2370442518096) ;
#30550 = CYLINDRICAL_SURFACE('',#35479,1.2370442518096) ;
#30551 = CYLINDRICAL_SURFACE('',#35480,1.2370442518096) ;
#30552 = CYLINDRICAL_SURFACE('',#35481,1.2370442518096) ;
#30553 = CYLINDRICAL_SURFACE('',#35482,1.2370442518096) ;
#30554 = CYLINDRICAL_SURFACE('',#35483,1.2370442518096) ;
#30555 = CYLINDRICAL_SURFACE('',#35485,1.7526) ;
#30556 = CYLINDRICAL_SURFACE('',#35487,1.7526) ;
#30557 = CYLINDRICAL_SURFACE('',#35488,1.7526) ;
#30558 = CYLINDRICAL_SURFACE('',#35489,1.7526) ;
#30559 = CYLINDRICAL_SURFACE('',#35490,1.7526) ;
#30560 = CYLINDRICAL_SURFACE('',#35491,1.7526) ;
#30561 = CYLINDRICAL_SURFACE('',#35492,1.7526) ;
#30562 = CYLINDRICAL_SURFACE('',#35493,1.7526) ;
#30563 = CYLINDRICAL_SURFACE('',#35495,1.2370442518096) ;
#30564 = CYLINDRICAL_SURFACE('',#35529,0.1) ;
#30565 = CYLINDRICAL_SURFACE('',#35553,0.1) ;
#30566 = CYLINDRICAL_SURFACE('',#35561,0.1) ;
#30567 = CYLINDRICAL_SURFACE('',#35571,0.1) ;
#30568 = CYLINDRICAL_SURFACE('',#35592,0.1) ;
#30569 = CYLINDRICAL_SURFACE('',#35596,0.1) ;
#30570 = CYLINDRICAL_SURFACE('',#35603,0.1) ;
#30571 = CYLINDRICAL_SURFACE('',#35622,0.1) ;
#30572 = CYLINDRICAL_SURFACE('',#35635,0.1) ;
#30573 = CYLINDRICAL_SURFACE('',#35639,0.1) ;
#30574 = CYLINDRICAL_SURFACE('',#35646,0.1) ;
#30575 = CYLINDRICAL_SURFACE('',#35650,0.1) ;
#30576 = CYLINDRICAL_SURFACE('',#35657,0.1) ;
#30577 = CYLINDRICAL_SURFACE('',#35681,0.1) ;
#30578 = CYLINDRICAL_SURFACE('',#35694,0.1) ;
#30579 = CYLINDRICAL_SURFACE('',#35697,0.1) ;
#30580 = CYLINDRICAL_SURFACE('',#35702,0.1) ;
#30581 = CYLINDRICAL_SURFACE('',#35708,0.1) ;
#30582 = CYLINDRICAL_SURFACE('',#35715,0.1) ;
#30583 = CYLINDRICAL_SURFACE('',#35718,0.1) ;
#30584 = CYLINDRICAL_SURFACE('',#35722,0.1) ;
#30585 = CYLINDRICAL_SURFACE('',#35723,0.1) ;
#30586 = CYLINDRICAL_SURFACE('',#35728,0.1) ;
#30587 = CYLINDRICAL_SURFACE('',#35733,0.1) ;
#30588 = CYLINDRICAL_SURFACE('',#35747,0.1) ;
#30589 = CYLINDRICAL_SURFACE('',#35752,0.1) ;
#30590 = CYLINDRICAL_SURFACE('',#35753,0.1) ;
#30591 = CYLINDRICAL_SURFACE('',#35757,0.1) ;
#30592 = CYLINDRICAL_SURFACE('',#35758,0.1) ;
#30593 = CYLINDRICAL_SURFACE('',#35759,0.1) ;
#30594 = CYLINDRICAL_SURFACE('',#35776,0.1) ;
#30595 = CYLINDRICAL_SURFACE('',#35789,0.1) ;
#30596 = CYLINDRICAL_SURFACE('',#35792,0.1) ;
#30597 = CYLINDRICAL_SURFACE('',#35795,0.1) ;
#30598 = CYLINDRICAL_SURFACE('',#35804,0.1) ;
#30599 = CYLINDRICAL_SURFACE('',#35811,0.1) ;
#30600 = CYLINDRICAL_SURFACE('',#35812,0.1) ;
#30601 = CYLINDRICAL_SURFACE('',#35815,0.1) ;
#30602 = CYLINDRICAL_SURFACE('',#35819,0.1) ;
#30603 = CYLINDRICAL_SURFACE('',#35821,0.1) ;
#30604 = CYLINDRICAL_SURFACE('',#35826,0.1) ;
#30605 = CYLINDRICAL_SURFACE('',#35831,0.1) ;
#30606 = CYLINDRICAL_SURFACE('',#35848,0.1) ;
#30607 = CYLINDRICAL_SURFACE('',#35849,0.1) ;
#30608 = CYLINDRICAL_SURFACE('',#35853,0.1) ;
#30609 = CYLINDRICAL_SURFACE('',#35854,0.1) ;
#30610 = CYLINDRICAL_SURFACE('',#35876,0.1) ;
#30611 = CYLINDRICAL_SURFACE('',#35882,3.429) ;
#30612 = CYLINDRICAL_SURFACE('',#35891,0.1) ;
#30613 = CYLINDRICAL_SURFACE('',#35896,3.429) ;
#30614 = CYLINDRICAL_SURFACE('',#35913,1.7526) ;
#30615 = CYLINDRICAL_SURFACE('',#35915,1.7526) ;
#30616 = CYLINDRICAL_SURFACE('',#35916,1.7526) ;
#30617 = CYLINDRICAL_SURFACE('',#35917,1.7526) ;
#30618 = CYLINDRICAL_SURFACE('',#35919,1.5) ;
#30619 = CYLINDRICAL_SURFACE('',#35921,1.5) ;
#30620 = CYLINDRICAL_SURFACE('',#35922,1.5) ;
#30621 = CYLINDRICAL_SURFACE('',#35923,1.5) ;
#30622 = CYLINDRICAL_SURFACE('',#35925,1.5) ;
#30623 = CYLINDRICAL_SURFACE('',#35926,1.7526) ;
#30624 = CYLINDRICAL_SURFACE('',#35927,0.125) ;
#30625 = CYLINDRICAL_SURFACE('',#35935,0.125) ;
#30626 = CYLINDRICAL_SURFACE('',#35947,0.125) ;
#30627 = CYLINDRICAL_SURFACE('',#35953,0.125) ;
#30628 = CYLINDRICAL_SURFACE('',#35954,0.125) ;
#30629 = CYLINDRICAL_SURFACE('',#35961,0.125) ;
#30630 = CYLINDRICAL_SURFACE('',#35963,0.125) ;
#30631 = CYLINDRICAL_SURFACE('',#35969,0.125) ;
#30632 = CYLINDRICAL_SURFACE('',#35970,0.0635000000000012) ;
#30633 = CYLINDRICAL_SURFACE('',#35971,0.125) ;
#30634 = CYLINDRICAL_SURFACE('',#35973,0.0634999999999974) ;
#30635 = CYLINDRICAL_SURFACE('',#35978,0.125) ;
#30636 = CYLINDRICAL_SURFACE('',#35986,0.125) ;
#30637 = CYLINDRICAL_SURFACE('',#35989,0.125) ;
#30638 = CYLINDRICAL_SURFACE('',#35995,0.634999999999996) ;
#30639 = CYLINDRICAL_SURFACE('',#35996,0.125) ;
#30640 = CYLINDRICAL_SURFACE('',#35998,0.125) ;
#30641 = CYLINDRICAL_SURFACE('',#36010,0.698499999999999) ;
#30642 = CYLINDRICAL_SURFACE('',#36013,0.698500000000001) ;
#30643 = CYLINDRICAL_SURFACE('',#36016,0.0634999999999973) ;
#30644 = CYLINDRICAL_SURFACE('',#36017,0.0635000000000008) ;
#30645 = CYLINDRICAL_SURFACE('',#36019,0.125) ;
#30646 = CYLINDRICAL_SURFACE('',#36028,0.125) ;
#30647 = CYLINDRICAL_SURFACE('',#36050,0.125) ;
#30648 = CYLINDRICAL_SURFACE('',#36051,0.125) ;
#30649 = CYLINDRICAL_SURFACE('',#36053,0.125) ;
#30650 = CYLINDRICAL_SURFACE('',#36055,0.125) ;
#30651 = CYLINDRICAL_SURFACE('',#36058,0.125) ;
#30652 = CYLINDRICAL_SURFACE('',#36061,0.125) ;
#30653 = CYLINDRICAL_SURFACE('',#36066,0.125) ;
#30654 = CYLINDRICAL_SURFACE('',#36070,0.125) ;
#30655 = CYLINDRICAL_SURFACE('',#36072,0.125) ;
#30656 = CYLINDRICAL_SURFACE('',#36075,0.125) ;
#30657 = CYLINDRICAL_SURFACE('',#36078,0.125) ;
#30658 = CYLINDRICAL_SURFACE('',#36083,0.125) ;
#30659 = CYLINDRICAL_SURFACE('',#36087,0.125) ;
#30660 = CYLINDRICAL_SURFACE('',#36089,0.125) ;
#30661 = CYLINDRICAL_SURFACE('',#36091,0.125) ;
#30662 = CYLINDRICAL_SURFACE('',#36094,0.125) ;
#30663 = CYLINDRICAL_SURFACE('',#36096,0.125) ;
#30664 = CYLINDRICAL_SURFACE('',#36098,0.125) ;
#30665 = CYLINDRICAL_SURFACE('',#36101,0.125) ;
#30666 = CYLINDRICAL_SURFACE('',#36106,0.125) ;
#30667 = CYLINDRICAL_SURFACE('',#36108,0.125) ;
#30668 = CYLINDRICAL_SURFACE('',#36112,0.125) ;
#30669 = CYLINDRICAL_SURFACE('',#36128,2.8575) ;
#30670 = CYLINDRICAL_SURFACE('',#36155,1.651) ;
#30671 = CYLINDRICAL_SURFACE('',#36175,0.095249999999997) ;
#30672 = CYLINDRICAL_SURFACE('',#36177,0.0952499999999953) ;
#30673 = CYLINDRICAL_SURFACE('',#36183,0.095249999999997) ;
#30674 = CYLINDRICAL_SURFACE('',#36185,0.0952499999999975) ;
#30675 = CYLINDRICAL_SURFACE('',#36191,0.0952500000000012) ;
#30676 = CYLINDRICAL_SURFACE('',#36193,0.0952500000000014) ;
#30677 = CYLINDRICAL_SURFACE('',#36197,0.635) ;
#30678 = CYLINDRICAL_SURFACE('',#36199,0.0635000000000001) ;
#30679 = CYLINDRICAL_SURFACE('',#36202,0.0635000000000013) ;
#30680 = CYLINDRICAL_SURFACE('',#36212,0.0634999999999983) ;
#30681 = CYLINDRICAL_SURFACE('',#36214,0.0635000000000001) ;
#30682 = CYLINDRICAL_SURFACE('',#36218,0.635) ;
#30683 = CYLINDRICAL_SURFACE('',#36223,0.0634999999999983) ;
#30684 = CYLINDRICAL_SURFACE('',#36225,0.0635000000000001) ;
#30685 = CYLINDRICAL_SURFACE('',#36229,0.635) ;
#30686 = CYLINDRICAL_SURFACE('',#36231,0.0635000000000001) ;
#30687 = CYLINDRICAL_SURFACE('',#36234,0.0635000000000012) ;
#30688 = CYLINDRICAL_SURFACE('',#36238,0.635) ;
#30689 = CYLINDRICAL_SURFACE('',#36243,0.0952500000000027) ;
#30690 = CYLINDRICAL_SURFACE('',#36245,0.0952499999999953) ;
#30691 = CYLINDRICAL_SURFACE('',#36251,0.635000000000001) ;
#30692 = CYLINDRICAL_SURFACE('',#36254,0.189865) ;
#30693 = CYLINDRICAL_SURFACE('',#36257,0.189865) ;
#30694 = CYLINDRICAL_SURFACE('',#36265,0.635000000000001) ;
#30695 = CYLINDRICAL_SURFACE('',#36268,0.189865) ;
#30696 = CYLINDRICAL_SURFACE('',#36271,0.189865) ;
#30697 = CYLINDRICAL_SURFACE('',#36279,0.635) ;
#30698 = CYLINDRICAL_SURFACE('',#36282,0.189865000000002) ;
#30699 = CYLINDRICAL_SURFACE('',#36285,0.189865000000002) ;
#30700 = CYLINDRICAL_SURFACE('',#36293,0.635) ;
#30701 = CYLINDRICAL_SURFACE('',#36296,0.189865000000002) ;
#30702 = CYLINDRICAL_SURFACE('',#36299,0.189865000000002) ;
#30703 = CYLINDRICAL_SURFACE('',#36326,5.22940367264148) ;
#30704 = CYLINDRICAL_SURFACE('',#36327,5.22940367264148) ;
#30705 = CYLINDRICAL_SURFACE('',#36328,5.22940367264148) ;
#30706 = CYLINDRICAL_SURFACE('',#36329,5.22940367264148) ;
#30707 = CYLINDRICAL_SURFACE('',#36372,1.25) ;
#30708 = CYLINDRICAL_SURFACE('',#36373,1.25) ;
#30709 = CYLINDRICAL_SURFACE('',#36374,1.25) ;
#30710 = CYLINDRICAL_SURFACE('',#36375,1.25) ;
#30711 = CYLINDRICAL_SURFACE('',#36376,1.25) ;
#30712 = CYLINDRICAL_SURFACE('',#36382,1.5) ;
#30713 = CYLINDRICAL_SURFACE('',#36384,1.5) ;
#30714 = CYLINDRICAL_SURFACE('',#36385,1.5) ;
#30715 = CYLINDRICAL_SURFACE('',#36386,1.5) ;
#30716 = CYLINDRICAL_SURFACE('',#36387,1.5) ;
#30717 = CYLINDRICAL_SURFACE('',#36388,1.5) ;
#30718 = CYLINDRICAL_SURFACE('',#36389,1.5) ;
#30719 = CYLINDRICAL_SURFACE('',#36390,1.5) ;
#30720 = CYLINDRICAL_SURFACE('',#36391,1.5) ;
#30721 = CYLINDRICAL_SURFACE('',#36392,1.5) ;
#30722 = CYLINDRICAL_SURFACE('',#36393,1.5) ;
#30723 = CYLINDRICAL_SURFACE('',#36394,1.5) ;
#30724 = CYLINDRICAL_SURFACE('',#36395,1.5) ;
#30725 = CYLINDRICAL_SURFACE('',#36396,1.5) ;
#30726 = CYLINDRICAL_SURFACE('',#36397,1.5) ;
#30727 = CYLINDRICAL_SURFACE('',#36398,1.17524047358084) ;
#30728 = CYLINDRICAL_SURFACE('',#36400,1.17524047358084) ;
#30729 = CYLINDRICAL_SURFACE('',#36401,1.17524047358084) ;
#30730 = CYLINDRICAL_SURFACE('',#36402,1.17524047358084) ;
#30731 = CYLINDRICAL_SURFACE('',#36403,1.17524047358084) ;
#30732 = CYLINDRICAL_SURFACE('',#36404,1.17524047358084) ;
#30733 = CYLINDRICAL_SURFACE('',#36405,1.17524047358084) ;
#30734 = CYLINDRICAL_SURFACE('',#36406,1.17524047358084) ;
#30735 = CYLINDRICAL_SURFACE('',#36407,1.17524047358084) ;
#30736 = CYLINDRICAL_SURFACE('',#36408,1.17524047358084) ;
#30737 = CYLINDRICAL_SURFACE('',#36409,1.17524047358084) ;
#30738 = CYLINDRICAL_SURFACE('',#36410,1.17524047358084) ;
#30739 = CYLINDRICAL_SURFACE('',#36411,1.17524047358084) ;
#30740 = CYLINDRICAL_SURFACE('',#36412,1.17524047358084) ;
#30741 = CYLINDRICAL_SURFACE('',#36413,1.17524047358084) ;
#30742 = CYLINDRICAL_SURFACE('',#36414,1.17524047358084) ;
#30743 = CYLINDRICAL_SURFACE('',#36419,1.17524047358084) ;
#30744 = CYLINDRICAL_SURFACE('',#36421,1.5) ;
#30745 = CYLINDRICAL_SURFACE('',#36453,2.99999999999999) ;
#30746 = CYLINDRICAL_SURFACE('',#36485,2.8) ;
#30747 = CYLINDRICAL_SURFACE('',#36492,3.) ;
#30748 = CYLINDRICAL_SURFACE('',#36502,1.6) ;
#30749 = ADVANCED_FACE('',(#2270),#29948,.F.) ;
#30750 = ADVANCED_FACE('',(#2271,#1000,#1001,#1002,#1003,#1004,#1005,#1006,
#1007,#1008,#1009,#1010,#1011,#1012,#1013,#1014,#1015,#1016,#1017,#1018,
#1019),#1706,.F.) ;
#30751 = ADVANCED_FACE('',(#2272),#29949,.F.) ;
#30752 = ADVANCED_FACE('',(#2273),#29950,.F.) ;
#30753 = ADVANCED_FACE('',(#2274,#1020,#1021),#1707,.T.) ;
#30754 = ADVANCED_FACE('',(#2275),#29951,.T.) ;
#30755 = ADVANCED_FACE('',(#2276),#1708,.F.) ;
#30756 = ADVANCED_FACE('',(#2277,#1022,#1023),#1709,.F.) ;
#30757 = ADVANCED_FACE('',(#2278),#29952,.T.) ;
#30758 = ADVANCED_FACE('',(#2279),#1710,.F.) ;
#30759 = ADVANCED_FACE('',(#2280,#1024,#1025),#1711,.F.) ;
#30760 = ADVANCED_FACE('',(#2281),#29953,.F.) ;
#30761 = ADVANCED_FACE('',(#2282),#1712,.F.) ;
#30762 = ADVANCED_FACE('',(#2283),#29954,.F.) ;
#30763 = ADVANCED_FACE('',(#2284),#1713,.F.) ;
#30764 = ADVANCED_FACE('',(#2285),#29955,.T.) ;
#30765 = ADVANCED_FACE('',(#2286),#1714,.F.) ;
#30766 = ADVANCED_FACE('',(#2287,#1026,#1027,#1028,#1029,#1030,#1031,#1032,
#1033,#1034,#1035,#1036,#1037,#1038,#1039,#1040,#1041,#1042,#1043,#1044,
#1045),#1715,.T.) ;
#30767 = ADVANCED_FACE('',(#2288,#1046,#1047),#1716,.F.) ;
#30768 = ADVANCED_FACE('',(#2289),#1717,.T.) ;
#30769 = ADVANCED_FACE('',(#2290),#29956,.F.) ;
#30770 = ADVANCED_FACE('',(#2291),#29957,.F.) ;
#30771 = ADVANCED_FACE('',(#2292),#29958,.F.) ;
#30772 = ADVANCED_FACE('',(#2293),#29959,.F.) ;
#30773 = ADVANCED_FACE('',(#2294),#29960,.F.) ;
#30774 = ADVANCED_FACE('',(#2295),#903,.T.) ;
#30775 = ADVANCED_FACE('',(#2296),#29961,.F.) ;
#30776 = ADVANCED_FACE('',(#2297),#29962,.F.) ;
#30777 = ADVANCED_FACE('',(#2298),#904,.T.) ;
#30778 = ADVANCED_FACE('',(#2299),#29963,.F.) ;
#30779 = ADVANCED_FACE('',(#2300),#29964,.F.) ;
#30780 = ADVANCED_FACE('',(#2301),#29965,.F.) ;
#30781 = ADVANCED_FACE('',(#2302),#29966,.T.) ;
#30782 = ADVANCED_FACE('',(#2303),#1718,.F.) ;
#30783 = ADVANCED_FACE('',(#2304),#29967,.T.) ;
#30784 = ADVANCED_FACE('',(#2305),#1719,.F.) ;
#30785 = ADVANCED_FACE('',(#2306),#29968,.T.) ;
#30786 = ADVANCED_FACE('',(#2307),#29969,.T.) ;
#30787 = ADVANCED_FACE('',(#2308),#1720,.F.) ;
#30788 = ADVANCED_FACE('',(#2309),#1721,.F.) ;
#30789 = ADVANCED_FACE('',(#2310),#29970,.T.) ;
#30790 = ADVANCED_FACE('',(#2311),#1722,.F.) ;
#30791 = ADVANCED_FACE('',(#2312),#29971,.T.) ;
#30792 = ADVANCED_FACE('',(#2313),#1723,.F.) ;
#30793 = ADVANCED_FACE('',(#2314),#29972,.T.) ;
#30794 = ADVANCED_FACE('',(#2315),#1724,.F.) ;
#30795 = ADVANCED_FACE('',(#2316),#29973,.F.) ;
#30796 = ADVANCED_FACE('',(#2317),#1725,.F.) ;
#30797 = ADVANCED_FACE('',(#2318),#29974,.T.) ;
#30798 = ADVANCED_FACE('',(#2319),#29975,.T.) ;
#30799 = ADVANCED_FACE('',(#2320),#1726,.F.) ;
#30800 = ADVANCED_FACE('',(#2321),#29976,.F.) ;
#30801 = ADVANCED_FACE('',(#2322),#1727,.F.) ;
#30802 = ADVANCED_FACE('',(#2323),#29977,.T.) ;
#30803 = ADVANCED_FACE('',(#2324),#29978,.F.) ;
#30804 = ADVANCED_FACE('',(#2325),#1728,.T.) ;
#30805 = ADVANCED_FACE('',(#2326),#29979,.T.) ;
#30806 = ADVANCED_FACE('',(#2327),#1729,.T.) ;
#30807 = ADVANCED_FACE('',(#2328),#29980,.T.) ;
#30808 = ADVANCED_FACE('',(#2329),#29981,.F.) ;
#30809 = ADVANCED_FACE('',(#2330),#1730,.T.) ;
#30810 = ADVANCED_FACE('',(#2331),#29982,.T.) ;
#30811 = ADVANCED_FACE('',(#2332),#1731,.F.) ;
#30812 = ADVANCED_FACE('',(#2333),#29983,.T.) ;
#30813 = ADVANCED_FACE('',(#2334),#1732,.T.) ;
#30814 = ADVANCED_FACE('',(#2335),#29984,.F.) ;
#30815 = ADVANCED_FACE('',(#2336),#1733,.F.) ;
#30816 = ADVANCED_FACE('',(#2337),#1734,.F.) ;
#30817 = ADVANCED_FACE('',(#2338),#1735,.F.) ;
#30818 = ADVANCED_FACE('',(#2339),#29985,.F.) ;
#30819 = ADVANCED_FACE('',(#2340),#29986,.F.) ;
#30820 = ADVANCED_FACE('',(#2341),#1736,.F.) ;
#30821 = ADVANCED_FACE('',(#2342),#29987,.F.) ;
#30822 = ADVANCED_FACE('',(#2343),#29988,.F.) ;
#30823 = ADVANCED_FACE('',(#2344),#29989,.F.) ;
#30824 = ADVANCED_FACE('',(#2345),#29990,.T.) ;
#30825 = ADVANCED_FACE('',(#2346),#29991,.F.) ;
#30826 = ADVANCED_FACE('',(#2347),#29992,.T.) ;
#30827 = ADVANCED_FACE('',(#2348),#862,.F.) ;
#30828 = ADVANCED_FACE('',(#2349),#863,.F.) ;
#30829 = ADVANCED_FACE('',(#2350),#1737,.F.) ;
#30830 = ADVANCED_FACE('',(#2351),#1738,.F.) ;
#30831 = ADVANCED_FACE('',(#2352),#29993,.F.) ;
#30832 = ADVANCED_FACE('',(#2353),#29994,.F.) ;
#30833 = ADVANCED_FACE('',(#2354),#29995,.F.) ;
#30834 = ADVANCED_FACE('',(#2355),#29996,.F.) ;
#30835 = ADVANCED_FACE('',(#2356),#29997,.F.) ;
#30836 = ADVANCED_FACE('',(#2357),#1739,.F.) ;
#30837 = ADVANCED_FACE('',(#2358),#29998,.F.) ;
#30838 = ADVANCED_FACE('',(#2359),#1740,.F.) ;
#30839 = ADVANCED_FACE('',(#2360),#29999,.F.) ;
#30840 = ADVANCED_FACE('',(#2361),#1741,.F.) ;
#30841 = ADVANCED_FACE('',(#2362),#30000,.F.) ;
#30842 = ADVANCED_FACE('',(#2363),#1742,.F.) ;
#30843 = ADVANCED_FACE('',(#2364),#30001,.F.) ;
#30844 = ADVANCED_FACE('',(#2365),#1743,.F.) ;
#30845 = ADVANCED_FACE('',(#2366),#30002,.F.) ;
#30846 = ADVANCED_FACE('',(#2367),#1744,.F.) ;
#30847 = ADVANCED_FACE('',(#2368),#30003,.F.) ;
#30848 = ADVANCED_FACE('',(#2369),#1745,.F.) ;
#30849 = ADVANCED_FACE('',(#2370),#30004,.F.) ;
#30850 = ADVANCED_FACE('',(#2371),#1746,.F.) ;
#30851 = ADVANCED_FACE('',(#2372),#30005,.F.) ;
#30852 = ADVANCED_FACE('',(#2373),#1747,.F.) ;
#30853 = ADVANCED_FACE('',(#2374),#30006,.F.) ;
#30854 = ADVANCED_FACE('',(#2375),#1748,.F.) ;
#30855 = ADVANCED_FACE('',(#2376),#30007,.F.) ;
#30856 = ADVANCED_FACE('',(#2377),#1749,.F.) ;
#30857 = ADVANCED_FACE('',(#2378),#30008,.F.) ;
#30858 = ADVANCED_FACE('',(#2379),#1750,.F.) ;
#30859 = ADVANCED_FACE('',(#2380),#30009,.T.) ;
#30860 = ADVANCED_FACE('',(#2381),#1751,.F.) ;
#30861 = ADVANCED_FACE('',(#2382),#30010,.F.) ;
#30862 = ADVANCED_FACE('',(#2383),#30011,.T.) ;
#30863 = ADVANCED_FACE('',(#2384),#30012,.T.) ;
#30864 = ADVANCED_FACE('',(#2385),#30013,.T.) ;
#30865 = ADVANCED_FACE('',(#2386),#30014,.F.) ;
#30866 = ADVANCED_FACE('',(#2387),#30015,.F.) ;
#30867 = ADVANCED_FACE('',(#2388),#30016,.T.) ;
#30868 = ADVANCED_FACE('',(#2389),#30017,.F.) ;
#30869 = ADVANCED_FACE('',(#2390),#30018,.F.) ;
#30870 = ADVANCED_FACE('',(#2391),#30019,.F.) ;
#30871 = ADVANCED_FACE('',(#2392),#30020,.T.) ;
#30872 = ADVANCED_FACE('',(#2393),#30021,.F.) ;
#30873 = ADVANCED_FACE('',(#2394),#30022,.F.) ;
#30874 = ADVANCED_FACE('',(#2395),#30023,.F.) ;
#30875 = ADVANCED_FACE('',(#2396),#30024,.T.) ;
#30876 = ADVANCED_FACE('',(#2397),#30025,.F.) ;
#30877 = ADVANCED_FACE('',(#2398),#30026,.F.) ;
#30878 = ADVANCED_FACE('',(#2399),#30027,.F.) ;
#30879 = ADVANCED_FACE('',(#2400),#30028,.F.) ;
#30880 = ADVANCED_FACE('',(#2401),#30029,.F.) ;
#30881 = ADVANCED_FACE('',(#2402),#30030,.F.) ;
#30882 = ADVANCED_FACE('',(#2403),#30031,.F.) ;
#30883 = ADVANCED_FACE('',(#2404),#30032,.F.) ;
#30884 = ADVANCED_FACE('',(#2405),#30033,.F.) ;
#30885 = ADVANCED_FACE('',(#2406),#30034,.F.) ;
#30886 = ADVANCED_FACE('',(#2407),#30035,.F.) ;
#30887 = ADVANCED_FACE('',(#2408),#30036,.F.) ;
#30888 = ADVANCED_FACE('',(#2409),#864,.F.) ;
#30889 = ADVANCED_FACE('',(#2410),#865,.F.) ;
#30890 = ADVANCED_FACE('',(#2411),#866,.F.) ;
#30891 = ADVANCED_FACE('',(#2412),#867,.F.) ;
#30892 = ADVANCED_FACE('',(#2413),#30037,.F.) ;
#30893 = ADVANCED_FACE('',(#2414),#30038,.F.) ;
#30894 = ADVANCED_FACE('',(#2415),#868,.T.) ;
#30895 = ADVANCED_FACE('',(#2416),#869,.T.) ;
#30896 = ADVANCED_FACE('',(#2417),#736,.T.) ;
#30897 = ADVANCED_FACE('',(#2418),#737,.T.) ;
#30898 = ADVANCED_FACE('',(#2419,#1048),#1752,.T.) ;
#30899 = ADVANCED_FACE('',(#2420),#1753,.F.) ;
#30900 = ADVANCED_FACE('',(#2421),#1754,.F.) ;
#30901 = ADVANCED_FACE('',(#2422),#1755,.F.) ;
#30902 = ADVANCED_FACE('',(#2423),#1756,.F.) ;
#30903 = ADVANCED_FACE('',(#2424),#1757,.F.) ;
#30904 = ADVANCED_FACE('',(#2425),#1758,.F.) ;
#30905 = ADVANCED_FACE('',(#2426,#1049),#1759,.F.) ;
#30906 = ADVANCED_FACE('',(#2427),#870,.T.) ;
#30907 = ADVANCED_FACE('',(#2428),#871,.T.) ;
#30908 = ADVANCED_FACE('',(#2429),#872,.T.) ;
#30909 = ADVANCED_FACE('',(#2430),#873,.T.) ;
#30910 = ADVANCED_FACE('',(#2431),#874,.T.) ;
#30911 = ADVANCED_FACE('',(#2432),#875,.T.) ;
#30912 = ADVANCED_FACE('',(#2433),#876,.T.) ;
#30913 = ADVANCED_FACE('',(#2434),#877,.T.) ;
#30914 = ADVANCED_FACE('',(#2435),#878,.T.) ;
#30915 = ADVANCED_FACE('',(#2436),#879,.T.) ;
#30916 = ADVANCED_FACE('',(#2437),#30039,.T.) ;
#30917 = ADVANCED_FACE('',(#2438),#30040,.T.) ;
#30918 = ADVANCED_FACE('',(#2439),#30041,.T.) ;
#30919 = ADVANCED_FACE('',(#2440),#30042,.T.) ;
#30920 = ADVANCED_FACE('',(#2441),#30043,.T.) ;
#30921 = ADVANCED_FACE('',(#2442),#30044,.T.) ;
#30922 = ADVANCED_FACE('',(#2443),#30045,.T.) ;
#30923 = ADVANCED_FACE('',(#2444),#30046,.T.) ;
#30924 = ADVANCED_FACE('',(#2445),#30047,.T.) ;
#30925 = ADVANCED_FACE('',(#2446),#30048,.T.) ;
#30926 = ADVANCED_FACE('',(#2447),#30049,.T.) ;
#30927 = ADVANCED_FACE('',(#2448),#30050,.T.) ;
#30928 = ADVANCED_FACE('',(#2449),#30051,.T.) ;
#30929 = ADVANCED_FACE('',(#2450),#226,.T.) ;
#30930 = ADVANCED_FACE('',(#2451),#880,.T.) ;
#30931 = ADVANCED_FACE('',(#2452,#1050),#1760,.F.) ;
#30932 = ADVANCED_FACE('',(#2453),#881,.T.) ;
#30933 = ADVANCED_FACE('',(#2454),#882,.F.) ;
#30934 = ADVANCED_FACE('',(#2455),#30052,.F.) ;
#30935 = ADVANCED_FACE('',(#2456),#30053,.F.) ;
#30936 = ADVANCED_FACE('',(#2457),#30054,.F.) ;
#30937 = ADVANCED_FACE('',(#2458),#1761,.T.) ;
#30938 = ADVANCED_FACE('',(#2459),#1762,.T.) ;
#30939 = ADVANCED_FACE('',(#2460),#1763,.T.) ;
#30940 = ADVANCED_FACE('',(#2461),#1764,.T.) ;
#30941 = ADVANCED_FACE('',(#2462),#1765,.T.) ;
#30942 = ADVANCED_FACE('',(#2463),#1766,.T.) ;
#30943 = ADVANCED_FACE('',(#2464),#1767,.T.) ;
#30944 = ADVANCED_FACE('',(#2465),#1768,.T.) ;
#30945 = ADVANCED_FACE('',(#2466),#1769,.T.) ;
#30946 = ADVANCED_FACE('',(#2467),#1770,.T.) ;
#30947 = ADVANCED_FACE('',(#2468),#1771,.T.) ;
#30948 = ADVANCED_FACE('',(#2469),#30055,.F.) ;
#30949 = ADVANCED_FACE('',(#2470),#1772,.T.) ;
#30950 = ADVANCED_FACE('',(#2471),#1773,.T.) ;
#30951 = ADVANCED_FACE('',(#2472),#1774,.T.) ;
#30952 = ADVANCED_FACE('',(#2473),#1775,.T.) ;
#30953 = ADVANCED_FACE('',(#2474),#1776,.T.) ;
#30954 = ADVANCED_FACE('',(#2475),#1777,.T.) ;
#30955 = ADVANCED_FACE('',(#2476),#1778,.T.) ;
#30956 = ADVANCED_FACE('',(#2477),#738,.T.) ;
#30957 = ADVANCED_FACE('',(#2478),#739,.T.) ;
#30958 = ADVANCED_FACE('',(#2479),#30056,.F.) ;
#30959 = ADVANCED_FACE('',(#2480),#30057,.F.) ;
#30960 = ADVANCED_FACE('',(#2481),#30058,.F.) ;
#30961 = ADVANCED_FACE('',(#2482),#30059,.F.) ;
#30962 = ADVANCED_FACE('',(#2483),#30060,.F.) ;
#30963 = ADVANCED_FACE('',(#2484),#30061,.F.) ;
#30964 = ADVANCED_FACE('',(#2485),#30062,.F.) ;
#30965 = ADVANCED_FACE('',(#2486),#30063,.F.) ;
#30966 = ADVANCED_FACE('',(#2487),#30064,.F.) ;
#30967 = ADVANCED_FACE('',(#2488),#30065,.F.) ;
#30968 = ADVANCED_FACE('',(#2489),#30066,.F.) ;
#30969 = ADVANCED_FACE('',(#2490),#30067,.F.) ;
#30970 = ADVANCED_FACE('',(#2491),#30068,.F.) ;
#30971 = ADVANCED_FACE('',(#2492),#30069,.F.) ;
#30972 = ADVANCED_FACE('',(#2493),#30070,.F.) ;
#30973 = ADVANCED_FACE('',(#2494),#30071,.F.) ;
#30974 = ADVANCED_FACE('',(#2495),#30072,.F.) ;
#30975 = ADVANCED_FACE('',(#2496),#30073,.F.) ;
#30976 = ADVANCED_FACE('',(#2497),#30074,.F.) ;
#30977 = ADVANCED_FACE('',(#2498),#30075,.F.) ;
#30978 = ADVANCED_FACE('',(#2499),#30076,.F.) ;
#30979 = ADVANCED_FACE('',(#2500),#30077,.F.) ;
#30980 = ADVANCED_FACE('',(#2501),#30078,.F.) ;
#30981 = ADVANCED_FACE('',(#2502),#30079,.F.) ;
#30982 = ADVANCED_FACE('',(#2503),#30080,.F.) ;
#30983 = ADVANCED_FACE('',(#2504),#30081,.F.) ;
#30984 = ADVANCED_FACE('',(#2505),#30082,.F.) ;
#30985 = ADVANCED_FACE('',(#2506),#30083,.F.) ;
#30986 = ADVANCED_FACE('',(#2507),#30084,.F.) ;
#30987 = ADVANCED_FACE('',(#2508),#30085,.F.) ;
#30988 = ADVANCED_FACE('',(#2509),#30086,.F.) ;
#30989 = ADVANCED_FACE('',(#2510),#30087,.F.) ;
#30990 = ADVANCED_FACE('',(#2511),#30088,.F.) ;
#30991 = ADVANCED_FACE('',(#2512),#30089,.F.) ;
#30992 = ADVANCED_FACE('',(#2513),#30090,.F.) ;
#30993 = ADVANCED_FACE('',(#2514),#30091,.F.) ;
#30994 = ADVANCED_FACE('',(#2515),#30092,.F.) ;
#30995 = ADVANCED_FACE('',(#2516),#30093,.F.) ;
#30996 = ADVANCED_FACE('',(#2517),#30094,.F.) ;
#30997 = ADVANCED_FACE('',(#2518),#30095,.F.) ;
#30998 = ADVANCED_FACE('',(#2519),#30096,.F.) ;
#30999 = ADVANCED_FACE('',(#2520),#30097,.F.) ;
#31000 = ADVANCED_FACE('',(#2521),#30098,.F.) ;
#31001 = ADVANCED_FACE('',(#2522),#30099,.F.) ;
#31002 = ADVANCED_FACE('',(#2523),#30100,.F.) ;
#31003 = ADVANCED_FACE('',(#2524),#30101,.F.) ;
#31004 = ADVANCED_FACE('',(#2525),#30102,.F.) ;
#31005 = ADVANCED_FACE('',(#2526),#30103,.F.) ;
#31006 = ADVANCED_FACE('',(#2527),#30104,.F.) ;
#31007 = ADVANCED_FACE('',(#2528),#30105,.F.) ;
#31008 = ADVANCED_FACE('',(#2529),#30106,.F.) ;
#31009 = ADVANCED_FACE('',(#2530),#30107,.F.) ;
#31010 = ADVANCED_FACE('',(#2531),#30108,.F.) ;
#31011 = ADVANCED_FACE('',(#2532),#30109,.F.) ;
#31012 = ADVANCED_FACE('',(#2533),#30110,.F.) ;
#31013 = ADVANCED_FACE('',(#2534),#30111,.F.) ;
#31014 = ADVANCED_FACE('',(#2535),#30112,.F.) ;
#31015 = ADVANCED_FACE('',(#2536),#30113,.F.) ;
#31016 = ADVANCED_FACE('',(#2537),#30114,.F.) ;
#31017 = ADVANCED_FACE('',(#2538),#30115,.F.) ;
#31018 = ADVANCED_FACE('',(#2539),#30116,.F.) ;
#31019 = ADVANCED_FACE('',(#2540),#30117,.F.) ;
#31020 = ADVANCED_FACE('',(#2541),#30118,.F.) ;
#31021 = ADVANCED_FACE('',(#2542),#30119,.F.) ;
#31022 = ADVANCED_FACE('',(#2543),#30120,.F.) ;
#31023 = ADVANCED_FACE('',(#2544),#30121,.T.) ;
#31024 = ADVANCED_FACE('',(#2545),#30122,.T.) ;
#31025 = ADVANCED_FACE('',(#2546),#30123,.T.) ;
#31026 = ADVANCED_FACE('',(#2547),#30124,.T.) ;
#31027 = ADVANCED_FACE('',(#2548),#1779,.T.) ;
#31028 = ADVANCED_FACE('',(#2549),#30125,.T.) ;
#31029 = ADVANCED_FACE('',(#2550),#30126,.F.) ;
#31030 = ADVANCED_FACE('',(#2551,#1051,#1052,#1053,#1054,#1055,#1056,#1057,
#1058),#1780,.T.) ;
#31031 = ADVANCED_FACE('',(#2552),#30127,.F.) ;
#31032 = ADVANCED_FACE('',(#2553,#1059,#1060,#1061,#1062,#1063,#1064,#1065,
#1066,#1067,#1068),#1781,.T.) ;
#31033 = ADVANCED_FACE('',(#2554,#1069,#1070,#1071,#1072,#1073,#1074,#1075,
#1076),#1782,.F.) ;
#31034 = ADVANCED_FACE('',(#2555,#1077,#1078,#1079,#1080,#1081,#1082,#1083,
#1084,#1085,#1086),#1783,.F.) ;
#31035 = ADVANCED_FACE('',(#2556),#1784,.T.) ;
#31036 = ADVANCED_FACE('',(#2557),#1785,.F.) ;
#31037 = ADVANCED_FACE('',(#2558),#30128,.T.) ;
#31038 = ADVANCED_FACE('',(#2559),#30129,.T.) ;
#31039 = ADVANCED_FACE('',(#2560),#30130,.T.) ;
#31040 = ADVANCED_FACE('',(#2561),#30131,.F.) ;
#31041 = ADVANCED_FACE('',(#2562),#1786,.F.) ;
#31042 = ADVANCED_FACE('',(#2563),#1787,.F.) ;
#31043 = ADVANCED_FACE('',(#2564),#1788,.F.) ;
#31044 = ADVANCED_FACE('',(#2565),#905,.T.) ;
#31045 = ADVANCED_FACE('',(#2566),#1789,.T.) ;
#31046 = ADVANCED_FACE('',(#2567),#1790,.F.) ;
#31047 = ADVANCED_FACE('',(#2568),#1791,.T.) ;
#31048 = ADVANCED_FACE('',(#2569),#1792,.T.) ;
#31049 = ADVANCED_FACE('',(#2570),#1793,.T.) ;
#31050 = ADVANCED_FACE('',(#2571),#1794,.T.) ;
#31051 = ADVANCED_FACE('',(#2572),#1795,.T.) ;
#31052 = ADVANCED_FACE('',(#2573),#30132,.F.) ;
#31053 = ADVANCED_FACE('',(#2574),#1796,.T.) ;
#31054 = ADVANCED_FACE('',(#2575),#30133,.F.) ;
#31055 = ADVANCED_FACE('',(#2576),#227,.F.) ;
#31056 = ADVANCED_FACE('',(#2577),#30134,.F.) ;
#31057 = ADVANCED_FACE('',(#2578),#228,.F.) ;
#31058 = ADVANCED_FACE('',(#2579),#30135,.F.) ;
#31059 = ADVANCED_FACE('',(#2580),#1797,.T.) ;
#31060 = ADVANCED_FACE('',(#2581),#30136,.T.) ;
#31061 = ADVANCED_FACE('',(#2582),#1798,.F.) ;
#31062 = ADVANCED_FACE('',(#2583),#30137,.T.) ;
#31063 = ADVANCED_FACE('',(#2584),#1799,.T.) ;
#31064 = ADVANCED_FACE('',(#2585),#30138,.F.) ;
#31065 = ADVANCED_FACE('',(#2586),#229,.F.) ;
#31066 = ADVANCED_FACE('',(#2587),#30139,.F.) ;
#31067 = ADVANCED_FACE('',(#2588),#230,.F.) ;
#31068 = ADVANCED_FACE('',(#2589),#30140,.F.) ;
#31069 = ADVANCED_FACE('',(#2590),#1800,.T.) ;
#31070 = ADVANCED_FACE('',(#2591),#30141,.T.) ;
#31071 = ADVANCED_FACE('',(#2592),#1801,.F.) ;
#31072 = ADVANCED_FACE('',(#2593),#30142,.T.) ;
#31073 = ADVANCED_FACE('',(#2594),#1802,.T.) ;
#31074 = ADVANCED_FACE('',(#2595),#1803,.T.) ;
#31075 = ADVANCED_FACE('',(#2596),#1804,.T.) ;
#31076 = ADVANCED_FACE('',(#2597),#1805,.T.) ;
#31077 = ADVANCED_FACE('',(#2598),#1806,.T.) ;
#31078 = ADVANCED_FACE('',(#2599),#1807,.T.) ;
#31079 = ADVANCED_FACE('',(#2600),#1808,.T.) ;
#31080 = ADVANCED_FACE('',(#2601),#1809,.T.) ;
#31081 = ADVANCED_FACE('',(#2602),#1810,.T.) ;
#31082 = ADVANCED_FACE('',(#2603),#1811,.T.) ;
#31083 = ADVANCED_FACE('',(#2604),#1812,.T.) ;
#31084 = ADVANCED_FACE('',(#2605),#1813,.T.) ;
#31085 = ADVANCED_FACE('',(#2606),#1814,.T.) ;
#31086 = ADVANCED_FACE('',(#2607),#1815,.F.) ;
#31087 = ADVANCED_FACE('',(#2608),#1816,.F.) ;
#31088 = ADVANCED_FACE('',(#2609),#30143,.F.) ;
#31089 = ADVANCED_FACE('',(#2610),#30144,.F.) ;
#31090 = ADVANCED_FACE('',(#2611),#30145,.F.) ;
#31091 = ADVANCED_FACE('',(#2612),#30146,.F.) ;
#31092 = ADVANCED_FACE('',(#2613),#30147,.F.) ;
#31093 = ADVANCED_FACE('',(#2614),#1817,.F.) ;
#31094 = ADVANCED_FACE('',(#2615),#883,.F.) ;
#31095 = ADVANCED_FACE('',(#2616),#30148,.F.) ;
#31096 = ADVANCED_FACE('',(#2617),#884,.F.) ;
#31097 = ADVANCED_FACE('',(#2618),#30149,.F.) ;
#31098 = ADVANCED_FACE('',(#2619),#885,.F.) ;
#31099 = ADVANCED_FACE('',(#2620),#30150,.F.) ;
#31100 = ADVANCED_FACE('',(#2621),#1818,.F.) ;
#31101 = ADVANCED_FACE('',(#2622),#1819,.F.) ;
#31102 = ADVANCED_FACE('',(#2623),#30151,.F.) ;
#31103 = ADVANCED_FACE('',(#2624),#886,.F.) ;
#31104 = ADVANCED_FACE('',(#2625),#30152,.F.) ;
#31105 = ADVANCED_FACE('',(#2626),#30153,.F.) ;
#31106 = ADVANCED_FACE('',(#2627),#30154,.F.) ;
#31107 = ADVANCED_FACE('',(#2628),#30155,.F.) ;
#31108 = ADVANCED_FACE('',(#2629),#30156,.F.) ;
#31109 = ADVANCED_FACE('',(#2630),#30157,.F.) ;
#31110 = ADVANCED_FACE('',(#2631),#231,.T.) ;
#31111 = ADVANCED_FACE('',(#2632),#30158,.T.) ;
#31112 = ADVANCED_FACE('',(#2633),#30159,.F.) ;
#31113 = ADVANCED_FACE('',(#2634),#30160,.F.) ;
#31114 = ADVANCED_FACE('',(#2635),#30161,.F.) ;
#31115 = ADVANCED_FACE('',(#2636),#1820,.F.) ;
#31116 = ADVANCED_FACE('',(#2637),#30162,.F.) ;
#31117 = ADVANCED_FACE('',(#2638),#1821,.F.) ;
#31118 = ADVANCED_FACE('',(#2639),#1822,.F.) ;
#31119 = ADVANCED_FACE('',(#2640),#1823,.F.) ;
#31120 = ADVANCED_FACE('',(#2641),#1824,.F.) ;
#31121 = ADVANCED_FACE('',(#2642),#1825,.F.) ;
#31122 = ADVANCED_FACE('',(#2643),#1826,.F.) ;
#31123 = ADVANCED_FACE('',(#2644),#1827,.F.) ;
#31124 = ADVANCED_FACE('',(#2645),#1828,.F.) ;
#31125 = ADVANCED_FACE('',(#2646),#1829,.F.) ;
#31126 = ADVANCED_FACE('',(#2647),#1830,.F.) ;
#31127 = ADVANCED_FACE('',(#2648),#1831,.F.) ;
#31128 = ADVANCED_FACE('',(#2649),#1832,.F.) ;
#31129 = ADVANCED_FACE('',(#2650),#1833,.F.) ;
#31130 = ADVANCED_FACE('',(#2651),#1834,.F.) ;
#31131 = ADVANCED_FACE('',(#2652),#1835,.F.) ;
#31132 = ADVANCED_FACE('',(#2653),#1836,.F.) ;
#31133 = ADVANCED_FACE('',(#2654),#1837,.F.) ;
#31134 = ADVANCED_FACE('',(#2655),#1838,.F.) ;
#31135 = ADVANCED_FACE('',(#2656),#1839,.T.) ;
#31136 = ADVANCED_FACE('',(#2657),#30163,.T.) ;
#31137 = ADVANCED_FACE('',(#2658),#30164,.T.) ;
#31138 = ADVANCED_FACE('',(#2659),#1840,.T.) ;
#31139 = ADVANCED_FACE('',(#2660),#30165,.T.) ;
#31140 = ADVANCED_FACE('',(#2661),#30166,.T.) ;
#31141 = ADVANCED_FACE('',(#2662),#232,.T.) ;
#31142 = ADVANCED_FACE('',(#2663),#30167,.T.) ;
#31143 = ADVANCED_FACE('',(#2664),#1841,.F.) ;
#31144 = ADVANCED_FACE('',(#2665),#1842,.F.) ;
#31145 = ADVANCED_FACE('',(#2666),#1843,.F.) ;
#31146 = ADVANCED_FACE('',(#2667),#1844,.F.) ;
#31147 = ADVANCED_FACE('',(#2668,#1087,#1088,#1089,#1090),#1845,.F.) ;
#31148 = ADVANCED_FACE('',(#2669),#1846,.T.) ;
#31149 = ADVANCED_FACE('',(#2670),#30168,.F.) ;
#31150 = ADVANCED_FACE('',(#2671),#887,.F.) ;
#31151 = ADVANCED_FACE('',(#2672),#30169,.F.) ;
#31152 = ADVANCED_FACE('',(#2673),#888,.F.) ;
#31153 = ADVANCED_FACE('',(#2674),#30170,.F.) ;
#31154 = ADVANCED_FACE('',(#2675),#889,.F.) ;
#31155 = ADVANCED_FACE('',(#2676),#30171,.F.) ;
#31156 = ADVANCED_FACE('',(#2677),#890,.F.) ;
#31157 = ADVANCED_FACE('',(#2678),#1847,.F.) ;
#31158 = ADVANCED_FACE('',(#2679),#1848,.F.) ;
#31159 = ADVANCED_FACE('',(#2680),#1849,.F.) ;
#31160 = ADVANCED_FACE('',(#2681),#1850,.T.) ;
#31161 = ADVANCED_FACE('',(#2682),#1851,.F.) ;
#31162 = ADVANCED_FACE('',(#2683),#1852,.F.) ;
#31163 = ADVANCED_FACE('',(#2684),#1853,.F.) ;
#31164 = ADVANCED_FACE('',(#2685),#1854,.F.) ;
#31165 = ADVANCED_FACE('',(#2686),#1855,.F.) ;
#31166 = ADVANCED_FACE('',(#2687),#1856,.F.) ;
#31167 = ADVANCED_FACE('',(#2688),#30172,.F.) ;
#31168 = ADVANCED_FACE('',(#2689),#30173,.F.) ;
#31169 = ADVANCED_FACE('',(#2690),#1857,.F.) ;
#31170 = ADVANCED_FACE('',(#2691),#1858,.F.) ;
#31171 = ADVANCED_FACE('',(#2692),#1859,.F.) ;
#31172 = ADVANCED_FACE('',(#2693),#1860,.F.) ;
#31173 = ADVANCED_FACE('',(#2694),#1861,.F.) ;
#31174 = ADVANCED_FACE('',(#2695),#1862,.F.) ;
#31175 = ADVANCED_FACE('',(#2696),#1863,.F.) ;
#31176 = ADVANCED_FACE('',(#2697),#1864,.F.) ;
#31177 = ADVANCED_FACE('',(#2698),#1865,.F.) ;
#31178 = ADVANCED_FACE('',(#2699),#1866,.F.) ;
#31179 = ADVANCED_FACE('',(#2700),#233,.T.) ;
#31180 = ADVANCED_FACE('',(#2701),#30174,.T.) ;
#31181 = ADVANCED_FACE('',(#2702),#234,.T.) ;
#31182 = ADVANCED_FACE('',(#2703),#30175,.T.) ;
#31183 = ADVANCED_FACE('',(#2704),#1867,.T.) ;
#31184 = ADVANCED_FACE('',(#2705),#30176,.T.) ;
#31185 = ADVANCED_FACE('',(#2706),#1868,.F.) ;
#31186 = ADVANCED_FACE('',(#2707),#30177,.T.) ;
#31187 = ADVANCED_FACE('',(#2708),#30178,.T.) ;
#31188 = ADVANCED_FACE('',(#2709,#1091),#1869,.F.) ;
#31189 = ADVANCED_FACE('',(#2710),#30179,.F.) ;
#31190 = ADVANCED_FACE('',(#2711),#891,.F.) ;
#31191 = ADVANCED_FACE('',(#2712),#906,.F.) ;
#31192 = ADVANCED_FACE('',(#2713),#907,.F.) ;
#31193 = ADVANCED_FACE('',(#2714),#908,.F.) ;
#31194 = ADVANCED_FACE('',(#2715),#909,.F.) ;
#31195 = ADVANCED_FACE('',(#2716),#910,.F.) ;
#31196 = ADVANCED_FACE('',(#2717),#911,.F.) ;
#31197 = ADVANCED_FACE('',(#2718),#912,.F.) ;
#31198 = ADVANCED_FACE('',(#2719),#913,.F.) ;
#31199 = ADVANCED_FACE('',(#2720),#1870,.F.) ;
#31200 = ADVANCED_FACE('',(#2721),#1871,.F.) ;
#31201 = ADVANCED_FACE('',(#2722),#1872,.F.) ;
#31202 = ADVANCED_FACE('',(#2723),#1873,.F.) ;
#31203 = ADVANCED_FACE('',(#2724),#30180,.F.) ;
#31204 = ADVANCED_FACE('',(#2725),#30181,.F.) ;
#31205 = ADVANCED_FACE('',(#2726),#30182,.T.) ;
#31206 = ADVANCED_FACE('',(#2727),#30183,.F.) ;
#31207 = ADVANCED_FACE('',(#2728),#30184,.T.) ;
#31208 = ADVANCED_FACE('',(#2729),#30185,.F.) ;
#31209 = ADVANCED_FACE('',(#2730),#30186,.T.) ;
#31210 = ADVANCED_FACE('',(#2731),#235,.T.) ;
#31211 = ADVANCED_FACE('',(#2732),#30187,.T.) ;
#31212 = ADVANCED_FACE('',(#2733),#236,.T.) ;
#31213 = ADVANCED_FACE('',(#2734),#237,.T.) ;
#31214 = ADVANCED_FACE('',(#2735),#238,.T.) ;
#31215 = ADVANCED_FACE('',(#2736),#1874,.T.) ;
#31216 = ADVANCED_FACE('',(#2737),#1875,.F.) ;
#31217 = ADVANCED_FACE('',(#2738),#30188,.T.) ;
#31218 = ADVANCED_FACE('',(#2739),#1876,.F.) ;
#31219 = ADVANCED_FACE('',(#2740),#30189,.T.) ;
#31220 = ADVANCED_FACE('',(#2741),#30190,.T.) ;
#31221 = ADVANCED_FACE('',(#2742),#30191,.T.) ;
#31222 = ADVANCED_FACE('',(#2743,#1092,#1093,#1094,#1095),#1877,.T.) ;
#31223 = ADVANCED_FACE('',(#2744),#740,.F.) ;
#31224 = ADVANCED_FACE('',(#2745),#30192,.T.) ;
#31225 = ADVANCED_FACE('',(#2746),#741,.F.) ;
#31226 = ADVANCED_FACE('',(#2747,#1096),#1878,.T.) ;
#31227 = ADVANCED_FACE('',(#2748),#30193,.T.) ;
#31228 = ADVANCED_FACE('',(#2749),#742,.F.) ;
#31229 = ADVANCED_FACE('',(#2750),#30194,.T.) ;
#31230 = ADVANCED_FACE('',(#2751),#743,.F.) ;
#31231 = ADVANCED_FACE('',(#2752),#914,.F.) ;
#31232 = ADVANCED_FACE('',(#2753),#915,.F.) ;
#31233 = ADVANCED_FACE('',(#2754),#916,.F.) ;
#31234 = ADVANCED_FACE('',(#2755),#917,.F.) ;
#31235 = ADVANCED_FACE('',(#2756),#918,.F.) ;
#31236 = ADVANCED_FACE('',(#2757),#919,.F.) ;
#31237 = ADVANCED_FACE('',(#2758,#1097,#1098,#1099,#1100,#1101,#1102,#1103,
#1104,#1105),#1879,.F.) ;
#31238 = ADVANCED_FACE('',(#2759),#920,.F.) ;
#31239 = ADVANCED_FACE('',(#2760),#921,.F.) ;
#31240 = ADVANCED_FACE('',(#2761),#1880,.T.) ;
#31241 = ADVANCED_FACE('',(#2762),#1881,.T.) ;
#31242 = ADVANCED_FACE('',(#2763),#1882,.T.) ;
#31243 = ADVANCED_FACE('',(#2764),#1883,.T.) ;
#31244 = ADVANCED_FACE('',(#2765),#1884,.T.) ;
#31245 = ADVANCED_FACE('',(#2766),#1885,.T.) ;
#31246 = ADVANCED_FACE('',(#2767),#1886,.T.) ;
#31247 = ADVANCED_FACE('',(#2768),#1887,.T.) ;
#31248 = ADVANCED_FACE('',(#2769),#1888,.T.) ;
#31249 = ADVANCED_FACE('',(#2770),#1889,.T.) ;
#31250 = ADVANCED_FACE('',(#2771),#1890,.T.) ;
#31251 = ADVANCED_FACE('',(#2772),#1891,.T.) ;
#31252 = ADVANCED_FACE('',(#2773,#1106,#1107,#1108,#1109,#1110,#1111,#1112,
#1113,#1114),#1892,.T.) ;
#31253 = ADVANCED_FACE('',(#2774),#1893,.T.) ;
#31254 = ADVANCED_FACE('',(#2775),#1894,.T.) ;
#31255 = ADVANCED_FACE('',(#2776),#1895,.T.) ;
#31256 = ADVANCED_FACE('',(#2777),#1896,.T.) ;
#31257 = ADVANCED_FACE('',(#2778),#1897,.T.) ;
#31258 = ADVANCED_FACE('',(#2779),#1898,.T.) ;
#31259 = ADVANCED_FACE('',(#2780),#1899,.F.) ;
#31260 = ADVANCED_FACE('',(#2781),#1900,.F.) ;
#31261 = ADVANCED_FACE('',(#2782),#1901,.F.) ;
#31262 = ADVANCED_FACE('',(#2783),#1902,.F.) ;
#31263 = ADVANCED_FACE('',(#2784),#1903,.F.) ;
#31264 = ADVANCED_FACE('',(#2785),#1904,.F.) ;
#31265 = ADVANCED_FACE('',(#2786),#1905,.F.) ;
#31266 = ADVANCED_FACE('',(#2787),#1906,.F.) ;
#31267 = ADVANCED_FACE('',(#2788),#1907,.F.) ;
#31268 = ADVANCED_FACE('',(#2789),#1908,.F.) ;
#31269 = ADVANCED_FACE('',(#2790),#1909,.F.) ;
#31270 = ADVANCED_FACE('',(#2791),#1910,.F.) ;
#31271 = ADVANCED_FACE('',(#2792),#1911,.F.) ;
#31272 = ADVANCED_FACE('',(#2793),#1912,.F.) ;
#31273 = ADVANCED_FACE('',(#2794),#1913,.F.) ;
#31274 = ADVANCED_FACE('',(#2795),#1914,.F.) ;
#31275 = ADVANCED_FACE('',(#2796),#1915,.F.) ;
#31276 = ADVANCED_FACE('',(#2797),#1916,.F.) ;
#31277 = ADVANCED_FACE('',(#2798),#1917,.F.) ;
#31278 = ADVANCED_FACE('',(#2799),#1918,.F.) ;
#31279 = ADVANCED_FACE('',(#2800),#1919,.F.) ;
#31280 = ADVANCED_FACE('',(#2801),#1920,.F.) ;
#31281 = ADVANCED_FACE('',(#2802),#1921,.F.) ;
#31282 = ADVANCED_FACE('',(#2803),#1922,.F.) ;
#31283 = ADVANCED_FACE('',(#2804),#1923,.F.) ;
#31284 = ADVANCED_FACE('',(#2805),#1924,.F.) ;
#31285 = ADVANCED_FACE('',(#2806),#1925,.F.) ;
#31286 = ADVANCED_FACE('',(#2807),#1926,.F.) ;
#31287 = ADVANCED_FACE('',(#2808),#1927,.F.) ;
#31288 = ADVANCED_FACE('',(#2809),#1928,.F.) ;
#31289 = ADVANCED_FACE('',(#2810),#1929,.F.) ;
#31290 = ADVANCED_FACE('',(#2811),#1930,.F.) ;
#31291 = ADVANCED_FACE('',(#2812),#1931,.F.) ;
#31292 = ADVANCED_FACE('',(#2813),#1932,.F.) ;
#31293 = ADVANCED_FACE('',(#2814),#1933,.F.) ;
#31294 = ADVANCED_FACE('',(#2815),#1934,.F.) ;
#31295 = ADVANCED_FACE('',(#2816),#1935,.T.) ;
#31296 = ADVANCED_FACE('',(#2817),#239,.T.) ;
#31297 = ADVANCED_FACE('',(#2818),#30195,.F.) ;
#31298 = ADVANCED_FACE('',(#2819,#1115,#1116),#1936,.T.) ;
#31299 = ADVANCED_FACE('',(#2820),#240,.T.) ;
#31300 = ADVANCED_FACE('',(#2821),#30196,.F.) ;
#31301 = ADVANCED_FACE('',(#2822,#1117,#1118),#1937,.T.) ;
#31302 = ADVANCED_FACE('',(#2823),#241,.T.) ;
#31303 = ADVANCED_FACE('',(#2824),#30197,.F.) ;
#31304 = ADVANCED_FACE('',(#2825,#1119,#1120),#1938,.T.) ;
#31305 = ADVANCED_FACE('',(#2826),#242,.T.) ;
#31306 = ADVANCED_FACE('',(#2827),#30198,.F.) ;
#31307 = ADVANCED_FACE('',(#2828,#1121,#1122),#1939,.T.) ;
#31308 = ADVANCED_FACE('',(#2829),#243,.T.) ;
#31309 = ADVANCED_FACE('',(#2830),#30199,.F.) ;
#31310 = ADVANCED_FACE('',(#2831,#1123,#1124),#1940,.T.) ;
#31311 = ADVANCED_FACE('',(#2832),#244,.T.) ;
#31312 = ADVANCED_FACE('',(#2833),#30200,.F.) ;
#31313 = ADVANCED_FACE('',(#2834,#1125,#1126),#1941,.T.) ;
#31314 = ADVANCED_FACE('',(#2835),#245,.T.) ;
#31315 = ADVANCED_FACE('',(#2836),#30201,.F.) ;
#31316 = ADVANCED_FACE('',(#2837,#1127,#1128),#1942,.T.) ;
#31317 = ADVANCED_FACE('',(#2838),#246,.T.) ;
#31318 = ADVANCED_FACE('',(#2839),#30202,.F.) ;
#31319 = ADVANCED_FACE('',(#2840,#1129,#1130),#1943,.T.) ;
#31320 = ADVANCED_FACE('',(#2841),#247,.T.) ;
#31321 = ADVANCED_FACE('',(#2842,#1131,#1132),#1944,.T.) ;
#31322 = ADVANCED_FACE('',(#2843),#30203,.F.) ;
#31323 = ADVANCED_FACE('',(#2844,#1133),#1945,.F.) ;
#31324 = ADVANCED_FACE('',(#2845,#1134),#1946,.F.) ;
#31325 = ADVANCED_FACE('',(#2846,#1135),#1947,.F.) ;
#31326 = ADVANCED_FACE('',(#2847,#1136),#1948,.F.) ;
#31327 = ADVANCED_FACE('',(#2848,#1137),#1949,.F.) ;
#31328 = ADVANCED_FACE('',(#2849,#1138),#1950,.F.) ;
#31329 = ADVANCED_FACE('',(#2850,#1139),#1951,.F.) ;
#31330 = ADVANCED_FACE('',(#2851,#1140),#1952,.F.) ;
#31331 = ADVANCED_FACE('',(#2852),#30204,.T.) ;
#31332 = ADVANCED_FACE('',(#2853),#248,.T.) ;
#31333 = ADVANCED_FACE('',(#2854),#30205,.T.) ;
#31334 = ADVANCED_FACE('',(#2855),#249,.T.) ;
#31335 = ADVANCED_FACE('',(#2856),#30206,.T.) ;
#31336 = ADVANCED_FACE('',(#2857),#250,.T.) ;
#31337 = ADVANCED_FACE('',(#2858),#30207,.T.) ;
#31338 = ADVANCED_FACE('',(#2859),#251,.T.) ;
#31339 = ADVANCED_FACE('',(#2860),#30208,.F.) ;
#31340 = ADVANCED_FACE('',(#2861),#1953,.F.) ;
#31341 = ADVANCED_FACE('',(#2862),#30209,.F.) ;
#31342 = ADVANCED_FACE('',(#2863),#1954,.F.) ;
#31343 = ADVANCED_FACE('',(#2864),#30210,.T.) ;
#31344 = ADVANCED_FACE('',(#2865),#252,.T.) ;
#31345 = ADVANCED_FACE('',(#2866),#30211,.T.) ;
#31346 = ADVANCED_FACE('',(#2867),#253,.T.) ;
#31347 = ADVANCED_FACE('',(#2868),#30212,.T.) ;
#31348 = ADVANCED_FACE('',(#2869),#254,.T.) ;
#31349 = ADVANCED_FACE('',(#2870),#30213,.T.) ;
#31350 = ADVANCED_FACE('',(#2871),#255,.T.) ;
#31351 = ADVANCED_FACE('',(#2872),#30214,.F.) ;
#31352 = ADVANCED_FACE('',(#2873),#1955,.F.) ;
#31353 = ADVANCED_FACE('',(#2874),#30215,.F.) ;
#31354 = ADVANCED_FACE('',(#2875),#1956,.F.) ;
#31355 = ADVANCED_FACE('',(#2876),#30216,.T.) ;
#31356 = ADVANCED_FACE('',(#2877),#256,.T.) ;
#31357 = ADVANCED_FACE('',(#2878),#30217,.T.) ;
#31358 = ADVANCED_FACE('',(#2879),#257,.T.) ;
#31359 = ADVANCED_FACE('',(#2880),#30218,.T.) ;
#31360 = ADVANCED_FACE('',(#2881),#258,.T.) ;
#31361 = ADVANCED_FACE('',(#2882),#30219,.T.) ;
#31362 = ADVANCED_FACE('',(#2883),#259,.T.) ;
#31363 = ADVANCED_FACE('',(#2884),#30220,.F.) ;
#31364 = ADVANCED_FACE('',(#2885),#1957,.F.) ;
#31365 = ADVANCED_FACE('',(#2886),#30221,.F.) ;
#31366 = ADVANCED_FACE('',(#2887),#1958,.F.) ;
#31367 = ADVANCED_FACE('',(#2888),#30222,.T.) ;
#31368 = ADVANCED_FACE('',(#2889),#260,.T.) ;
#31369 = ADVANCED_FACE('',(#2890),#30223,.T.) ;
#31370 = ADVANCED_FACE('',(#2891),#261,.T.) ;
#31371 = ADVANCED_FACE('',(#2892),#30224,.T.) ;
#31372 = ADVANCED_FACE('',(#2893),#262,.T.) ;
#31373 = ADVANCED_FACE('',(#2894),#30225,.T.) ;
#31374 = ADVANCED_FACE('',(#2895),#263,.T.) ;
#31375 = ADVANCED_FACE('',(#2896),#30226,.F.) ;
#31376 = ADVANCED_FACE('',(#2897),#1959,.F.) ;
#31377 = ADVANCED_FACE('',(#2898),#30227,.F.) ;
#31378 = ADVANCED_FACE('',(#2899),#1960,.F.) ;
#31379 = ADVANCED_FACE('',(#2900),#30228,.T.) ;
#31380 = ADVANCED_FACE('',(#2901),#264,.T.) ;
#31381 = ADVANCED_FACE('',(#2902),#30229,.T.) ;
#31382 = ADVANCED_FACE('',(#2903),#265,.T.) ;
#31383 = ADVANCED_FACE('',(#2904),#30230,.T.) ;
#31384 = ADVANCED_FACE('',(#2905),#266,.T.) ;
#31385 = ADVANCED_FACE('',(#2906),#30231,.T.) ;
#31386 = ADVANCED_FACE('',(#2907),#267,.T.) ;
#31387 = ADVANCED_FACE('',(#2908),#30232,.F.) ;
#31388 = ADVANCED_FACE('',(#2909),#1961,.F.) ;
#31389 = ADVANCED_FACE('',(#2910),#30233,.F.) ;
#31390 = ADVANCED_FACE('',(#2911),#1962,.F.) ;
#31391 = ADVANCED_FACE('',(#2912),#30234,.T.) ;
#31392 = ADVANCED_FACE('',(#2913),#268,.T.) ;
#31393 = ADVANCED_FACE('',(#2914),#30235,.T.) ;
#31394 = ADVANCED_FACE('',(#2915),#269,.T.) ;
#31395 = ADVANCED_FACE('',(#2916),#30236,.T.) ;
#31396 = ADVANCED_FACE('',(#2917),#270,.T.) ;
#31397 = ADVANCED_FACE('',(#2918),#30237,.T.) ;
#31398 = ADVANCED_FACE('',(#2919),#271,.T.) ;
#31399 = ADVANCED_FACE('',(#2920),#30238,.F.) ;
#31400 = ADVANCED_FACE('',(#2921),#1963,.F.) ;
#31401 = ADVANCED_FACE('',(#2922),#30239,.F.) ;
#31402 = ADVANCED_FACE('',(#2923),#1964,.F.) ;
#31403 = ADVANCED_FACE('',(#2924),#30240,.T.) ;
#31404 = ADVANCED_FACE('',(#2925),#272,.T.) ;
#31405 = ADVANCED_FACE('',(#2926),#30241,.T.) ;
#31406 = ADVANCED_FACE('',(#2927),#273,.T.) ;
#31407 = ADVANCED_FACE('',(#2928),#30242,.T.) ;
#31408 = ADVANCED_FACE('',(#2929),#274,.T.) ;
#31409 = ADVANCED_FACE('',(#2930),#30243,.T.) ;
#31410 = ADVANCED_FACE('',(#2931),#275,.T.) ;
#31411 = ADVANCED_FACE('',(#2932),#30244,.F.) ;
#31412 = ADVANCED_FACE('',(#2933),#1965,.F.) ;
#31413 = ADVANCED_FACE('',(#2934),#30245,.F.) ;
#31414 = ADVANCED_FACE('',(#2935),#1966,.F.) ;
#31415 = ADVANCED_FACE('',(#2936),#30246,.T.) ;
#31416 = ADVANCED_FACE('',(#2937),#276,.T.) ;
#31417 = ADVANCED_FACE('',(#2938),#30247,.T.) ;
#31418 = ADVANCED_FACE('',(#2939),#277,.T.) ;
#31419 = ADVANCED_FACE('',(#2940),#30248,.T.) ;
#31420 = ADVANCED_FACE('',(#2941),#278,.T.) ;
#31421 = ADVANCED_FACE('',(#2942),#30249,.T.) ;
#31422 = ADVANCED_FACE('',(#2943),#279,.T.) ;
#31423 = ADVANCED_FACE('',(#2944),#30250,.F.) ;
#31424 = ADVANCED_FACE('',(#2945),#1967,.F.) ;
#31425 = ADVANCED_FACE('',(#2946),#30251,.F.) ;
#31426 = ADVANCED_FACE('',(#2947),#1968,.F.) ;
#31427 = ADVANCED_FACE('',(#2948),#30252,.T.) ;
#31428 = ADVANCED_FACE('',(#2949),#280,.T.) ;
#31429 = ADVANCED_FACE('',(#2950),#30253,.T.) ;
#31430 = ADVANCED_FACE('',(#2951),#281,.T.) ;
#31431 = ADVANCED_FACE('',(#2952),#30254,.T.) ;
#31432 = ADVANCED_FACE('',(#2953),#282,.T.) ;
#31433 = ADVANCED_FACE('',(#2954),#30255,.T.) ;
#31434 = ADVANCED_FACE('',(#2955),#283,.T.) ;
#31435 = ADVANCED_FACE('',(#2956),#30256,.F.) ;
#31436 = ADVANCED_FACE('',(#2957),#1969,.F.) ;
#31437 = ADVANCED_FACE('',(#2958),#30257,.F.) ;
#31438 = ADVANCED_FACE('',(#2959),#1970,.F.) ;
#31439 = ADVANCED_FACE('',(#2960),#30258,.T.) ;
#31440 = ADVANCED_FACE('',(#2961),#284,.T.) ;
#31441 = ADVANCED_FACE('',(#2962),#30259,.T.) ;
#31442 = ADVANCED_FACE('',(#2963),#285,.T.) ;
#31443 = ADVANCED_FACE('',(#2964),#30260,.T.) ;
#31444 = ADVANCED_FACE('',(#2965),#286,.T.) ;
#31445 = ADVANCED_FACE('',(#2966),#30261,.T.) ;
#31446 = ADVANCED_FACE('',(#2967),#287,.T.) ;
#31447 = ADVANCED_FACE('',(#2968),#30262,.F.) ;
#31448 = ADVANCED_FACE('',(#2969),#1971,.F.) ;
#31449 = ADVANCED_FACE('',(#2970),#30263,.F.) ;
#31450 = ADVANCED_FACE('',(#2971),#1972,.F.) ;
#31451 = ADVANCED_FACE('',(#2972),#30264,.T.) ;
#31452 = ADVANCED_FACE('',(#2973),#288,.T.) ;
#31453 = ADVANCED_FACE('',(#2974),#30265,.T.) ;
#31454 = ADVANCED_FACE('',(#2975),#289,.T.) ;
#31455 = ADVANCED_FACE('',(#2976),#30266,.T.) ;
#31456 = ADVANCED_FACE('',(#2977),#290,.T.) ;
#31457 = ADVANCED_FACE('',(#2978),#30267,.T.) ;
#31458 = ADVANCED_FACE('',(#2979),#291,.T.) ;
#31459 = ADVANCED_FACE('',(#2980),#30268,.F.) ;
#31460 = ADVANCED_FACE('',(#2981),#1973,.F.) ;
#31461 = ADVANCED_FACE('',(#2982),#30269,.F.) ;
#31462 = ADVANCED_FACE('',(#2983),#1974,.F.) ;
#31463 = ADVANCED_FACE('',(#2984),#30270,.T.) ;
#31464 = ADVANCED_FACE('',(#2985),#292,.T.) ;
#31465 = ADVANCED_FACE('',(#2986),#30271,.T.) ;
#31466 = ADVANCED_FACE('',(#2987),#293,.T.) ;
#31467 = ADVANCED_FACE('',(#2988),#30272,.T.) ;
#31468 = ADVANCED_FACE('',(#2989),#294,.T.) ;
#31469 = ADVANCED_FACE('',(#2990),#30273,.T.) ;
#31470 = ADVANCED_FACE('',(#2991),#295,.T.) ;
#31471 = ADVANCED_FACE('',(#2992),#30274,.F.) ;
#31472 = ADVANCED_FACE('',(#2993),#1975,.F.) ;
#31473 = ADVANCED_FACE('',(#2994),#30275,.F.) ;
#31474 = ADVANCED_FACE('',(#2995),#1976,.F.) ;
#31475 = ADVANCED_FACE('',(#2996),#30276,.T.) ;
#31476 = ADVANCED_FACE('',(#2997),#296,.T.) ;
#31477 = ADVANCED_FACE('',(#2998),#30277,.T.) ;
#31478 = ADVANCED_FACE('',(#2999),#297,.T.) ;
#31479 = ADVANCED_FACE('',(#3000),#30278,.T.) ;
#31480 = ADVANCED_FACE('',(#3001),#298,.T.) ;
#31481 = ADVANCED_FACE('',(#3002),#30279,.T.) ;
#31482 = ADVANCED_FACE('',(#3003),#299,.T.) ;
#31483 = ADVANCED_FACE('',(#3004),#30280,.F.) ;
#31484 = ADVANCED_FACE('',(#3005),#1977,.F.) ;
#31485 = ADVANCED_FACE('',(#3006),#30281,.F.) ;
#31486 = ADVANCED_FACE('',(#3007),#1978,.F.) ;
#31487 = ADVANCED_FACE('',(#3008),#30282,.T.) ;
#31488 = ADVANCED_FACE('',(#3009),#300,.T.) ;
#31489 = ADVANCED_FACE('',(#3010),#30283,.T.) ;
#31490 = ADVANCED_FACE('',(#3011),#301,.T.) ;
#31491 = ADVANCED_FACE('',(#3012),#30284,.T.) ;
#31492 = ADVANCED_FACE('',(#3013),#302,.T.) ;
#31493 = ADVANCED_FACE('',(#3014),#30285,.T.) ;
#31494 = ADVANCED_FACE('',(#3015),#303,.T.) ;
#31495 = ADVANCED_FACE('',(#3016),#30286,.F.) ;
#31496 = ADVANCED_FACE('',(#3017),#1979,.F.) ;
#31497 = ADVANCED_FACE('',(#3018),#30287,.F.) ;
#31498 = ADVANCED_FACE('',(#3019),#1980,.F.) ;
#31499 = ADVANCED_FACE('',(#3020),#30288,.T.) ;
#31500 = ADVANCED_FACE('',(#3021),#304,.T.) ;
#31501 = ADVANCED_FACE('',(#3022),#30289,.T.) ;
#31502 = ADVANCED_FACE('',(#3023),#305,.T.) ;
#31503 = ADVANCED_FACE('',(#3024),#30290,.T.) ;
#31504 = ADVANCED_FACE('',(#3025),#306,.T.) ;
#31505 = ADVANCED_FACE('',(#3026),#30291,.T.) ;
#31506 = ADVANCED_FACE('',(#3027),#307,.T.) ;
#31507 = ADVANCED_FACE('',(#3028),#30292,.F.) ;
#31508 = ADVANCED_FACE('',(#3029),#1981,.F.) ;
#31509 = ADVANCED_FACE('',(#3030),#30293,.F.) ;
#31510 = ADVANCED_FACE('',(#3031),#1982,.F.) ;
#31511 = ADVANCED_FACE('',(#3032),#30294,.T.) ;
#31512 = ADVANCED_FACE('',(#3033),#308,.T.) ;
#31513 = ADVANCED_FACE('',(#3034),#30295,.T.) ;
#31514 = ADVANCED_FACE('',(#3035),#309,.T.) ;
#31515 = ADVANCED_FACE('',(#3036),#30296,.T.) ;
#31516 = ADVANCED_FACE('',(#3037),#310,.T.) ;
#31517 = ADVANCED_FACE('',(#3038),#30297,.T.) ;
#31518 = ADVANCED_FACE('',(#3039),#311,.T.) ;
#31519 = ADVANCED_FACE('',(#3040),#30298,.F.) ;
#31520 = ADVANCED_FACE('',(#3041),#1983,.F.) ;
#31521 = ADVANCED_FACE('',(#3042),#30299,.F.) ;
#31522 = ADVANCED_FACE('',(#3043),#1984,.F.) ;
#31523 = ADVANCED_FACE('',(#3044),#30300,.T.) ;
#31524 = ADVANCED_FACE('',(#3045),#312,.T.) ;
#31525 = ADVANCED_FACE('',(#3046),#30301,.T.) ;
#31526 = ADVANCED_FACE('',(#3047),#313,.T.) ;
#31527 = ADVANCED_FACE('',(#3048),#30302,.T.) ;
#31528 = ADVANCED_FACE('',(#3049),#314,.T.) ;
#31529 = ADVANCED_FACE('',(#3050),#30303,.T.) ;
#31530 = ADVANCED_FACE('',(#3051),#315,.T.) ;
#31531 = ADVANCED_FACE('',(#3052),#30304,.F.) ;
#31532 = ADVANCED_FACE('',(#3053),#1985,.F.) ;
#31533 = ADVANCED_FACE('',(#3054),#30305,.F.) ;
#31534 = ADVANCED_FACE('',(#3055),#1986,.F.) ;
#31535 = ADVANCED_FACE('',(#3056),#30306,.T.) ;
#31536 = ADVANCED_FACE('',(#3057),#316,.T.) ;
#31537 = ADVANCED_FACE('',(#3058),#30307,.T.) ;
#31538 = ADVANCED_FACE('',(#3059),#317,.T.) ;
#31539 = ADVANCED_FACE('',(#3060),#30308,.T.) ;
#31540 = ADVANCED_FACE('',(#3061),#318,.T.) ;
#31541 = ADVANCED_FACE('',(#3062),#30309,.T.) ;
#31542 = ADVANCED_FACE('',(#3063),#319,.T.) ;
#31543 = ADVANCED_FACE('',(#3064),#30310,.F.) ;
#31544 = ADVANCED_FACE('',(#3065),#1987,.F.) ;
#31545 = ADVANCED_FACE('',(#3066),#30311,.F.) ;
#31546 = ADVANCED_FACE('',(#3067),#1988,.F.) ;
#31547 = ADVANCED_FACE('',(#3068),#30312,.T.) ;
#31548 = ADVANCED_FACE('',(#3069),#320,.T.) ;
#31549 = ADVANCED_FACE('',(#3070),#30313,.T.) ;
#31550 = ADVANCED_FACE('',(#3071),#321,.T.) ;
#31551 = ADVANCED_FACE('',(#3072),#30314,.T.) ;
#31552 = ADVANCED_FACE('',(#3073),#322,.T.) ;
#31553 = ADVANCED_FACE('',(#3074),#30315,.T.) ;
#31554 = ADVANCED_FACE('',(#3075),#323,.T.) ;
#31555 = ADVANCED_FACE('',(#3076),#30316,.F.) ;
#31556 = ADVANCED_FACE('',(#3077),#1989,.F.) ;
#31557 = ADVANCED_FACE('',(#3078),#30317,.F.) ;
#31558 = ADVANCED_FACE('',(#3079),#1990,.F.) ;
#31559 = ADVANCED_FACE('',(#3080),#30318,.T.) ;
#31560 = ADVANCED_FACE('',(#3081),#324,.T.) ;
#31561 = ADVANCED_FACE('',(#3082),#30319,.T.) ;
#31562 = ADVANCED_FACE('',(#3083),#325,.T.) ;
#31563 = ADVANCED_FACE('',(#3084),#30320,.T.) ;
#31564 = ADVANCED_FACE('',(#3085),#326,.T.) ;
#31565 = ADVANCED_FACE('',(#3086),#30321,.T.) ;
#31566 = ADVANCED_FACE('',(#3087),#327,.T.) ;
#31567 = ADVANCED_FACE('',(#3088),#30322,.F.) ;
#31568 = ADVANCED_FACE('',(#3089),#1991,.F.) ;
#31569 = ADVANCED_FACE('',(#3090),#30323,.F.) ;
#31570 = ADVANCED_FACE('',(#3091),#1992,.F.) ;
#31571 = ADVANCED_FACE('',(#3092),#30324,.T.) ;
#31572 = ADVANCED_FACE('',(#3093),#328,.T.) ;
#31573 = ADVANCED_FACE('',(#3094),#30325,.T.) ;
#31574 = ADVANCED_FACE('',(#3095),#329,.T.) ;
#31575 = ADVANCED_FACE('',(#3096),#30326,.T.) ;
#31576 = ADVANCED_FACE('',(#3097),#330,.T.) ;
#31577 = ADVANCED_FACE('',(#3098),#30327,.T.) ;
#31578 = ADVANCED_FACE('',(#3099),#331,.T.) ;
#31579 = ADVANCED_FACE('',(#3100),#30328,.F.) ;
#31580 = ADVANCED_FACE('',(#3101),#1993,.F.) ;
#31581 = ADVANCED_FACE('',(#3102),#30329,.F.) ;
#31582 = ADVANCED_FACE('',(#3103),#1994,.F.) ;
#31583 = ADVANCED_FACE('',(#3104),#30330,.T.) ;
#31584 = ADVANCED_FACE('',(#3105),#332,.T.) ;
#31585 = ADVANCED_FACE('',(#3106),#30331,.T.) ;
#31586 = ADVANCED_FACE('',(#3107),#333,.T.) ;
#31587 = ADVANCED_FACE('',(#3108),#30332,.T.) ;
#31588 = ADVANCED_FACE('',(#3109),#334,.T.) ;
#31589 = ADVANCED_FACE('',(#3110),#30333,.T.) ;
#31590 = ADVANCED_FACE('',(#3111),#335,.T.) ;
#31591 = ADVANCED_FACE('',(#3112),#30334,.F.) ;
#31592 = ADVANCED_FACE('',(#3113),#1995,.F.) ;
#31593 = ADVANCED_FACE('',(#3114),#30335,.F.) ;
#31594 = ADVANCED_FACE('',(#3115),#1996,.F.) ;
#31595 = ADVANCED_FACE('',(#3116),#30336,.T.) ;
#31596 = ADVANCED_FACE('',(#3117),#336,.T.) ;
#31597 = ADVANCED_FACE('',(#3118),#30337,.T.) ;
#31598 = ADVANCED_FACE('',(#3119),#337,.T.) ;
#31599 = ADVANCED_FACE('',(#3120),#30338,.T.) ;
#31600 = ADVANCED_FACE('',(#3121),#338,.T.) ;
#31601 = ADVANCED_FACE('',(#3122),#30339,.T.) ;
#31602 = ADVANCED_FACE('',(#3123),#339,.T.) ;
#31603 = ADVANCED_FACE('',(#3124),#30340,.F.) ;
#31604 = ADVANCED_FACE('',(#3125),#1997,.F.) ;
#31605 = ADVANCED_FACE('',(#3126),#30341,.F.) ;
#31606 = ADVANCED_FACE('',(#3127),#1998,.F.) ;
#31607 = ADVANCED_FACE('',(#3128),#30342,.T.) ;
#31608 = ADVANCED_FACE('',(#3129),#340,.T.) ;
#31609 = ADVANCED_FACE('',(#3130),#30343,.T.) ;
#31610 = ADVANCED_FACE('',(#3131),#341,.T.) ;
#31611 = ADVANCED_FACE('',(#3132),#30344,.T.) ;
#31612 = ADVANCED_FACE('',(#3133),#342,.T.) ;
#31613 = ADVANCED_FACE('',(#3134),#30345,.T.) ;
#31614 = ADVANCED_FACE('',(#3135),#343,.T.) ;
#31615 = ADVANCED_FACE('',(#3136),#30346,.F.) ;
#31616 = ADVANCED_FACE('',(#3137),#1999,.F.) ;
#31617 = ADVANCED_FACE('',(#3138),#30347,.F.) ;
#31618 = ADVANCED_FACE('',(#3139),#2000,.F.) ;
#31619 = ADVANCED_FACE('',(#3140),#30348,.T.) ;
#31620 = ADVANCED_FACE('',(#3141),#344,.T.) ;
#31621 = ADVANCED_FACE('',(#3142),#30349,.T.) ;
#31622 = ADVANCED_FACE('',(#3143),#345,.T.) ;
#31623 = ADVANCED_FACE('',(#3144),#30350,.T.) ;
#31624 = ADVANCED_FACE('',(#3145),#346,.T.) ;
#31625 = ADVANCED_FACE('',(#3146),#30351,.T.) ;
#31626 = ADVANCED_FACE('',(#3147),#347,.T.) ;
#31627 = ADVANCED_FACE('',(#3148),#30352,.F.) ;
#31628 = ADVANCED_FACE('',(#3149),#2001,.F.) ;
#31629 = ADVANCED_FACE('',(#3150),#30353,.F.) ;
#31630 = ADVANCED_FACE('',(#3151),#2002,.F.) ;
#31631 = ADVANCED_FACE('',(#3152),#30354,.T.) ;
#31632 = ADVANCED_FACE('',(#3153),#348,.T.) ;
#31633 = ADVANCED_FACE('',(#3154),#30355,.T.) ;
#31634 = ADVANCED_FACE('',(#3155),#349,.T.) ;
#31635 = ADVANCED_FACE('',(#3156),#30356,.T.) ;
#31636 = ADVANCED_FACE('',(#3157),#350,.T.) ;
#31637 = ADVANCED_FACE('',(#3158),#30357,.T.) ;
#31638 = ADVANCED_FACE('',(#3159),#351,.T.) ;
#31639 = ADVANCED_FACE('',(#3160),#30358,.F.) ;
#31640 = ADVANCED_FACE('',(#3161),#2003,.F.) ;
#31641 = ADVANCED_FACE('',(#3162),#30359,.F.) ;
#31642 = ADVANCED_FACE('',(#3163),#2004,.F.) ;
#31643 = ADVANCED_FACE('',(#3164,#1141,#1142,#1143),#2005,.T.) ;
#31644 = ADVANCED_FACE('',(#3165),#30360,.T.) ;
#31645 = ADVANCED_FACE('',(#3166),#352,.T.) ;
#31646 = ADVANCED_FACE('',(#3167),#30361,.T.) ;
#31647 = ADVANCED_FACE('',(#3168),#353,.T.) ;
#31648 = ADVANCED_FACE('',(#3169),#30362,.T.) ;
#31649 = ADVANCED_FACE('',(#3170),#354,.T.) ;
#31650 = ADVANCED_FACE('',(#3171),#30363,.T.) ;
#31651 = ADVANCED_FACE('',(#3172),#355,.T.) ;
#31652 = ADVANCED_FACE('',(#3173),#30364,.F.) ;
#31653 = ADVANCED_FACE('',(#3174),#2006,.F.) ;
#31654 = ADVANCED_FACE('',(#3175),#30365,.F.) ;
#31655 = ADVANCED_FACE('',(#3176),#2007,.F.) ;
#31656 = ADVANCED_FACE('',(#3177),#2008,.F.) ;
#31657 = ADVANCED_FACE('',(#3178),#30366,.F.) ;
#31658 = ADVANCED_FACE('',(#3179),#30367,.F.) ;
#31659 = ADVANCED_FACE('',(#3180),#2009,.F.) ;
#31660 = ADVANCED_FACE('',(#3181),#30368,.F.) ;
#31661 = ADVANCED_FACE('',(#3182),#30369,.F.) ;
#31662 = ADVANCED_FACE('',(#3183),#2010,.F.) ;
#31663 = ADVANCED_FACE('',(#3184,#1144),#2011,.F.) ;
#31664 = ADVANCED_FACE('',(#3185),#30370,.F.) ;
#31665 = ADVANCED_FACE('',(#3186),#30371,.F.) ;
#31666 = ADVANCED_FACE('',(#3187),#356,.F.) ;
#31667 = ADVANCED_FACE('',(#3188),#30372,.F.) ;
#31668 = ADVANCED_FACE('',(#3189),#357,.F.) ;
#31669 = ADVANCED_FACE('',(#3190),#358,.F.) ;
#31670 = ADVANCED_FACE('',(#3191),#30373,.F.) ;
#31671 = ADVANCED_FACE('',(#3192),#30374,.F.) ;
#31672 = ADVANCED_FACE('',(#3193),#359,.F.) ;
#31673 = ADVANCED_FACE('',(#3194),#30375,.F.) ;
#31674 = ADVANCED_FACE('',(#3195),#30376,.T.) ;
#31675 = ADVANCED_FACE('',(#3196),#30377,.F.) ;
#31676 = ADVANCED_FACE('',(#3197),#30378,.T.) ;
#31677 = ADVANCED_FACE('',(#3198),#11,.F.) ;
#31678 = ADVANCED_FACE('',(#3199),#12,.F.) ;
#31679 = ADVANCED_FACE('',(#3200),#30379,.F.) ;
#31680 = ADVANCED_FACE('',(#3201),#13,.F.) ;
#31681 = ADVANCED_FACE('',(#3202),#14,.F.) ;
#31682 = ADVANCED_FACE('',(#3203),#2012,.F.) ;
#31683 = ADVANCED_FACE('',(#3204),#2013,.F.) ;
#31684 = ADVANCED_FACE('',(#3205),#2014,.F.) ;
#31685 = ADVANCED_FACE('',(#3206),#2015,.F.) ;
#31686 = ADVANCED_FACE('',(#3207),#15,.F.) ;
#31687 = ADVANCED_FACE('',(#3208),#16,.F.) ;
#31688 = ADVANCED_FACE('',(#3209),#30380,.F.) ;
#31689 = ADVANCED_FACE('',(#3210),#30381,.F.) ;
#31690 = ADVANCED_FACE('',(#3211),#30382,.F.) ;
#31691 = ADVANCED_FACE('',(#3212),#30383,.F.) ;
#31692 = ADVANCED_FACE('',(#3213),#17,.F.) ;
#31693 = ADVANCED_FACE('',(#3214),#18,.F.) ;
#31694 = ADVANCED_FACE('',(#3215),#30384,.F.) ;
#31695 = ADVANCED_FACE('',(#3216),#30385,.F.) ;
#31696 = ADVANCED_FACE('',(#3217),#360,.F.) ;
#31697 = ADVANCED_FACE('',(#3218),#30386,.F.) ;
#31698 = ADVANCED_FACE('',(#3219),#361,.F.) ;
#31699 = ADVANCED_FACE('',(#3220),#362,.F.) ;
#31700 = ADVANCED_FACE('',(#3221),#30387,.F.) ;
#31701 = ADVANCED_FACE('',(#3222),#30388,.F.) ;
#31702 = ADVANCED_FACE('',(#3223),#363,.F.) ;
#31703 = ADVANCED_FACE('',(#3224),#30389,.F.) ;
#31704 = ADVANCED_FACE('',(#3225),#30390,.T.) ;
#31705 = ADVANCED_FACE('',(#3226),#30391,.F.) ;
#31706 = ADVANCED_FACE('',(#3227),#30392,.T.) ;
#31707 = ADVANCED_FACE('',(#3228),#19,.F.) ;
#31708 = ADVANCED_FACE('',(#3229),#20,.F.) ;
#31709 = ADVANCED_FACE('',(#3230),#30393,.F.) ;
#31710 = ADVANCED_FACE('',(#3231),#21,.F.) ;
#31711 = ADVANCED_FACE('',(#3232),#22,.F.) ;
#31712 = ADVANCED_FACE('',(#3233),#2016,.F.) ;
#31713 = ADVANCED_FACE('',(#3234),#2017,.F.) ;
#31714 = ADVANCED_FACE('',(#3235),#2018,.F.) ;
#31715 = ADVANCED_FACE('',(#3236),#2019,.F.) ;
#31716 = ADVANCED_FACE('',(#3237),#23,.F.) ;
#31717 = ADVANCED_FACE('',(#3238),#24,.F.) ;
#31718 = ADVANCED_FACE('',(#3239),#30394,.F.) ;
#31719 = ADVANCED_FACE('',(#3240),#30395,.F.) ;
#31720 = ADVANCED_FACE('',(#3241),#30396,.F.) ;
#31721 = ADVANCED_FACE('',(#3242),#30397,.F.) ;
#31722 = ADVANCED_FACE('',(#3243),#25,.F.) ;
#31723 = ADVANCED_FACE('',(#3244),#26,.F.) ;
#31724 = ADVANCED_FACE('',(#3245),#30398,.F.) ;
#31725 = ADVANCED_FACE('',(#3246),#30399,.F.) ;
#31726 = ADVANCED_FACE('',(#3247),#364,.F.) ;
#31727 = ADVANCED_FACE('',(#3248),#30400,.F.) ;
#31728 = ADVANCED_FACE('',(#3249),#365,.F.) ;
#31729 = ADVANCED_FACE('',(#3250),#366,.F.) ;
#31730 = ADVANCED_FACE('',(#3251),#30401,.F.) ;
#31731 = ADVANCED_FACE('',(#3252),#30402,.F.) ;
#31732 = ADVANCED_FACE('',(#3253),#367,.F.) ;
#31733 = ADVANCED_FACE('',(#3254),#30403,.F.) ;
#31734 = ADVANCED_FACE('',(#3255),#30404,.T.) ;
#31735 = ADVANCED_FACE('',(#3256),#30405,.F.) ;
#31736 = ADVANCED_FACE('',(#3257),#30406,.T.) ;
#31737 = ADVANCED_FACE('',(#3258),#27,.F.) ;
#31738 = ADVANCED_FACE('',(#3259),#28,.F.) ;
#31739 = ADVANCED_FACE('',(#3260),#30407,.F.) ;
#31740 = ADVANCED_FACE('',(#3261),#29,.F.) ;
#31741 = ADVANCED_FACE('',(#3262),#30,.F.) ;
#31742 = ADVANCED_FACE('',(#3263),#2020,.F.) ;
#31743 = ADVANCED_FACE('',(#3264),#2021,.F.) ;
#31744 = ADVANCED_FACE('',(#3265),#2022,.F.) ;
#31745 = ADVANCED_FACE('',(#3266),#2023,.F.) ;
#31746 = ADVANCED_FACE('',(#3267),#31,.F.) ;
#31747 = ADVANCED_FACE('',(#3268),#32,.F.) ;
#31748 = ADVANCED_FACE('',(#3269),#30408,.F.) ;
#31749 = ADVANCED_FACE('',(#3270),#30409,.F.) ;
#31750 = ADVANCED_FACE('',(#3271),#30410,.F.) ;
#31751 = ADVANCED_FACE('',(#3272),#30411,.F.) ;
#31752 = ADVANCED_FACE('',(#3273),#33,.F.) ;
#31753 = ADVANCED_FACE('',(#3274),#34,.F.) ;
#31754 = ADVANCED_FACE('',(#3275),#30412,.F.) ;
#31755 = ADVANCED_FACE('',(#3276),#30413,.F.) ;
#31756 = ADVANCED_FACE('',(#3277),#368,.F.) ;
#31757 = ADVANCED_FACE('',(#3278),#30414,.F.) ;
#31758 = ADVANCED_FACE('',(#3279),#369,.F.) ;
#31759 = ADVANCED_FACE('',(#3280),#370,.F.) ;
#31760 = ADVANCED_FACE('',(#3281),#30415,.F.) ;
#31761 = ADVANCED_FACE('',(#3282),#30416,.F.) ;
#31762 = ADVANCED_FACE('',(#3283),#371,.F.) ;
#31763 = ADVANCED_FACE('',(#3284),#30417,.F.) ;
#31764 = ADVANCED_FACE('',(#3285),#30418,.T.) ;
#31765 = ADVANCED_FACE('',(#3286),#30419,.F.) ;
#31766 = ADVANCED_FACE('',(#3287),#30420,.T.) ;
#31767 = ADVANCED_FACE('',(#3288),#35,.F.) ;
#31768 = ADVANCED_FACE('',(#3289),#36,.F.) ;
#31769 = ADVANCED_FACE('',(#3290),#30421,.F.) ;
#31770 = ADVANCED_FACE('',(#3291),#37,.F.) ;
#31771 = ADVANCED_FACE('',(#3292),#38,.F.) ;
#31772 = ADVANCED_FACE('',(#3293),#2024,.F.) ;
#31773 = ADVANCED_FACE('',(#3294),#2025,.F.) ;
#31774 = ADVANCED_FACE('',(#3295),#2026,.F.) ;
#31775 = ADVANCED_FACE('',(#3296),#2027,.F.) ;
#31776 = ADVANCED_FACE('',(#3297),#39,.F.) ;
#31777 = ADVANCED_FACE('',(#3298),#40,.F.) ;
#31778 = ADVANCED_FACE('',(#3299),#30422,.F.) ;
#31779 = ADVANCED_FACE('',(#3300),#30423,.F.) ;
#31780 = ADVANCED_FACE('',(#3301),#30424,.F.) ;
#31781 = ADVANCED_FACE('',(#3302),#30425,.F.) ;
#31782 = ADVANCED_FACE('',(#3303),#41,.F.) ;
#31783 = ADVANCED_FACE('',(#3304),#42,.F.) ;
#31784 = ADVANCED_FACE('',(#3305),#30426,.F.) ;
#31785 = ADVANCED_FACE('',(#3306),#30427,.F.) ;
#31786 = ADVANCED_FACE('',(#3307),#372,.F.) ;
#31787 = ADVANCED_FACE('',(#3308),#30428,.F.) ;
#31788 = ADVANCED_FACE('',(#3309),#373,.F.) ;
#31789 = ADVANCED_FACE('',(#3310),#374,.F.) ;
#31790 = ADVANCED_FACE('',(#3311),#30429,.F.) ;
#31791 = ADVANCED_FACE('',(#3312),#30430,.F.) ;
#31792 = ADVANCED_FACE('',(#3313),#375,.F.) ;
#31793 = ADVANCED_FACE('',(#3314),#30431,.F.) ;
#31794 = ADVANCED_FACE('',(#3315),#30432,.T.) ;
#31795 = ADVANCED_FACE('',(#3316),#30433,.F.) ;
#31796 = ADVANCED_FACE('',(#3317),#30434,.T.) ;
#31797 = ADVANCED_FACE('',(#3318),#43,.F.) ;
#31798 = ADVANCED_FACE('',(#3319),#44,.F.) ;
#31799 = ADVANCED_FACE('',(#3320),#30435,.F.) ;
#31800 = ADVANCED_FACE('',(#3321),#45,.F.) ;
#31801 = ADVANCED_FACE('',(#3322),#46,.F.) ;
#31802 = ADVANCED_FACE('',(#3323),#2028,.F.) ;
#31803 = ADVANCED_FACE('',(#3324),#2029,.F.) ;
#31804 = ADVANCED_FACE('',(#3325),#2030,.F.) ;
#31805 = ADVANCED_FACE('',(#3326),#2031,.F.) ;
#31806 = ADVANCED_FACE('',(#3327),#47,.F.) ;
#31807 = ADVANCED_FACE('',(#3328),#48,.F.) ;
#31808 = ADVANCED_FACE('',(#3329),#30436,.F.) ;
#31809 = ADVANCED_FACE('',(#3330),#30437,.F.) ;
#31810 = ADVANCED_FACE('',(#3331),#30438,.F.) ;
#31811 = ADVANCED_FACE('',(#3332),#30439,.F.) ;
#31812 = ADVANCED_FACE('',(#3333),#49,.F.) ;
#31813 = ADVANCED_FACE('',(#3334),#50,.F.) ;
#31814 = ADVANCED_FACE('',(#3335),#30440,.F.) ;
#31815 = ADVANCED_FACE('',(#3336),#30441,.F.) ;
#31816 = ADVANCED_FACE('',(#3337),#376,.F.) ;
#31817 = ADVANCED_FACE('',(#3338),#30442,.F.) ;
#31818 = ADVANCED_FACE('',(#3339),#377,.F.) ;
#31819 = ADVANCED_FACE('',(#3340),#378,.F.) ;
#31820 = ADVANCED_FACE('',(#3341),#30443,.F.) ;
#31821 = ADVANCED_FACE('',(#3342),#30444,.F.) ;
#31822 = ADVANCED_FACE('',(#3343),#379,.F.) ;
#31823 = ADVANCED_FACE('',(#3344),#30445,.F.) ;
#31824 = ADVANCED_FACE('',(#3345),#30446,.T.) ;
#31825 = ADVANCED_FACE('',(#3346),#30447,.F.) ;
#31826 = ADVANCED_FACE('',(#3347),#30448,.T.) ;
#31827 = ADVANCED_FACE('',(#3348),#51,.F.) ;
#31828 = ADVANCED_FACE('',(#3349),#52,.F.) ;
#31829 = ADVANCED_FACE('',(#3350),#30449,.F.) ;
#31830 = ADVANCED_FACE('',(#3351),#53,.F.) ;
#31831 = ADVANCED_FACE('',(#3352),#54,.F.) ;
#31832 = ADVANCED_FACE('',(#3353),#2032,.F.) ;
#31833 = ADVANCED_FACE('',(#3354),#2033,.F.) ;
#31834 = ADVANCED_FACE('',(#3355),#2034,.F.) ;
#31835 = ADVANCED_FACE('',(#3356),#2035,.F.) ;
#31836 = ADVANCED_FACE('',(#3357),#55,.F.) ;
#31837 = ADVANCED_FACE('',(#3358),#56,.F.) ;
#31838 = ADVANCED_FACE('',(#3359),#30450,.F.) ;
#31839 = ADVANCED_FACE('',(#3360),#30451,.F.) ;
#31840 = ADVANCED_FACE('',(#3361),#30452,.F.) ;
#31841 = ADVANCED_FACE('',(#3362),#30453,.F.) ;
#31842 = ADVANCED_FACE('',(#3363),#57,.F.) ;
#31843 = ADVANCED_FACE('',(#3364),#58,.F.) ;
#31844 = ADVANCED_FACE('',(#3365),#30454,.F.) ;
#31845 = ADVANCED_FACE('',(#3366),#30455,.F.) ;
#31846 = ADVANCED_FACE('',(#3367),#380,.F.) ;
#31847 = ADVANCED_FACE('',(#3368),#30456,.F.) ;
#31848 = ADVANCED_FACE('',(#3369),#381,.F.) ;
#31849 = ADVANCED_FACE('',(#3370),#382,.F.) ;
#31850 = ADVANCED_FACE('',(#3371),#30457,.F.) ;
#31851 = ADVANCED_FACE('',(#3372),#30458,.F.) ;
#31852 = ADVANCED_FACE('',(#3373),#383,.F.) ;
#31853 = ADVANCED_FACE('',(#3374),#30459,.F.) ;
#31854 = ADVANCED_FACE('',(#3375),#30460,.T.) ;
#31855 = ADVANCED_FACE('',(#3376),#30461,.F.) ;
#31856 = ADVANCED_FACE('',(#3377),#30462,.T.) ;
#31857 = ADVANCED_FACE('',(#3378),#59,.F.) ;
#31858 = ADVANCED_FACE('',(#3379),#60,.F.) ;
#31859 = ADVANCED_FACE('',(#3380),#30463,.F.) ;
#31860 = ADVANCED_FACE('',(#3381),#61,.F.) ;
#31861 = ADVANCED_FACE('',(#3382),#62,.F.) ;
#31862 = ADVANCED_FACE('',(#3383),#2036,.F.) ;
#31863 = ADVANCED_FACE('',(#3384),#2037,.F.) ;
#31864 = ADVANCED_FACE('',(#3385),#2038,.F.) ;
#31865 = ADVANCED_FACE('',(#3386),#2039,.F.) ;
#31866 = ADVANCED_FACE('',(#3387),#63,.F.) ;
#31867 = ADVANCED_FACE('',(#3388),#64,.F.) ;
#31868 = ADVANCED_FACE('',(#3389),#30464,.F.) ;
#31869 = ADVANCED_FACE('',(#3390),#30465,.F.) ;
#31870 = ADVANCED_FACE('',(#3391),#30466,.F.) ;
#31871 = ADVANCED_FACE('',(#3392),#30467,.F.) ;
#31872 = ADVANCED_FACE('',(#3393),#65,.F.) ;
#31873 = ADVANCED_FACE('',(#3394),#66,.F.) ;
#31874 = ADVANCED_FACE('',(#3395),#30468,.F.) ;
#31875 = ADVANCED_FACE('',(#3396),#30469,.F.) ;
#31876 = ADVANCED_FACE('',(#3397),#384,.F.) ;
#31877 = ADVANCED_FACE('',(#3398),#30470,.F.) ;
#31878 = ADVANCED_FACE('',(#3399),#385,.F.) ;
#31879 = ADVANCED_FACE('',(#3400),#386,.F.) ;
#31880 = ADVANCED_FACE('',(#3401),#30471,.F.) ;
#31881 = ADVANCED_FACE('',(#3402),#30472,.F.) ;
#31882 = ADVANCED_FACE('',(#3403),#387,.F.) ;
#31883 = ADVANCED_FACE('',(#3404),#30473,.F.) ;
#31884 = ADVANCED_FACE('',(#3405),#30474,.T.) ;
#31885 = ADVANCED_FACE('',(#3406),#30475,.F.) ;
#31886 = ADVANCED_FACE('',(#3407),#30476,.T.) ;
#31887 = ADVANCED_FACE('',(#3408),#67,.F.) ;
#31888 = ADVANCED_FACE('',(#3409),#68,.F.) ;
#31889 = ADVANCED_FACE('',(#3410),#30477,.F.) ;
#31890 = ADVANCED_FACE('',(#3411),#69,.F.) ;
#31891 = ADVANCED_FACE('',(#3412),#70,.F.) ;
#31892 = ADVANCED_FACE('',(#3413),#2040,.F.) ;
#31893 = ADVANCED_FACE('',(#3414),#2041,.F.) ;
#31894 = ADVANCED_FACE('',(#3415),#2042,.F.) ;
#31895 = ADVANCED_FACE('',(#3416),#2043,.F.) ;
#31896 = ADVANCED_FACE('',(#3417),#71,.F.) ;
#31897 = ADVANCED_FACE('',(#3418),#72,.F.) ;
#31898 = ADVANCED_FACE('',(#3419),#30478,.F.) ;
#31899 = ADVANCED_FACE('',(#3420),#30479,.F.) ;
#31900 = ADVANCED_FACE('',(#3421),#30480,.F.) ;
#31901 = ADVANCED_FACE('',(#3422),#30481,.F.) ;
#31902 = ADVANCED_FACE('',(#3423),#73,.F.) ;
#31903 = ADVANCED_FACE('',(#3424),#74,.F.) ;
#31904 = ADVANCED_FACE('',(#3425),#30482,.F.) ;
#31905 = ADVANCED_FACE('',(#3426),#30483,.F.) ;
#31906 = ADVANCED_FACE('',(#3427),#388,.F.) ;
#31907 = ADVANCED_FACE('',(#3428),#30484,.F.) ;
#31908 = ADVANCED_FACE('',(#3429),#389,.F.) ;
#31909 = ADVANCED_FACE('',(#3430),#390,.F.) ;
#31910 = ADVANCED_FACE('',(#3431),#30485,.F.) ;
#31911 = ADVANCED_FACE('',(#3432),#30486,.F.) ;
#31912 = ADVANCED_FACE('',(#3433),#391,.F.) ;
#31913 = ADVANCED_FACE('',(#3434),#30487,.F.) ;
#31914 = ADVANCED_FACE('',(#3435),#30488,.T.) ;
#31915 = ADVANCED_FACE('',(#3436),#30489,.F.) ;
#31916 = ADVANCED_FACE('',(#3437),#30490,.T.) ;
#31917 = ADVANCED_FACE('',(#3438),#75,.F.) ;
#31918 = ADVANCED_FACE('',(#3439),#76,.F.) ;
#31919 = ADVANCED_FACE('',(#3440),#30491,.F.) ;
#31920 = ADVANCED_FACE('',(#3441),#77,.F.) ;
#31921 = ADVANCED_FACE('',(#3442),#78,.F.) ;
#31922 = ADVANCED_FACE('',(#3443),#2044,.F.) ;
#31923 = ADVANCED_FACE('',(#3444),#2045,.F.) ;
#31924 = ADVANCED_FACE('',(#3445),#2046,.F.) ;
#31925 = ADVANCED_FACE('',(#3446),#2047,.F.) ;
#31926 = ADVANCED_FACE('',(#3447),#79,.F.) ;
#31927 = ADVANCED_FACE('',(#3448),#80,.F.) ;
#31928 = ADVANCED_FACE('',(#3449),#30492,.F.) ;
#31929 = ADVANCED_FACE('',(#3450),#30493,.F.) ;
#31930 = ADVANCED_FACE('',(#3451),#30494,.F.) ;
#31931 = ADVANCED_FACE('',(#3452),#30495,.F.) ;
#31932 = ADVANCED_FACE('',(#3453),#81,.F.) ;
#31933 = ADVANCED_FACE('',(#3454),#82,.F.) ;
#31934 = ADVANCED_FACE('',(#3455),#2048,.F.) ;
#31935 = ADVANCED_FACE('',(#3456),#2049,.F.) ;
#31936 = ADVANCED_FACE('',(#3457),#2050,.F.) ;
#31937 = ADVANCED_FACE('',(#3458),#2051,.F.) ;
#31938 = ADVANCED_FACE('',(#3459),#2052,.F.) ;
#31939 = ADVANCED_FACE('',(#3460),#2053,.F.) ;
#31940 = ADVANCED_FACE('',(#3461),#2054,.F.) ;
#31941 = ADVANCED_FACE('',(#3462),#2055,.F.) ;
#31942 = ADVANCED_FACE('',(#3463),#2056,.F.) ;
#31943 = ADVANCED_FACE('',(#3464),#2057,.F.) ;
#31944 = ADVANCED_FACE('',(#3465),#2058,.F.) ;
#31945 = ADVANCED_FACE('',(#3466),#2059,.F.) ;
#31946 = ADVANCED_FACE('',(#3467),#2060,.F.) ;
#31947 = ADVANCED_FACE('',(#3468),#2061,.F.) ;
#31948 = ADVANCED_FACE('',(#3469),#2062,.F.) ;
#31949 = ADVANCED_FACE('',(#3470),#2063,.F.) ;
#31950 = ADVANCED_FACE('',(#3471),#2064,.F.) ;
#31951 = ADVANCED_FACE('',(#3472),#2065,.F.) ;
#31952 = ADVANCED_FACE('',(#3473),#2066,.F.) ;
#31953 = ADVANCED_FACE('',(#3474),#2067,.F.) ;
#31954 = ADVANCED_FACE('',(#3475),#2068,.F.) ;
#31955 = ADVANCED_FACE('',(#3476),#2069,.F.) ;
#31956 = ADVANCED_FACE('',(#3477),#2070,.F.) ;
#31957 = ADVANCED_FACE('',(#3478),#2071,.F.) ;
#31958 = ADVANCED_FACE('',(#3479),#2072,.F.) ;
#31959 = ADVANCED_FACE('',(#3480),#2073,.F.) ;
#31960 = ADVANCED_FACE('',(#3481),#2074,.F.) ;
#31961 = ADVANCED_FACE('',(#3482),#2075,.F.) ;
#31962 = ADVANCED_FACE('',(#3483),#30496,.T.) ;
#31963 = ADVANCED_FACE('',(#3484),#2076,.T.) ;
#31964 = ADVANCED_FACE('',(#3485),#30497,.T.) ;
#31965 = ADVANCED_FACE('',(#3486),#30498,.T.) ;
#31966 = ADVANCED_FACE('',(#3487),#30499,.T.) ;
#31967 = ADVANCED_FACE('',(#3488),#30500,.T.) ;
#31968 = ADVANCED_FACE('',(#3489),#30501,.T.) ;
#31969 = ADVANCED_FACE('',(#3490),#30502,.T.) ;
#31970 = ADVANCED_FACE('',(#3491),#30503,.T.) ;
#31971 = ADVANCED_FACE('',(#3492),#30504,.T.) ;
#31972 = ADVANCED_FACE('',(#3493),#2077,.T.) ;
#31973 = ADVANCED_FACE('',(#3494),#30505,.T.) ;
#31974 = ADVANCED_FACE('',(#3495),#2078,.T.) ;
#31975 = ADVANCED_FACE('',(#3496),#2079,.T.) ;
#31976 = ADVANCED_FACE('',(#3497),#2080,.T.) ;
#31977 = ADVANCED_FACE('',(#3498),#2081,.T.) ;
#31978 = ADVANCED_FACE('',(#3499),#2082,.T.) ;
#31979 = ADVANCED_FACE('',(#3500),#2083,.T.) ;
#31980 = ADVANCED_FACE('',(#3501),#2084,.T.) ;
#31981 = ADVANCED_FACE('',(#3502),#2085,.T.) ;
#31982 = ADVANCED_FACE('',(#3503),#2086,.T.) ;
#31983 = ADVANCED_FACE('',(#3504),#2087,.T.) ;
#31984 = ADVANCED_FACE('',(#3505),#2088,.T.) ;
#31985 = ADVANCED_FACE('',(#3506),#2089,.T.) ;
#31986 = ADVANCED_FACE('',(#3507),#2090,.T.) ;
#31987 = ADVANCED_FACE('',(#3508),#2091,.T.) ;
#31988 = ADVANCED_FACE('',(#3509),#2092,.T.) ;
#31989 = ADVANCED_FACE('',(#3510),#2093,.T.) ;
#31990 = ADVANCED_FACE('',(#3511),#2094,.T.) ;
#31991 = ADVANCED_FACE('',(#3512),#2095,.F.) ;
#31992 = ADVANCED_FACE('',(#3513),#2096,.F.) ;
#31993 = ADVANCED_FACE('',(#3514),#2097,.F.) ;
#31994 = ADVANCED_FACE('',(#3515),#2098,.F.) ;
#31995 = ADVANCED_FACE('',(#3516),#2099,.F.) ;
#31996 = ADVANCED_FACE('',(#3517),#2100,.F.) ;
#31997 = ADVANCED_FACE('',(#3518),#2101,.F.) ;
#31998 = ADVANCED_FACE('',(#3519),#2102,.F.) ;
#31999 = ADVANCED_FACE('',(#3520),#2103,.F.) ;
#32000 = ADVANCED_FACE('',(#3521),#2104,.F.) ;
#32001 = ADVANCED_FACE('',(#3522),#2105,.T.) ;
#32002 = ADVANCED_FACE('',(#3523),#2106,.F.) ;
#32003 = ADVANCED_FACE('',(#3524),#2107,.F.) ;
#32004 = ADVANCED_FACE('',(#3525),#2108,.F.) ;
#32005 = ADVANCED_FACE('',(#3526),#2109,.F.) ;
#32006 = ADVANCED_FACE('',(#3527),#2110,.F.) ;
#32007 = ADVANCED_FACE('',(#3528),#2111,.F.) ;
#32008 = ADVANCED_FACE('',(#3529),#2112,.F.) ;
#32009 = ADVANCED_FACE('',(#3530),#2113,.F.) ;
#32010 = ADVANCED_FACE('',(#3531,#1145,#1146,#1147),#2114,.T.) ;
#32011 = ADVANCED_FACE('',(#3532),#392,.T.) ;
#32012 = ADVANCED_FACE('',(#3533),#30506,.F.) ;
#32013 = ADVANCED_FACE('',(#3534),#393,.F.) ;
#32014 = ADVANCED_FACE('',(#3535),#2115,.F.) ;
#32015 = ADVANCED_FACE('',(#3536),#30507,.F.) ;
#32016 = ADVANCED_FACE('',(#3537,#1148,#1149,#1150),#2116,.T.) ;
#32017 = ADVANCED_FACE('',(#3538),#394,.T.) ;
#32018 = ADVANCED_FACE('',(#3539),#30508,.F.) ;
#32019 = ADVANCED_FACE('',(#3540),#395,.F.) ;
#32020 = ADVANCED_FACE('',(#3541),#2117,.F.) ;
#32021 = ADVANCED_FACE('',(#3542),#30509,.F.) ;
#32022 = ADVANCED_FACE('',(#3543,#1151,#1152,#1153),#2118,.T.) ;
#32023 = ADVANCED_FACE('',(#3544),#396,.T.) ;
#32024 = ADVANCED_FACE('',(#3545),#30510,.F.) ;
#32025 = ADVANCED_FACE('',(#3546),#397,.F.) ;
#32026 = ADVANCED_FACE('',(#3547),#2119,.F.) ;
#32027 = ADVANCED_FACE('',(#3548),#30511,.F.) ;
#32028 = ADVANCED_FACE('',(#3549,#1154,#1155,#1156),#2120,.T.) ;
#32029 = ADVANCED_FACE('',(#3550),#398,.T.) ;
#32030 = ADVANCED_FACE('',(#3551),#30512,.F.) ;
#32031 = ADVANCED_FACE('',(#3552),#399,.F.) ;
#32032 = ADVANCED_FACE('',(#3553),#2121,.F.) ;
#32033 = ADVANCED_FACE('',(#3554),#30513,.F.) ;
#32034 = ADVANCED_FACE('',(#3555,#1157,#1158,#1159),#2122,.T.) ;
#32035 = ADVANCED_FACE('',(#3556),#400,.T.) ;
#32036 = ADVANCED_FACE('',(#3557),#30514,.F.) ;
#32037 = ADVANCED_FACE('',(#3558),#401,.F.) ;
#32038 = ADVANCED_FACE('',(#3559),#2123,.F.) ;
#32039 = ADVANCED_FACE('',(#3560),#30515,.F.) ;
#32040 = ADVANCED_FACE('',(#3561,#1160,#1161,#1162),#2124,.T.) ;
#32041 = ADVANCED_FACE('',(#3562),#402,.T.) ;
#32042 = ADVANCED_FACE('',(#3563),#30516,.F.) ;
#32043 = ADVANCED_FACE('',(#3564),#403,.F.) ;
#32044 = ADVANCED_FACE('',(#3565),#2125,.F.) ;
#32045 = ADVANCED_FACE('',(#3566),#30517,.F.) ;
#32046 = ADVANCED_FACE('',(#3567,#1163,#1164,#1165),#2126,.T.) ;
#32047 = ADVANCED_FACE('',(#3568),#404,.T.) ;
#32048 = ADVANCED_FACE('',(#3569),#30518,.F.) ;
#32049 = ADVANCED_FACE('',(#3570),#405,.F.) ;
#32050 = ADVANCED_FACE('',(#3571),#2127,.F.) ;
#32051 = ADVANCED_FACE('',(#3572),#30519,.F.) ;
#32052 = ADVANCED_FACE('',(#3573,#1166,#1167,#1168),#2128,.T.) ;
#32053 = ADVANCED_FACE('',(#3574),#406,.T.) ;
#32054 = ADVANCED_FACE('',(#3575),#30520,.F.) ;
#32055 = ADVANCED_FACE('',(#3576),#407,.F.) ;
#32056 = ADVANCED_FACE('',(#3577),#2129,.F.) ;
#32057 = ADVANCED_FACE('',(#3578),#30521,.F.) ;
#32058 = ADVANCED_FACE('',(#3579),#408,.T.) ;
#32059 = ADVANCED_FACE('',(#3580),#30522,.F.) ;
#32060 = ADVANCED_FACE('',(#3581),#409,.F.) ;
#32061 = ADVANCED_FACE('',(#3582),#2130,.F.) ;
#32062 = ADVANCED_FACE('',(#3583),#2131,.T.) ;
#32063 = ADVANCED_FACE('',(#3584),#30523,.F.) ;
#32064 = ADVANCED_FACE('',(#3585),#2132,.F.) ;
#32065 = ADVANCED_FACE('',(#3586),#30524,.F.) ;
#32066 = ADVANCED_FACE('',(#3587),#2133,.F.) ;
#32067 = ADVANCED_FACE('',(#3588),#30525,.F.) ;
#32068 = ADVANCED_FACE('',(#3589),#30526,.F.) ;
#32069 = ADVANCED_FACE('',(#3590),#2134,.F.) ;
#32070 = ADVANCED_FACE('',(#3591),#30527,.F.) ;
#32071 = ADVANCED_FACE('',(#3592),#2135,.F.) ;
#32072 = ADVANCED_FACE('',(#3593),#30528,.F.) ;
#32073 = ADVANCED_FACE('',(#3594),#30529,.F.) ;
#32074 = ADVANCED_FACE('',(#3595),#2136,.F.) ;
#32075 = ADVANCED_FACE('',(#3596),#30530,.F.) ;
#32076 = ADVANCED_FACE('',(#3597),#2137,.F.) ;
#32077 = ADVANCED_FACE('',(#3598),#30531,.F.) ;
#32078 = ADVANCED_FACE('',(#3599),#30532,.F.) ;
#32079 = ADVANCED_FACE('',(#3600),#2138,.F.) ;
#32080 = ADVANCED_FACE('',(#3601),#30533,.F.) ;
#32081 = ADVANCED_FACE('',(#3602),#2139,.F.) ;
#32082 = ADVANCED_FACE('',(#3603),#30534,.F.) ;
#32083 = ADVANCED_FACE('',(#3604),#30535,.F.) ;
#32084 = ADVANCED_FACE('',(#3605),#2140,.F.) ;
#32085 = ADVANCED_FACE('',(#3606),#30536,.F.) ;
#32086 = ADVANCED_FACE('',(#3607),#2141,.F.) ;
#32087 = ADVANCED_FACE('',(#3608),#30537,.F.) ;
#32088 = ADVANCED_FACE('',(#3609),#30538,.F.) ;
#32089 = ADVANCED_FACE('',(#3610),#2142,.F.) ;
#32090 = ADVANCED_FACE('',(#3611),#30539,.F.) ;
#32091 = ADVANCED_FACE('',(#3612),#2143,.F.) ;
#32092 = ADVANCED_FACE('',(#3613),#30540,.F.) ;
#32093 = ADVANCED_FACE('',(#3614),#30541,.F.) ;
#32094 = ADVANCED_FACE('',(#3615),#2144,.F.) ;
#32095 = ADVANCED_FACE('',(#3616),#30542,.F.) ;
#32096 = ADVANCED_FACE('',(#3617),#2145,.F.) ;
#32097 = ADVANCED_FACE('',(#3618),#30543,.F.) ;
#32098 = ADVANCED_FACE('',(#3619),#30544,.F.) ;
#32099 = ADVANCED_FACE('',(#3620),#2146,.F.) ;
#32100 = ADVANCED_FACE('',(#3621),#30545,.F.) ;
#32101 = ADVANCED_FACE('',(#3622),#2147,.F.) ;
#32102 = ADVANCED_FACE('',(#3623),#30546,.F.) ;
#32103 = ADVANCED_FACE('',(#3624),#30547,.T.) ;
#32104 = ADVANCED_FACE('',(#3625),#30548,.T.) ;
#32105 = ADVANCED_FACE('',(#3626),#30549,.T.) ;
#32106 = ADVANCED_FACE('',(#3627),#30550,.T.) ;
#32107 = ADVANCED_FACE('',(#3628),#30551,.T.) ;
#32108 = ADVANCED_FACE('',(#3629),#30552,.T.) ;
#32109 = ADVANCED_FACE('',(#3630),#30553,.T.) ;
#32110 = ADVANCED_FACE('',(#3631),#30554,.T.) ;
#32111 = ADVANCED_FACE('',(#3632),#30555,.T.) ;
#32112 = ADVANCED_FACE('',(#3633),#30556,.T.) ;
#32113 = ADVANCED_FACE('',(#3634),#30557,.T.) ;
#32114 = ADVANCED_FACE('',(#3635),#30558,.T.) ;
#32115 = ADVANCED_FACE('',(#3636),#30559,.T.) ;
#32116 = ADVANCED_FACE('',(#3637),#30560,.T.) ;
#32117 = ADVANCED_FACE('',(#3638),#30561,.T.) ;
#32118 = ADVANCED_FACE('',(#3639),#30562,.T.) ;
#32119 = ADVANCED_FACE('',(#3640),#30563,.T.) ;
#32120 = ADVANCED_FACE('',(#3641),#922,.T.) ;
#32121 = ADVANCED_FACE('',(#3642),#923,.T.) ;
#32122 = ADVANCED_FACE('',(#3643),#924,.T.) ;
#32123 = ADVANCED_FACE('',(#3644),#925,.T.) ;
#32124 = ADVANCED_FACE('',(#3645),#926,.T.) ;
#32125 = ADVANCED_FACE('',(#3646),#927,.T.) ;
#32126 = ADVANCED_FACE('',(#3647),#928,.T.) ;
#32127 = ADVANCED_FACE('',(#3648),#929,.F.) ;
#32128 = ADVANCED_FACE('',(#3649),#410,.T.) ;
#32129 = ADVANCED_FACE('',(#3650),#411,.T.) ;
#32130 = ADVANCED_FACE('',(#3651),#930,.T.) ;
#32131 = ADVANCED_FACE('',(#3652),#931,.T.) ;
#32132 = ADVANCED_FACE('',(#3653),#932,.T.) ;
#32133 = ADVANCED_FACE('',(#3654),#933,.T.) ;
#32134 = ADVANCED_FACE('',(#3655),#934,.T.) ;
#32135 = ADVANCED_FACE('',(#3656),#935,.T.) ;
#32136 = ADVANCED_FACE('',(#3657),#936,.T.) ;
#32137 = ADVANCED_FACE('',(#3658),#30564,.T.) ;
#32138 = ADVANCED_FACE('',(#3659),#2148,.T.) ;
#32139 = ADVANCED_FACE('',(#3660),#937,.T.) ;
#32140 = ADVANCED_FACE('',(#3661),#938,.T.) ;
#32141 = ADVANCED_FACE('',(#3662),#939,.T.) ;
#32142 = ADVANCED_FACE('',(#3663),#940,.T.) ;
#32143 = ADVANCED_FACE('',(#3664),#941,.T.) ;
#32144 = ADVANCED_FACE('',(#3665),#942,.T.) ;
#32145 = ADVANCED_FACE('',(#3666),#943,.T.) ;
#32146 = ADVANCED_FACE('',(#3667),#944,.F.) ;
#32147 = ADVANCED_FACE('',(#3668),#412,.T.) ;
#32148 = ADVANCED_FACE('',(#3669),#945,.T.) ;
#32149 = ADVANCED_FACE('',(#3670),#946,.T.) ;
#32150 = ADVANCED_FACE('',(#3671),#947,.T.) ;
#32151 = ADVANCED_FACE('',(#3672),#948,.T.) ;
#32152 = ADVANCED_FACE('',(#3673),#949,.T.) ;
#32153 = ADVANCED_FACE('',(#3674),#950,.T.) ;
#32154 = ADVANCED_FACE('',(#3675),#951,.T.) ;
#32155 = ADVANCED_FACE('',(#3676),#30565,.T.) ;
#32156 = ADVANCED_FACE('',(#3677),#2149,.F.) ;
#32157 = ADVANCED_FACE('',(#3678),#952,.F.) ;
#32158 = ADVANCED_FACE('',(#3679),#30566,.T.) ;
#32159 = ADVANCED_FACE('',(#3680),#83,.T.) ;
#32160 = ADVANCED_FACE('',(#3681),#413,.T.) ;
#32161 = ADVANCED_FACE('',(#3682),#2150,.T.) ;
#32162 = ADVANCED_FACE('',(#3683),#30567,.F.) ;
#32163 = ADVANCED_FACE('',(#3684),#953,.T.) ;
#32164 = ADVANCED_FACE('',(#3685),#954,.T.) ;
#32165 = ADVANCED_FACE('',(#3686),#955,.T.) ;
#32166 = ADVANCED_FACE('',(#3687),#84,.F.) ;
#32167 = ADVANCED_FACE('',(#3688),#85,.F.) ;
#32168 = ADVANCED_FACE('',(#3689),#956,.T.) ;
#32169 = ADVANCED_FACE('',(#3690),#957,.T.) ;
#32170 = ADVANCED_FACE('',(#3691),#958,.T.) ;
#32171 = ADVANCED_FACE('',(#3692),#414,.T.) ;
#32172 = ADVANCED_FACE('',(#3693),#2151,.T.) ;
#32173 = ADVANCED_FACE('',(#3694),#30568,.F.) ;
#32174 = ADVANCED_FACE('',(#3695),#959,.F.) ;
#32175 = ADVANCED_FACE('',(#3696),#30569,.T.) ;
#32176 = ADVANCED_FACE('',(#3697),#86,.T.) ;
#32177 = ADVANCED_FACE('',(#3698),#2152,.T.) ;
#32178 = ADVANCED_FACE('',(#3699),#30570,.F.) ;
#32179 = ADVANCED_FACE('',(#3700),#87,.F.) ;
#32180 = ADVANCED_FACE('',(#3701),#960,.T.) ;
#32181 = ADVANCED_FACE('',(#3702),#961,.T.) ;
#32182 = ADVANCED_FACE('',(#3703),#962,.T.) ;
#32183 = ADVANCED_FACE('',(#3704),#415,.T.) ;
#32184 = ADVANCED_FACE('',(#3705),#892,.F.) ;
#32185 = ADVANCED_FACE('',(#3706),#416,.F.) ;
#32186 = ADVANCED_FACE('',(#3707),#30571,.F.) ;
#32187 = ADVANCED_FACE('',(#3708),#88,.F.) ;
#32188 = ADVANCED_FACE('',(#3709),#963,.T.) ;
#32189 = ADVANCED_FACE('',(#3710),#964,.T.) ;
#32190 = ADVANCED_FACE('',(#3711),#965,.T.) ;
#32191 = ADVANCED_FACE('',(#3712),#417,.T.) ;
#32192 = ADVANCED_FACE('',(#3713),#2153,.T.) ;
#32193 = ADVANCED_FACE('',(#3714),#30572,.F.) ;
#32194 = ADVANCED_FACE('',(#3715),#966,.F.) ;
#32195 = ADVANCED_FACE('',(#3716),#30573,.T.) ;
#32196 = ADVANCED_FACE('',(#3717),#89,.T.) ;
#32197 = ADVANCED_FACE('',(#3718),#2154,.T.) ;
#32198 = ADVANCED_FACE('',(#3719),#30574,.F.) ;
#32199 = ADVANCED_FACE('',(#3720),#967,.F.) ;
#32200 = ADVANCED_FACE('',(#3721),#30575,.T.) ;
#32201 = ADVANCED_FACE('',(#3722),#90,.T.) ;
#32202 = ADVANCED_FACE('',(#3723),#2155,.T.) ;
#32203 = ADVANCED_FACE('',(#3724),#30576,.F.) ;
#32204 = ADVANCED_FACE('',(#3725),#968,.T.) ;
#32205 = ADVANCED_FACE('',(#3726),#418,.F.) ;
#32206 = ADVANCED_FACE('',(#3727),#969,.T.) ;
#32207 = ADVANCED_FACE('',(#3728),#744,.T.) ;
#32208 = ADVANCED_FACE('',(#3729,#1169),#2156,.T.) ;
#32209 = ADVANCED_FACE('',(#3730),#970,.T.) ;
#32210 = ADVANCED_FACE('',(#3731),#971,.T.) ;
#32211 = ADVANCED_FACE('',(#3732),#972,.T.) ;
#32212 = ADVANCED_FACE('',(#3733),#91,.F.) ;
#32213 = ADVANCED_FACE('',(#3734),#2157,.T.) ;
#32214 = ADVANCED_FACE('',(#3735),#30577,.T.) ;
#32215 = ADVANCED_FACE('',(#3736),#419,.T.) ;
#32216 = ADVANCED_FACE('',(#3737),#92,.F.) ;
#32217 = ADVANCED_FACE('',(#3738),#973,.T.) ;
#32218 = ADVANCED_FACE('',(#3739),#974,.T.) ;
#32219 = ADVANCED_FACE('',(#3740),#975,.T.) ;
#32220 = ADVANCED_FACE('',(#3741),#30578,.T.) ;
#32221 = ADVANCED_FACE('',(#3742),#2158,.T.) ;
#32222 = ADVANCED_FACE('',(#3743),#30579,.F.) ;
#32223 = ADVANCED_FACE('',(#3744),#2159,.F.) ;
#32224 = ADVANCED_FACE('',(#3745),#976,.F.) ;
#32225 = ADVANCED_FACE('',(#3746),#30580,.T.) ;
#32226 = ADVANCED_FACE('',(#3747),#977,.F.) ;
#32227 = ADVANCED_FACE('',(#3748),#30581,.T.) ;
#32228 = ADVANCED_FACE('',(#3749),#93,.T.) ;
#32229 = ADVANCED_FACE('',(#3750),#94,.T.) ;
#32230 = ADVANCED_FACE('',(#3751),#30582,.F.) ;
#32231 = ADVANCED_FACE('',(#3752),#2160,.T.) ;
#32232 = ADVANCED_FACE('',(#3753),#30583,.F.) ;
#32233 = ADVANCED_FACE('',(#3754),#95,.T.) ;
#32234 = ADVANCED_FACE('',(#3755),#30584,.T.) ;
#32235 = ADVANCED_FACE('',(#3756),#30585,.T.) ;
#32236 = ADVANCED_FACE('',(#3757),#978,.F.) ;
#32237 = ADVANCED_FACE('',(#3758),#979,.F.) ;
#32238 = ADVANCED_FACE('',(#3759),#30586,.T.) ;
#32239 = ADVANCED_FACE('',(#3760),#96,.T.) ;
#32240 = ADVANCED_FACE('',(#3761),#30587,.T.) ;
#32241 = ADVANCED_FACE('',(#3762),#980,.F.) ;
#32242 = ADVANCED_FACE('',(#3763),#97,.T.) ;
#32243 = ADVANCED_FACE('',(#3764),#420,.T.) ;
#32244 = ADVANCED_FACE('',(#3765),#421,.T.) ;
#32245 = ADVANCED_FACE('',(#3766),#2161,.F.) ;
#32246 = ADVANCED_FACE('',(#3767),#30588,.F.) ;
#32247 = ADVANCED_FACE('',(#3768),#2162,.T.) ;
#32248 = ADVANCED_FACE('',(#3769),#98,.T.) ;
#32249 = ADVANCED_FACE('',(#3770),#30589,.T.) ;
#32250 = ADVANCED_FACE('',(#3771),#30590,.T.) ;
#32251 = ADVANCED_FACE('',(#3772),#981,.F.) ;
#32252 = ADVANCED_FACE('',(#3773),#30591,.F.) ;
#32253 = ADVANCED_FACE('',(#3774),#30592,.F.) ;
#32254 = ADVANCED_FACE('',(#3775),#982,.F.) ;
#32255 = ADVANCED_FACE('',(#3776),#983,.F.) ;
#32256 = ADVANCED_FACE('',(#3777),#30593,.F.) ;
#32257 = ADVANCED_FACE('',(#3778),#984,.T.) ;
#32258 = ADVANCED_FACE('',(#3779),#985,.T.) ;
#32259 = ADVANCED_FACE('',(#3780),#986,.T.) ;
#32260 = ADVANCED_FACE('',(#3781),#99,.F.) ;
#32261 = ADVANCED_FACE('',(#3782),#2163,.T.) ;
#32262 = ADVANCED_FACE('',(#3783),#30594,.T.) ;
#32263 = ADVANCED_FACE('',(#3784),#422,.T.) ;
#32264 = ADVANCED_FACE('',(#3785),#100,.F.) ;
#32265 = ADVANCED_FACE('',(#3786),#987,.T.) ;
#32266 = ADVANCED_FACE('',(#3787),#988,.T.) ;
#32267 = ADVANCED_FACE('',(#3788),#989,.T.) ;
#32268 = ADVANCED_FACE('',(#3789),#30595,.T.) ;
#32269 = ADVANCED_FACE('',(#3790),#2164,.T.) ;
#32270 = ADVANCED_FACE('',(#3791),#30596,.F.) ;
#32271 = ADVANCED_FACE('',(#3792),#2165,.F.) ;
#32272 = ADVANCED_FACE('',(#3793),#30597,.T.) ;
#32273 = ADVANCED_FACE('',(#3794),#990,.F.) ;
#32274 = ADVANCED_FACE('',(#3795),#991,.F.) ;
#32275 = ADVANCED_FACE('',(#3796),#30598,.T.) ;
#32276 = ADVANCED_FACE('',(#3797),#101,.T.) ;
#32277 = ADVANCED_FACE('',(#3798),#102,.T.) ;
#32278 = ADVANCED_FACE('',(#3799),#30599,.F.) ;
#32279 = ADVANCED_FACE('',(#3800),#30600,.F.) ;
#32280 = ADVANCED_FACE('',(#3801),#2166,.T.) ;
#32281 = ADVANCED_FACE('',(#3802),#30601,.F.) ;
#32282 = ADVANCED_FACE('',(#3803),#103,.T.) ;
#32283 = ADVANCED_FACE('',(#3804),#30602,.T.) ;
#32284 = ADVANCED_FACE('',(#3805),#992,.F.) ;
#32285 = ADVANCED_FACE('',(#3806),#30603,.T.) ;
#32286 = ADVANCED_FACE('',(#3807),#2167,.T.) ;
#32287 = ADVANCED_FACE('',(#3808),#993,.F.) ;
#32288 = ADVANCED_FACE('',(#3809),#30604,.T.) ;
#32289 = ADVANCED_FACE('',(#3810),#104,.T.) ;
#32290 = ADVANCED_FACE('',(#3811),#30605,.T.) ;
#32291 = ADVANCED_FACE('',(#3812),#994,.F.) ;
#32292 = ADVANCED_FACE('',(#3813),#105,.T.) ;
#32293 = ADVANCED_FACE('',(#3814),#423,.T.) ;
#32294 = ADVANCED_FACE('',(#3815),#424,.T.) ;
#32295 = ADVANCED_FACE('',(#3816),#2168,.T.) ;
#32296 = ADVANCED_FACE('',(#3817),#2169,.T.) ;
#32297 = ADVANCED_FACE('',(#3818),#106,.T.) ;
#32298 = ADVANCED_FACE('',(#3819),#30606,.T.) ;
#32299 = ADVANCED_FACE('',(#3820),#30607,.T.) ;
#32300 = ADVANCED_FACE('',(#3821),#995,.F.) ;
#32301 = ADVANCED_FACE('',(#3822),#30608,.F.) ;
#32302 = ADVANCED_FACE('',(#3823),#30609,.F.) ;
#32303 = ADVANCED_FACE('',(#3824),#425,.F.) ;
#32304 = ADVANCED_FACE('',(#3825),#426,.F.) ;
#32305 = ADVANCED_FACE('',(#3826),#427,.F.) ;
#32306 = ADVANCED_FACE('',(#3827),#2170,.T.) ;
#32307 = ADVANCED_FACE('',(#3828),#893,.F.) ;
#32308 = ADVANCED_FACE('',(#3829),#2171,.T.) ;
#32309 = ADVANCED_FACE('',(#3830),#428,.T.) ;
#32310 = ADVANCED_FACE('',(#3831),#996,.F.) ;
#32311 = ADVANCED_FACE('',(#3832),#429,.T.) ;
#32312 = ADVANCED_FACE('',(#3833),#430,.T.) ;
#32313 = ADVANCED_FACE('',(#3834),#30610,.T.) ;
#32314 = ADVANCED_FACE('',(#3835),#997,.F.) ;
#32315 = ADVANCED_FACE('',(#3836),#107,.T.) ;
#32316 = ADVANCED_FACE('',(#3837),#431,.T.) ;
#32317 = ADVANCED_FACE('',(#3838),#30611,.T.) ;
#32318 = ADVANCED_FACE('',(#3839),#998,.F.) ;
#32319 = ADVANCED_FACE('',(#3840),#432,.T.) ;
#32320 = ADVANCED_FACE('',(#3841),#433,.T.) ;
#32321 = ADVANCED_FACE('',(#3842),#434,.T.) ;
#32322 = ADVANCED_FACE('',(#3843),#999,.F.) ;
#32323 = ADVANCED_FACE('',(#3844),#30612,.T.) ;
#32324 = ADVANCED_FACE('',(#3845),#108,.T.) ;
#32325 = ADVANCED_FACE('',(#3846),#435,.T.) ;
#32326 = ADVANCED_FACE('',(#3847),#30613,.T.) ;
#32327 = ADVANCED_FACE('',(#3848),#894,.T.) ;
#32328 = ADVANCED_FACE('',(#3849),#895,.F.) ;
#32329 = ADVANCED_FACE('',(#3850),#896,.F.) ;
#32330 = ADVANCED_FACE('',(#3851),#2172,.F.) ;
#32331 = ADVANCED_FACE('',(#3852),#745,.T.) ;
#32332 = ADVANCED_FACE('',(#3853),#30614,.F.) ;
#32333 = ADVANCED_FACE('',(#3854),#30615,.F.) ;
#32334 = ADVANCED_FACE('',(#3855),#30616,.F.) ;
#32335 = ADVANCED_FACE('',(#3856),#30617,.F.) ;
#32336 = ADVANCED_FACE('',(#3857),#30618,.F.) ;
#32337 = ADVANCED_FACE('',(#3858),#30619,.F.) ;
#32338 = ADVANCED_FACE('',(#3859),#30620,.F.) ;
#32339 = ADVANCED_FACE('',(#3860),#30621,.F.) ;
#32340 = ADVANCED_FACE('',(#3861),#30622,.F.) ;
#32341 = ADVANCED_FACE('',(#3862),#30623,.F.) ;
#32342 = ADVANCED_FACE('',(#3863),#30624,.T.) ;
#32343 = ADVANCED_FACE('',(#3864),#436,.T.) ;
#32344 = ADVANCED_FACE('',(#3865),#30625,.T.) ;
#32345 = ADVANCED_FACE('',(#3866),#437,.T.) ;
#32346 = ADVANCED_FACE('',(#3867),#438,.T.) ;
#32347 = ADVANCED_FACE('',(#3868),#30626,.T.) ;
#32348 = ADVANCED_FACE('',(#3869),#439,.T.) ;
#32349 = ADVANCED_FACE('',(#3870),#30627,.T.) ;
#32350 = ADVANCED_FACE('',(#3871),#30628,.T.) ;
#32351 = ADVANCED_FACE('',(#3872),#440,.T.) ;
#32352 = ADVANCED_FACE('',(#3873),#30629,.T.) ;
#32353 = ADVANCED_FACE('',(#3874),#30630,.T.) ;
#32354 = ADVANCED_FACE('',(#3875),#441,.T.) ;
#32355 = ADVANCED_FACE('',(#3876),#30631,.T.) ;
#32356 = ADVANCED_FACE('',(#3877),#30632,.F.) ;
#32357 = ADVANCED_FACE('',(#3878),#30633,.T.) ;
#32358 = ADVANCED_FACE('',(#3879),#30634,.F.) ;
#32359 = ADVANCED_FACE('',(#3880),#109,.T.) ;
#32360 = ADVANCED_FACE('',(#3881),#110,.T.) ;
#32361 = ADVANCED_FACE('',(#3882),#30635,.T.) ;
#32362 = ADVANCED_FACE('',(#3883),#111,.T.) ;
#32363 = ADVANCED_FACE('',(#3884),#112,.T.) ;
#32364 = ADVANCED_FACE('',(#3885),#2173,.T.) ;
#32365 = ADVANCED_FACE('',(#3886),#30636,.T.) ;
#32366 = ADVANCED_FACE('',(#3887),#2174,.T.) ;
#32367 = ADVANCED_FACE('',(#3888),#30637,.T.) ;
#32368 = ADVANCED_FACE('',(#3889),#2175,.T.) ;
#32369 = ADVANCED_FACE('',(#3890),#2176,.T.) ;
#32370 = ADVANCED_FACE('',(#3891),#2177,.T.) ;
#32371 = ADVANCED_FACE('',(#3892),#2178,.T.) ;
#32372 = ADVANCED_FACE('',(#3893),#30638,.T.) ;
#32373 = ADVANCED_FACE('',(#3894),#30639,.T.) ;
#32374 = ADVANCED_FACE('',(#3895),#30640,.T.) ;
#32375 = ADVANCED_FACE('',(#3896),#2179,.T.) ;
#32376 = ADVANCED_FACE('',(#3897),#2180,.T.) ;
#32377 = ADVANCED_FACE('',(#3898),#2181,.T.) ;
#32378 = ADVANCED_FACE('',(#3899),#2182,.T.) ;
#32379 = ADVANCED_FACE('',(#3900),#2183,.T.) ;
#32380 = ADVANCED_FACE('',(#3901,#1170),#2184,.T.) ;
#32381 = ADVANCED_FACE('',(#3902),#30641,.T.) ;
#32382 = ADVANCED_FACE('',(#3903),#30642,.T.) ;
#32383 = ADVANCED_FACE('',(#3904),#30643,.F.) ;
#32384 = ADVANCED_FACE('',(#3905),#30644,.F.) ;
#32385 = ADVANCED_FACE('',(#3906),#2185,.T.) ;
#32386 = ADVANCED_FACE('',(#3907),#30645,.T.) ;
#32387 = ADVANCED_FACE('',(#3908),#2186,.T.) ;
#32388 = ADVANCED_FACE('',(#3909),#2187,.T.) ;
#32389 = ADVANCED_FACE('',(#3910),#30646,.T.) ;
#32390 = ADVANCED_FACE('',(#3911),#2188,.T.) ;
#32391 = ADVANCED_FACE('',(#3912),#442,.F.) ;
#32392 = ADVANCED_FACE('',(#3913),#443,.F.) ;
#32393 = ADVANCED_FACE('',(#3914),#444,.F.) ;
#32394 = ADVANCED_FACE('',(#3915),#113,.T.) ;
#32395 = ADVANCED_FACE('',(#3916),#445,.F.) ;
#32396 = ADVANCED_FACE('',(#3917),#114,.T.) ;
#32397 = ADVANCED_FACE('',(#3918),#30647,.T.) ;
#32398 = ADVANCED_FACE('',(#3919),#30648,.F.) ;
#32399 = ADVANCED_FACE('',(#3920),#30649,.F.) ;
#32400 = ADVANCED_FACE('',(#3921),#30650,.T.) ;
#32401 = ADVANCED_FACE('',(#3922),#30651,.T.) ;
#32402 = ADVANCED_FACE('',(#3923),#30652,.T.) ;
#32403 = ADVANCED_FACE('',(#3924),#446,.T.) ;
#32404 = ADVANCED_FACE('',(#3925),#30653,.T.) ;
#32405 = ADVANCED_FACE('',(#3926),#447,.T.) ;
#32406 = ADVANCED_FACE('',(#3927),#30654,.T.) ;
#32407 = ADVANCED_FACE('',(#3928),#30655,.T.) ;
#32408 = ADVANCED_FACE('',(#3929),#30656,.T.) ;
#32409 = ADVANCED_FACE('',(#3930),#30657,.T.) ;
#32410 = ADVANCED_FACE('',(#3931),#448,.T.) ;
#32411 = ADVANCED_FACE('',(#3932),#30658,.T.) ;
#32412 = ADVANCED_FACE('',(#3933),#449,.T.) ;
#32413 = ADVANCED_FACE('',(#3934),#30659,.T.) ;
#32414 = ADVANCED_FACE('',(#3935),#30660,.F.) ;
#32415 = ADVANCED_FACE('',(#3936),#30661,.T.) ;
#32416 = ADVANCED_FACE('',(#3937),#30662,.T.) ;
#32417 = ADVANCED_FACE('',(#3938),#30663,.T.) ;
#32418 = ADVANCED_FACE('',(#3939),#30664,.T.) ;
#32419 = ADVANCED_FACE('',(#3940),#30665,.T.) ;
#32420 = ADVANCED_FACE('',(#3941),#115,.T.) ;
#32421 = ADVANCED_FACE('',(#3942),#116,.T.) ;
#32422 = ADVANCED_FACE('',(#3943),#30666,.F.) ;
#32423 = ADVANCED_FACE('',(#3944),#30667,.T.) ;
#32424 = ADVANCED_FACE('',(#3945),#450,.T.) ;
#32425 = ADVANCED_FACE('',(#3946),#30668,.T.) ;
#32426 = ADVANCED_FACE('',(#3947),#451,.T.) ;
#32427 = ADVANCED_FACE('',(#3948),#117,.T.) ;
#32428 = ADVANCED_FACE('',(#3949),#118,.T.) ;
#32429 = ADVANCED_FACE('',(#3950),#119,.T.) ;
#32430 = ADVANCED_FACE('',(#3951),#120,.T.) ;
#32431 = ADVANCED_FACE('',(#3952),#452,.T.) ;
#32432 = ADVANCED_FACE('',(#3953),#453,.T.) ;
#32433 = ADVANCED_FACE('',(#3954),#454,.T.) ;
#32434 = ADVANCED_FACE('',(#3955,#1171),#2189,.T.) ;
#32435 = ADVANCED_FACE('',(#3956),#30669,.T.) ;
#32436 = ADVANCED_FACE('',(#3957),#455,.F.) ;
#32437 = ADVANCED_FACE('',(#3958,#1172),#2190,.T.) ;
#32438 = ADVANCED_FACE('',(#3959),#746,.F.) ;
#32439 = ADVANCED_FACE('',(#3960),#747,.F.) ;
#32440 = ADVANCED_FACE('',(#3961),#748,.T.) ;
#32441 = ADVANCED_FACE('',(#3962),#749,.T.) ;
#32442 = ADVANCED_FACE('',(#3963),#750,.T.) ;
#32443 = ADVANCED_FACE('',(#3964),#751,.T.) ;
#32444 = ADVANCED_FACE('',(#3965),#752,.T.) ;
#32445 = ADVANCED_FACE('',(#3966),#30670,.F.) ;
#32446 = ADVANCED_FACE('',(#3967,#1173),#2191,.T.) ;
#32447 = ADVANCED_FACE('',(#3968),#2192,.T.) ;
#32448 = ADVANCED_FACE('',(#3969),#2193,.T.) ;
#32449 = ADVANCED_FACE('',(#3970),#2194,.T.) ;
#32450 = ADVANCED_FACE('',(#3971),#2195,.T.) ;
#32451 = ADVANCED_FACE('',(#3972),#456,.T.) ;
#32452 = ADVANCED_FACE('',(#3973),#30671,.T.) ;
#32453 = ADVANCED_FACE('',(#3974),#30672,.T.) ;
#32454 = ADVANCED_FACE('',(#3975),#457,.T.) ;
#32455 = ADVANCED_FACE('',(#3976),#30673,.T.) ;
#32456 = ADVANCED_FACE('',(#3977),#30674,.T.) ;
#32457 = ADVANCED_FACE('',(#3978),#458,.T.) ;
#32458 = ADVANCED_FACE('',(#3979),#30675,.T.) ;
#32459 = ADVANCED_FACE('',(#3980),#30676,.T.) ;
#32460 = ADVANCED_FACE('',(#3981),#2196,.T.) ;
#32461 = ADVANCED_FACE('',(#3982),#2197,.T.) ;
#32462 = ADVANCED_FACE('',(#3983),#30677,.F.) ;
#32463 = ADVANCED_FACE('',(#3984),#30678,.F.) ;
#32464 = ADVANCED_FACE('',(#3985),#30679,.F.) ;
#32465 = ADVANCED_FACE('',(#3986),#459,.F.) ;
#32466 = ADVANCED_FACE('',(#3987),#2198,.T.) ;
#32467 = ADVANCED_FACE('',(#3988),#2199,.T.) ;
#32468 = ADVANCED_FACE('',(#3989),#460,.F.) ;
#32469 = ADVANCED_FACE('',(#3990),#30680,.F.) ;
#32470 = ADVANCED_FACE('',(#3991),#30681,.F.) ;
#32471 = ADVANCED_FACE('',(#3992),#2200,.T.) ;
#32472 = ADVANCED_FACE('',(#3993),#2201,.T.) ;
#32473 = ADVANCED_FACE('',(#3994),#30682,.F.) ;
#32474 = ADVANCED_FACE('',(#3995),#461,.F.) ;
#32475 = ADVANCED_FACE('',(#3996),#30683,.F.) ;
#32476 = ADVANCED_FACE('',(#3997),#30684,.F.) ;
#32477 = ADVANCED_FACE('',(#3998),#2202,.T.) ;
#32478 = ADVANCED_FACE('',(#3999),#2203,.T.) ;
#32479 = ADVANCED_FACE('',(#4000),#30685,.F.) ;
#32480 = ADVANCED_FACE('',(#4001),#30686,.F.) ;
#32481 = ADVANCED_FACE('',(#4002),#30687,.F.) ;
#32482 = ADVANCED_FACE('',(#4003),#462,.F.) ;
#32483 = ADVANCED_FACE('',(#4004),#30688,.F.) ;
#32484 = ADVANCED_FACE('',(#4005),#463,.T.) ;
#32485 = ADVANCED_FACE('',(#4006),#30689,.T.) ;
#32486 = ADVANCED_FACE('',(#4007),#30690,.T.) ;
#32487 = ADVANCED_FACE('',(#4008),#2204,.T.) ;
#32488 = ADVANCED_FACE('',(#4009),#2205,.T.) ;
#32489 = ADVANCED_FACE('',(#4010),#2206,.T.) ;
#32490 = ADVANCED_FACE('',(#4011),#30691,.T.) ;
#32491 = ADVANCED_FACE('',(#4012),#30692,.T.) ;
#32492 = ADVANCED_FACE('',(#4013),#30693,.T.) ;
#32493 = ADVANCED_FACE('',(#4014),#464,.T.) ;
#32494 = ADVANCED_FACE('',(#4015),#2207,.T.) ;
#32495 = ADVANCED_FACE('',(#4016),#2208,.T.) ;
#32496 = ADVANCED_FACE('',(#4017),#2209,.T.) ;
#32497 = ADVANCED_FACE('',(#4018),#30694,.T.) ;
#32498 = ADVANCED_FACE('',(#4019),#30695,.T.) ;
#32499 = ADVANCED_FACE('',(#4020),#30696,.T.) ;
#32500 = ADVANCED_FACE('',(#4021),#465,.T.) ;
#32501 = ADVANCED_FACE('',(#4022),#2210,.T.) ;
#32502 = ADVANCED_FACE('',(#4023),#2211,.T.) ;
#32503 = ADVANCED_FACE('',(#4024),#2212,.T.) ;
#32504 = ADVANCED_FACE('',(#4025),#30697,.T.) ;
#32505 = ADVANCED_FACE('',(#4026),#30698,.T.) ;
#32506 = ADVANCED_FACE('',(#4027),#30699,.T.) ;
#32507 = ADVANCED_FACE('',(#4028),#466,.T.) ;
#32508 = ADVANCED_FACE('',(#4029),#2213,.T.) ;
#32509 = ADVANCED_FACE('',(#4030),#2214,.T.) ;
#32510 = ADVANCED_FACE('',(#4031),#2215,.T.) ;
#32511 = ADVANCED_FACE('',(#4032),#30700,.T.) ;
#32512 = ADVANCED_FACE('',(#4033),#30701,.T.) ;
#32513 = ADVANCED_FACE('',(#4034),#30702,.T.) ;
#32514 = ADVANCED_FACE('',(#4035),#467,.T.) ;
#32515 = ADVANCED_FACE('',(#4036),#2216,.T.) ;
#32516 = ADVANCED_FACE('',(#4037),#2217,.T.) ;
#32517 = ADVANCED_FACE('',(#4038),#2218,.T.) ;
#32518 = ADVANCED_FACE('',(#4039),#2219,.T.) ;
#32519 = ADVANCED_FACE('',(#4040,#1174),#2220,.T.) ;
#32520 = ADVANCED_FACE('',(#4041),#753,.T.) ;
#32521 = ADVANCED_FACE('',(#4042),#2221,.T.) ;
#32522 = ADVANCED_FACE('',(#4043),#2222,.T.) ;
#32523 = ADVANCED_FACE('',(#4044),#754,.T.) ;
#32524 = ADVANCED_FACE('',(#4045),#2223,.T.) ;
#32525 = ADVANCED_FACE('',(#4046),#2224,.T.) ;
#32526 = ADVANCED_FACE('',(#4047),#755,.T.) ;
#32527 = ADVANCED_FACE('',(#4048),#756,.T.) ;
#32528 = ADVANCED_FACE('',(#4049),#2225,.T.) ;
#32529 = ADVANCED_FACE('',(#4050),#2226,.T.) ;
#32530 = ADVANCED_FACE('',(#4051),#757,.T.) ;
#32531 = ADVANCED_FACE('',(#4052),#2227,.T.) ;
#32532 = ADVANCED_FACE('',(#4053),#2228,.T.) ;
#32533 = ADVANCED_FACE('',(#4054),#30703,.T.) ;
#32534 = ADVANCED_FACE('',(#4055),#30704,.T.) ;
#32535 = ADVANCED_FACE('',(#4056),#30705,.T.) ;
#32536 = ADVANCED_FACE('',(#4057),#30706,.T.) ;
#32537 = ADVANCED_FACE('',(#4058),#2229,.T.) ;
#32538 = ADVANCED_FACE('',(#4059),#2230,.T.) ;
#32539 = ADVANCED_FACE('',(#4060),#2231,.T.) ;
#32540 = ADVANCED_FACE('',(#4061),#2232,.T.) ;
#32541 = ADVANCED_FACE('',(#4062),#2233,.T.) ;
#32542 = ADVANCED_FACE('',(#4063),#2234,.T.) ;
#32543 = ADVANCED_FACE('',(#4064),#2235,.T.) ;
#32544 = ADVANCED_FACE('',(#4065),#2236,.T.) ;
#32545 = ADVANCED_FACE('',(#4066),#2237,.T.) ;
#32546 = ADVANCED_FACE('',(#4067),#2238,.T.) ;
#32547 = ADVANCED_FACE('',(#4068),#2239,.T.) ;
#32548 = ADVANCED_FACE('',(#4069),#2240,.T.) ;
#32549 = ADVANCED_FACE('',(#4070,#1175,#1176,#1177,#1178,#1179),#2241,.T.) ;
#32550 = ADVANCED_FACE('',(#4071,#1180,#1181,#1182,#1183,#1184),#2242,.T.) ;
#32551 = ADVANCED_FACE('',(#4072),#2243,.T.) ;
#32552 = ADVANCED_FACE('',(#4073),#2244,.F.) ;
#32553 = ADVANCED_FACE('',(#4074),#2245,.T.) ;
#32554 = ADVANCED_FACE('',(#4075),#2246,.T.) ;
#32555 = ADVANCED_FACE('',(#4076),#30707,.F.) ;
#32556 = ADVANCED_FACE('',(#4077),#30708,.F.) ;
#32557 = ADVANCED_FACE('',(#4078),#30709,.F.) ;
#32558 = ADVANCED_FACE('',(#4079),#30710,.F.) ;
#32559 = ADVANCED_FACE('',(#4080),#30711,.F.) ;
#32560 = ADVANCED_FACE('',(#4081),#30712,.T.) ;
#32561 = ADVANCED_FACE('',(#4082),#30713,.T.) ;
#32562 = ADVANCED_FACE('',(#4083),#30714,.T.) ;
#32563 = ADVANCED_FACE('',(#4084),#30715,.T.) ;
#32564 = ADVANCED_FACE('',(#4085),#30716,.T.) ;
#32565 = ADVANCED_FACE('',(#4086),#30717,.T.) ;
#32566 = ADVANCED_FACE('',(#4087),#30718,.T.) ;
#32567 = ADVANCED_FACE('',(#4088),#30719,.T.) ;
#32568 = ADVANCED_FACE('',(#4089),#30720,.T.) ;
#32569 = ADVANCED_FACE('',(#4090),#30721,.T.) ;
#32570 = ADVANCED_FACE('',(#4091),#30722,.T.) ;
#32571 = ADVANCED_FACE('',(#4092),#30723,.T.) ;
#32572 = ADVANCED_FACE('',(#4093),#30724,.T.) ;
#32573 = ADVANCED_FACE('',(#4094),#30725,.T.) ;
#32574 = ADVANCED_FACE('',(#4095),#30726,.T.) ;
#32575 = ADVANCED_FACE('',(#4096),#30727,.T.) ;
#32576 = ADVANCED_FACE('',(#4097),#30728,.T.) ;
#32577 = ADVANCED_FACE('',(#4098),#30729,.T.) ;
#32578 = ADVANCED_FACE('',(#4099),#30730,.T.) ;
#32579 = ADVANCED_FACE('',(#4100),#30731,.T.) ;
#32580 = ADVANCED_FACE('',(#4101),#30732,.T.) ;
#32581 = ADVANCED_FACE('',(#4102),#30733,.T.) ;
#32582 = ADVANCED_FACE('',(#4103),#30734,.T.) ;
#32583 = ADVANCED_FACE('',(#4104),#30735,.T.) ;
#32584 = ADVANCED_FACE('',(#4105),#30736,.T.) ;
#32585 = ADVANCED_FACE('',(#4106),#30737,.T.) ;
#32586 = ADVANCED_FACE('',(#4107),#30738,.T.) ;
#32587 = ADVANCED_FACE('',(#4108),#30739,.T.) ;
#32588 = ADVANCED_FACE('',(#4109),#30740,.T.) ;
#32589 = ADVANCED_FACE('',(#4110),#30741,.T.) ;
#32590 = ADVANCED_FACE('',(#4111),#30742,.T.) ;
#32591 = ADVANCED_FACE('',(#4112),#897,.T.) ;
#32592 = ADVANCED_FACE('',(#4113),#898,.T.) ;
#32593 = ADVANCED_FACE('',(#4114),#30743,.T.) ;
#32594 = ADVANCED_FACE('',(#4115),#30744,.T.) ;
#32595 = ADVANCED_FACE('',(#4116),#899,.F.) ;
#32596 = ADVANCED_FACE('',(#4117),#900,.F.) ;
#32597 = ADVANCED_FACE('',(#4118),#468,.T.) ;
#32598 = ADVANCED_FACE('',(#4119,#1185),#121,.T.) ;
#32599 = ADVANCED_FACE('',(#4120),#30745,.T.) ;
#32600 = ADVANCED_FACE('',(#4121),#469,.T.) ;
#32601 = ADVANCED_FACE('',(#4122,#1186),#2247,.T.) ;
#32602 = ADVANCED_FACE('',(#4123),#758,.F.) ;
#32603 = ADVANCED_FACE('',(#4124),#759,.F.) ;
#32604 = ADVANCED_FACE('',(#4125),#760,.T.) ;
#32605 = ADVANCED_FACE('',(#4126),#2248,.F.) ;
#32606 = ADVANCED_FACE('',(#4127),#901,.F.) ;
#32607 = ADVANCED_FACE('',(#4128),#2249,.T.) ;
#32608 = ADVANCED_FACE('',(#4129),#2250,.T.) ;
#32609 = ADVANCED_FACE('',(#4130),#2251,.T.) ;
#32610 = ADVANCED_FACE('',(#4131),#2252,.T.) ;
#32611 = ADVANCED_FACE('',(#4132),#2253,.T.) ;
#32612 = ADVANCED_FACE('',(#4133),#2254,.T.) ;
#32613 = ADVANCED_FACE('',(#4134),#2255,.T.) ;
#32614 = ADVANCED_FACE('',(#4135),#2256,.T.) ;
#32615 = ADVANCED_FACE('',(#4136),#2257,.T.) ;
#32616 = ADVANCED_FACE('',(#4137),#2258,.T.) ;
#32617 = ADVANCED_FACE('',(#4138),#2259,.T.) ;
#32618 = ADVANCED_FACE('',(#4139),#2260,.T.) ;
#32619 = ADVANCED_FACE('',(#4140),#2261,.T.) ;
#32620 = ADVANCED_FACE('',(#4141),#902,.F.) ;
#32621 = ADVANCED_FACE('',(#4142),#2262,.T.) ;
#32622 = ADVANCED_FACE('',(#4143),#2263,.T.) ;
#32623 = ADVANCED_FACE('',(#4144),#2264,.T.) ;
#32624 = ADVANCED_FACE('',(#4145),#2265,.T.) ;
#32625 = ADVANCED_FACE('',(#4146),#2266,.T.) ;
#32626 = ADVANCED_FACE('',(#4147),#2267,.F.) ;
#32627 = ADVANCED_FACE('',(#4148),#761,.F.) ;
#32628 = ADVANCED_FACE('',(#4149),#30746,.T.) ;
#32629 = ADVANCED_FACE('',(#4150),#762,.F.) ;
#32630 = ADVANCED_FACE('',(#4151),#763,.F.) ;
#32631 = ADVANCED_FACE('',(#4152),#470,.T.) ;
#32632 = ADVANCED_FACE('',(#4153),#30747,.T.) ;
#32633 = ADVANCED_FACE('',(#4154,#1187),#2268,.T.) ;
#32634 = ADVANCED_FACE('',(#4155),#471,.T.) ;
#32635 = ADVANCED_FACE('',(#4156,#1188),#2269,.F.) ;
#32636 = ADVANCED_FACE('',(#4157),#30748,.F.) ;
#32637 = CLOSED_SHELL('',(#30749,#30750,#30751,#30752,#30753,#30754,#30755,
#30756,#30757,#30758,#30759,#30760,#30761,#30762,#30763,#30764,#30765,#30766,
#30767,#30768,#30769,#30770,#30771,#30772,#30773,#30774,#30775,#30776,#30777,
#30778,#30779,#30780,#30781,#30782,#30783,#30784,#30785,#30786,#30787,#30788,
#30789,#30790,#30791,#30792,#30793,#30794,#30795,#30796,#30797,#30798,#30799,
#30800,#30801,#30802,#30803,#30804,#30805,#30806,#30807,#30808,#30809,#30810,
#30811,#30812,#30813,#30814,#30815,#30816,#30817,#30818,#30819,#30820,#30821,
#30822,#30823,#30824,#30825,#30826,#30827,#30828,#30829,#30830,#30831,#30832,
#30833,#30834,#30835,#30836,#30837,#30838,#30839,#30840,#30841,#30842,#30843,
#30844,#30845,#30846,#30847,#30848,#30849,#30850,#30851,#30852,#30853,#30854,
#30855,#30856,#30857,#30858,#30859,#30860,#30861,#30862,#30863,#30864,#30865,
#30866,#30867,#30868,#30869,#30870,#30871,#30872,#30873,#30874,#30875,#30876)) ;
#32638 = CLOSED_SHELL('',(#30877,#30878,#30879,#30880,#30881,#30882,#30883,
#30884,#30885,#30886,#30887,#30888,#30889,#30890,#30891,#30892,#30893,#30894,
#30895,#30896,#30897,#30898,#30899,#30900,#30901,#30902,#30903,#30904,#30905,
#30906,#30907,#30908,#30909,#30910,#30911,#30912,#30913,#30914,#30915)) ;
#32639 = CLOSED_SHELL('',(#30916,#30917,#30918,#30919,#30920,#30921,#30922,
#30923,#30924,#30925,#30926,#30927,#30928,#30929,#30930,#30931,#30932,#30933,
#30934,#30935,#30936,#30937,#30938,#30939,#30940,#30941,#30942,#30943,#30944,
#30945,#30946,#30947,#30948,#30949,#30950,#30951,#30952,#30953,#30954,#30955,
#30956,#30957)) ;
#32640 = CLOSED_SHELL('',(#30958,#30959,#30960,#30961,#30962,#30963,#30964,
#30965,#30966,#30967,#30968,#30969,#30970,#30971,#30972,#30973,#30974,#30975,
#30976,#30977,#30978,#30979,#30980,#30981,#30982,#30983,#30984,#30985,#30986,
#30987,#30988,#30989,#30990,#30991,#30992,#30993,#30994,#30995,#30996,#30997,
#30998,#30999,#31000,#31001,#31002,#31003,#31004,#31005,#31006,#31007,#31008,
#31009,#31010,#31011,#31012,#31013,#31014,#31015,#31016,#31017,#31018,#31019,
#31020,#31021,#31022,#31023,#31024,#31025,#31026,#31027,#31028,#31029,#31030,
#31031,#31032,#31033,#31034,#31035,#31036,#31037,#31038,#31039,#31040,#31041,
#31042,#31043,#31044,#31045,#31046,#31047,#31048,#31049,#31050,#31051,#31052,
#31053,#31054,#31055,#31056,#31057,#31058,#31059,#31060,#31061,#31062,#31063,
#31064,#31065,#31066,#31067,#31068,#31069,#31070,#31071,#31072,#31073,#31074,
#31075,#31076,#31077,#31078,#31079,#31080,#31081,#31082,#31083,#31084,#31085,
#31086,#31087,#31088,#31089,#31090,#31091,#31092,#31093,#31094,#31095,#31096,
#31097,#31098,#31099,#31100,#31101,#31102,#31103,#31104,#31105,#31106,#31107,
#31108,#31109,#31110,#31111,#31112,#31113,#31114,#31115,#31116,#31117,#31118,
#31119,#31120,#31121,#31122,#31123,#31124,#31125,#31126,#31127,#31128,#31129,
#31130,#31131,#31132,#31133,#31134,#31135,#31136,#31137,#31138,#31139,#31140,
#31141,#31142,#31143,#31144,#31145,#31146,#31147,#31148,#31149,#31150,#31151,
#31152,#31153,#31154,#31155,#31156,#31157,#31158,#31159,#31160,#31161,#31162,
#31163,#31164,#31165,#31166,#31167,#31168,#31169,#31170,#31171,#31172,#31173,
#31174,#31175,#31176,#31177,#31178,#31179,#31180,#31181,#31182,#31183,#31184,
#31185,#31186,#31187,#31188,#31189,#31190,#31191,#31192,#31193,#31194,#31195,
#31196,#31197,#31198,#31199,#31200,#31201,#31202,#31203,#31204,#31205,#31206,
#31207,#31208,#31209,#31210,#31211,#31212,#31213,#31214,#31215,#31216,#31217,
#31218,#31219,#31220,#31221,#31222,#31223,#31224,#31225,#31226,#31227,#31228,
#31229,#31230,#31231,#31232,#31233,#31234,#31235,#31236,#31237,#31238,#31239,
#31240,#31241,#31242,#31243,#31244,#31245,#31246,#31247,#31248,#31249,#31250,
#31251,#31252,#31253,#31254,#31255,#31256,#31257,#31258)) ;
#32641 = CLOSED_SHELL('',(#31259,#31260,#31261,#31262,#31263,#31264,#31265,
#31266,#31267,#31268,#31269,#31270,#31271,#31272,#31273,#31274,#31275,#31276,
#31277,#31278,#31279,#31280,#31281,#31282,#31283,#31284,#31285,#31286,#31287,
#31288,#31289,#31290,#31291,#31292,#31293,#31294,#31295,#31296,#31297,#31298,
#31299,#31300,#31301,#31302,#31303,#31304,#31305,#31306,#31307,#31308,#31309,
#31310,#31311,#31312,#31313,#31314,#31315,#31316,#31317,#31318,#31319,#31320,
#31321,#31322,#31323,#31324,#31325,#31326,#31327,#31328,#31329,#31330,#31331,
#31332,#31333,#31334,#31335,#31336,#31337,#31338,#31339,#31340,#31341,#31342,
#31343,#31344,#31345,#31346,#31347,#31348,#31349,#31350,#31351,#31352,#31353,
#31354,#31355,#31356,#31357,#31358,#31359,#31360,#31361,#31362,#31363,#31364,
#31365,#31366,#31367,#31368,#31369,#31370,#31371,#31372,#31373,#31374,#31375,
#31376,#31377,#31378,#31379,#31380,#31381,#31382,#31383,#31384,#31385,#31386,
#31387,#31388,#31389,#31390,#31391,#31392,#31393,#31394,#31395,#31396,#31397,
#31398,#31399,#31400,#31401,#31402,#31403,#31404,#31405,#31406,#31407,#31408,
#31409,#31410,#31411,#31412,#31413,#31414,#31415,#31416,#31417,#31418,#31419,
#31420,#31421,#31422,#31423,#31424,#31425,#31426,#31427,#31428,#31429,#31430,
#31431,#31432,#31433,#31434,#31435,#31436,#31437,#31438,#31439,#31440,#31441,
#31442,#31443,#31444,#31445,#31446,#31447,#31448,#31449,#31450,#31451,#31452,
#31453,#31454,#31455,#31456,#31457,#31458,#31459,#31460,#31461,#31462,#31463,
#31464,#31465,#31466,#31467,#31468,#31469,#31470,#31471,#31472,#31473,#31474,
#31475,#31476,#31477,#31478,#31479,#31480,#31481,#31482,#31483,#31484,#31485,
#31486,#31487,#31488,#31489,#31490,#31491,#31492,#31493,#31494,#31495,#31496,
#31497,#31498,#31499,#31500,#31501,#31502,#31503,#31504,#31505,#31506,#31507,
#31508,#31509,#31510,#31511,#31512,#31513,#31514,#31515,#31516,#31517,#31518,
#31519,#31520,#31521,#31522,#31523,#31524,#31525,#31526,#31527,#31528,#31529,
#31530,#31531,#31532,#31533,#31534,#31535,#31536,#31537,#31538,#31539,#31540,
#31541,#31542,#31543,#31544,#31545,#31546,#31547,#31548,#31549,#31550,#31551,
#31552,#31553,#31554,#31555,#31556,#31557,#31558,#31559,#31560,#31561,#31562,
#31563,#31564,#31565,#31566,#31567,#31568,#31569,#31570,#31571,#31572,#31573,
#31574,#31575,#31576,#31577,#31578,#31579,#31580,#31581,#31582,#31583,#31584,
#31585,#31586,#31587,#31588,#31589,#31590,#31591,#31592,#31593,#31594,#31595,
#31596,#31597,#31598,#31599,#31600,#31601,#31602,#31603,#31604,#31605,#31606,
#31607,#31608,#31609,#31610,#31611,#31612,#31613,#31614,#31615,#31616,#31617,
#31618,#31619,#31620,#31621,#31622,#31623,#31624,#31625,#31626,#31627,#31628,
#31629,#31630,#31631,#31632,#31633,#31634,#31635,#31636,#31637,#31638,#31639,
#31640,#31641,#31642,#31643,#31644,#31645,#31646,#31647,#31648,#31649,#31650,
#31651,#31652,#31653,#31654,#31655,#31656,#31657,#31658,#31659,#31660,#31661,
#31662,#31663,#31664,#31665,#31666,#31667,#31668,#31669,#31670,#31671,#31672,
#31673,#31674,#31675,#31676,#31677,#31678,#31679,#31680,#31681,#31682,#31683,
#31684,#31685,#31686,#31687,#31688,#31689,#31690,#31691,#31692,#31693,#31694,
#31695,#31696,#31697,#31698,#31699,#31700,#31701,#31702,#31703,#31704,#31705,
#31706,#31707,#31708,#31709,#31710,#31711,#31712,#31713,#31714,#31715,#31716,
#31717,#31718,#31719,#31720,#31721,#31722,#31723,#31724,#31725,#31726,#31727,
#31728,#31729,#31730,#31731,#31732,#31733,#31734,#31735,#31736,#31737,#31738,
#31739,#31740,#31741,#31742,#31743,#31744,#31745,#31746,#31747,#31748,#31749,
#31750,#31751,#31752,#31753,#31754,#31755,#31756,#31757,#31758,#31759,#31760,
#31761,#31762,#31763,#31764,#31765,#31766,#31767,#31768,#31769,#31770,#31771,
#31772,#31773,#31774,#31775,#31776,#31777,#31778,#31779,#31780,#31781,#31782,
#31783,#31784,#31785,#31786,#31787,#31788,#31789,#31790,#31791,#31792,#31793,
#31794,#31795,#31796,#31797,#31798,#31799,#31800,#31801,#31802,#31803,#31804,
#31805,#31806,#31807,#31808,#31809,#31810,#31811,#31812,#31813,#31814,#31815,
#31816,#31817,#31818,#31819,#31820,#31821,#31822,#31823,#31824,#31825,#31826,
#31827,#31828,#31829,#31830,#31831,#31832,#31833,#31834,#31835,#31836,#31837,
#31838,#31839,#31840,#31841,#31842,#31843,#31844,#31845,#31846,#31847,#31848,
#31849,#31850,#31851,#31852,#31853,#31854,#31855,#31856,#31857,#31858,#31859,
#31860,#31861,#31862,#31863,#31864,#31865,#31866,#31867,#31868,#31869,#31870,
#31871,#31872,#31873,#31874,#31875,#31876,#31877,#31878,#31879,#31880,#31881,
#31882,#31883,#31884,#31885,#31886,#31887,#31888,#31889,#31890,#31891,#31892,
#31893,#31894,#31895,#31896,#31897,#31898,#31899,#31900,#31901,#31902,#31903,
#31904,#31905,#31906,#31907,#31908,#31909,#31910,#31911,#31912,#31913,#31914,
#31915,#31916,#31917,#31918,#31919,#31920,#31921,#31922,#31923,#31924,#31925,
#31926,#31927,#31928,#31929,#31930,#31931,#31932,#31933,#31934,#31935,#31936,
#31937,#31938,#31939,#31940,#31941,#31942,#31943,#31944,#31945,#31946,#31947,
#31948,#31949,#31950,#31951,#31952,#31953,#31954,#31955,#31956,#31957,#31958,
#31959,#31960,#31961,#31962,#31963,#31964,#31965,#31966,#31967,#31968,#31969,
#31970,#31971,#31972,#31973,#31974,#31975,#31976,#31977,#31978,#31979,#31980,
#31981,#31982,#31983,#31984,#31985,#31986,#31987,#31988,#31989,#31990,#31991,
#31992,#31993,#31994,#31995,#31996,#31997,#31998,#31999,#32000,#32001,#32002,
#32003,#32004,#32005,#32006,#32007,#32008,#32009,#32010,#32011,#32012,#32013,
#32014,#32015,#32016,#32017,#32018,#32019,#32020,#32021,#32022,#32023,#32024,
#32025,#32026,#32027,#32028,#32029,#32030,#32031,#32032,#32033,#32034,#32035,
#32036,#32037,#32038,#32039,#32040,#32041,#32042,#32043,#32044,#32045,#32046,
#32047,#32048,#32049,#32050,#32051,#32052,#32053,#32054,#32055,#32056,#32057,
#32058,#32059,#32060,#32061,#32062,#32063,#32064,#32065,#32066,#32067,#32068,
#32069,#32070,#32071,#32072,#32073,#32074,#32075,#32076,#32077,#32078,#32079,
#32080,#32081,#32082,#32083,#32084,#32085,#32086,#32087,#32088,#32089,#32090,
#32091,#32092,#32093,#32094,#32095,#32096,#32097,#32098,#32099,#32100,#32101,
#32102)) ;
#32642 = CLOSED_SHELL('',(#32103,#32104,#32105,#32106,#32107,#32108,#32109,
#32110,#32111,#32112,#32113,#32114,#32115,#32116,#32117,#32118,#32119,#32120,
#32121,#32122,#32123,#32124,#32125,#32126,#32127,#32128,#32129,#32130,#32131,
#32132,#32133,#32134,#32135,#32136,#32137,#32138,#32139,#32140,#32141,#32142,
#32143,#32144,#32145,#32146,#32147,#32148,#32149,#32150,#32151,#32152,#32153,
#32154,#32155,#32156,#32157,#32158,#32159,#32160,#32161,#32162,#32163,#32164,
#32165,#32166,#32167,#32168,#32169,#32170,#32171,#32172,#32173,#32174,#32175,
#32176,#32177,#32178,#32179,#32180,#32181,#32182,#32183,#32184,#32185,#32186,
#32187,#32188,#32189,#32190,#32191,#32192,#32193,#32194,#32195,#32196,#32197,
#32198,#32199,#32200,#32201,#32202,#32203,#32204,#32205,#32206,#32207,#32208,
#32209,#32210,#32211,#32212,#32213,#32214,#32215,#32216,#32217,#32218,#32219,
#32220,#32221,#32222,#32223,#32224,#32225,#32226,#32227,#32228,#32229,#32230,
#32231,#32232,#32233,#32234,#32235,#32236,#32237,#32238,#32239,#32240,#32241,
#32242,#32243,#32244,#32245,#32246,#32247,#32248,#32249,#32250,#32251,#32252,
#32253,#32254,#32255,#32256,#32257,#32258,#32259,#32260,#32261,#32262,#32263,
#32264,#32265,#32266,#32267,#32268,#32269,#32270,#32271,#32272,#32273,#32274,
#32275,#32276,#32277,#32278,#32279,#32280,#32281,#32282,#32283,#32284,#32285,
#32286,#32287,#32288,#32289,#32290,#32291,#32292,#32293,#32294,#32295,#32296,
#32297,#32298,#32299,#32300,#32301,#32302,#32303,#32304,#32305,#32306,#32307,
#32308,#32309,#32310,#32311,#32312,#32313,#32314,#32315,#32316,#32317,#32318,
#32319,#32320,#32321,#32322,#32323,#32324,#32325,#32326,#32327,#32328,#32329,
#32330,#32331)) ;
#32643 = CLOSED_SHELL('',(#32332,#32333,#32334,#32335,#32336,#32337,#32338,
#32339,#32340,#32341,#32342,#32343,#32344,#32345,#32346,#32347,#32348,#32349,
#32350,#32351,#32352,#32353,#32354,#32355,#32356,#32357,#32358,#32359,#32360,
#32361,#32362,#32363,#32364,#32365,#32366,#32367,#32368,#32369,#32370,#32371,
#32372,#32373,#32374,#32375,#32376,#32377,#32378,#32379,#32380,#32381,#32382,
#32383,#32384,#32385,#32386,#32387,#32388,#32389,#32390,#32391,#32392,#32393,
#32394,#32395,#32396,#32397,#32398,#32399,#32400,#32401,#32402,#32403,#32404,
#32405,#32406,#32407,#32408,#32409,#32410,#32411,#32412,#32413,#32414,#32415,
#32416,#32417,#32418,#32419,#32420,#32421,#32422,#32423,#32424,#32425,#32426,
#32427,#32428,#32429,#32430,#32431,#32432,#32433,#32434,#32435,#32436,#32437,
#32438,#32439)) ;
#32644 = CLOSED_SHELL('',(#32440,#32441,#32442,#32443,#32444,#32445,#32446,
#32447,#32448,#32449,#32450,#32451,#32452,#32453,#32454,#32455,#32456,#32457,
#32458,#32459,#32460,#32461,#32462,#32463,#32464,#32465,#32466,#32467,#32468,
#32469,#32470,#32471,#32472,#32473,#32474,#32475,#32476,#32477,#32478,#32479,
#32480,#32481,#32482,#32483,#32484,#32485,#32486,#32487,#32488,#32489,#32490,
#32491,#32492,#32493,#32494,#32495,#32496,#32497,#32498,#32499,#32500,#32501,
#32502,#32503,#32504,#32505,#32506,#32507,#32508,#32509,#32510,#32511,#32512,
#32513,#32514,#32515,#32516,#32517,#32518,#32519,#32520,#32521,#32522,#32523,
#32524,#32525,#32526,#32527,#32528,#32529,#32530,#32531,#32532,#32533,#32534,
#32535,#32536)) ;
#32645 = CLOSED_SHELL('',(#32537,#32538,#32539,#32540,#32541,#32542,#32543,
#32544,#32545,#32546,#32547,#32548,#32549,#32550,#32551,#32552,#32553,#32554,
#32555,#32556,#32557,#32558,#32559)) ;
#32646 = CLOSED_SHELL('',(#32560,#32561,#32562,#32563,#32564,#32565,#32566,
#32567,#32568,#32569,#32570,#32571,#32572,#32573,#32574,#32575,#32576,#32577,
#32578,#32579,#32580,#32581,#32582,#32583,#32584,#32585,#32586,#32587,#32588,
#32589,#32590,#32591,#32592,#32593,#32594,#32595,#32596,#32597,#32598,#32599,
#32600,#32601,#32602,#32603,#32604,#32605,#32606,#32607,#32608,#32609,#32610,
#32611,#32612,#32613,#32614,#32615,#32616,#32617,#32618,#32619,#32620,#32621,
#32622,#32623,#32624)) ;
#32647 = CLOSED_SHELL('',(#32625,#32626,#32627,#32628,#32629,#32630)) ;
#32648 = CLOSED_SHELL('',(#32631,#32632,#32633,#32634,#32635,#32636)) ;
#32649 = DERIVED_UNIT_ELEMENT(#32671,1.) ;
#32650 = DERIVED_UNIT_ELEMENT(#86332,-3.) ;
#32651 = DERIVED_UNIT_ELEMENT(#32671,1.) ;
#32652 = DERIVED_UNIT_ELEMENT(#86332,-3.) ;
#32653 = DERIVED_UNIT_ELEMENT(#32671,1.) ;
#32654 = DERIVED_UNIT_ELEMENT(#86332,-3.) ;
#32655 = DERIVED_UNIT_ELEMENT(#32671,1.) ;
#32656 = DERIVED_UNIT_ELEMENT(#86332,-3.) ;
#32657 = DERIVED_UNIT_ELEMENT(#32671,1.) ;
#32658 = DERIVED_UNIT_ELEMENT(#86332,-3.) ;
#32659 = DERIVED_UNIT_ELEMENT(#32671,1.) ;
#32660 = DERIVED_UNIT_ELEMENT(#86332,-3.) ;
#32661 = DERIVED_UNIT_ELEMENT(#32671,1.) ;
#32662 = DERIVED_UNIT_ELEMENT(#86332,-3.) ;
#32663 = DERIVED_UNIT_ELEMENT(#32671,1.) ;
#32664 = DERIVED_UNIT_ELEMENT(#86332,-3.) ;
#32665 = DERIVED_UNIT_ELEMENT(#32671,1.) ;
#32666 = DERIVED_UNIT_ELEMENT(#86332,-3.) ;
#32667 = DERIVED_UNIT_ELEMENT(#32671,1.) ;
#32668 = DERIVED_UNIT_ELEMENT(#86332,-3.) ;
#32669 = DERIVED_UNIT_ELEMENT(#32671,1.) ;
#32670 = DERIVED_UNIT_ELEMENT(#86332,-3.) ;
#32671 = (
MASS_UNIT()
NAMED_UNIT(*)
SI_UNIT(.KILO.,.GRAM.)
) ;
#32672 = DERIVED_UNIT((#32649,#32650)) ;
#32673 = DERIVED_UNIT((#32651,#32652)) ;
#32674 = DERIVED_UNIT((#32653,#32654)) ;
#32675 = DERIVED_UNIT((#32655,#32656)) ;
#32676 = DERIVED_UNIT((#32657,#32658)) ;
#32677 = DERIVED_UNIT((#32659,#32660)) ;
#32678 = DERIVED_UNIT((#32661,#32662)) ;
#32679 = DERIVED_UNIT((#32663,#32664)) ;
#32680 = DERIVED_UNIT((#32665,#32666)) ;
#32681 = DERIVED_UNIT((#32667,#32668)) ;
#32682 = DERIVED_UNIT((#32669,#32670)) ;
#32683 = MEASURE_REPRESENTATION_ITEM('density measure',
POSITIVE_RATIO_MEASURE(7850.),#32672) ;
#32684 = MEASURE_REPRESENTATION_ITEM('density measure',
POSITIVE_RATIO_MEASURE(7850.),#32673) ;
#32685 = MEASURE_REPRESENTATION_ITEM('density measure',
POSITIVE_RATIO_MEASURE(7850.),#32674) ;
#32686 = MEASURE_REPRESENTATION_ITEM('density measure',
POSITIVE_RATIO_MEASURE(7850.),#32675) ;
#32687 = MEASURE_REPRESENTATION_ITEM('density measure',
POSITIVE_RATIO_MEASURE(7850.),#32676) ;
#32688 = MEASURE_REPRESENTATION_ITEM('density measure',
POSITIVE_RATIO_MEASURE(7850.),#32677) ;
#32689 = MEASURE_REPRESENTATION_ITEM('density measure',
POSITIVE_RATIO_MEASURE(7850.),#32678) ;
#32690 = MEASURE_REPRESENTATION_ITEM('density measure',
POSITIVE_RATIO_MEASURE(7850.),#32679) ;
#32691 = MEASURE_REPRESENTATION_ITEM('density measure',
POSITIVE_RATIO_MEASURE(7850.),#32680) ;
#32692 = MEASURE_REPRESENTATION_ITEM('density measure',
POSITIVE_RATIO_MEASURE(7850.),#32681) ;
#32693 = MEASURE_REPRESENTATION_ITEM('density measure',
POSITIVE_RATIO_MEASURE(7850.),#32682) ;
#32694 = PROPERTY_DEFINITION_REPRESENTATION(#32749,#32716) ;
#32695 = PROPERTY_DEFINITION_REPRESENTATION(#32750,#32717) ;
#32696 = PROPERTY_DEFINITION_REPRESENTATION(#32751,#32718) ;
#32697 = PROPERTY_DEFINITION_REPRESENTATION(#32752,#32719) ;
#32698 = PROPERTY_DEFINITION_REPRESENTATION(#32753,#32720) ;
#32699 = PROPERTY_DEFINITION_REPRESENTATION(#32754,#32721) ;
#32700 = PROPERTY_DEFINITION_REPRESENTATION(#32755,#32722) ;
#32701 = PROPERTY_DEFINITION_REPRESENTATION(#32756,#32723) ;
#32702 = PROPERTY_DEFINITION_REPRESENTATION(#32757,#32724) ;
#32703 = PROPERTY_DEFINITION_REPRESENTATION(#32758,#32725) ;
#32704 = PROPERTY_DEFINITION_REPRESENTATION(#32759,#32726) ;
#32705 = PROPERTY_DEFINITION_REPRESENTATION(#32760,#32727) ;
#32706 = PROPERTY_DEFINITION_REPRESENTATION(#32761,#32728) ;
#32707 = PROPERTY_DEFINITION_REPRESENTATION(#32762,#32729) ;
#32708 = PROPERTY_DEFINITION_REPRESENTATION(#32763,#32730) ;
#32709 = PROPERTY_DEFINITION_REPRESENTATION(#32764,#32731) ;
#32710 = PROPERTY_DEFINITION_REPRESENTATION(#32765,#32732) ;
#32711 = PROPERTY_DEFINITION_REPRESENTATION(#32766,#32733) ;
#32712 = PROPERTY_DEFINITION_REPRESENTATION(#32767,#32734) ;
#32713 = PROPERTY_DEFINITION_REPRESENTATION(#32768,#32735) ;
#32714 = PROPERTY_DEFINITION_REPRESENTATION(#32769,#32736) ;
#32715 = PROPERTY_DEFINITION_REPRESENTATION(#32770,#32737) ;
#32716 = REPRESENTATION('material name',(#32738),#86307) ;
#32717 = REPRESENTATION('density',(#32683),#86307) ;
#32718 = REPRESENTATION('material name',(#32739),#86310) ;
#32719 = REPRESENTATION('density',(#32684),#86310) ;
#32720 = REPRESENTATION('material name',(#32740),#86312) ;
#32721 = REPRESENTATION('density',(#32685),#86312) ;
#32722 = REPRESENTATION('material name',(#32741),#86315) ;
#32723 = REPRESENTATION('density',(#32686),#86315) ;
#32724 = REPRESENTATION('material name',(#32742),#86317) ;
#32725 = REPRESENTATION('density',(#32687),#86317) ;
#32726 = REPRESENTATION('material name',(#32743),#86319) ;
#32727 = REPRESENTATION('density',(#32688),#86319) ;
#32728 = REPRESENTATION('material name',(#32744),#86321) ;
#32729 = REPRESENTATION('density',(#32689),#86321) ;
#32730 = REPRESENTATION('material name',(#32745),#86322) ;
#32731 = REPRESENTATION('density',(#32690),#86322) ;
#32732 = REPRESENTATION('material name',(#32746),#86327) ;
#32733 = REPRESENTATION('density',(#32691),#86327) ;
#32734 = REPRESENTATION('material name',(#32747),#86328) ;
#32735 = REPRESENTATION('density',(#32692),#86328) ;
#32736 = REPRESENTATION('material name',(#32748),#86329) ;
#32737 = REPRESENTATION('density',(#32693),#86329) ;
#32738 = DESCRIPTIVE_REPRESENTATION_ITEM('Steel','Steel') ;
#32739 = DESCRIPTIVE_REPRESENTATION_ITEM('Steel','Steel') ;
#32740 = DESCRIPTIVE_REPRESENTATION_ITEM('Steel','Steel') ;
#32741 = DESCRIPTIVE_REPRESENTATION_ITEM('Steel','Steel') ;
#32742 = DESCRIPTIVE_REPRESENTATION_ITEM('Steel','Steel') ;
#32743 = DESCRIPTIVE_REPRESENTATION_ITEM('Steel','Steel') ;
#32744 = DESCRIPTIVE_REPRESENTATION_ITEM('Steel','Steel') ;
#32745 = DESCRIPTIVE_REPRESENTATION_ITEM('Steel','Steel') ;
#32746 = DESCRIPTIVE_REPRESENTATION_ITEM('Steel','Steel') ;
#32747 = DESCRIPTIVE_REPRESENTATION_ITEM('Steel AISI 4340 242 HR',
'Steel AISI 4340 242 HR') ;
#32748 = DESCRIPTIVE_REPRESENTATION_ITEM('Steel','Steel') ;
#32749 = PROPERTY_DEFINITION('material property','material name',#86479) ;
#32750 = PROPERTY_DEFINITION('material property','density of part',#86479) ;
#32751 = PROPERTY_DEFINITION('material property','material name',#86482) ;
#32752 = PROPERTY_DEFINITION('material property','density of part',#86482) ;
#32753 = PROPERTY_DEFINITION('material property','material name',#86484) ;
#32754 = PROPERTY_DEFINITION('material property','density of part',#86484) ;
#32755 = PROPERTY_DEFINITION('material property','material name',#86487) ;
#32756 = PROPERTY_DEFINITION('material property','density of part',#86487) ;
#32757 = PROPERTY_DEFINITION('material property','material name',#86489) ;
#32758 = PROPERTY_DEFINITION('material property','density of part',#86489) ;
#32759 = PROPERTY_DEFINITION('material property','material name',#86491) ;
#32760 = PROPERTY_DEFINITION('material property','density of part',#86491) ;
#32761 = PROPERTY_DEFINITION('material property','material name',#86493) ;
#32762 = PROPERTY_DEFINITION('material property','density of part',#86493) ;
#32763 = PROPERTY_DEFINITION('material property','material name',#86494) ;
#32764 = PROPERTY_DEFINITION('material property','density of part',#86494) ;
#32765 = PROPERTY_DEFINITION('material property','material name',#86499) ;
#32766 = PROPERTY_DEFINITION('material property','density of part',#86499) ;
#32767 = PROPERTY_DEFINITION('material property','material name',#86500) ;
#32768 = PROPERTY_DEFINITION('material property','density of part',#86500) ;
#32769 = PROPERTY_DEFINITION('material property','material name',#86501) ;
#32770 = PROPERTY_DEFINITION('material property','density of part',#86501) ;
#32771 = AXIS2_PLACEMENT_3D('',#46346,#36523,#36524) ;
#32772 = AXIS2_PLACEMENT_3D('',#46347,#36525,#36526) ;
#32773 = AXIS2_PLACEMENT_3D('',#46348,#36527,#36528) ;
#32774 = AXIS2_PLACEMENT_3D('',#46349,#36529,#36530) ;
#32775 = AXIS2_PLACEMENT_3D('',#46352,#36531,#36532) ;
#32776 = AXIS2_PLACEMENT_3D('',#46356,#36534,#36535) ;
#32777 = AXIS2_PLACEMENT_3D('',#46358,#36537,#36538) ;
#32778 = AXIS2_PLACEMENT_3D('',#46370,#36544,#36545) ;
#32779 = AXIS2_PLACEMENT_3D('',#46380,#36546,#36547) ;
#32780 = AXIS2_PLACEMENT_3D('',#46381,#36548,#36549) ;
#32781 = AXIS2_PLACEMENT_3D('',#46392,#36550,#36551) ;
#32782 = AXIS2_PLACEMENT_3D('',#46394,#36552,#36553) ;
#32783 = AXIS2_PLACEMENT_3D('',#46395,#36554,#36555) ;
#32784 = AXIS2_PLACEMENT_3D('',#46398,#36556,#36557) ;
#32785 = AXIS2_PLACEMENT_3D('',#46400,#36558,#36559) ;
#32786 = AXIS2_PLACEMENT_3D('',#46402,#36560,#36561) ;
#32787 = AXIS2_PLACEMENT_3D('',#46403,#36562,#36563) ;
#32788 = AXIS2_PLACEMENT_3D('',#46406,#36564,#36565) ;
#32789 = AXIS2_PLACEMENT_3D('',#46408,#36566,#36567) ;
#32790 = AXIS2_PLACEMENT_3D('',#46410,#36568,#36569) ;
#32791 = AXIS2_PLACEMENT_3D('',#46411,#36570,#36571) ;
#32792 = AXIS2_PLACEMENT_3D('',#46416,#36573,#36574) ;
#32793 = AXIS2_PLACEMENT_3D('',#46419,#36576,#36577) ;
#32794 = AXIS2_PLACEMENT_3D('',#46424,#36579,#36580) ;
#32795 = AXIS2_PLACEMENT_3D('',#46427,#36582,#36583) ;
#32796 = AXIS2_PLACEMENT_3D('',#46432,#36585,#36586) ;
#32797 = AXIS2_PLACEMENT_3D('',#46435,#36588,#36589) ;
#32798 = AXIS2_PLACEMENT_3D('',#46440,#36591,#36592) ;
#32799 = AXIS2_PLACEMENT_3D('',#46443,#36594,#36595) ;
#32800 = AXIS2_PLACEMENT_3D('',#46448,#36597,#36598) ;
#32801 = AXIS2_PLACEMENT_3D('',#46451,#36600,#36601) ;
#32802 = AXIS2_PLACEMENT_3D('',#46456,#36603,#36604) ;
#32803 = AXIS2_PLACEMENT_3D('',#46459,#36606,#36607) ;
#32804 = AXIS2_PLACEMENT_3D('',#46461,#36608,#36609) ;
#32805 = AXIS2_PLACEMENT_3D('',#46463,#36610,#36611) ;
#32806 = AXIS2_PLACEMENT_3D('',#46465,#36612,#36613) ;
#32807 = AXIS2_PLACEMENT_3D('',#46467,#36614,#36615) ;
#32808 = AXIS2_PLACEMENT_3D('',#46469,#36616,#36617) ;
#32809 = AXIS2_PLACEMENT_3D('',#46471,#36618,#36619) ;
#32810 = AXIS2_PLACEMENT_3D('',#46474,#36620,#36621) ;
#32811 = AXIS2_PLACEMENT_3D('',#46476,#36622,#36623) ;
#32812 = AXIS2_PLACEMENT_3D('',#46478,#36624,#36625) ;
#32813 = AXIS2_PLACEMENT_3D('',#46479,#36626,#36627) ;
#32814 = AXIS2_PLACEMENT_3D('',#46482,#36628,#36629) ;
#32815 = AXIS2_PLACEMENT_3D('',#46484,#36630,#36631) ;
#32816 = AXIS2_PLACEMENT_3D('',#46486,#36632,#36633) ;
#32817 = AXIS2_PLACEMENT_3D('',#46487,#36634,#36635) ;
#32818 = AXIS2_PLACEMENT_3D('',#46490,#36636,#36637) ;
#32819 = AXIS2_PLACEMENT_3D('',#46492,#36638,#36639) ;
#32820 = AXIS2_PLACEMENT_3D('',#46494,#36640,#36641) ;
#32821 = AXIS2_PLACEMENT_3D('',#46495,#36642,#36643) ;
#32822 = AXIS2_PLACEMENT_3D('',#46498,#36644,#36645) ;
#32823 = AXIS2_PLACEMENT_3D('',#46500,#36646,#36647) ;
#32824 = AXIS2_PLACEMENT_3D('',#46502,#36648,#36649) ;
#32825 = AXIS2_PLACEMENT_3D('',#46503,#36650,#36651) ;
#32826 = AXIS2_PLACEMENT_3D('',#46504,#36652,#36653) ;
#32827 = AXIS2_PLACEMENT_3D('',#46506,#36654,#36655) ;
#32828 = AXIS2_PLACEMENT_3D('',#46508,#36656,#36657) ;
#32829 = AXIS2_PLACEMENT_3D('',#46510,#36659,#36660) ;
#32830 = AXIS2_PLACEMENT_3D('',#46512,#36661,#36662) ;
#32831 = AXIS2_PLACEMENT_3D('',#46515,#36664,#36665) ;
#32832 = AXIS2_PLACEMENT_3D('',#46516,#36666,#36667) ;
#32833 = AXIS2_PLACEMENT_3D('',#46520,#36669,#36670) ;
#32834 = AXIS2_PLACEMENT_3D('',#46524,#36672,#36673) ;
#32835 = AXIS2_PLACEMENT_3D('',#46528,#36675,#36676) ;
#32836 = AXIS2_PLACEMENT_3D('',#46532,#36678,#36679) ;
#32837 = AXIS2_PLACEMENT_3D('',#46536,#36681,#36682) ;
#32838 = AXIS2_PLACEMENT_3D('',#46540,#36684,#36685) ;
#32839 = AXIS2_PLACEMENT_3D('',#46544,#36687,#36688) ;
#32840 = AXIS2_PLACEMENT_3D('',#46548,#36690,#36691) ;
#32841 = AXIS2_PLACEMENT_3D('',#46551,#36693,#36694) ;
#32842 = AXIS2_PLACEMENT_3D('',#46553,#36695,#36696) ;
#32843 = AXIS2_PLACEMENT_3D('',#46554,#36697,#36698) ;
#32844 = AXIS2_PLACEMENT_3D('',#46557,#36699,#36700) ;
#32845 = AXIS2_PLACEMENT_3D('',#46561,#36702,#36703) ;
#32846 = AXIS2_PLACEMENT_3D('',#46563,#36705,#36706) ;
#32847 = AXIS2_PLACEMENT_3D('',#46572,#36712,#36713) ;
#32848 = AXIS2_PLACEMENT_3D('',#46576,#36715,#36716) ;
#32849 = AXIS2_PLACEMENT_3D('',#46580,#36718,#36719) ;
#32850 = AXIS2_PLACEMENT_3D('',#46584,#36721,#36722) ;
#32851 = AXIS2_PLACEMENT_3D('',#46588,#36724,#36725) ;
#32852 = AXIS2_PLACEMENT_3D('',#46592,#36727,#36728) ;
#32853 = AXIS2_PLACEMENT_3D('',#46596,#36730,#36731) ;
#32854 = AXIS2_PLACEMENT_3D('',#46600,#36733,#36734) ;
#32855 = AXIS2_PLACEMENT_3D('',#46603,#36736,#36737) ;
#32856 = AXIS2_PLACEMENT_3D('',#46605,#36738,#36739) ;
#32857 = AXIS2_PLACEMENT_3D('',#46607,#36740,#36741) ;
#32858 = AXIS2_PLACEMENT_3D('',#46608,#36742,#36743) ;
#32859 = AXIS2_PLACEMENT_3D('',#46611,#36744,#36745) ;
#32860 = AXIS2_PLACEMENT_3D('',#46615,#36747,#36748) ;
#32861 = AXIS2_PLACEMENT_3D('',#46617,#36750,#36751) ;
#32862 = AXIS2_PLACEMENT_3D('',#46624,#36756,#36757) ;
#32863 = AXIS2_PLACEMENT_3D('',#46628,#36759,#36760) ;
#32864 = AXIS2_PLACEMENT_3D('',#46632,#36762,#36763) ;
#32865 = AXIS2_PLACEMENT_3D('',#46636,#36765,#36766) ;
#32866 = AXIS2_PLACEMENT_3D('',#46640,#36768,#36769) ;
#32867 = AXIS2_PLACEMENT_3D('',#46644,#36771,#36772) ;
#32868 = AXIS2_PLACEMENT_3D('',#46648,#36774,#36775) ;
#32869 = AXIS2_PLACEMENT_3D('',#46652,#36777,#36778) ;
#32870 = AXIS2_PLACEMENT_3D('',#46655,#36780,#36781) ;
#32871 = AXIS2_PLACEMENT_3D('',#46657,#36782,#36783) ;
#32872 = AXIS2_PLACEMENT_3D('',#46659,#36784,#36785) ;
#32873 = AXIS2_PLACEMENT_3D('',#46660,#36786,#36787) ;
#32874 = AXIS2_PLACEMENT_3D('',#46664,#36789,#36790) ;
#32875 = AXIS2_PLACEMENT_3D('',#46666,#36792,#36793) ;
#32876 = AXIS2_PLACEMENT_3D('',#46670,#36796,#36797) ;
#32877 = AXIS2_PLACEMENT_3D('',#46673,#36800,#36801) ;
#32878 = AXIS2_PLACEMENT_3D('',#46675,#36803,#36804) ;
#32879 = AXIS2_PLACEMENT_3D('',#46678,#36805,#36806) ;
#32880 = AXIS2_PLACEMENT_3D('',#46682,#36808,#36809) ;
#32881 = AXIS2_PLACEMENT_3D('',#46684,#36811,#36812) ;
#32882 = AXIS2_PLACEMENT_3D('',#46691,#36817,#36818) ;
#32883 = AXIS2_PLACEMENT_3D('',#46704,#36825,#36826) ;
#32884 = AXIS2_PLACEMENT_3D('',#46706,#36827,#36828) ;
#32885 = AXIS2_PLACEMENT_3D('',#46708,#36829,#36830) ;
#32886 = AXIS2_PLACEMENT_3D('',#46709,#36831,#36832) ;
#32887 = AXIS2_PLACEMENT_3D('',#46711,#36833,#36834) ;
#32888 = AXIS2_PLACEMENT_3D('',#46713,#36835,#36836) ;
#32889 = AXIS2_PLACEMENT_3D('',#46716,#36837,#36838) ;
#32890 = AXIS2_PLACEMENT_3D('',#46720,#36840,#36841) ;
#32891 = AXIS2_PLACEMENT_3D('',#46724,#36843,#36844) ;
#32892 = AXIS2_PLACEMENT_3D('',#46728,#36846,#36847) ;
#32893 = AXIS2_PLACEMENT_3D('',#46732,#36849,#36850) ;
#32894 = AXIS2_PLACEMENT_3D('',#46736,#36852,#36853) ;
#32895 = AXIS2_PLACEMENT_3D('',#46740,#36855,#36856) ;
#32896 = AXIS2_PLACEMENT_3D('',#46744,#36858,#36859) ;
#32897 = AXIS2_PLACEMENT_3D('',#46748,#36861,#36862) ;
#32898 = AXIS2_PLACEMENT_3D('',#46752,#36864,#36865) ;
#32899 = AXIS2_PLACEMENT_3D('',#46756,#36867,#36868) ;
#32900 = AXIS2_PLACEMENT_3D('',#46760,#36870,#36871) ;
#32901 = AXIS2_PLACEMENT_3D('',#46763,#36873,#36874) ;
#32902 = AXIS2_PLACEMENT_3D('',#46765,#36875,#36876) ;
#32903 = AXIS2_PLACEMENT_3D('',#46767,#36877,#36878) ;
#32904 = AXIS2_PLACEMENT_3D('',#46769,#36879,#36880) ;
#32905 = AXIS2_PLACEMENT_3D('',#46772,#36881,#36882) ;
#32906 = AXIS2_PLACEMENT_3D('',#46774,#36883,#36884) ;
#32907 = AXIS2_PLACEMENT_3D('',#46776,#36885,#36886) ;
#32908 = AXIS2_PLACEMENT_3D('',#46777,#36887,#36888) ;
#32909 = AXIS2_PLACEMENT_3D('',#46780,#36889,#36890) ;
#32910 = AXIS2_PLACEMENT_3D('',#46782,#36891,#36892) ;
#32911 = AXIS2_PLACEMENT_3D('',#46784,#36893,#36894) ;
#32912 = AXIS2_PLACEMENT_3D('',#46785,#36895,#36896) ;
#32913 = AXIS2_PLACEMENT_3D('',#46788,#36897,#36898) ;
#32914 = AXIS2_PLACEMENT_3D('',#46790,#36899,#36900) ;
#32915 = AXIS2_PLACEMENT_3D('',#46792,#36901,#36902) ;
#32916 = AXIS2_PLACEMENT_3D('',#46793,#36903,#36904) ;
#32917 = AXIS2_PLACEMENT_3D('',#46796,#36905,#36906) ;
#32918 = AXIS2_PLACEMENT_3D('',#46798,#36907,#36908) ;
#32919 = AXIS2_PLACEMENT_3D('',#46800,#36909,#36910) ;
#32920 = AXIS2_PLACEMENT_3D('',#46801,#36911,#36912) ;
#32921 = AXIS2_PLACEMENT_3D('',#46804,#36913,#36914) ;
#32922 = AXIS2_PLACEMENT_3D('',#46806,#36915,#36916) ;
#32923 = AXIS2_PLACEMENT_3D('',#46808,#36917,#36918) ;
#32924 = AXIS2_PLACEMENT_3D('',#46809,#36919,#36920) ;
#32925 = AXIS2_PLACEMENT_3D('',#46812,#36921,#36922) ;
#32926 = AXIS2_PLACEMENT_3D('',#46814,#36923,#36924) ;
#32927 = AXIS2_PLACEMENT_3D('',#46816,#36925,#36926) ;
#32928 = AXIS2_PLACEMENT_3D('',#46826,#36927,#36928) ;
#32929 = AXIS2_PLACEMENT_3D('',#46828,#36929,#36930) ;
#32930 = AXIS2_PLACEMENT_3D('',#46830,#36931,#36932) ;
#32931 = AXIS2_PLACEMENT_3D('',#46838,#36933,#36934) ;
#32932 = AXIS2_PLACEMENT_3D('',#46840,#36935,#36936) ;
#32933 = AXIS2_PLACEMENT_3D('',#46844,#36938,#36939) ;
#32934 = AXIS2_PLACEMENT_3D('',#46848,#36941,#36942) ;
#32935 = AXIS2_PLACEMENT_3D('',#46852,#36944,#36945) ;
#32936 = AXIS2_PLACEMENT_3D('',#46856,#36947,#36948) ;
#32937 = AXIS2_PLACEMENT_3D('',#46860,#36950,#36951) ;
#32938 = AXIS2_PLACEMENT_3D('',#46863,#36953,#36954) ;
#32939 = AXIS2_PLACEMENT_3D('',#46866,#36956,#36957) ;
#32940 = AXIS2_PLACEMENT_3D('',#46868,#36958,#36959) ;
#32941 = AXIS2_PLACEMENT_3D('',#46869,#36960,#36961) ;
#32942 = AXIS2_PLACEMENT_3D('',#46873,#36963,#36964) ;
#32943 = AXIS2_PLACEMENT_3D('',#46876,#36966,#36967) ;
#32944 = AXIS2_PLACEMENT_3D('',#46877,#36968,#36969) ;
#32945 = AXIS2_PLACEMENT_3D('',#46880,#36972,#36973) ;
#32946 = AXIS2_PLACEMENT_3D('',#46882,#36975,#36976) ;
#32947 = AXIS2_PLACEMENT_3D('',#46885,#36979,#36980) ;
#32948 = AXIS2_PLACEMENT_3D('',#46887,#36982,#36983) ;
#32949 = AXIS2_PLACEMENT_3D('',#46919,#36987,#36988) ;
#32950 = AXIS2_PLACEMENT_3D('',#46921,#36990,#36991) ;
#32951 = AXIS2_PLACEMENT_3D('',#46953,#36995,#36996) ;
#32952 = AXIS2_PLACEMENT_3D('',#46955,#36998,#36999) ;
#32953 = AXIS2_PLACEMENT_3D('',#46957,#37001,#37002) ;
#32954 = AXIS2_PLACEMENT_3D('',#46959,#37004,#37005) ;
#32955 = AXIS2_PLACEMENT_3D('',#46962,#37007,#37008) ;
#32956 = AXIS2_PLACEMENT_3D('',#46963,#37009,#37010) ;
#32957 = AXIS2_PLACEMENT_3D('',#46967,#37013,#37014) ;
#32958 = AXIS2_PLACEMENT_3D('',#46970,#37016,#37017) ;
#32959 = AXIS2_PLACEMENT_3D('',#46971,#37018,#37019) ;
#32960 = AXIS2_PLACEMENT_3D('',#46974,#37022,#37023) ;
#32961 = AXIS2_PLACEMENT_3D('',#46975,#37024,#37025) ;
#32962 = AXIS2_PLACEMENT_3D('',#46978,#37026,#37027) ;
#32963 = AXIS2_PLACEMENT_3D('',#46982,#37029,#37030) ;
#32964 = AXIS2_PLACEMENT_3D('',#46984,#37032,#37033) ;
#32965 = AXIS2_PLACEMENT_3D('',#46990,#37037,#37038) ;
#32966 = AXIS2_PLACEMENT_3D('',#46997,#37042,#37043) ;
#32967 = AXIS2_PLACEMENT_3D('',#46998,#37044,#37045) ;
#32968 = AXIS2_PLACEMENT_3D('',#47000,#37046,#37047) ;
#32969 = AXIS2_PLACEMENT_3D('',#47002,#37049,#37050) ;
#32970 = AXIS2_PLACEMENT_3D('',#47004,#37051,#37052) ;
#32971 = AXIS2_PLACEMENT_3D('',#47006,#37054,#37055) ;
#32972 = AXIS2_PLACEMENT_3D('',#47008,#37057,#37058) ;
#32973 = AXIS2_PLACEMENT_3D('',#47010,#37060,#37061) ;
#32974 = AXIS2_PLACEMENT_3D('',#47011,#37062,#37063) ;
#32975 = AXIS2_PLACEMENT_3D('',#47014,#37066,#37067) ;
#32976 = AXIS2_PLACEMENT_3D('',#47016,#37069,#37070) ;
#32977 = AXIS2_PLACEMENT_3D('',#47019,#37073,#37074) ;
#32978 = AXIS2_PLACEMENT_3D('',#47021,#37076,#37077) ;
#32979 = AXIS2_PLACEMENT_3D('',#47022,#37078,#37079) ;
#32980 = AXIS2_PLACEMENT_3D('',#47025,#37082,#37083) ;
#32981 = AXIS2_PLACEMENT_3D('',#47027,#37085,#37086) ;
#32982 = AXIS2_PLACEMENT_3D('',#47030,#37089,#37090) ;
#32983 = AXIS2_PLACEMENT_3D('',#47031,#37091,#37092) ;
#32984 = AXIS2_PLACEMENT_3D('',#47033,#37094,#37095) ;
#32985 = AXIS2_PLACEMENT_3D('',#47036,#37098,#37099) ;
#32986 = AXIS2_PLACEMENT_3D('',#47038,#37101,#37102) ;
#32987 = AXIS2_PLACEMENT_3D('',#47040,#37104,#37105) ;
#32988 = AXIS2_PLACEMENT_3D('',#47042,#37107,#37108) ;
#32989 = AXIS2_PLACEMENT_3D('',#47043,#37109,#37110) ;
#32990 = AXIS2_PLACEMENT_3D('',#47046,#37113,#37114) ;
#32991 = AXIS2_PLACEMENT_3D('',#47048,#37116,#37117) ;
#32992 = AXIS2_PLACEMENT_3D('',#47050,#37119,#37120) ;
#32993 = AXIS2_PLACEMENT_3D('',#47052,#37122,#37123) ;
#32994 = AXIS2_PLACEMENT_3D('',#47054,#37125,#37126) ;
#32995 = AXIS2_PLACEMENT_3D('',#47055,#37127,#37128) ;
#32996 = AXIS2_PLACEMENT_3D('',#47056,#37129,#37130) ;
#32997 = AXIS2_PLACEMENT_3D('',#47057,#37131,#37132) ;
#32998 = AXIS2_PLACEMENT_3D('',#47060,#37134,#37135) ;
#32999 = AXIS2_PLACEMENT_3D('',#47061,#37136,#37137) ;
#33000 = AXIS2_PLACEMENT_3D('',#47062,#37138,#37139) ;
#33001 = AXIS2_PLACEMENT_3D('',#47063,#37140,#37141) ;
#33002 = AXIS2_PLACEMENT_3D('',#47065,#37143,#37144) ;
#33003 = AXIS2_PLACEMENT_3D('',#47067,#37146,#37147) ;
#33004 = AXIS2_PLACEMENT_3D('',#47068,#37148,#37149) ;
#33005 = AXIS2_PLACEMENT_3D('',#47070,#37151,#37152) ;
#33006 = AXIS2_PLACEMENT_3D('',#47073,#37155,#37156) ;
#33007 = AXIS2_PLACEMENT_3D('',#47076,#37159,#37160) ;
#33008 = AXIS2_PLACEMENT_3D('',#47077,#37161,#37162) ;
#33009 = AXIS2_PLACEMENT_3D('',#47078,#37163,#37164) ;
#33010 = AXIS2_PLACEMENT_3D('',#47079,#37165,#37166) ;
#33011 = AXIS2_PLACEMENT_3D('',#47081,#37168,#37169) ;
#33012 = AXIS2_PLACEMENT_3D('',#47083,#37171,#37172) ;
#33013 = AXIS2_PLACEMENT_3D('',#47084,#37173,#37174) ;
#33014 = AXIS2_PLACEMENT_3D('',#47085,#37175,#37176) ;
#33015 = AXIS2_PLACEMENT_3D('',#47087,#37178,#37179) ;
#33016 = AXIS2_PLACEMENT_3D('',#47089,#37181,#37182) ;
#33017 = AXIS2_PLACEMENT_3D('',#47091,#37184,#37185) ;
#33018 = AXIS2_PLACEMENT_3D('',#47093,#37187,#37188) ;
#33019 = AXIS2_PLACEMENT_3D('',#47096,#37191,#37192) ;
#33020 = AXIS2_PLACEMENT_3D('',#47098,#37194,#37195) ;
#33021 = AXIS2_PLACEMENT_3D('',#47100,#37197,#37198) ;
#33022 = AXIS2_PLACEMENT_3D('',#47101,#37199,#37200) ;
#33023 = AXIS2_PLACEMENT_3D('',#47104,#37203,#37204) ;
#33024 = AXIS2_PLACEMENT_3D('',#47106,#37206,#37207) ;
#33025 = AXIS2_PLACEMENT_3D('',#47108,#37209,#37210) ;
#33026 = AXIS2_PLACEMENT_3D('',#47109,#37211,#37212) ;
#33027 = AXIS2_PLACEMENT_3D('',#47112,#37215,#37216) ;
#33028 = AXIS2_PLACEMENT_3D('',#47114,#37218,#37219) ;
#33029 = AXIS2_PLACEMENT_3D('',#47116,#37221,#37222) ;
#33030 = AXIS2_PLACEMENT_3D('',#47117,#37223,#37224) ;
#33031 = AXIS2_PLACEMENT_3D('',#47120,#37227,#37228) ;
#33032 = AXIS2_PLACEMENT_3D('',#47122,#37230,#37231) ;
#33033 = AXIS2_PLACEMENT_3D('',#47124,#37233,#37234) ;
#33034 = AXIS2_PLACEMENT_3D('',#47125,#37235,#37236) ;
#33035 = AXIS2_PLACEMENT_3D('',#47128,#37239,#37240) ;
#33036 = AXIS2_PLACEMENT_3D('',#47130,#37242,#37243) ;
#33037 = AXIS2_PLACEMENT_3D('',#47132,#37245,#37246) ;
#33038 = AXIS2_PLACEMENT_3D('',#47133,#37247,#37248) ;
#33039 = AXIS2_PLACEMENT_3D('',#47136,#37251,#37252) ;
#33040 = AXIS2_PLACEMENT_3D('',#47138,#37254,#37255) ;
#33041 = AXIS2_PLACEMENT_3D('',#47140,#37257,#37258) ;
#33042 = AXIS2_PLACEMENT_3D('',#47141,#37259,#37260) ;
#33043 = AXIS2_PLACEMENT_3D('',#47143,#37262,#37263) ;
#33044 = AXIS2_PLACEMENT_3D('',#47144,#37264,#37265) ;
#33045 = AXIS2_PLACEMENT_3D('',#47146,#37267,#37268) ;
#33046 = AXIS2_PLACEMENT_3D('',#47147,#37269,#37270) ;
#33047 = AXIS2_PLACEMENT_3D('',#47148,#37271,#37272) ;
#33048 = AXIS2_PLACEMENT_3D('',#47149,#37273,#37274) ;
#33049 = AXIS2_PLACEMENT_3D('',#47152,#37277,#37278) ;
#33050 = AXIS2_PLACEMENT_3D('',#47155,#37281,#37282) ;
#33051 = AXIS2_PLACEMENT_3D('',#47156,#37283,#37284) ;
#33052 = AXIS2_PLACEMENT_3D('',#47157,#37285,#37286) ;
#33053 = AXIS2_PLACEMENT_3D('',#47160,#37289,#37290) ;
#33054 = AXIS2_PLACEMENT_3D('',#47163,#37293,#37294) ;
#33055 = AXIS2_PLACEMENT_3D('',#47164,#37295,#37296) ;
#33056 = AXIS2_PLACEMENT_3D('',#47165,#37297,#37298) ;
#33057 = AXIS2_PLACEMENT_3D('',#47168,#37301,#37302) ;
#33058 = AXIS2_PLACEMENT_3D('',#47171,#37305,#37306) ;
#33059 = AXIS2_PLACEMENT_3D('',#47172,#37307,#37308) ;
#33060 = AXIS2_PLACEMENT_3D('',#47173,#37309,#37310) ;
#33061 = AXIS2_PLACEMENT_3D('',#47174,#37311,#37312) ;
#33062 = AXIS2_PLACEMENT_3D('',#47175,#37313,#37314) ;
#33063 = AXIS2_PLACEMENT_3D('',#47176,#37315,#37316) ;
#33064 = AXIS2_PLACEMENT_3D('',#47192,#37318,#37319) ;
#33065 = AXIS2_PLACEMENT_3D('',#47207,#37320,#37321) ;
#33066 = AXIS2_PLACEMENT_3D('',#47283,#37323,#37324) ;
#33067 = AXIS2_PLACEMENT_3D('',#47361,#37326,#37327) ;
#33068 = AXIS2_PLACEMENT_3D('',#47439,#37329,#37330) ;
#33069 = AXIS2_PLACEMENT_3D('',#47459,#37332,#37333) ;
#33070 = AXIS2_PLACEMENT_3D('',#47478,#37334,#37335) ;
#33071 = AXIS2_PLACEMENT_3D('',#47500,#37337,#37338) ;
#33072 = AXIS2_PLACEMENT_3D('',#47521,#37339,#37340) ;
#33073 = AXIS2_PLACEMENT_3D('',#47597,#37342,#37343) ;
#33074 = AXIS2_PLACEMENT_3D('',#47673,#37345,#37346) ;
#33075 = AXIS2_PLACEMENT_3D('',#47753,#37348,#37349) ;
#33076 = AXIS2_PLACEMENT_3D('',#47829,#37351,#37352) ;
#33077 = AXIS2_PLACEMENT_3D('',#47855,#37354,#37355) ;
#33078 = AXIS2_PLACEMENT_3D('',#47880,#37356,#37357) ;
#33079 = AXIS2_PLACEMENT_3D('',#47896,#37359,#37360) ;
#33080 = AXIS2_PLACEMENT_3D('',#47921,#37362,#37363) ;
#33081 = AXIS2_PLACEMENT_3D('',#47922,#37364,#37365) ;
#33082 = AXIS2_PLACEMENT_3D('',#47959,#37366,#37367) ;
#33083 = AXIS2_PLACEMENT_3D('',#47968,#37368,#37369) ;
#33084 = AXIS2_PLACEMENT_3D('',#48009,#37370,#37371) ;
#33085 = AXIS2_PLACEMENT_3D('',#48082,#37372,#37373) ;
#33086 = AXIS2_PLACEMENT_3D('',#48155,#37374,#37375) ;
#33087 = AXIS2_PLACEMENT_3D('',#48158,#37376,#37377) ;
#33088 = AXIS2_PLACEMENT_3D('',#48166,#37378,#37379) ;
#33089 = AXIS2_PLACEMENT_3D('',#48169,#37380,#37381) ;
#33090 = AXIS2_PLACEMENT_3D('',#48517,#37382,#37383) ;
#33091 = AXIS2_PLACEMENT_3D('',#48519,#37384,#37385) ;
#33092 = AXIS2_PLACEMENT_3D('',#48521,#37386,#37387) ;
#33093 = AXIS2_PLACEMENT_3D('',#48523,#37388,#37389) ;
#33094 = AXIS2_PLACEMENT_3D('',#48525,#37390,#37391) ;
#33095 = AXIS2_PLACEMENT_3D('',#48526,#37392,#37393) ;
#33096 = AXIS2_PLACEMENT_3D('',#48527,#37394,#37395) ;
#33097 = AXIS2_PLACEMENT_3D('',#48547,#37398,#37399) ;
#33098 = AXIS2_PLACEMENT_3D('',#48564,#37401,#37402) ;
#33099 = AXIS2_PLACEMENT_3D('',#48572,#37404,#37405) ;
#33100 = AXIS2_PLACEMENT_3D('',#48582,#37407,#37408) ;
#33101 = AXIS2_PLACEMENT_3D('',#48599,#37410,#37411) ;
#33102 = AXIS2_PLACEMENT_3D('',#48613,#37412,#37413) ;
#33103 = AXIS2_PLACEMENT_3D('',#48614,#37414,#37415) ;
#33104 = AXIS2_PLACEMENT_3D('',#48615,#37416,#37417) ;
#33105 = AXIS2_PLACEMENT_3D('',#48616,#37418,#37419) ;
#33106 = AXIS2_PLACEMENT_3D('',#48617,#37420,#37421) ;
#33107 = AXIS2_PLACEMENT_3D('',#48618,#37422,#37423) ;
#33108 = AXIS2_PLACEMENT_3D('',#48619,#37424,#37425) ;
#33109 = AXIS2_PLACEMENT_3D('',#48620,#37426,#37427) ;
#33110 = AXIS2_PLACEMENT_3D('',#48621,#37428,#37429) ;
#33111 = AXIS2_PLACEMENT_3D('',#48622,#37430,#37431) ;
#33112 = AXIS2_PLACEMENT_3D('',#48623,#37432,#37433) ;
#33113 = AXIS2_PLACEMENT_3D('',#48624,#37434,#37435) ;
#33114 = AXIS2_PLACEMENT_3D('',#48625,#37436,#37437) ;
#33115 = AXIS2_PLACEMENT_3D('',#48626,#37438,#37439) ;
#33116 = AXIS2_PLACEMENT_3D('',#48627,#37440,#37441) ;
#33117 = AXIS2_PLACEMENT_3D('',#48628,#37442,#37443) ;
#33118 = AXIS2_PLACEMENT_3D('',#48629,#37444,#37445) ;
#33119 = AXIS2_PLACEMENT_3D('',#48630,#37446,#37447) ;
#33120 = AXIS2_PLACEMENT_3D('',#48631,#37448,#37449) ;
#33121 = AXIS2_PLACEMENT_3D('',#48632,#37450,#37451) ;
#33122 = AXIS2_PLACEMENT_3D('',#48633,#37452,#37453) ;
#33123 = AXIS2_PLACEMENT_3D('',#48634,#37454,#37455) ;
#33124 = AXIS2_PLACEMENT_3D('',#48635,#37456,#37457) ;
#33125 = AXIS2_PLACEMENT_3D('',#48636,#37458,#37459) ;
#33126 = AXIS2_PLACEMENT_3D('',#48647,#37461,#37462) ;
#33127 = AXIS2_PLACEMENT_3D('',#48648,#37463,#37464) ;
#33128 = AXIS2_PLACEMENT_3D('',#48689,#37466,#37467) ;
#33129 = AXIS2_PLACEMENT_3D('',#48724,#37468,#37469) ;
#33130 = AXIS2_PLACEMENT_3D('',#48800,#37471,#37472) ;
#33131 = AXIS2_PLACEMENT_3D('',#48876,#37474,#37475) ;
#33132 = AXIS2_PLACEMENT_3D('',#48952,#37477,#37478) ;
#33133 = AXIS2_PLACEMENT_3D('',#49028,#37480,#37481) ;
#33134 = AXIS2_PLACEMENT_3D('',#49056,#37483,#37484) ;
#33135 = AXIS2_PLACEMENT_3D('',#49060,#37486,#37487) ;
#33136 = AXIS2_PLACEMENT_3D('',#49061,#37488,#37489) ;
#33137 = AXIS2_PLACEMENT_3D('',#49063,#37490,#37491) ;
#33138 = AXIS2_PLACEMENT_3D('',#49082,#37492,#37493) ;
#33139 = AXIS2_PLACEMENT_3D('',#49158,#37495,#37496) ;
#33140 = AXIS2_PLACEMENT_3D('',#49234,#37498,#37499) ;
#33141 = AXIS2_PLACEMENT_3D('',#49312,#37501,#37502) ;
#33142 = AXIS2_PLACEMENT_3D('',#49390,#37504,#37505) ;
#33143 = AXIS2_PLACEMENT_3D('',#49423,#37506,#37507) ;
#33144 = AXIS2_PLACEMENT_3D('',#49450,#37508,#37509) ;
#33145 = AXIS2_PLACEMENT_3D('',#49489,#37510,#37511) ;
#33146 = AXIS2_PLACEMENT_3D('',#49522,#37512,#37513) ;
#33147 = AXIS2_PLACEMENT_3D('',#49524,#37514,#37515) ;
#33148 = AXIS2_PLACEMENT_3D('',#49526,#37516,#37517) ;
#33149 = AXIS2_PLACEMENT_3D('',#49528,#37518,#37519) ;
#33150 = AXIS2_PLACEMENT_3D('',#49529,#37520,#37521) ;
#33151 = AXIS2_PLACEMENT_3D('',#49530,#37522,#37523) ;
#33152 = AXIS2_PLACEMENT_3D('',#49532,#37525,#37526) ;
#33153 = AXIS2_PLACEMENT_3D('',#49535,#37527,#37528) ;
#33154 = AXIS2_PLACEMENT_3D('',#49545,#37533,#37534) ;
#33155 = AXIS2_PLACEMENT_3D('',#49555,#37539,#37540) ;
#33156 = AXIS2_PLACEMENT_3D('',#49565,#37545,#37546) ;
#33157 = AXIS2_PLACEMENT_3D('',#49573,#37551,#37552) ;
#33158 = AXIS2_PLACEMENT_3D('',#49605,#37554,#37555) ;
#33159 = AXIS2_PLACEMENT_3D('',#49636,#37556,#37557) ;
#33160 = AXIS2_PLACEMENT_3D('',#49641,#37559,#37560) ;
#33161 = AXIS2_PLACEMENT_3D('',#49659,#37561,#37562) ;
#33162 = AXIS2_PLACEMENT_3D('',#49677,#37563,#37564) ;
#33163 = AXIS2_PLACEMENT_3D('',#49695,#37565,#37566) ;
#33164 = AXIS2_PLACEMENT_3D('',#49712,#37567,#37568) ;
#33165 = AXIS2_PLACEMENT_3D('',#49713,#37569,#37570) ;
#33166 = AXIS2_PLACEMENT_3D('',#49714,#37571,#37572) ;
#33167 = AXIS2_PLACEMENT_3D('',#49715,#37573,#37574) ;
#33168 = AXIS2_PLACEMENT_3D('',#49716,#37575,#37576) ;
#33169 = AXIS2_PLACEMENT_3D('',#49717,#37577,#37578) ;
#33170 = AXIS2_PLACEMENT_3D('',#49718,#37579,#37580) ;
#33171 = AXIS2_PLACEMENT_3D('',#49719,#37581,#37582) ;
#33172 = AXIS2_PLACEMENT_3D('',#49720,#37583,#37584) ;
#33173 = AXIS2_PLACEMENT_3D('',#49721,#37585,#37586) ;
#33174 = AXIS2_PLACEMENT_3D('',#49722,#37587,#37588) ;
#33175 = AXIS2_PLACEMENT_3D('',#49725,#37591,#37592) ;
#33176 = AXIS2_PLACEMENT_3D('',#49727,#37594,#37595) ;
#33177 = AXIS2_PLACEMENT_3D('',#49728,#37596,#37597) ;
#33178 = AXIS2_PLACEMENT_3D('',#49730,#37599,#37600) ;
#33179 = AXIS2_PLACEMENT_3D('',#49732,#37602,#37603) ;
#33180 = AXIS2_PLACEMENT_3D('',#49734,#37605,#37606) ;
#33181 = AXIS2_PLACEMENT_3D('',#49735,#37607,#37608) ;
#33182 = AXIS2_PLACEMENT_3D('',#49737,#37610,#37611) ;
#33183 = AXIS2_PLACEMENT_3D('',#49739,#37613,#37614) ;
#33184 = AXIS2_PLACEMENT_3D('',#49741,#37616,#37617) ;
#33185 = AXIS2_PLACEMENT_3D('',#49742,#37618,#37619) ;
#33186 = AXIS2_PLACEMENT_3D('',#49743,#37620,#37621) ;
#33187 = AXIS2_PLACEMENT_3D('',#49744,#37622,#37623) ;
#33188 = AXIS2_PLACEMENT_3D('',#49745,#37624,#37625) ;
#33189 = AXIS2_PLACEMENT_3D('',#49747,#37627,#37628) ;
#33190 = AXIS2_PLACEMENT_3D('',#49749,#37630,#37631) ;
#33191 = AXIS2_PLACEMENT_3D('',#49751,#37633,#37634) ;
#33192 = AXIS2_PLACEMENT_3D('',#49752,#37635,#37636) ;
#33193 = AXIS2_PLACEMENT_3D('',#49753,#37637,#37638) ;
#33194 = AXIS2_PLACEMENT_3D('',#49790,#37639,#37640) ;
#33195 = AXIS2_PLACEMENT_3D('',#50219,#37641,#37642) ;
#33196 = AXIS2_PLACEMENT_3D('',#50220,#37643,#37644) ;
#33197 = AXIS2_PLACEMENT_3D('',#50221,#37645,#37646) ;
#33198 = AXIS2_PLACEMENT_3D('',#50222,#37647,#37648) ;
#33199 = AXIS2_PLACEMENT_3D('',#50223,#37649,#37650) ;
#33200 = AXIS2_PLACEMENT_3D('',#50224,#37651,#37652) ;
#33201 = AXIS2_PLACEMENT_3D('',#50225,#37653,#37654) ;
#33202 = AXIS2_PLACEMENT_3D('',#50259,#37656,#37657) ;
#33203 = AXIS2_PLACEMENT_3D('',#50296,#37658,#37659) ;
#33204 = AXIS2_PLACEMENT_3D('',#50535,#37661,#37662) ;
#33205 = AXIS2_PLACEMENT_3D('',#50673,#37664,#37665) ;
#33206 = AXIS2_PLACEMENT_3D('',#50748,#37666,#37667) ;
#33207 = AXIS2_PLACEMENT_3D('',#50760,#37669,#37670) ;
#33208 = AXIS2_PLACEMENT_3D('',#50779,#37671,#37672) ;
#33209 = AXIS2_PLACEMENT_3D('',#51021,#37674,#37675) ;
#33210 = AXIS2_PLACEMENT_3D('',#51184,#37677,#37678) ;
#33211 = AXIS2_PLACEMENT_3D('',#51286,#37679,#37680) ;
#33212 = AXIS2_PLACEMENT_3D('',#51320,#37682,#37683) ;
#33213 = AXIS2_PLACEMENT_3D('',#51357,#37684,#37685) ;
#33214 = AXIS2_PLACEMENT_3D('',#51598,#37687,#37688) ;
#33215 = AXIS2_PLACEMENT_3D('',#51736,#37690,#37691) ;
#33216 = AXIS2_PLACEMENT_3D('',#51822,#37692,#37693) ;
#33217 = AXIS2_PLACEMENT_3D('',#51854,#37695,#37696) ;
#33218 = AXIS2_PLACEMENT_3D('',#51891,#37697,#37698) ;
#33219 = AXIS2_PLACEMENT_3D('',#52130,#37700,#37701) ;
#33220 = AXIS2_PLACEMENT_3D('',#52268,#37703,#37704) ;
#33221 = AXIS2_PLACEMENT_3D('',#52345,#37705,#37706) ;
#33222 = AXIS2_PLACEMENT_3D('',#52350,#37708,#37709) ;
#33223 = AXIS2_PLACEMENT_3D('',#52394,#37710,#37711) ;
#33224 = AXIS2_PLACEMENT_3D('',#52598,#37713,#37714) ;
#33225 = AXIS2_PLACEMENT_3D('',#52703,#37715,#37716) ;
#33226 = AXIS2_PLACEMENT_3D('',#52850,#37718,#37719) ;
#33227 = AXIS2_PLACEMENT_3D('',#53059,#37720,#37721) ;
#33228 = AXIS2_PLACEMENT_3D('',#53064,#37723,#37724) ;
#33229 = AXIS2_PLACEMENT_3D('',#53108,#37725,#37726) ;
#33230 = AXIS2_PLACEMENT_3D('',#53312,#37728,#37729) ;
#33231 = AXIS2_PLACEMENT_3D('',#53417,#37730,#37731) ;
#33232 = AXIS2_PLACEMENT_3D('',#53564,#37733,#37734) ;
#33233 = AXIS2_PLACEMENT_3D('',#53773,#37735,#37736) ;
#33234 = AXIS2_PLACEMENT_3D('',#53778,#37738,#37739) ;
#33235 = AXIS2_PLACEMENT_3D('',#53822,#37740,#37741) ;
#33236 = AXIS2_PLACEMENT_3D('',#54026,#37743,#37744) ;
#33237 = AXIS2_PLACEMENT_3D('',#54131,#37745,#37746) ;
#33238 = AXIS2_PLACEMENT_3D('',#54278,#37748,#37749) ;
#33239 = AXIS2_PLACEMENT_3D('',#54487,#37750,#37751) ;
#33240 = AXIS2_PLACEMENT_3D('',#54492,#37753,#37754) ;
#33241 = AXIS2_PLACEMENT_3D('',#54536,#37755,#37756) ;
#33242 = AXIS2_PLACEMENT_3D('',#54740,#37758,#37759) ;
#33243 = AXIS2_PLACEMENT_3D('',#54845,#37760,#37761) ;
#33244 = AXIS2_PLACEMENT_3D('',#54992,#37763,#37764) ;
#33245 = AXIS2_PLACEMENT_3D('',#55201,#37765,#37766) ;
#33246 = AXIS2_PLACEMENT_3D('',#55235,#37768,#37769) ;
#33247 = AXIS2_PLACEMENT_3D('',#55272,#37770,#37771) ;
#33248 = AXIS2_PLACEMENT_3D('',#55507,#37773,#37774) ;
#33249 = AXIS2_PLACEMENT_3D('',#55645,#37776,#37777) ;
#33250 = AXIS2_PLACEMENT_3D('',#55720,#37778,#37779) ;
#33251 = AXIS2_PLACEMENT_3D('',#55754,#37781,#37782) ;
#33252 = AXIS2_PLACEMENT_3D('',#55791,#37783,#37784) ;
#33253 = AXIS2_PLACEMENT_3D('',#56032,#37786,#37787) ;
#33254 = AXIS2_PLACEMENT_3D('',#56170,#37789,#37790) ;
#33255 = AXIS2_PLACEMENT_3D('',#56256,#37791,#37792) ;
#33256 = AXIS2_PLACEMENT_3D('',#56261,#37794,#37795) ;
#33257 = AXIS2_PLACEMENT_3D('',#56305,#37796,#37797) ;
#33258 = AXIS2_PLACEMENT_3D('',#56509,#37799,#37800) ;
#33259 = AXIS2_PLACEMENT_3D('',#56614,#37801,#37802) ;
#33260 = AXIS2_PLACEMENT_3D('',#56761,#37804,#37805) ;
#33261 = AXIS2_PLACEMENT_3D('',#56970,#37806,#37807) ;
#33262 = AXIS2_PLACEMENT_3D('',#56975,#37809,#37810) ;
#33263 = AXIS2_PLACEMENT_3D('',#57019,#37811,#37812) ;
#33264 = AXIS2_PLACEMENT_3D('',#57223,#37814,#37815) ;
#33265 = AXIS2_PLACEMENT_3D('',#57326,#37816,#37817) ;
#33266 = AXIS2_PLACEMENT_3D('',#57473,#37819,#37820) ;
#33267 = AXIS2_PLACEMENT_3D('',#57682,#37821,#37822) ;
#33268 = AXIS2_PLACEMENT_3D('',#57714,#37824,#37825) ;
#33269 = AXIS2_PLACEMENT_3D('',#57751,#37826,#37827) ;
#33270 = AXIS2_PLACEMENT_3D('',#57994,#37829,#37830) ;
#33271 = AXIS2_PLACEMENT_3D('',#58132,#37832,#37833) ;
#33272 = AXIS2_PLACEMENT_3D('',#58211,#37834,#37835) ;
#33273 = AXIS2_PLACEMENT_3D('',#58243,#37837,#37838) ;
#33274 = AXIS2_PLACEMENT_3D('',#58280,#37839,#37840) ;
#33275 = AXIS2_PLACEMENT_3D('',#58521,#37842,#37843) ;
#33276 = AXIS2_PLACEMENT_3D('',#58659,#37845,#37846) ;
#33277 = AXIS2_PLACEMENT_3D('',#58734,#37847,#37848) ;
#33278 = AXIS2_PLACEMENT_3D('',#58739,#37850,#37851) ;
#33279 = AXIS2_PLACEMENT_3D('',#58783,#37852,#37853) ;
#33280 = AXIS2_PLACEMENT_3D('',#58987,#37855,#37856) ;
#33281 = AXIS2_PLACEMENT_3D('',#59092,#37857,#37858) ;
#33282 = AXIS2_PLACEMENT_3D('',#59239,#37860,#37861) ;
#33283 = AXIS2_PLACEMENT_3D('',#59448,#37862,#37863) ;
#33284 = AXIS2_PLACEMENT_3D('',#59453,#37865,#37866) ;
#33285 = AXIS2_PLACEMENT_3D('',#59497,#37867,#37868) ;
#33286 = AXIS2_PLACEMENT_3D('',#59701,#37870,#37871) ;
#33287 = AXIS2_PLACEMENT_3D('',#59806,#37872,#37873) ;
#33288 = AXIS2_PLACEMENT_3D('',#59953,#37875,#37876) ;
#33289 = AXIS2_PLACEMENT_3D('',#60162,#37877,#37878) ;
#33290 = AXIS2_PLACEMENT_3D('',#60371,#37879,#37880) ;
#33291 = AXIS2_PLACEMENT_3D('',#60584,#37881,#37882) ;
#33292 = AXIS2_PLACEMENT_3D('',#60805,#37883,#37884) ;
#33293 = AXIS2_PLACEMENT_3D('',#61032,#37885,#37886) ;
#33294 = AXIS2_PLACEMENT_3D('',#61243,#37887,#37888) ;
#33295 = AXIS2_PLACEMENT_3D('',#61454,#37889,#37890) ;
#33296 = AXIS2_PLACEMENT_3D('',#61684,#37891,#37892) ;
#33297 = AXIS2_PLACEMENT_3D('',#61911,#37893,#37894) ;
#33298 = AXIS2_PLACEMENT_3D('',#62122,#37895,#37896) ;
#33299 = AXIS2_PLACEMENT_3D('',#62331,#37897,#37898) ;
#33300 = AXIS2_PLACEMENT_3D('',#62544,#37899,#37900) ;
#33301 = AXIS2_PLACEMENT_3D('',#62755,#37901,#37902) ;
#33302 = AXIS2_PLACEMENT_3D('',#62980,#37903,#37904) ;
#33303 = AXIS2_PLACEMENT_3D('',#63206,#37905,#37906) ;
#33304 = AXIS2_PLACEMENT_3D('',#63431,#37907,#37908) ;
#33305 = AXIS2_PLACEMENT_3D('',#63656,#37909,#37910) ;
#33306 = AXIS2_PLACEMENT_3D('',#63659,#37911,#37912) ;
#33307 = AXIS2_PLACEMENT_3D('',#63663,#37914,#37915) ;
#33308 = AXIS2_PLACEMENT_3D('',#63665,#37917,#37918) ;
#33309 = AXIS2_PLACEMENT_3D('',#63668,#37919,#37920) ;
#33310 = AXIS2_PLACEMENT_3D('',#63672,#37922,#37923) ;
#33311 = AXIS2_PLACEMENT_3D('',#63674,#37925,#37926) ;
#33312 = AXIS2_PLACEMENT_3D('',#63677,#37927,#37928) ;
#33313 = AXIS2_PLACEMENT_3D('',#63681,#37930,#37931) ;
#33314 = AXIS2_PLACEMENT_3D('',#63683,#37933,#37934) ;
#33315 = AXIS2_PLACEMENT_3D('',#63686,#37935,#37936) ;
#33316 = AXIS2_PLACEMENT_3D('',#63690,#37938,#37939) ;
#33317 = AXIS2_PLACEMENT_3D('',#63692,#37941,#37942) ;
#33318 = AXIS2_PLACEMENT_3D('',#63695,#37943,#37944) ;
#33319 = AXIS2_PLACEMENT_3D('',#63699,#37946,#37947) ;
#33320 = AXIS2_PLACEMENT_3D('',#63701,#37949,#37950) ;
#33321 = AXIS2_PLACEMENT_3D('',#63705,#37952,#37953) ;
#33322 = AXIS2_PLACEMENT_3D('',#63710,#37956,#37957) ;
#33323 = AXIS2_PLACEMENT_3D('',#63714,#37959,#37960) ;
#33324 = AXIS2_PLACEMENT_3D('',#63717,#37963,#37964) ;
#33325 = AXIS2_PLACEMENT_3D('',#63720,#37965,#37966) ;
#33326 = AXIS2_PLACEMENT_3D('',#63724,#37968,#37969) ;
#33327 = AXIS2_PLACEMENT_3D('',#63726,#37971,#37972) ;
#33328 = AXIS2_PLACEMENT_3D('',#63729,#37973,#37974) ;
#33329 = AXIS2_PLACEMENT_3D('',#63733,#37976,#37977) ;
#33330 = AXIS2_PLACEMENT_3D('',#63735,#37979,#37980) ;
#33331 = AXIS2_PLACEMENT_3D('',#63742,#37984,#37985) ;
#33332 = AXIS2_PLACEMENT_3D('',#63750,#37989,#37990) ;
#33333 = AXIS2_PLACEMENT_3D('',#63774,#38002,#38003) ;
#33334 = AXIS2_PLACEMENT_3D('',#63778,#38005,#38006) ;
#33335 = AXIS2_PLACEMENT_3D('',#64139,#38012,#38013) ;
#33336 = AXIS2_PLACEMENT_3D('',#64165,#38026,#38027) ;
#33337 = AXIS2_PLACEMENT_3D('',#64166,#38028,#38029) ;
#33338 = AXIS2_PLACEMENT_3D('',#64169,#38030,#38031) ;
#33339 = AXIS2_PLACEMENT_3D('',#64173,#38033,#38034) ;
#33340 = AXIS2_PLACEMENT_3D('',#64175,#38036,#38037) ;
#33341 = AXIS2_PLACEMENT_3D('',#64185,#38043,#38044) ;
#33342 = AXIS2_PLACEMENT_3D('',#64193,#38048,#38049) ;
#33343 = AXIS2_PLACEMENT_3D('',#64201,#38053,#38054) ;
#33344 = AXIS2_PLACEMENT_3D('',#64209,#38058,#38059) ;
#33345 = AXIS2_PLACEMENT_3D('',#64212,#38061,#38062) ;
#33346 = AXIS2_PLACEMENT_3D('',#64246,#38079,#38080) ;
#33347 = AXIS2_PLACEMENT_3D('',#64601,#38082,#38083) ;
#33348 = AXIS2_PLACEMENT_3D('',#64605,#38085,#38086) ;
#33349 = AXIS2_PLACEMENT_3D('',#64609,#38088,#38089) ;
#33350 = AXIS2_PLACEMENT_3D('',#64612,#38091,#38092) ;
#33351 = AXIS2_PLACEMENT_3D('',#64627,#38099,#38100) ;
#33352 = AXIS2_PLACEMENT_3D('',#64631,#38102,#38103) ;
#33353 = AXIS2_PLACEMENT_3D('',#64633,#38105,#38106) ;
#33354 = AXIS2_PLACEMENT_3D('',#64645,#38112,#38113) ;
#33355 = AXIS2_PLACEMENT_3D('',#64653,#38117,#38118) ;
#33356 = AXIS2_PLACEMENT_3D('',#64659,#38122,#38123) ;
#33357 = AXIS2_PLACEMENT_3D('',#64686,#38136,#38137) ;
#33358 = AXIS2_PLACEMENT_3D('',#64690,#38139,#38140) ;
#33359 = AXIS2_PLACEMENT_3D('',#64697,#38144,#38145) ;
#33360 = AXIS2_PLACEMENT_3D('',#65048,#38146,#38147) ;
#33361 = AXIS2_PLACEMENT_3D('',#65054,#38150,#38151) ;
#33362 = AXIS2_PLACEMENT_3D('',#65062,#38155,#38156) ;
#33363 = AXIS2_PLACEMENT_3D('',#65070,#38160,#38161) ;
#33364 = AXIS2_PLACEMENT_3D('',#65078,#38165,#38166) ;
#33365 = AXIS2_PLACEMENT_3D('',#65091,#38173,#38174) ;
#33366 = AXIS2_PLACEMENT_3D('',#65095,#38176,#38177) ;
#33367 = AXIS2_PLACEMENT_3D('',#65099,#38179,#38180) ;
#33368 = AXIS2_PLACEMENT_3D('',#65103,#38182,#38183) ;
#33369 = AXIS2_PLACEMENT_3D('',#65457,#38185,#38186) ;
#33370 = AXIS2_PLACEMENT_3D('',#65461,#38188,#38189) ;
#33371 = AXIS2_PLACEMENT_3D('',#65500,#38209,#38210) ;
#33372 = AXIS2_PLACEMENT_3D('',#65502,#38211,#38212) ;
#33373 = AXIS2_PLACEMENT_3D('',#65503,#38213,#38214) ;
#33374 = AXIS2_PLACEMENT_3D('',#65505,#38215,#38216) ;
#33375 = AXIS2_PLACEMENT_3D('',#65511,#38221,#38222) ;
#33376 = AXIS2_PLACEMENT_3D('',#65534,#38229,#38230) ;
#33377 = AXIS2_PLACEMENT_3D('',#65536,#38231,#38232) ;
#33378 = AXIS2_PLACEMENT_3D('',#65538,#38234,#38235) ;
#33379 = AXIS2_PLACEMENT_3D('',#65541,#38237,#38238) ;
#33380 = AXIS2_PLACEMENT_3D('',#65542,#38239,#38240) ;
#33381 = AXIS2_PLACEMENT_3D('',#65544,#38241,#38242) ;
#33382 = AXIS2_PLACEMENT_3D('',#65546,#38244,#38245) ;
#33383 = AXIS2_PLACEMENT_3D('',#65548,#38246,#38247) ;
#33384 = AXIS2_PLACEMENT_3D('',#65551,#38249,#38250) ;
#33385 = AXIS2_PLACEMENT_3D('',#65552,#38251,#38252) ;
#33386 = AXIS2_PLACEMENT_3D('',#65554,#38254,#38255) ;
#33387 = AXIS2_PLACEMENT_3D('',#65560,#38259,#38260) ;
#33388 = AXIS2_PLACEMENT_3D('',#65620,#38264,#38265) ;
#33389 = AXIS2_PLACEMENT_3D('',#65624,#38268,#38269) ;
#33390 = AXIS2_PLACEMENT_3D('',#65629,#38273,#38274) ;
#33391 = AXIS2_PLACEMENT_3D('',#65633,#38277,#38278) ;
#33392 = AXIS2_PLACEMENT_3D('',#65635,#38280,#38281) ;
#33393 = AXIS2_PLACEMENT_3D('',#65636,#38282,#38283) ;
#33394 = AXIS2_PLACEMENT_3D('',#65638,#38285,#38286) ;
#33395 = AXIS2_PLACEMENT_3D('',#65643,#38290,#38291) ;
#33396 = AXIS2_PLACEMENT_3D('',#65645,#38293,#38294) ;
#33397 = AXIS2_PLACEMENT_3D('',#65647,#38295,#38296) ;
#33398 = AXIS2_PLACEMENT_3D('',#65650,#38298,#38299) ;
#33399 = AXIS2_PLACEMENT_3D('',#65651,#38300,#38301) ;
#33400 = AXIS2_PLACEMENT_3D('',#65657,#38305,#38306) ;
#33401 = AXIS2_PLACEMENT_3D('',#65659,#38307,#38308) ;
#33402 = AXIS2_PLACEMENT_3D('',#65661,#38309,#38310) ;
#33403 = AXIS2_PLACEMENT_3D('',#65663,#38312,#38313) ;
#33404 = AXIS2_PLACEMENT_3D('',#65665,#38314,#38315) ;
#33405 = AXIS2_PLACEMENT_3D('',#65666,#38316,#38317) ;
#33406 = AXIS2_PLACEMENT_3D('',#65667,#38318,#38319) ;
#33407 = AXIS2_PLACEMENT_3D('',#65669,#38320,#38321) ;
#33408 = AXIS2_PLACEMENT_3D('',#65671,#38323,#38324) ;
#33409 = AXIS2_PLACEMENT_3D('',#65673,#38325,#38326) ;
#33410 = AXIS2_PLACEMENT_3D('',#65674,#38327,#38328) ;
#33411 = AXIS2_PLACEMENT_3D('',#65675,#38329,#38330) ;
#33412 = AXIS2_PLACEMENT_3D('',#65677,#38331,#38332) ;
#33413 = AXIS2_PLACEMENT_3D('',#65679,#38334,#38335) ;
#33414 = AXIS2_PLACEMENT_3D('',#65685,#38339,#38340) ;
#33415 = AXIS2_PLACEMENT_3D('',#65688,#38342,#38343) ;
#33416 = AXIS2_PLACEMENT_3D('',#65689,#38344,#38345) ;
#33417 = AXIS2_PLACEMENT_3D('',#65693,#38348,#38349) ;
#33418 = AXIS2_PLACEMENT_3D('',#65696,#38351,#38352) ;
#33419 = AXIS2_PLACEMENT_3D('',#65697,#38353,#38354) ;
#33420 = AXIS2_PLACEMENT_3D('',#65701,#38357,#38358) ;
#33421 = AXIS2_PLACEMENT_3D('',#65703,#38359,#38360) ;
#33422 = AXIS2_PLACEMENT_3D('',#65705,#38361,#38362) ;
#33423 = AXIS2_PLACEMENT_3D('',#65707,#38364,#38365) ;
#33424 = AXIS2_PLACEMENT_3D('',#65709,#38366,#38367) ;
#33425 = AXIS2_PLACEMENT_3D('',#65710,#38368,#38369) ;
#33426 = AXIS2_PLACEMENT_3D('',#65711,#38370,#38371) ;
#33427 = AXIS2_PLACEMENT_3D('',#65713,#38372,#38373) ;
#33428 = AXIS2_PLACEMENT_3D('',#65715,#38375,#38376) ;
#33429 = AXIS2_PLACEMENT_3D('',#65717,#38377,#38378) ;
#33430 = AXIS2_PLACEMENT_3D('',#65718,#38379,#38380) ;
#33431 = AXIS2_PLACEMENT_3D('',#65719,#38381,#38382) ;
#33432 = AXIS2_PLACEMENT_3D('',#65721,#38383,#38384) ;
#33433 = AXIS2_PLACEMENT_3D('',#65723,#38386,#38387) ;
#33434 = AXIS2_PLACEMENT_3D('',#65729,#38391,#38392) ;
#33435 = AXIS2_PLACEMENT_3D('',#65732,#38394,#38395) ;
#33436 = AXIS2_PLACEMENT_3D('',#65733,#38396,#38397) ;
#33437 = AXIS2_PLACEMENT_3D('',#65737,#38400,#38401) ;
#33438 = AXIS2_PLACEMENT_3D('',#65740,#38403,#38404) ;
#33439 = AXIS2_PLACEMENT_3D('',#65741,#38405,#38406) ;
#33440 = AXIS2_PLACEMENT_3D('',#65745,#38409,#38410) ;
#33441 = AXIS2_PLACEMENT_3D('',#65754,#38415,#38416) ;
#33442 = AXIS2_PLACEMENT_3D('',#65760,#38420,#38421) ;
#33443 = AXIS2_PLACEMENT_3D('',#65766,#38425,#38426) ;
#33444 = AXIS2_PLACEMENT_3D('',#65772,#38430,#38431) ;
#33445 = AXIS2_PLACEMENT_3D('',#65778,#38435,#38436) ;
#33446 = AXIS2_PLACEMENT_3D('',#65781,#38439,#38440) ;
#33447 = AXIS2_PLACEMENT_3D('',#65790,#38445,#38446) ;
#33448 = AXIS2_PLACEMENT_3D('',#65796,#38450,#38451) ;
#33449 = AXIS2_PLACEMENT_3D('',#65802,#38455,#38456) ;
#33450 = AXIS2_PLACEMENT_3D('',#65808,#38460,#38461) ;
#33451 = AXIS2_PLACEMENT_3D('',#65814,#38465,#38466) ;
#33452 = AXIS2_PLACEMENT_3D('',#65817,#38469,#38470) ;
#33453 = AXIS2_PLACEMENT_3D('',#65818,#38471,#38472) ;
#33454 = AXIS2_PLACEMENT_3D('',#65819,#38473,#38474) ;
#33455 = AXIS2_PLACEMENT_3D('',#65821,#38475,#38476) ;
#33456 = AXIS2_PLACEMENT_3D('',#65823,#38477,#38478) ;
#33457 = AXIS2_PLACEMENT_3D('',#65825,#38480,#38481) ;
#33458 = AXIS2_PLACEMENT_3D('',#65827,#38482,#38483) ;
#33459 = AXIS2_PLACEMENT_3D('',#65829,#38484,#38485) ;
#33460 = AXIS2_PLACEMENT_3D('',#65831,#38487,#38488) ;
#33461 = AXIS2_PLACEMENT_3D('',#65834,#38490,#38491) ;
#33462 = AXIS2_PLACEMENT_3D('',#65835,#38492,#38493) ;
#33463 = AXIS2_PLACEMENT_3D('',#65837,#38494,#38495) ;
#33464 = AXIS2_PLACEMENT_3D('',#65839,#38496,#38497) ;
#33465 = AXIS2_PLACEMENT_3D('',#65841,#38499,#38500) ;
#33466 = AXIS2_PLACEMENT_3D('',#65843,#38501,#38502) ;
#33467 = AXIS2_PLACEMENT_3D('',#65846,#38504,#38505) ;
#33468 = AXIS2_PLACEMENT_3D('',#65847,#38506,#38507) ;
#33469 = AXIS2_PLACEMENT_3D('',#65854,#38512,#38513) ;
#33470 = AXIS2_PLACEMENT_3D('',#65856,#38514,#38515) ;
#33471 = AXIS2_PLACEMENT_3D('',#65858,#38517,#38518) ;
#33472 = AXIS2_PLACEMENT_3D('',#65860,#38520,#38521) ;
#33473 = AXIS2_PLACEMENT_3D('',#65862,#38522,#38523) ;
#33474 = AXIS2_PLACEMENT_3D('',#65864,#38525,#38526) ;
#33475 = AXIS2_PLACEMENT_3D('',#65866,#38528,#38529) ;
#33476 = AXIS2_PLACEMENT_3D('',#65868,#38530,#38531) ;
#33477 = AXIS2_PLACEMENT_3D('',#65870,#38533,#38534) ;
#33478 = AXIS2_PLACEMENT_3D('',#65872,#38536,#38537) ;
#33479 = AXIS2_PLACEMENT_3D('',#65875,#38539,#38540) ;
#33480 = AXIS2_PLACEMENT_3D('',#65876,#38541,#38542) ;
#33481 = AXIS2_PLACEMENT_3D('',#65879,#38544,#38545) ;
#33482 = AXIS2_PLACEMENT_3D('',#65880,#38546,#38547) ;
#33483 = AXIS2_PLACEMENT_3D('',#65882,#38548,#38549) ;
#33484 = AXIS2_PLACEMENT_3D('',#65886,#38551,#38552) ;
#33485 = AXIS2_PLACEMENT_3D('',#65887,#38553,#38554) ;
#33486 = AXIS2_PLACEMENT_3D('',#65888,#38555,#38556) ;
#33487 = AXIS2_PLACEMENT_3D('',#65891,#38558,#38559) ;
#33488 = AXIS2_PLACEMENT_3D('',#65892,#38560,#38561) ;
#33489 = AXIS2_PLACEMENT_3D('',#65895,#38562,#38563) ;
#33490 = AXIS2_PLACEMENT_3D('',#65899,#38565,#38566) ;
#33491 = AXIS2_PLACEMENT_3D('',#65901,#38568,#38569) ;
#33492 = AXIS2_PLACEMENT_3D('',#65904,#38570,#38571) ;
#33493 = AXIS2_PLACEMENT_3D('',#65908,#38573,#38574) ;
#33494 = AXIS2_PLACEMENT_3D('',#65910,#38576,#38577) ;
#33495 = AXIS2_PLACEMENT_3D('',#65913,#38578,#38579) ;
#33496 = AXIS2_PLACEMENT_3D('',#65917,#38581,#38582) ;
#33497 = AXIS2_PLACEMENT_3D('',#65919,#38584,#38585) ;
#33498 = AXIS2_PLACEMENT_3D('',#65922,#38586,#38587) ;
#33499 = AXIS2_PLACEMENT_3D('',#65926,#38589,#38590) ;
#33500 = AXIS2_PLACEMENT_3D('',#65928,#38592,#38593) ;
#33501 = AXIS2_PLACEMENT_3D('',#65930,#38594,#38595) ;
#33502 = AXIS2_PLACEMENT_3D('',#65932,#38596,#38597) ;
#33503 = AXIS2_PLACEMENT_3D('',#65934,#38599,#38600) ;
#33504 = AXIS2_PLACEMENT_3D('',#65937,#38601,#38602) ;
#33505 = AXIS2_PLACEMENT_3D('',#65941,#38604,#38605) ;
#33506 = AXIS2_PLACEMENT_3D('',#65943,#38607,#38608) ;
#33507 = AXIS2_PLACEMENT_3D('',#65945,#38609,#38610) ;
#33508 = AXIS2_PLACEMENT_3D('',#65947,#38611,#38612) ;
#33509 = AXIS2_PLACEMENT_3D('',#65948,#38613,#38614) ;
#33510 = AXIS2_PLACEMENT_3D('',#65949,#38615,#38616) ;
#33511 = AXIS2_PLACEMENT_3D('',#65950,#38617,#38618) ;
#33512 = AXIS2_PLACEMENT_3D('',#65952,#38620,#38621) ;
#33513 = AXIS2_PLACEMENT_3D('',#65955,#38624,#38625) ;
#33514 = AXIS2_PLACEMENT_3D('',#65958,#38628,#38629) ;
#33515 = AXIS2_PLACEMENT_3D('',#65961,#38632,#38633) ;
#33516 = AXIS2_PLACEMENT_3D('',#65962,#38634,#38635) ;
#33517 = AXIS2_PLACEMENT_3D('',#65964,#38637,#38638) ;
#33518 = AXIS2_PLACEMENT_3D('',#65967,#38641,#38642) ;
#33519 = AXIS2_PLACEMENT_3D('',#65969,#38644,#38645) ;
#33520 = AXIS2_PLACEMENT_3D('',#65971,#38647,#38648) ;
#33521 = AXIS2_PLACEMENT_3D('',#65972,#38649,#38650) ;
#33522 = AXIS2_PLACEMENT_3D('',#65975,#38653,#38654) ;
#33523 = AXIS2_PLACEMENT_3D('',#65977,#38656,#38657) ;
#33524 = AXIS2_PLACEMENT_3D('',#65979,#38659,#38660) ;
#33525 = AXIS2_PLACEMENT_3D('',#65980,#38661,#38662) ;
#33526 = AXIS2_PLACEMENT_3D('',#65983,#38665,#38666) ;
#33527 = AXIS2_PLACEMENT_3D('',#65985,#38668,#38669) ;
#33528 = AXIS2_PLACEMENT_3D('',#65987,#38671,#38672) ;
#33529 = AXIS2_PLACEMENT_3D('',#65988,#38673,#38674) ;
#33530 = AXIS2_PLACEMENT_3D('',#65989,#38675,#38676) ;
#33531 = AXIS2_PLACEMENT_3D('',#65990,#38677,#38678) ;
#33532 = AXIS2_PLACEMENT_3D('',#65993,#38681,#38682) ;
#33533 = AXIS2_PLACEMENT_3D('',#65995,#38684,#38685) ;
#33534 = AXIS2_PLACEMENT_3D('',#65997,#38687,#38688) ;
#33535 = AXIS2_PLACEMENT_3D('',#65998,#38689,#38690) ;
#33536 = AXIS2_PLACEMENT_3D('',#66002,#38693,#38694) ;
#33537 = AXIS2_PLACEMENT_3D('',#66003,#38695,#38696) ;
#33538 = AXIS2_PLACEMENT_3D('',#66007,#38699,#38700) ;
#33539 = AXIS2_PLACEMENT_3D('',#66008,#38701,#38702) ;
#33540 = AXIS2_PLACEMENT_3D('',#66010,#38703,#38704) ;
#33541 = AXIS2_PLACEMENT_3D('',#66012,#38706,#38707) ;
#33542 = AXIS2_PLACEMENT_3D('',#66015,#38709,#38710) ;
#33543 = AXIS2_PLACEMENT_3D('',#66016,#38711,#38712) ;
#33544 = AXIS2_PLACEMENT_3D('',#66020,#38715,#38716) ;
#33545 = AXIS2_PLACEMENT_3D('',#66021,#38717,#38718) ;
#33546 = AXIS2_PLACEMENT_3D('',#66024,#38720,#38721) ;
#33547 = AXIS2_PLACEMENT_3D('',#66025,#38722,#38723) ;
#33548 = AXIS2_PLACEMENT_3D('',#66027,#38724,#38725) ;
#33549 = AXIS2_PLACEMENT_3D('',#66029,#38727,#38728) ;
#33550 = AXIS2_PLACEMENT_3D('',#66031,#38729,#38730) ;
#33551 = AXIS2_PLACEMENT_3D('',#66032,#38731,#38732) ;
#33552 = AXIS2_PLACEMENT_3D('',#66033,#38733,#38734) ;
#33553 = AXIS2_PLACEMENT_3D('',#66035,#38736,#38737) ;
#33554 = AXIS2_PLACEMENT_3D('',#66038,#38740,#38741) ;
#33555 = AXIS2_PLACEMENT_3D('',#66041,#38744,#38745) ;
#33556 = AXIS2_PLACEMENT_3D('',#66044,#38748,#38749) ;
#33557 = AXIS2_PLACEMENT_3D('',#66047,#38752,#38753) ;
#33558 = AXIS2_PLACEMENT_3D('',#66062,#38761,#38762) ;
#33559 = AXIS2_PLACEMENT_3D('',#66066,#38764,#38765) ;
#33560 = AXIS2_PLACEMENT_3D('',#66071,#38768,#38769) ;
#33561 = AXIS2_PLACEMENT_3D('',#66073,#38770,#38771) ;
#33562 = AXIS2_PLACEMENT_3D('',#66075,#38772,#38773) ;
#33563 = AXIS2_PLACEMENT_3D('',#66077,#38774,#38775) ;
#33564 = AXIS2_PLACEMENT_3D('',#66078,#38776,#38777) ;
#33565 = AXIS2_PLACEMENT_3D('',#66080,#38778,#38779) ;
#33566 = AXIS2_PLACEMENT_3D('',#66083,#38781,#38782) ;
#33567 = AXIS2_PLACEMENT_3D('',#66084,#38783,#38784) ;
#33568 = AXIS2_PLACEMENT_3D('',#66086,#38785,#38786) ;
#33569 = AXIS2_PLACEMENT_3D('',#66090,#38788,#38789) ;
#33570 = AXIS2_PLACEMENT_3D('',#66091,#38790,#38791) ;
#33571 = AXIS2_PLACEMENT_3D('',#66092,#38792,#38793) ;
#33572 = AXIS2_PLACEMENT_3D('',#66094,#38795,#38796) ;
#33573 = AXIS2_PLACEMENT_3D('',#66096,#38797,#38798) ;
#33574 = AXIS2_PLACEMENT_3D('',#66100,#38800,#38801) ;
#33575 = AXIS2_PLACEMENT_3D('',#66101,#38802,#38803) ;
#33576 = AXIS2_PLACEMENT_3D('',#66102,#38804,#38805) ;
#33577 = AXIS2_PLACEMENT_3D('',#66104,#38807,#38808) ;
#33578 = AXIS2_PLACEMENT_3D('',#66106,#38809,#38810) ;
#33579 = AXIS2_PLACEMENT_3D('',#66110,#38812,#38813) ;
#33580 = AXIS2_PLACEMENT_3D('',#66111,#38814,#38815) ;
#33581 = AXIS2_PLACEMENT_3D('',#66112,#38816,#38817) ;
#33582 = AXIS2_PLACEMENT_3D('',#66114,#38819,#38820) ;
#33583 = AXIS2_PLACEMENT_3D('',#66116,#38821,#38822) ;
#33584 = AXIS2_PLACEMENT_3D('',#66120,#38824,#38825) ;
#33585 = AXIS2_PLACEMENT_3D('',#66121,#38826,#38827) ;
#33586 = AXIS2_PLACEMENT_3D('',#66122,#38828,#38829) ;
#33587 = AXIS2_PLACEMENT_3D('',#66124,#38831,#38832) ;
#33588 = AXIS2_PLACEMENT_3D('',#66130,#38836,#38837) ;
#33589 = AXIS2_PLACEMENT_3D('',#66131,#38838,#38839) ;
#33590 = AXIS2_PLACEMENT_3D('',#66132,#38840,#38841) ;
#33591 = AXIS2_PLACEMENT_3D('',#66133,#38842,#38843) ;
#33592 = AXIS2_PLACEMENT_3D('',#66134,#38844,#38845) ;
#33593 = AXIS2_PLACEMENT_3D('',#66137,#38847,#38848) ;
#33594 = AXIS2_PLACEMENT_3D('',#66140,#38851,#38852) ;
#33595 = AXIS2_PLACEMENT_3D('',#66144,#38856,#38857) ;
#33596 = AXIS2_PLACEMENT_3D('',#66147,#38860,#38861) ;
#33597 = AXIS2_PLACEMENT_3D('',#66149,#38863,#38864) ;
#33598 = AXIS2_PLACEMENT_3D('',#66151,#38866,#38867) ;
#33599 = AXIS2_PLACEMENT_3D('',#66152,#38868,#38869) ;
#33600 = AXIS2_PLACEMENT_3D('',#66158,#38873,#38874) ;
#33601 = AXIS2_PLACEMENT_3D('',#66161,#38877,#38878) ;
#33602 = AXIS2_PLACEMENT_3D('',#66162,#38879,#38880) ;
#33603 = AXIS2_PLACEMENT_3D('',#66163,#38881,#38882) ;
#33604 = AXIS2_PLACEMENT_3D('',#66164,#38883,#38884) ;
#33605 = AXIS2_PLACEMENT_3D('',#66165,#38885,#38886) ;
#33606 = AXIS2_PLACEMENT_3D('',#66166,#38887,#38888) ;
#33607 = AXIS2_PLACEMENT_3D('',#66169,#38891,#38892) ;
#33608 = AXIS2_PLACEMENT_3D('',#66171,#38894,#38895) ;
#33609 = AXIS2_PLACEMENT_3D('',#66173,#38897,#38898) ;
#33610 = AXIS2_PLACEMENT_3D('',#66174,#38899,#38900) ;
#33611 = AXIS2_PLACEMENT_3D('',#66177,#38903,#38904) ;
#33612 = AXIS2_PLACEMENT_3D('',#66179,#38906,#38907) ;
#33613 = AXIS2_PLACEMENT_3D('',#66181,#38909,#38910) ;
#33614 = AXIS2_PLACEMENT_3D('',#66182,#38911,#38912) ;
#33615 = AXIS2_PLACEMENT_3D('',#66183,#38913,#38914) ;
#33616 = AXIS2_PLACEMENT_3D('',#66184,#38915,#38916) ;
#33617 = AXIS2_PLACEMENT_3D('',#66185,#38917,#38918) ;
#33618 = AXIS2_PLACEMENT_3D('',#66186,#38919,#38920) ;
#33619 = AXIS2_PLACEMENT_3D('',#66187,#38921,#38922) ;
#33620 = AXIS2_PLACEMENT_3D('',#66188,#38923,#38924) ;
#33621 = AXIS2_PLACEMENT_3D('',#66189,#38925,#38926) ;
#33622 = AXIS2_PLACEMENT_3D('',#66192,#38928,#38929) ;
#33623 = AXIS2_PLACEMENT_3D('',#66193,#38930,#38931) ;
#33624 = AXIS2_PLACEMENT_3D('',#66196,#38934,#38935) ;
#33625 = AXIS2_PLACEMENT_3D('',#66198,#38936,#38937) ;
#33626 = AXIS2_PLACEMENT_3D('',#66200,#38939,#38940) ;
#33627 = AXIS2_PLACEMENT_3D('',#66203,#38943,#38944) ;
#33628 = AXIS2_PLACEMENT_3D('',#66204,#38945,#38946) ;
#33629 = AXIS2_PLACEMENT_3D('',#66205,#38947,#38948) ;
#33630 = AXIS2_PLACEMENT_3D('',#66206,#38949,#38950) ;
#33631 = AXIS2_PLACEMENT_3D('',#66207,#38951,#38952) ;
#33632 = AXIS2_PLACEMENT_3D('',#66213,#38956,#38957) ;
#33633 = AXIS2_PLACEMENT_3D('',#66216,#38958,#38959) ;
#33634 = AXIS2_PLACEMENT_3D('',#66218,#38961,#38962) ;
#33635 = AXIS2_PLACEMENT_3D('',#66219,#38963,#38964) ;
#33636 = AXIS2_PLACEMENT_3D('',#66957,#38966,#38967) ;
#33637 = AXIS2_PLACEMENT_3D('',#66963,#38971,#38972) ;
#33638 = AXIS2_PLACEMENT_3D('',#66969,#38976,#38977) ;
#33639 = AXIS2_PLACEMENT_3D('',#66975,#38981,#38982) ;
#33640 = AXIS2_PLACEMENT_3D('',#66981,#38986,#38987) ;
#33641 = AXIS2_PLACEMENT_3D('',#66982,#38988,#38989) ;
#33642 = AXIS2_PLACEMENT_3D('',#66983,#38990,#38991) ;
#33643 = AXIS2_PLACEMENT_3D('',#66984,#38992,#38993) ;
#33644 = AXIS2_PLACEMENT_3D('',#66985,#38994,#38995) ;
#33645 = AXIS2_PLACEMENT_3D('',#66986,#38996,#38997) ;
#33646 = AXIS2_PLACEMENT_3D('',#66987,#38998,#38999) ;
#33647 = AXIS2_PLACEMENT_3D('',#66988,#39000,#39001) ;
#33648 = AXIS2_PLACEMENT_3D('',#66989,#39002,#39003) ;
#33649 = AXIS2_PLACEMENT_3D('',#66990,#39004,#39005) ;
#33650 = AXIS2_PLACEMENT_3D('',#66991,#39006,#39007) ;
#33651 = AXIS2_PLACEMENT_3D('',#66992,#39008,#39009) ;
#33652 = AXIS2_PLACEMENT_3D('',#66993,#39010,#39011) ;
#33653 = AXIS2_PLACEMENT_3D('',#66994,#39012,#39013) ;
#33654 = AXIS2_PLACEMENT_3D('',#66995,#39014,#39015) ;
#33655 = AXIS2_PLACEMENT_3D('',#66996,#39016,#39017) ;
#33656 = AXIS2_PLACEMENT_3D('',#66997,#39018,#39019) ;
#33657 = AXIS2_PLACEMENT_3D('',#66998,#39020,#39021) ;
#33658 = AXIS2_PLACEMENT_3D('',#66999,#39022,#39023) ;
#33659 = AXIS2_PLACEMENT_3D('',#67000,#39024,#39025) ;
#33660 = AXIS2_PLACEMENT_3D('',#67001,#39026,#39027) ;
#33661 = AXIS2_PLACEMENT_3D('',#67002,#39028,#39029) ;
#33662 = AXIS2_PLACEMENT_3D('',#67003,#39030,#39031) ;
#33663 = AXIS2_PLACEMENT_3D('',#67004,#39032,#39033) ;
#33664 = AXIS2_PLACEMENT_3D('',#67005,#39034,#39035) ;
#33665 = AXIS2_PLACEMENT_3D('',#67007,#39036,#39037) ;
#33666 = AXIS2_PLACEMENT_3D('',#67010,#39039,#39040) ;
#33667 = AXIS2_PLACEMENT_3D('',#67011,#39041,#39042) ;
#33668 = AXIS2_PLACEMENT_3D('',#67012,#39043,#39044) ;
#33669 = AXIS2_PLACEMENT_3D('',#67013,#39045,#39046) ;
#33670 = AXIS2_PLACEMENT_3D('',#67015,#39047,#39048) ;
#33671 = AXIS2_PLACEMENT_3D('',#67017,#39050,#39051) ;
#33672 = AXIS2_PLACEMENT_3D('',#67018,#39052,#39053) ;
#33673 = AXIS2_PLACEMENT_3D('',#67019,#39054,#39055) ;
#33674 = AXIS2_PLACEMENT_3D('',#67021,#39057,#39058) ;
#33675 = AXIS2_PLACEMENT_3D('',#67023,#39059,#39060) ;
#33676 = AXIS2_PLACEMENT_3D('',#67025,#39062,#39063) ;
#33677 = AXIS2_PLACEMENT_3D('',#67027,#39064,#39065) ;
#33678 = AXIS2_PLACEMENT_3D('',#67029,#39067,#39068) ;
#33679 = AXIS2_PLACEMENT_3D('',#67031,#39069,#39070) ;
#33680 = AXIS2_PLACEMENT_3D('',#67034,#39072,#39073) ;
#33681 = AXIS2_PLACEMENT_3D('',#67044,#39074,#39075) ;
#33682 = AXIS2_PLACEMENT_3D('',#67045,#39076,#39077) ;
#33683 = AXIS2_PLACEMENT_3D('',#67046,#39078,#39079) ;
#33684 = AXIS2_PLACEMENT_3D('',#67056,#39080,#39081) ;
#33685 = AXIS2_PLACEMENT_3D('',#67058,#39082,#39083) ;
#33686 = AXIS2_PLACEMENT_3D('',#67062,#39085,#39086) ;
#33687 = AXIS2_PLACEMENT_3D('',#67064,#39088,#39089) ;
#33688 = AXIS2_PLACEMENT_3D('',#67065,#39090,#39091) ;
#33689 = AXIS2_PLACEMENT_3D('',#67075,#39092,#39093) ;
#33690 = AXIS2_PLACEMENT_3D('',#67076,#39094,#39095) ;
#33691 = AXIS2_PLACEMENT_3D('',#67077,#39096,#39097) ;
#33692 = AXIS2_PLACEMENT_3D('',#68689,#39098,#39099) ;
#33693 = AXIS2_PLACEMENT_3D('',#69260,#39118,#39119) ;
#33694 = AXIS2_PLACEMENT_3D('',#69266,#39123,#39124) ;
#33695 = AXIS2_PLACEMENT_3D('',#69270,#39127,#39128) ;
#33696 = AXIS2_PLACEMENT_3D('',#69274,#39131,#39132) ;
#33697 = AXIS2_PLACEMENT_3D('',#69278,#39135,#39136) ;
#33698 = AXIS2_PLACEMENT_3D('',#69282,#39139,#39140) ;
#33699 = AXIS2_PLACEMENT_3D('',#69284,#39142,#39143) ;
#33700 = AXIS2_PLACEMENT_3D('',#69290,#39147,#39148) ;
#33701 = AXIS2_PLACEMENT_3D('',#69294,#39151,#39152) ;
#33702 = AXIS2_PLACEMENT_3D('',#69298,#39155,#39156) ;
#33703 = AXIS2_PLACEMENT_3D('',#69302,#39159,#39160) ;
#33704 = AXIS2_PLACEMENT_3D('',#69306,#39163,#39164) ;
#33705 = AXIS2_PLACEMENT_3D('',#69308,#39166,#39167) ;
#33706 = AXIS2_PLACEMENT_3D('',#69321,#39174,#39175) ;
#33707 = AXIS2_PLACEMENT_3D('',#69324,#39178,#39179) ;
#33708 = AXIS2_PLACEMENT_3D('',#69326,#39181,#39182) ;
#33709 = AXIS2_PLACEMENT_3D('',#69328,#39184,#39185) ;
#33710 = AXIS2_PLACEMENT_3D('',#69330,#39187,#39188) ;
#33711 = AXIS2_PLACEMENT_3D('',#69332,#39190,#39191) ;
#33712 = AXIS2_PLACEMENT_3D('',#69333,#39192,#39193) ;
#33713 = AXIS2_PLACEMENT_3D('',#69334,#39194,#39195) ;
#33714 = AXIS2_PLACEMENT_3D('',#69335,#39196,#39197) ;
#33715 = AXIS2_PLACEMENT_3D('',#69336,#39198,#39199) ;
#33716 = AXIS2_PLACEMENT_3D('',#69337,#39200,#39201) ;
#33717 = AXIS2_PLACEMENT_3D('',#69338,#39202,#39203) ;
#33718 = AXIS2_PLACEMENT_3D('',#69339,#39204,#39205) ;
#33719 = AXIS2_PLACEMENT_3D('',#69340,#39206,#39207) ;
#33720 = AXIS2_PLACEMENT_3D('',#69349,#39212,#39213) ;
#33721 = AXIS2_PLACEMENT_3D('',#69355,#39217,#39218) ;
#33722 = AXIS2_PLACEMENT_3D('',#69361,#39222,#39223) ;
#33723 = AXIS2_PLACEMENT_3D('',#69363,#39225,#39226) ;
#33724 = AXIS2_PLACEMENT_3D('',#69372,#39231,#39232) ;
#33725 = AXIS2_PLACEMENT_3D('',#69378,#39236,#39237) ;
#33726 = AXIS2_PLACEMENT_3D('',#69384,#39241,#39242) ;
#33727 = AXIS2_PLACEMENT_3D('',#69386,#39244,#39245) ;
#33728 = AXIS2_PLACEMENT_3D('',#69395,#39250,#39251) ;
#33729 = AXIS2_PLACEMENT_3D('',#69401,#39255,#39256) ;
#33730 = AXIS2_PLACEMENT_3D('',#69407,#39260,#39261) ;
#33731 = AXIS2_PLACEMENT_3D('',#69409,#39263,#39264) ;
#33732 = AXIS2_PLACEMENT_3D('',#69418,#39269,#39270) ;
#33733 = AXIS2_PLACEMENT_3D('',#69424,#39274,#39275) ;
#33734 = AXIS2_PLACEMENT_3D('',#69430,#39279,#39280) ;
#33735 = AXIS2_PLACEMENT_3D('',#69432,#39282,#39283) ;
#33736 = AXIS2_PLACEMENT_3D('',#69441,#39288,#39289) ;
#33737 = AXIS2_PLACEMENT_3D('',#69447,#39293,#39294) ;
#33738 = AXIS2_PLACEMENT_3D('',#69453,#39298,#39299) ;
#33739 = AXIS2_PLACEMENT_3D('',#69455,#39301,#39302) ;
#33740 = AXIS2_PLACEMENT_3D('',#69464,#39307,#39308) ;
#33741 = AXIS2_PLACEMENT_3D('',#69470,#39312,#39313) ;
#33742 = AXIS2_PLACEMENT_3D('',#69476,#39317,#39318) ;
#33743 = AXIS2_PLACEMENT_3D('',#69478,#39320,#39321) ;
#33744 = AXIS2_PLACEMENT_3D('',#69487,#39326,#39327) ;
#33745 = AXIS2_PLACEMENT_3D('',#69493,#39331,#39332) ;
#33746 = AXIS2_PLACEMENT_3D('',#69499,#39336,#39337) ;
#33747 = AXIS2_PLACEMENT_3D('',#69501,#39339,#39340) ;
#33748 = AXIS2_PLACEMENT_3D('',#69510,#39345,#39346) ;
#33749 = AXIS2_PLACEMENT_3D('',#69516,#39350,#39351) ;
#33750 = AXIS2_PLACEMENT_3D('',#69522,#39355,#39356) ;
#33751 = AXIS2_PLACEMENT_3D('',#69524,#39358,#39359) ;
#33752 = AXIS2_PLACEMENT_3D('',#69533,#39364,#39365) ;
#33753 = AXIS2_PLACEMENT_3D('',#69539,#39369,#39370) ;
#33754 = AXIS2_PLACEMENT_3D('',#69545,#39374,#39375) ;
#33755 = AXIS2_PLACEMENT_3D('',#69547,#39377,#39378) ;
#33756 = AXIS2_PLACEMENT_3D('',#69637,#39428,#39429) ;
#33757 = AXIS2_PLACEMENT_3D('',#69639,#39430,#39431) ;
#33758 = AXIS2_PLACEMENT_3D('',#69641,#39432,#39433) ;
#33759 = AXIS2_PLACEMENT_3D('',#69642,#39434,#39435) ;
#33760 = AXIS2_PLACEMENT_3D('',#69643,#39436,#39437) ;
#33761 = AXIS2_PLACEMENT_3D('',#69645,#39438,#39439) ;
#33762 = AXIS2_PLACEMENT_3D('',#69647,#39441,#39442) ;
#33763 = AXIS2_PLACEMENT_3D('',#69660,#39448,#39449) ;
#33764 = AXIS2_PLACEMENT_3D('',#69664,#39451,#39452) ;
#33765 = AXIS2_PLACEMENT_3D('',#69668,#39454,#39455) ;
#33766 = AXIS2_PLACEMENT_3D('',#69671,#39457,#39458) ;
#33767 = AXIS2_PLACEMENT_3D('',#69672,#39459,#39460) ;
#33768 = AXIS2_PLACEMENT_3D('',#69674,#39461,#39462) ;
#33769 = AXIS2_PLACEMENT_3D('',#69676,#39463,#39464) ;
#33770 = AXIS2_PLACEMENT_3D('',#69677,#39465,#39466) ;
#33771 = AXIS2_PLACEMENT_3D('',#69678,#39467,#39468) ;
#33772 = AXIS2_PLACEMENT_3D('',#69680,#39469,#39470) ;
#33773 = AXIS2_PLACEMENT_3D('',#69682,#39472,#39473) ;
#33774 = AXIS2_PLACEMENT_3D('',#69695,#39479,#39480) ;
#33775 = AXIS2_PLACEMENT_3D('',#69699,#39482,#39483) ;
#33776 = AXIS2_PLACEMENT_3D('',#69703,#39485,#39486) ;
#33777 = AXIS2_PLACEMENT_3D('',#69706,#39488,#39489) ;
#33778 = AXIS2_PLACEMENT_3D('',#69707,#39490,#39491) ;
#33779 = AXIS2_PLACEMENT_3D('',#69709,#39492,#39493) ;
#33780 = AXIS2_PLACEMENT_3D('',#69711,#39494,#39495) ;
#33781 = AXIS2_PLACEMENT_3D('',#69712,#39496,#39497) ;
#33782 = AXIS2_PLACEMENT_3D('',#69713,#39498,#39499) ;
#33783 = AXIS2_PLACEMENT_3D('',#69715,#39500,#39501) ;
#33784 = AXIS2_PLACEMENT_3D('',#69717,#39503,#39504) ;
#33785 = AXIS2_PLACEMENT_3D('',#69730,#39510,#39511) ;
#33786 = AXIS2_PLACEMENT_3D('',#69734,#39513,#39514) ;
#33787 = AXIS2_PLACEMENT_3D('',#69738,#39516,#39517) ;
#33788 = AXIS2_PLACEMENT_3D('',#69741,#39519,#39520) ;
#33789 = AXIS2_PLACEMENT_3D('',#69742,#39521,#39522) ;
#33790 = AXIS2_PLACEMENT_3D('',#69744,#39523,#39524) ;
#33791 = AXIS2_PLACEMENT_3D('',#69746,#39525,#39526) ;
#33792 = AXIS2_PLACEMENT_3D('',#69747,#39527,#39528) ;
#33793 = AXIS2_PLACEMENT_3D('',#69748,#39529,#39530) ;
#33794 = AXIS2_PLACEMENT_3D('',#69750,#39531,#39532) ;
#33795 = AXIS2_PLACEMENT_3D('',#69752,#39534,#39535) ;
#33796 = AXIS2_PLACEMENT_3D('',#69765,#39541,#39542) ;
#33797 = AXIS2_PLACEMENT_3D('',#69769,#39544,#39545) ;
#33798 = AXIS2_PLACEMENT_3D('',#69773,#39547,#39548) ;
#33799 = AXIS2_PLACEMENT_3D('',#69776,#39550,#39551) ;
#33800 = AXIS2_PLACEMENT_3D('',#69777,#39552,#39553) ;
#33801 = AXIS2_PLACEMENT_3D('',#69779,#39554,#39555) ;
#33802 = AXIS2_PLACEMENT_3D('',#69781,#39556,#39557) ;
#33803 = AXIS2_PLACEMENT_3D('',#69782,#39558,#39559) ;
#33804 = AXIS2_PLACEMENT_3D('',#69783,#39560,#39561) ;
#33805 = AXIS2_PLACEMENT_3D('',#69785,#39562,#39563) ;
#33806 = AXIS2_PLACEMENT_3D('',#69787,#39565,#39566) ;
#33807 = AXIS2_PLACEMENT_3D('',#69800,#39572,#39573) ;
#33808 = AXIS2_PLACEMENT_3D('',#69804,#39575,#39576) ;
#33809 = AXIS2_PLACEMENT_3D('',#69808,#39578,#39579) ;
#33810 = AXIS2_PLACEMENT_3D('',#69811,#39581,#39582) ;
#33811 = AXIS2_PLACEMENT_3D('',#69812,#39583,#39584) ;
#33812 = AXIS2_PLACEMENT_3D('',#69814,#39585,#39586) ;
#33813 = AXIS2_PLACEMENT_3D('',#69816,#39587,#39588) ;
#33814 = AXIS2_PLACEMENT_3D('',#69817,#39589,#39590) ;
#33815 = AXIS2_PLACEMENT_3D('',#69818,#39591,#39592) ;
#33816 = AXIS2_PLACEMENT_3D('',#69820,#39593,#39594) ;
#33817 = AXIS2_PLACEMENT_3D('',#69822,#39596,#39597) ;
#33818 = AXIS2_PLACEMENT_3D('',#69835,#39603,#39604) ;
#33819 = AXIS2_PLACEMENT_3D('',#69839,#39606,#39607) ;
#33820 = AXIS2_PLACEMENT_3D('',#69843,#39609,#39610) ;
#33821 = AXIS2_PLACEMENT_3D('',#69846,#39612,#39613) ;
#33822 = AXIS2_PLACEMENT_3D('',#69847,#39614,#39615) ;
#33823 = AXIS2_PLACEMENT_3D('',#69849,#39616,#39617) ;
#33824 = AXIS2_PLACEMENT_3D('',#69851,#39618,#39619) ;
#33825 = AXIS2_PLACEMENT_3D('',#69852,#39620,#39621) ;
#33826 = AXIS2_PLACEMENT_3D('',#69853,#39622,#39623) ;
#33827 = AXIS2_PLACEMENT_3D('',#69855,#39624,#39625) ;
#33828 = AXIS2_PLACEMENT_3D('',#69857,#39627,#39628) ;
#33829 = AXIS2_PLACEMENT_3D('',#69870,#39634,#39635) ;
#33830 = AXIS2_PLACEMENT_3D('',#69874,#39637,#39638) ;
#33831 = AXIS2_PLACEMENT_3D('',#69878,#39640,#39641) ;
#33832 = AXIS2_PLACEMENT_3D('',#69881,#39643,#39644) ;
#33833 = AXIS2_PLACEMENT_3D('',#69882,#39645,#39646) ;
#33834 = AXIS2_PLACEMENT_3D('',#69884,#39647,#39648) ;
#33835 = AXIS2_PLACEMENT_3D('',#69886,#39649,#39650) ;
#33836 = AXIS2_PLACEMENT_3D('',#69887,#39651,#39652) ;
#33837 = AXIS2_PLACEMENT_3D('',#69888,#39653,#39654) ;
#33838 = AXIS2_PLACEMENT_3D('',#69890,#39655,#39656) ;
#33839 = AXIS2_PLACEMENT_3D('',#69892,#39658,#39659) ;
#33840 = AXIS2_PLACEMENT_3D('',#69905,#39665,#39666) ;
#33841 = AXIS2_PLACEMENT_3D('',#69909,#39668,#39669) ;
#33842 = AXIS2_PLACEMENT_3D('',#69913,#39671,#39672) ;
#33843 = AXIS2_PLACEMENT_3D('',#69916,#39674,#39675) ;
#33844 = AXIS2_PLACEMENT_3D('',#69917,#39676,#39677) ;
#33845 = AXIS2_PLACEMENT_3D('',#69919,#39678,#39679) ;
#33846 = AXIS2_PLACEMENT_3D('',#69921,#39680,#39681) ;
#33847 = AXIS2_PLACEMENT_3D('',#69922,#39682,#39683) ;
#33848 = AXIS2_PLACEMENT_3D('',#69923,#39684,#39685) ;
#33849 = AXIS2_PLACEMENT_3D('',#69936,#39691,#39692) ;
#33850 = AXIS2_PLACEMENT_3D('',#69940,#39694,#39695) ;
#33851 = AXIS2_PLACEMENT_3D('',#69944,#39697,#39698) ;
#33852 = AXIS2_PLACEMENT_3D('',#69947,#39700,#39701) ;
#33853 = AXIS2_PLACEMENT_3D('',#69948,#39702,#39703) ;
#33854 = AXIS2_PLACEMENT_3D('',#69950,#39704,#39705) ;
#33855 = AXIS2_PLACEMENT_3D('',#69952,#39707,#39708) ;
#33856 = AXIS2_PLACEMENT_3D('',#69954,#39709,#39710) ;
#33857 = AXIS2_PLACEMENT_3D('',#69955,#39711,#39712) ;
#33858 = AXIS2_PLACEMENT_3D('',#69957,#39713,#39714) ;
#33859 = AXIS2_PLACEMENT_3D('',#69958,#39715,#39716) ;
#33860 = AXIS2_PLACEMENT_3D('',#69960,#39717,#39718) ;
#33861 = AXIS2_PLACEMENT_3D('',#69961,#39719,#39720) ;
#33862 = AXIS2_PLACEMENT_3D('',#69963,#39721,#39722) ;
#33863 = AXIS2_PLACEMENT_3D('',#69964,#39723,#39724) ;
#33864 = AXIS2_PLACEMENT_3D('',#69966,#39725,#39726) ;
#33865 = AXIS2_PLACEMENT_3D('',#69967,#39727,#39728) ;
#33866 = AXIS2_PLACEMENT_3D('',#69969,#39729,#39730) ;
#33867 = AXIS2_PLACEMENT_3D('',#69970,#39731,#39732) ;
#33868 = AXIS2_PLACEMENT_3D('',#69972,#39733,#39734) ;
#33869 = AXIS2_PLACEMENT_3D('',#69973,#39735,#39736) ;
#33870 = AXIS2_PLACEMENT_3D('',#69975,#39737,#39738) ;
#33871 = AXIS2_PLACEMENT_3D('',#69976,#39739,#39740) ;
#33872 = AXIS2_PLACEMENT_3D('',#69978,#39741,#39742) ;
#33873 = AXIS2_PLACEMENT_3D('',#69981,#39744,#39745) ;
#33874 = AXIS2_PLACEMENT_3D('',#69982,#39746,#39747) ;
#33875 = AXIS2_PLACEMENT_3D('',#69984,#39748,#39749) ;
#33876 = AXIS2_PLACEMENT_3D('',#69985,#39750,#39751) ;
#33877 = AXIS2_PLACEMENT_3D('',#69986,#39752,#39753) ;
#33878 = AXIS2_PLACEMENT_3D('',#69988,#39754,#39755) ;
#33879 = AXIS2_PLACEMENT_3D('',#69990,#39757,#39758) ;
#33880 = AXIS2_PLACEMENT_3D('',#69992,#39759,#39760) ;
#33881 = AXIS2_PLACEMENT_3D('',#69993,#39761,#39762) ;
#33882 = AXIS2_PLACEMENT_3D('',#69994,#39763,#39764) ;
#33883 = AXIS2_PLACEMENT_3D('',#69996,#39765,#39766) ;
#33884 = AXIS2_PLACEMENT_3D('',#69998,#39768,#39769) ;
#33885 = AXIS2_PLACEMENT_3D('',#70000,#39770,#39771) ;
#33886 = AXIS2_PLACEMENT_3D('',#70001,#39772,#39773) ;
#33887 = AXIS2_PLACEMENT_3D('',#70002,#39774,#39775) ;
#33888 = AXIS2_PLACEMENT_3D('',#70004,#39776,#39777) ;
#33889 = AXIS2_PLACEMENT_3D('',#70006,#39779,#39780) ;
#33890 = AXIS2_PLACEMENT_3D('',#70007,#39781,#39782) ;
#33891 = AXIS2_PLACEMENT_3D('',#70008,#39783,#39784) ;
#33892 = AXIS2_PLACEMENT_3D('',#70012,#39786,#39787) ;
#33893 = AXIS2_PLACEMENT_3D('',#70014,#39789,#39790) ;
#33894 = AXIS2_PLACEMENT_3D('',#70018,#39792,#39793) ;
#33895 = AXIS2_PLACEMENT_3D('',#70029,#39799,#39800) ;
#33896 = AXIS2_PLACEMENT_3D('',#70030,#39801,#39802) ;
#33897 = AXIS2_PLACEMENT_3D('',#70033,#39804,#39805) ;
#33898 = AXIS2_PLACEMENT_3D('',#70034,#39806,#39807) ;
#33899 = AXIS2_PLACEMENT_3D('',#70038,#39810,#39811) ;
#33900 = AXIS2_PLACEMENT_3D('',#70040,#39812,#39813) ;
#33901 = AXIS2_PLACEMENT_3D('',#70043,#39815,#39816) ;
#33902 = AXIS2_PLACEMENT_3D('',#70044,#39817,#39818) ;
#33903 = AXIS2_PLACEMENT_3D('',#70046,#39819,#39820) ;
#33904 = AXIS2_PLACEMENT_3D('',#70047,#39821,#39822) ;
#33905 = AXIS2_PLACEMENT_3D('',#70048,#39823,#39824) ;
#33906 = AXIS2_PLACEMENT_3D('',#70050,#39825,#39826) ;
#33907 = AXIS2_PLACEMENT_3D('',#70052,#39828,#39829) ;
#33908 = AXIS2_PLACEMENT_3D('',#70054,#39830,#39831) ;
#33909 = AXIS2_PLACEMENT_3D('',#70055,#39832,#39833) ;
#33910 = AXIS2_PLACEMENT_3D('',#70056,#39834,#39835) ;
#33911 = AXIS2_PLACEMENT_3D('',#70058,#39836,#39837) ;
#33912 = AXIS2_PLACEMENT_3D('',#70060,#39839,#39840) ;
#33913 = AXIS2_PLACEMENT_3D('',#70062,#39841,#39842) ;
#33914 = AXIS2_PLACEMENT_3D('',#70063,#39843,#39844) ;
#33915 = AXIS2_PLACEMENT_3D('',#70064,#39845,#39846) ;
#33916 = AXIS2_PLACEMENT_3D('',#70066,#39847,#39848) ;
#33917 = AXIS2_PLACEMENT_3D('',#70068,#39850,#39851) ;
#33918 = AXIS2_PLACEMENT_3D('',#70069,#39852,#39853) ;
#33919 = AXIS2_PLACEMENT_3D('',#70070,#39854,#39855) ;
#33920 = AXIS2_PLACEMENT_3D('',#70074,#39857,#39858) ;
#33921 = AXIS2_PLACEMENT_3D('',#70076,#39860,#39861) ;
#33922 = AXIS2_PLACEMENT_3D('',#70080,#39863,#39864) ;
#33923 = AXIS2_PLACEMENT_3D('',#70091,#39870,#39871) ;
#33924 = AXIS2_PLACEMENT_3D('',#70092,#39872,#39873) ;
#33925 = AXIS2_PLACEMENT_3D('',#70095,#39875,#39876) ;
#33926 = AXIS2_PLACEMENT_3D('',#70096,#39877,#39878) ;
#33927 = AXIS2_PLACEMENT_3D('',#70100,#39881,#39882) ;
#33928 = AXIS2_PLACEMENT_3D('',#70102,#39883,#39884) ;
#33929 = AXIS2_PLACEMENT_3D('',#70105,#39886,#39887) ;
#33930 = AXIS2_PLACEMENT_3D('',#70106,#39888,#39889) ;
#33931 = AXIS2_PLACEMENT_3D('',#70108,#39890,#39891) ;
#33932 = AXIS2_PLACEMENT_3D('',#70109,#39892,#39893) ;
#33933 = AXIS2_PLACEMENT_3D('',#70110,#39894,#39895) ;
#33934 = AXIS2_PLACEMENT_3D('',#70112,#39896,#39897) ;
#33935 = AXIS2_PLACEMENT_3D('',#70114,#39899,#39900) ;
#33936 = AXIS2_PLACEMENT_3D('',#70116,#39901,#39902) ;
#33937 = AXIS2_PLACEMENT_3D('',#70117,#39903,#39904) ;
#33938 = AXIS2_PLACEMENT_3D('',#70118,#39905,#39906) ;
#33939 = AXIS2_PLACEMENT_3D('',#70120,#39907,#39908) ;
#33940 = AXIS2_PLACEMENT_3D('',#70122,#39910,#39911) ;
#33941 = AXIS2_PLACEMENT_3D('',#70124,#39912,#39913) ;
#33942 = AXIS2_PLACEMENT_3D('',#70125,#39914,#39915) ;
#33943 = AXIS2_PLACEMENT_3D('',#70126,#39916,#39917) ;
#33944 = AXIS2_PLACEMENT_3D('',#70128,#39918,#39919) ;
#33945 = AXIS2_PLACEMENT_3D('',#70130,#39921,#39922) ;
#33946 = AXIS2_PLACEMENT_3D('',#70131,#39923,#39924) ;
#33947 = AXIS2_PLACEMENT_3D('',#70132,#39925,#39926) ;
#33948 = AXIS2_PLACEMENT_3D('',#70136,#39928,#39929) ;
#33949 = AXIS2_PLACEMENT_3D('',#70138,#39931,#39932) ;
#33950 = AXIS2_PLACEMENT_3D('',#70142,#39934,#39935) ;
#33951 = AXIS2_PLACEMENT_3D('',#70153,#39941,#39942) ;
#33952 = AXIS2_PLACEMENT_3D('',#70154,#39943,#39944) ;
#33953 = AXIS2_PLACEMENT_3D('',#70157,#39946,#39947) ;
#33954 = AXIS2_PLACEMENT_3D('',#70158,#39948,#39949) ;
#33955 = AXIS2_PLACEMENT_3D('',#70162,#39952,#39953) ;
#33956 = AXIS2_PLACEMENT_3D('',#70164,#39954,#39955) ;
#33957 = AXIS2_PLACEMENT_3D('',#70167,#39957,#39958) ;
#33958 = AXIS2_PLACEMENT_3D('',#70168,#39959,#39960) ;
#33959 = AXIS2_PLACEMENT_3D('',#70170,#39961,#39962) ;
#33960 = AXIS2_PLACEMENT_3D('',#70171,#39963,#39964) ;
#33961 = AXIS2_PLACEMENT_3D('',#70172,#39965,#39966) ;
#33962 = AXIS2_PLACEMENT_3D('',#70174,#39967,#39968) ;
#33963 = AXIS2_PLACEMENT_3D('',#70176,#39970,#39971) ;
#33964 = AXIS2_PLACEMENT_3D('',#70178,#39972,#39973) ;
#33965 = AXIS2_PLACEMENT_3D('',#70179,#39974,#39975) ;
#33966 = AXIS2_PLACEMENT_3D('',#70180,#39976,#39977) ;
#33967 = AXIS2_PLACEMENT_3D('',#70182,#39978,#39979) ;
#33968 = AXIS2_PLACEMENT_3D('',#70184,#39981,#39982) ;
#33969 = AXIS2_PLACEMENT_3D('',#70186,#39983,#39984) ;
#33970 = AXIS2_PLACEMENT_3D('',#70187,#39985,#39986) ;
#33971 = AXIS2_PLACEMENT_3D('',#70188,#39987,#39988) ;
#33972 = AXIS2_PLACEMENT_3D('',#70190,#39989,#39990) ;
#33973 = AXIS2_PLACEMENT_3D('',#70192,#39992,#39993) ;
#33974 = AXIS2_PLACEMENT_3D('',#70193,#39994,#39995) ;
#33975 = AXIS2_PLACEMENT_3D('',#70194,#39996,#39997) ;
#33976 = AXIS2_PLACEMENT_3D('',#70198,#39999,#40000) ;
#33977 = AXIS2_PLACEMENT_3D('',#70200,#40002,#40003) ;
#33978 = AXIS2_PLACEMENT_3D('',#70204,#40005,#40006) ;
#33979 = AXIS2_PLACEMENT_3D('',#70215,#40012,#40013) ;
#33980 = AXIS2_PLACEMENT_3D('',#70216,#40014,#40015) ;
#33981 = AXIS2_PLACEMENT_3D('',#70219,#40017,#40018) ;
#33982 = AXIS2_PLACEMENT_3D('',#70220,#40019,#40020) ;
#33983 = AXIS2_PLACEMENT_3D('',#70224,#40023,#40024) ;
#33984 = AXIS2_PLACEMENT_3D('',#70226,#40025,#40026) ;
#33985 = AXIS2_PLACEMENT_3D('',#70229,#40028,#40029) ;
#33986 = AXIS2_PLACEMENT_3D('',#70230,#40030,#40031) ;
#33987 = AXIS2_PLACEMENT_3D('',#70232,#40032,#40033) ;
#33988 = AXIS2_PLACEMENT_3D('',#70233,#40034,#40035) ;
#33989 = AXIS2_PLACEMENT_3D('',#70234,#40036,#40037) ;
#33990 = AXIS2_PLACEMENT_3D('',#70236,#40038,#40039) ;
#33991 = AXIS2_PLACEMENT_3D('',#70238,#40041,#40042) ;
#33992 = AXIS2_PLACEMENT_3D('',#70240,#40043,#40044) ;
#33993 = AXIS2_PLACEMENT_3D('',#70241,#40045,#40046) ;
#33994 = AXIS2_PLACEMENT_3D('',#70242,#40047,#40048) ;
#33995 = AXIS2_PLACEMENT_3D('',#70244,#40049,#40050) ;
#33996 = AXIS2_PLACEMENT_3D('',#70246,#40052,#40053) ;
#33997 = AXIS2_PLACEMENT_3D('',#70248,#40054,#40055) ;
#33998 = AXIS2_PLACEMENT_3D('',#70249,#40056,#40057) ;
#33999 = AXIS2_PLACEMENT_3D('',#70250,#40058,#40059) ;
#34000 = AXIS2_PLACEMENT_3D('',#70252,#40060,#40061) ;
#34001 = AXIS2_PLACEMENT_3D('',#70254,#40063,#40064) ;
#34002 = AXIS2_PLACEMENT_3D('',#70255,#40065,#40066) ;
#34003 = AXIS2_PLACEMENT_3D('',#70256,#40067,#40068) ;
#34004 = AXIS2_PLACEMENT_3D('',#70260,#40070,#40071) ;
#34005 = AXIS2_PLACEMENT_3D('',#70262,#40073,#40074) ;
#34006 = AXIS2_PLACEMENT_3D('',#70266,#40076,#40077) ;
#34007 = AXIS2_PLACEMENT_3D('',#70277,#40083,#40084) ;
#34008 = AXIS2_PLACEMENT_3D('',#70278,#40085,#40086) ;
#34009 = AXIS2_PLACEMENT_3D('',#70281,#40088,#40089) ;
#34010 = AXIS2_PLACEMENT_3D('',#70282,#40090,#40091) ;
#34011 = AXIS2_PLACEMENT_3D('',#70286,#40094,#40095) ;
#34012 = AXIS2_PLACEMENT_3D('',#70288,#40096,#40097) ;
#34013 = AXIS2_PLACEMENT_3D('',#70291,#40099,#40100) ;
#34014 = AXIS2_PLACEMENT_3D('',#70292,#40101,#40102) ;
#34015 = AXIS2_PLACEMENT_3D('',#70294,#40103,#40104) ;
#34016 = AXIS2_PLACEMENT_3D('',#70295,#40105,#40106) ;
#34017 = AXIS2_PLACEMENT_3D('',#70296,#40107,#40108) ;
#34018 = AXIS2_PLACEMENT_3D('',#70298,#40109,#40110) ;
#34019 = AXIS2_PLACEMENT_3D('',#70300,#40112,#40113) ;
#34020 = AXIS2_PLACEMENT_3D('',#70302,#40114,#40115) ;
#34021 = AXIS2_PLACEMENT_3D('',#70303,#40116,#40117) ;
#34022 = AXIS2_PLACEMENT_3D('',#70304,#40118,#40119) ;
#34023 = AXIS2_PLACEMENT_3D('',#70306,#40120,#40121) ;
#34024 = AXIS2_PLACEMENT_3D('',#70308,#40123,#40124) ;
#34025 = AXIS2_PLACEMENT_3D('',#70310,#40125,#40126) ;
#34026 = AXIS2_PLACEMENT_3D('',#70311,#40127,#40128) ;
#34027 = AXIS2_PLACEMENT_3D('',#70312,#40129,#40130) ;
#34028 = AXIS2_PLACEMENT_3D('',#70314,#40131,#40132) ;
#34029 = AXIS2_PLACEMENT_3D('',#70316,#40134,#40135) ;
#34030 = AXIS2_PLACEMENT_3D('',#70317,#40136,#40137) ;
#34031 = AXIS2_PLACEMENT_3D('',#70318,#40138,#40139) ;
#34032 = AXIS2_PLACEMENT_3D('',#70322,#40141,#40142) ;
#34033 = AXIS2_PLACEMENT_3D('',#70324,#40144,#40145) ;
#34034 = AXIS2_PLACEMENT_3D('',#70328,#40147,#40148) ;
#34035 = AXIS2_PLACEMENT_3D('',#70339,#40154,#40155) ;
#34036 = AXIS2_PLACEMENT_3D('',#70340,#40156,#40157) ;
#34037 = AXIS2_PLACEMENT_3D('',#70343,#40159,#40160) ;
#34038 = AXIS2_PLACEMENT_3D('',#70344,#40161,#40162) ;
#34039 = AXIS2_PLACEMENT_3D('',#70348,#40165,#40166) ;
#34040 = AXIS2_PLACEMENT_3D('',#70350,#40167,#40168) ;
#34041 = AXIS2_PLACEMENT_3D('',#70353,#40170,#40171) ;
#34042 = AXIS2_PLACEMENT_3D('',#70354,#40172,#40173) ;
#34043 = AXIS2_PLACEMENT_3D('',#70356,#40174,#40175) ;
#34044 = AXIS2_PLACEMENT_3D('',#70357,#40176,#40177) ;
#34045 = AXIS2_PLACEMENT_3D('',#70358,#40178,#40179) ;
#34046 = AXIS2_PLACEMENT_3D('',#70360,#40180,#40181) ;
#34047 = AXIS2_PLACEMENT_3D('',#70362,#40183,#40184) ;
#34048 = AXIS2_PLACEMENT_3D('',#70364,#40185,#40186) ;
#34049 = AXIS2_PLACEMENT_3D('',#70365,#40187,#40188) ;
#34050 = AXIS2_PLACEMENT_3D('',#70366,#40189,#40190) ;
#34051 = AXIS2_PLACEMENT_3D('',#70368,#40191,#40192) ;
#34052 = AXIS2_PLACEMENT_3D('',#70370,#40194,#40195) ;
#34053 = AXIS2_PLACEMENT_3D('',#70372,#40196,#40197) ;
#34054 = AXIS2_PLACEMENT_3D('',#70373,#40198,#40199) ;
#34055 = AXIS2_PLACEMENT_3D('',#70374,#40200,#40201) ;
#34056 = AXIS2_PLACEMENT_3D('',#70376,#40202,#40203) ;
#34057 = AXIS2_PLACEMENT_3D('',#70378,#40205,#40206) ;
#34058 = AXIS2_PLACEMENT_3D('',#70379,#40207,#40208) ;
#34059 = AXIS2_PLACEMENT_3D('',#70380,#40209,#40210) ;
#34060 = AXIS2_PLACEMENT_3D('',#70384,#40212,#40213) ;
#34061 = AXIS2_PLACEMENT_3D('',#70386,#40215,#40216) ;
#34062 = AXIS2_PLACEMENT_3D('',#70390,#40218,#40219) ;
#34063 = AXIS2_PLACEMENT_3D('',#70401,#40225,#40226) ;
#34064 = AXIS2_PLACEMENT_3D('',#70402,#40227,#40228) ;
#34065 = AXIS2_PLACEMENT_3D('',#70405,#40230,#40231) ;
#34066 = AXIS2_PLACEMENT_3D('',#70406,#40232,#40233) ;
#34067 = AXIS2_PLACEMENT_3D('',#70410,#40236,#40237) ;
#34068 = AXIS2_PLACEMENT_3D('',#70412,#40238,#40239) ;
#34069 = AXIS2_PLACEMENT_3D('',#70415,#40241,#40242) ;
#34070 = AXIS2_PLACEMENT_3D('',#70416,#40243,#40244) ;
#34071 = AXIS2_PLACEMENT_3D('',#70418,#40245,#40246) ;
#34072 = AXIS2_PLACEMENT_3D('',#70419,#40247,#40248) ;
#34073 = AXIS2_PLACEMENT_3D('',#70420,#40249,#40250) ;
#34074 = AXIS2_PLACEMENT_3D('',#70422,#40251,#40252) ;
#34075 = AXIS2_PLACEMENT_3D('',#70424,#40254,#40255) ;
#34076 = AXIS2_PLACEMENT_3D('',#70426,#40256,#40257) ;
#34077 = AXIS2_PLACEMENT_3D('',#70427,#40258,#40259) ;
#34078 = AXIS2_PLACEMENT_3D('',#70428,#40260,#40261) ;
#34079 = AXIS2_PLACEMENT_3D('',#70430,#40262,#40263) ;
#34080 = AXIS2_PLACEMENT_3D('',#70432,#40265,#40266) ;
#34081 = AXIS2_PLACEMENT_3D('',#70434,#40267,#40268) ;
#34082 = AXIS2_PLACEMENT_3D('',#70435,#40269,#40270) ;
#34083 = AXIS2_PLACEMENT_3D('',#70436,#40271,#40272) ;
#34084 = AXIS2_PLACEMENT_3D('',#70438,#40273,#40274) ;
#34085 = AXIS2_PLACEMENT_3D('',#70440,#40276,#40277) ;
#34086 = AXIS2_PLACEMENT_3D('',#70441,#40278,#40279) ;
#34087 = AXIS2_PLACEMENT_3D('',#70442,#40280,#40281) ;
#34088 = AXIS2_PLACEMENT_3D('',#70446,#40283,#40284) ;
#34089 = AXIS2_PLACEMENT_3D('',#70448,#40286,#40287) ;
#34090 = AXIS2_PLACEMENT_3D('',#70452,#40289,#40290) ;
#34091 = AXIS2_PLACEMENT_3D('',#70463,#40296,#40297) ;
#34092 = AXIS2_PLACEMENT_3D('',#70464,#40298,#40299) ;
#34093 = AXIS2_PLACEMENT_3D('',#70467,#40301,#40302) ;
#34094 = AXIS2_PLACEMENT_3D('',#70468,#40303,#40304) ;
#34095 = AXIS2_PLACEMENT_3D('',#70472,#40307,#40308) ;
#34096 = AXIS2_PLACEMENT_3D('',#70474,#40309,#40310) ;
#34097 = AXIS2_PLACEMENT_3D('',#70477,#40312,#40313) ;
#34098 = AXIS2_PLACEMENT_3D('',#70478,#40314,#40315) ;
#34099 = AXIS2_PLACEMENT_3D('',#70480,#40316,#40317) ;
#34100 = AXIS2_PLACEMENT_3D('',#70481,#40318,#40319) ;
#34101 = AXIS2_PLACEMENT_3D('',#70482,#40320,#40321) ;
#34102 = AXIS2_PLACEMENT_3D('',#70484,#40322,#40323) ;
#34103 = AXIS2_PLACEMENT_3D('',#70486,#40325,#40326) ;
#34104 = AXIS2_PLACEMENT_3D('',#70488,#40327,#40328) ;
#34105 = AXIS2_PLACEMENT_3D('',#70489,#40329,#40330) ;
#34106 = AXIS2_PLACEMENT_3D('',#70490,#40331,#40332) ;
#34107 = AXIS2_PLACEMENT_3D('',#70492,#40333,#40334) ;
#34108 = AXIS2_PLACEMENT_3D('',#70494,#40336,#40337) ;
#34109 = AXIS2_PLACEMENT_3D('',#70496,#40338,#40339) ;
#34110 = AXIS2_PLACEMENT_3D('',#70497,#40340,#40341) ;
#34111 = AXIS2_PLACEMENT_3D('',#70498,#40342,#40343) ;
#34112 = AXIS2_PLACEMENT_3D('',#70500,#40344,#40345) ;
#34113 = AXIS2_PLACEMENT_3D('',#70502,#40347,#40348) ;
#34114 = AXIS2_PLACEMENT_3D('',#70503,#40349,#40350) ;
#34115 = AXIS2_PLACEMENT_3D('',#70504,#40351,#40352) ;
#34116 = AXIS2_PLACEMENT_3D('',#70508,#40354,#40355) ;
#34117 = AXIS2_PLACEMENT_3D('',#70510,#40357,#40358) ;
#34118 = AXIS2_PLACEMENT_3D('',#70518,#40362,#40363) ;
#34119 = AXIS2_PLACEMENT_3D('',#70522,#40365,#40366) ;
#34120 = AXIS2_PLACEMENT_3D('',#70526,#40369,#40370) ;
#34121 = AXIS2_PLACEMENT_3D('',#70529,#40372,#40373) ;
#34122 = AXIS2_PLACEMENT_3D('',#70530,#40374,#40375) ;
#34123 = AXIS2_PLACEMENT_3D('',#70534,#40378,#40379) ;
#34124 = AXIS2_PLACEMENT_3D('',#70537,#40380,#40381) ;
#34125 = AXIS2_PLACEMENT_3D('',#70541,#40383,#40384) ;
#34126 = AXIS2_PLACEMENT_3D('',#70543,#40386,#40387) ;
#34127 = AXIS2_PLACEMENT_3D('',#70546,#40388,#40389) ;
#34128 = AXIS2_PLACEMENT_3D('',#70547,#40390,#40391) ;
#34129 = AXIS2_PLACEMENT_3D('',#70548,#40392,#40393) ;
#34130 = AXIS2_PLACEMENT_3D('',#70549,#40394,#40395) ;
#34131 = AXIS2_PLACEMENT_3D('',#70552,#40396,#40397) ;
#34132 = AXIS2_PLACEMENT_3D('',#70555,#40400,#40401) ;
#34133 = AXIS2_PLACEMENT_3D('',#70558,#40402,#40403) ;
#34134 = AXIS2_PLACEMENT_3D('',#70559,#40404,#40405) ;
#34135 = AXIS2_PLACEMENT_3D('',#70560,#40406,#40407) ;
#34136 = AXIS2_PLACEMENT_3D('',#70561,#40408,#40409) ;
#34137 = AXIS2_PLACEMENT_3D('',#70564,#40410,#40411) ;
#34138 = AXIS2_PLACEMENT_3D('',#70567,#40414,#40415) ;
#34139 = AXIS2_PLACEMENT_3D('',#70570,#40416,#40417) ;
#34140 = AXIS2_PLACEMENT_3D('',#70571,#40418,#40419) ;
#34141 = AXIS2_PLACEMENT_3D('',#70572,#40420,#40421) ;
#34142 = AXIS2_PLACEMENT_3D('',#70573,#40422,#40423) ;
#34143 = AXIS2_PLACEMENT_3D('',#70576,#40424,#40425) ;
#34144 = AXIS2_PLACEMENT_3D('',#70579,#40428,#40429) ;
#34145 = AXIS2_PLACEMENT_3D('',#70580,#40430,#40431) ;
#34146 = AXIS2_PLACEMENT_3D('',#70581,#40432,#40433) ;
#34147 = AXIS2_PLACEMENT_3D('',#70582,#40434,#40435) ;
#34148 = AXIS2_PLACEMENT_3D('',#70586,#40437,#40438) ;
#34149 = AXIS2_PLACEMENT_3D('',#70588,#40440,#40441) ;
#34150 = AXIS2_PLACEMENT_3D('',#70592,#40444,#40445) ;
#34151 = AXIS2_PLACEMENT_3D('',#70595,#40447,#40448) ;
#34152 = AXIS2_PLACEMENT_3D('',#70596,#40449,#40450) ;
#34153 = AXIS2_PLACEMENT_3D('',#70600,#40453,#40454) ;
#34154 = AXIS2_PLACEMENT_3D('',#70603,#40455,#40456) ;
#34155 = AXIS2_PLACEMENT_3D('',#70607,#40458,#40459) ;
#34156 = AXIS2_PLACEMENT_3D('',#70609,#40461,#40462) ;
#34157 = AXIS2_PLACEMENT_3D('',#70612,#40463,#40464) ;
#34158 = AXIS2_PLACEMENT_3D('',#70613,#40465,#40466) ;
#34159 = AXIS2_PLACEMENT_3D('',#70614,#40467,#40468) ;
#34160 = AXIS2_PLACEMENT_3D('',#70615,#40469,#40470) ;
#34161 = AXIS2_PLACEMENT_3D('',#70618,#40471,#40472) ;
#34162 = AXIS2_PLACEMENT_3D('',#70621,#40475,#40476) ;
#34163 = AXIS2_PLACEMENT_3D('',#70624,#40477,#40478) ;
#34164 = AXIS2_PLACEMENT_3D('',#70625,#40479,#40480) ;
#34165 = AXIS2_PLACEMENT_3D('',#70626,#40481,#40482) ;
#34166 = AXIS2_PLACEMENT_3D('',#70627,#40483,#40484) ;
#34167 = AXIS2_PLACEMENT_3D('',#70630,#40485,#40486) ;
#34168 = AXIS2_PLACEMENT_3D('',#70633,#40489,#40490) ;
#34169 = AXIS2_PLACEMENT_3D('',#70636,#40491,#40492) ;
#34170 = AXIS2_PLACEMENT_3D('',#70637,#40493,#40494) ;
#34171 = AXIS2_PLACEMENT_3D('',#70638,#40495,#40496) ;
#34172 = AXIS2_PLACEMENT_3D('',#70639,#40497,#40498) ;
#34173 = AXIS2_PLACEMENT_3D('',#70642,#40499,#40500) ;
#34174 = AXIS2_PLACEMENT_3D('',#70645,#40503,#40504) ;
#34175 = AXIS2_PLACEMENT_3D('',#70646,#40505,#40506) ;
#34176 = AXIS2_PLACEMENT_3D('',#70647,#40507,#40508) ;
#34177 = AXIS2_PLACEMENT_3D('',#70648,#40509,#40510) ;
#34178 = AXIS2_PLACEMENT_3D('',#70652,#40512,#40513) ;
#34179 = AXIS2_PLACEMENT_3D('',#70654,#40515,#40516) ;
#34180 = AXIS2_PLACEMENT_3D('',#70658,#40519,#40520) ;
#34181 = AXIS2_PLACEMENT_3D('',#70661,#40522,#40523) ;
#34182 = AXIS2_PLACEMENT_3D('',#70662,#40524,#40525) ;
#34183 = AXIS2_PLACEMENT_3D('',#70666,#40528,#40529) ;
#34184 = AXIS2_PLACEMENT_3D('',#70669,#40530,#40531) ;
#34185 = AXIS2_PLACEMENT_3D('',#70673,#40533,#40534) ;
#34186 = AXIS2_PLACEMENT_3D('',#70675,#40536,#40537) ;
#34187 = AXIS2_PLACEMENT_3D('',#70678,#40538,#40539) ;
#34188 = AXIS2_PLACEMENT_3D('',#70679,#40540,#40541) ;
#34189 = AXIS2_PLACEMENT_3D('',#70680,#40542,#40543) ;
#34190 = AXIS2_PLACEMENT_3D('',#70681,#40544,#40545) ;
#34191 = AXIS2_PLACEMENT_3D('',#70684,#40546,#40547) ;
#34192 = AXIS2_PLACEMENT_3D('',#70687,#40550,#40551) ;
#34193 = AXIS2_PLACEMENT_3D('',#70690,#40552,#40553) ;
#34194 = AXIS2_PLACEMENT_3D('',#70691,#40554,#40555) ;
#34195 = AXIS2_PLACEMENT_3D('',#70692,#40556,#40557) ;
#34196 = AXIS2_PLACEMENT_3D('',#70693,#40558,#40559) ;
#34197 = AXIS2_PLACEMENT_3D('',#70696,#40560,#40561) ;
#34198 = AXIS2_PLACEMENT_3D('',#70699,#40564,#40565) ;
#34199 = AXIS2_PLACEMENT_3D('',#70702,#40566,#40567) ;
#34200 = AXIS2_PLACEMENT_3D('',#70703,#40568,#40569) ;
#34201 = AXIS2_PLACEMENT_3D('',#70704,#40570,#40571) ;
#34202 = AXIS2_PLACEMENT_3D('',#70705,#40572,#40573) ;
#34203 = AXIS2_PLACEMENT_3D('',#70708,#40574,#40575) ;
#34204 = AXIS2_PLACEMENT_3D('',#70711,#40578,#40579) ;
#34205 = AXIS2_PLACEMENT_3D('',#70712,#40580,#40581) ;
#34206 = AXIS2_PLACEMENT_3D('',#70713,#40582,#40583) ;
#34207 = AXIS2_PLACEMENT_3D('',#70714,#40584,#40585) ;
#34208 = AXIS2_PLACEMENT_3D('',#70718,#40587,#40588) ;
#34209 = AXIS2_PLACEMENT_3D('',#70720,#40590,#40591) ;
#34210 = AXIS2_PLACEMENT_3D('',#70724,#40594,#40595) ;
#34211 = AXIS2_PLACEMENT_3D('',#70727,#40597,#40598) ;
#34212 = AXIS2_PLACEMENT_3D('',#70728,#40599,#40600) ;
#34213 = AXIS2_PLACEMENT_3D('',#70732,#40603,#40604) ;
#34214 = AXIS2_PLACEMENT_3D('',#70735,#40605,#40606) ;
#34215 = AXIS2_PLACEMENT_3D('',#70739,#40608,#40609) ;
#34216 = AXIS2_PLACEMENT_3D('',#70741,#40611,#40612) ;
#34217 = AXIS2_PLACEMENT_3D('',#70744,#40613,#40614) ;
#34218 = AXIS2_PLACEMENT_3D('',#70745,#40615,#40616) ;
#34219 = AXIS2_PLACEMENT_3D('',#70746,#40617,#40618) ;
#34220 = AXIS2_PLACEMENT_3D('',#70747,#40619,#40620) ;
#34221 = AXIS2_PLACEMENT_3D('',#70750,#40621,#40622) ;
#34222 = AXIS2_PLACEMENT_3D('',#70753,#40625,#40626) ;
#34223 = AXIS2_PLACEMENT_3D('',#70756,#40627,#40628) ;
#34224 = AXIS2_PLACEMENT_3D('',#70757,#40629,#40630) ;
#34225 = AXIS2_PLACEMENT_3D('',#70758,#40631,#40632) ;
#34226 = AXIS2_PLACEMENT_3D('',#70759,#40633,#40634) ;
#34227 = AXIS2_PLACEMENT_3D('',#70762,#40635,#40636) ;
#34228 = AXIS2_PLACEMENT_3D('',#70765,#40639,#40640) ;
#34229 = AXIS2_PLACEMENT_3D('',#70768,#40641,#40642) ;
#34230 = AXIS2_PLACEMENT_3D('',#70769,#40643,#40644) ;
#34231 = AXIS2_PLACEMENT_3D('',#70770,#40645,#40646) ;
#34232 = AXIS2_PLACEMENT_3D('',#70771,#40647,#40648) ;
#34233 = AXIS2_PLACEMENT_3D('',#70774,#40649,#40650) ;
#34234 = AXIS2_PLACEMENT_3D('',#70777,#40653,#40654) ;
#34235 = AXIS2_PLACEMENT_3D('',#70778,#40655,#40656) ;
#34236 = AXIS2_PLACEMENT_3D('',#70779,#40657,#40658) ;
#34237 = AXIS2_PLACEMENT_3D('',#70780,#40659,#40660) ;
#34238 = AXIS2_PLACEMENT_3D('',#70784,#40662,#40663) ;
#34239 = AXIS2_PLACEMENT_3D('',#70786,#40665,#40666) ;
#34240 = AXIS2_PLACEMENT_3D('',#70790,#40669,#40670) ;
#34241 = AXIS2_PLACEMENT_3D('',#70793,#40672,#40673) ;
#34242 = AXIS2_PLACEMENT_3D('',#70794,#40674,#40675) ;
#34243 = AXIS2_PLACEMENT_3D('',#70798,#40678,#40679) ;
#34244 = AXIS2_PLACEMENT_3D('',#70801,#40680,#40681) ;
#34245 = AXIS2_PLACEMENT_3D('',#70805,#40683,#40684) ;
#34246 = AXIS2_PLACEMENT_3D('',#70807,#40686,#40687) ;
#34247 = AXIS2_PLACEMENT_3D('',#70810,#40688,#40689) ;
#34248 = AXIS2_PLACEMENT_3D('',#70811,#40690,#40691) ;
#34249 = AXIS2_PLACEMENT_3D('',#70812,#40692,#40693) ;
#34250 = AXIS2_PLACEMENT_3D('',#70813,#40694,#40695) ;
#34251 = AXIS2_PLACEMENT_3D('',#70816,#40696,#40697) ;
#34252 = AXIS2_PLACEMENT_3D('',#70819,#40700,#40701) ;
#34253 = AXIS2_PLACEMENT_3D('',#70822,#40702,#40703) ;
#34254 = AXIS2_PLACEMENT_3D('',#70823,#40704,#40705) ;
#34255 = AXIS2_PLACEMENT_3D('',#70824,#40706,#40707) ;
#34256 = AXIS2_PLACEMENT_3D('',#70825,#40708,#40709) ;
#34257 = AXIS2_PLACEMENT_3D('',#70828,#40710,#40711) ;
#34258 = AXIS2_PLACEMENT_3D('',#70831,#40714,#40715) ;
#34259 = AXIS2_PLACEMENT_3D('',#70834,#40716,#40717) ;
#34260 = AXIS2_PLACEMENT_3D('',#70835,#40718,#40719) ;
#34261 = AXIS2_PLACEMENT_3D('',#70836,#40720,#40721) ;
#34262 = AXIS2_PLACEMENT_3D('',#70837,#40722,#40723) ;
#34263 = AXIS2_PLACEMENT_3D('',#70840,#40724,#40725) ;
#34264 = AXIS2_PLACEMENT_3D('',#70843,#40728,#40729) ;
#34265 = AXIS2_PLACEMENT_3D('',#70844,#40730,#40731) ;
#34266 = AXIS2_PLACEMENT_3D('',#70845,#40732,#40733) ;
#34267 = AXIS2_PLACEMENT_3D('',#70846,#40734,#40735) ;
#34268 = AXIS2_PLACEMENT_3D('',#70850,#40737,#40738) ;
#34269 = AXIS2_PLACEMENT_3D('',#70852,#40740,#40741) ;
#34270 = AXIS2_PLACEMENT_3D('',#70856,#40744,#40745) ;
#34271 = AXIS2_PLACEMENT_3D('',#70859,#40747,#40748) ;
#34272 = AXIS2_PLACEMENT_3D('',#70860,#40749,#40750) ;
#34273 = AXIS2_PLACEMENT_3D('',#70864,#40753,#40754) ;
#34274 = AXIS2_PLACEMENT_3D('',#70867,#40755,#40756) ;
#34275 = AXIS2_PLACEMENT_3D('',#70871,#40758,#40759) ;
#34276 = AXIS2_PLACEMENT_3D('',#70873,#40761,#40762) ;
#34277 = AXIS2_PLACEMENT_3D('',#70876,#40763,#40764) ;
#34278 = AXIS2_PLACEMENT_3D('',#70877,#40765,#40766) ;
#34279 = AXIS2_PLACEMENT_3D('',#70878,#40767,#40768) ;
#34280 = AXIS2_PLACEMENT_3D('',#70879,#40769,#40770) ;
#34281 = AXIS2_PLACEMENT_3D('',#70882,#40771,#40772) ;
#34282 = AXIS2_PLACEMENT_3D('',#70885,#40775,#40776) ;
#34283 = AXIS2_PLACEMENT_3D('',#70888,#40777,#40778) ;
#34284 = AXIS2_PLACEMENT_3D('',#70889,#40779,#40780) ;
#34285 = AXIS2_PLACEMENT_3D('',#70890,#40781,#40782) ;
#34286 = AXIS2_PLACEMENT_3D('',#70891,#40783,#40784) ;
#34287 = AXIS2_PLACEMENT_3D('',#70894,#40785,#40786) ;
#34288 = AXIS2_PLACEMENT_3D('',#70897,#40789,#40790) ;
#34289 = AXIS2_PLACEMENT_3D('',#70900,#40791,#40792) ;
#34290 = AXIS2_PLACEMENT_3D('',#70901,#40793,#40794) ;
#34291 = AXIS2_PLACEMENT_3D('',#70902,#40795,#40796) ;
#34292 = AXIS2_PLACEMENT_3D('',#70903,#40797,#40798) ;
#34293 = AXIS2_PLACEMENT_3D('',#70906,#40799,#40800) ;
#34294 = AXIS2_PLACEMENT_3D('',#70909,#40803,#40804) ;
#34295 = AXIS2_PLACEMENT_3D('',#70910,#40805,#40806) ;
#34296 = AXIS2_PLACEMENT_3D('',#70911,#40807,#40808) ;
#34297 = AXIS2_PLACEMENT_3D('',#70912,#40809,#40810) ;
#34298 = AXIS2_PLACEMENT_3D('',#70916,#40812,#40813) ;
#34299 = AXIS2_PLACEMENT_3D('',#70918,#40815,#40816) ;
#34300 = AXIS2_PLACEMENT_3D('',#70922,#40819,#40820) ;
#34301 = AXIS2_PLACEMENT_3D('',#70925,#40822,#40823) ;
#34302 = AXIS2_PLACEMENT_3D('',#70926,#40824,#40825) ;
#34303 = AXIS2_PLACEMENT_3D('',#70930,#40828,#40829) ;
#34304 = AXIS2_PLACEMENT_3D('',#70933,#40830,#40831) ;
#34305 = AXIS2_PLACEMENT_3D('',#70937,#40833,#40834) ;
#34306 = AXIS2_PLACEMENT_3D('',#70939,#40836,#40837) ;
#34307 = AXIS2_PLACEMENT_3D('',#70942,#40838,#40839) ;
#34308 = AXIS2_PLACEMENT_3D('',#70943,#40840,#40841) ;
#34309 = AXIS2_PLACEMENT_3D('',#70944,#40842,#40843) ;
#34310 = AXIS2_PLACEMENT_3D('',#70945,#40844,#40845) ;
#34311 = AXIS2_PLACEMENT_3D('',#70948,#40846,#40847) ;
#34312 = AXIS2_PLACEMENT_3D('',#70951,#40850,#40851) ;
#34313 = AXIS2_PLACEMENT_3D('',#70954,#40852,#40853) ;
#34314 = AXIS2_PLACEMENT_3D('',#70955,#40854,#40855) ;
#34315 = AXIS2_PLACEMENT_3D('',#70956,#40856,#40857) ;
#34316 = AXIS2_PLACEMENT_3D('',#70957,#40858,#40859) ;
#34317 = AXIS2_PLACEMENT_3D('',#70960,#40860,#40861) ;
#34318 = AXIS2_PLACEMENT_3D('',#70963,#40864,#40865) ;
#34319 = AXIS2_PLACEMENT_3D('',#70966,#40866,#40867) ;
#34320 = AXIS2_PLACEMENT_3D('',#70967,#40868,#40869) ;
#34321 = AXIS2_PLACEMENT_3D('',#70968,#40870,#40871) ;
#34322 = AXIS2_PLACEMENT_3D('',#70969,#40872,#40873) ;
#34323 = AXIS2_PLACEMENT_3D('',#70972,#40874,#40875) ;
#34324 = AXIS2_PLACEMENT_3D('',#70975,#40878,#40879) ;
#34325 = AXIS2_PLACEMENT_3D('',#70976,#40880,#40881) ;
#34326 = AXIS2_PLACEMENT_3D('',#70977,#40882,#40883) ;
#34327 = AXIS2_PLACEMENT_3D('',#70978,#40884,#40885) ;
#34328 = AXIS2_PLACEMENT_3D('',#70982,#40887,#40888) ;
#34329 = AXIS2_PLACEMENT_3D('',#70984,#40890,#40891) ;
#34330 = AXIS2_PLACEMENT_3D('',#70988,#40894,#40895) ;
#34331 = AXIS2_PLACEMENT_3D('',#70991,#40897,#40898) ;
#34332 = AXIS2_PLACEMENT_3D('',#70992,#40899,#40900) ;
#34333 = AXIS2_PLACEMENT_3D('',#70996,#40903,#40904) ;
#34334 = AXIS2_PLACEMENT_3D('',#70999,#40905,#40906) ;
#34335 = AXIS2_PLACEMENT_3D('',#71003,#40908,#40909) ;
#34336 = AXIS2_PLACEMENT_3D('',#71005,#40911,#40912) ;
#34337 = AXIS2_PLACEMENT_3D('',#71008,#40913,#40914) ;
#34338 = AXIS2_PLACEMENT_3D('',#71009,#40915,#40916) ;
#34339 = AXIS2_PLACEMENT_3D('',#71010,#40917,#40918) ;
#34340 = AXIS2_PLACEMENT_3D('',#71011,#40919,#40920) ;
#34341 = AXIS2_PLACEMENT_3D('',#71014,#40921,#40922) ;
#34342 = AXIS2_PLACEMENT_3D('',#71017,#40925,#40926) ;
#34343 = AXIS2_PLACEMENT_3D('',#71020,#40927,#40928) ;
#34344 = AXIS2_PLACEMENT_3D('',#71021,#40929,#40930) ;
#34345 = AXIS2_PLACEMENT_3D('',#71022,#40931,#40932) ;
#34346 = AXIS2_PLACEMENT_3D('',#71023,#40933,#40934) ;
#34347 = AXIS2_PLACEMENT_3D('',#71026,#40935,#40936) ;
#34348 = AXIS2_PLACEMENT_3D('',#71029,#40939,#40940) ;
#34349 = AXIS2_PLACEMENT_3D('',#71032,#40941,#40942) ;
#34350 = AXIS2_PLACEMENT_3D('',#71033,#40943,#40944) ;
#34351 = AXIS2_PLACEMENT_3D('',#71034,#40945,#40946) ;
#34352 = AXIS2_PLACEMENT_3D('',#71035,#40947,#40948) ;
#34353 = AXIS2_PLACEMENT_3D('',#71038,#40949,#40950) ;
#34354 = AXIS2_PLACEMENT_3D('',#71041,#40953,#40954) ;
#34355 = AXIS2_PLACEMENT_3D('',#71042,#40955,#40956) ;
#34356 = AXIS2_PLACEMENT_3D('',#71043,#40957,#40958) ;
#34357 = AXIS2_PLACEMENT_3D('',#71044,#40959,#40960) ;
#34358 = AXIS2_PLACEMENT_3D('',#71048,#40962,#40963) ;
#34359 = AXIS2_PLACEMENT_3D('',#71050,#40965,#40966) ;
#34360 = AXIS2_PLACEMENT_3D('',#71054,#40969,#40970) ;
#34361 = AXIS2_PLACEMENT_3D('',#71057,#40972,#40973) ;
#34362 = AXIS2_PLACEMENT_3D('',#71058,#40974,#40975) ;
#34363 = AXIS2_PLACEMENT_3D('',#71062,#40978,#40979) ;
#34364 = AXIS2_PLACEMENT_3D('',#71065,#40980,#40981) ;
#34365 = AXIS2_PLACEMENT_3D('',#71069,#40983,#40984) ;
#34366 = AXIS2_PLACEMENT_3D('',#71071,#40986,#40987) ;
#34367 = AXIS2_PLACEMENT_3D('',#71074,#40988,#40989) ;
#34368 = AXIS2_PLACEMENT_3D('',#71075,#40990,#40991) ;
#34369 = AXIS2_PLACEMENT_3D('',#71076,#40992,#40993) ;
#34370 = AXIS2_PLACEMENT_3D('',#71077,#40994,#40995) ;
#34371 = AXIS2_PLACEMENT_3D('',#71080,#40996,#40997) ;
#34372 = AXIS2_PLACEMENT_3D('',#71083,#41000,#41001) ;
#34373 = AXIS2_PLACEMENT_3D('',#71086,#41002,#41003) ;
#34374 = AXIS2_PLACEMENT_3D('',#71087,#41004,#41005) ;
#34375 = AXIS2_PLACEMENT_3D('',#71088,#41006,#41007) ;
#34376 = AXIS2_PLACEMENT_3D('',#71089,#41008,#41009) ;
#34377 = AXIS2_PLACEMENT_3D('',#71092,#41010,#41011) ;
#34378 = AXIS2_PLACEMENT_3D('',#71095,#41014,#41015) ;
#34379 = AXIS2_PLACEMENT_3D('',#71097,#41016,#41017) ;
#34380 = AXIS2_PLACEMENT_3D('',#71098,#41018,#41019) ;
#34381 = AXIS2_PLACEMENT_3D('',#71099,#41020,#41021) ;
#34382 = AXIS2_PLACEMENT_3D('',#71100,#41022,#41023) ;
#34383 = AXIS2_PLACEMENT_3D('',#71102,#41024,#41025) ;
#34384 = AXIS2_PLACEMENT_3D('',#71104,#41027,#41028) ;
#34385 = AXIS2_PLACEMENT_3D('',#71105,#41029,#41030) ;
#34386 = AXIS2_PLACEMENT_3D('',#71106,#41031,#41032) ;
#34387 = AXIS2_PLACEMENT_3D('',#71107,#41033,#41034) ;
#34388 = AXIS2_PLACEMENT_3D('',#71111,#41036,#41037) ;
#34389 = AXIS2_PLACEMENT_3D('',#71113,#41039,#41040) ;
#34390 = AXIS2_PLACEMENT_3D('',#71117,#41042,#41043) ;
#34391 = AXIS2_PLACEMENT_3D('',#71124,#41047,#41048) ;
#34392 = AXIS2_PLACEMENT_3D('',#71126,#41050,#41051) ;
#34393 = AXIS2_PLACEMENT_3D('',#71129,#41053,#41054) ;
#34394 = AXIS2_PLACEMENT_3D('',#71130,#41055,#41056) ;
#34395 = AXIS2_PLACEMENT_3D('',#71134,#41059,#41060) ;
#34396 = AXIS2_PLACEMENT_3D('',#71137,#41061,#41062) ;
#34397 = AXIS2_PLACEMENT_3D('',#71141,#41064,#41065) ;
#34398 = AXIS2_PLACEMENT_3D('',#71143,#41067,#41068) ;
#34399 = AXIS2_PLACEMENT_3D('',#71146,#41069,#41070) ;
#34400 = AXIS2_PLACEMENT_3D('',#71147,#41071,#41072) ;
#34401 = AXIS2_PLACEMENT_3D('',#71148,#41073,#41074) ;
#34402 = AXIS2_PLACEMENT_3D('',#71149,#41075,#41076) ;
#34403 = AXIS2_PLACEMENT_3D('',#71152,#41077,#41078) ;
#34404 = AXIS2_PLACEMENT_3D('',#71155,#41081,#41082) ;
#34405 = AXIS2_PLACEMENT_3D('',#71158,#41083,#41084) ;
#34406 = AXIS2_PLACEMENT_3D('',#71159,#41085,#41086) ;
#34407 = AXIS2_PLACEMENT_3D('',#71160,#41087,#41088) ;
#34408 = AXIS2_PLACEMENT_3D('',#71161,#41089,#41090) ;
#34409 = AXIS2_PLACEMENT_3D('',#71164,#41091,#41092) ;
#34410 = AXIS2_PLACEMENT_3D('',#71167,#41095,#41096) ;
#34411 = AXIS2_PLACEMENT_3D('',#71169,#41097,#41098) ;
#34412 = AXIS2_PLACEMENT_3D('',#71170,#41099,#41100) ;
#34413 = AXIS2_PLACEMENT_3D('',#71171,#41101,#41102) ;
#34414 = AXIS2_PLACEMENT_3D('',#71172,#41103,#41104) ;
#34415 = AXIS2_PLACEMENT_3D('',#71174,#41105,#41106) ;
#34416 = AXIS2_PLACEMENT_3D('',#71176,#41108,#41109) ;
#34417 = AXIS2_PLACEMENT_3D('',#71177,#41110,#41111) ;
#34418 = AXIS2_PLACEMENT_3D('',#71178,#41112,#41113) ;
#34419 = AXIS2_PLACEMENT_3D('',#71179,#41114,#41115) ;
#34420 = AXIS2_PLACEMENT_3D('',#71183,#41117,#41118) ;
#34421 = AXIS2_PLACEMENT_3D('',#71185,#41120,#41121) ;
#34422 = AXIS2_PLACEMENT_3D('',#71189,#41123,#41124) ;
#34423 = AXIS2_PLACEMENT_3D('',#71196,#41128,#41129) ;
#34424 = AXIS2_PLACEMENT_3D('',#71198,#41131,#41132) ;
#34425 = AXIS2_PLACEMENT_3D('',#71201,#41134,#41135) ;
#34426 = AXIS2_PLACEMENT_3D('',#71202,#41136,#41137) ;
#34427 = AXIS2_PLACEMENT_3D('',#71206,#41140,#41141) ;
#34428 = AXIS2_PLACEMENT_3D('',#71209,#41142,#41143) ;
#34429 = AXIS2_PLACEMENT_3D('',#71213,#41145,#41146) ;
#34430 = AXIS2_PLACEMENT_3D('',#71215,#41148,#41149) ;
#34431 = AXIS2_PLACEMENT_3D('',#71218,#41150,#41151) ;
#34432 = AXIS2_PLACEMENT_3D('',#71219,#41152,#41153) ;
#34433 = AXIS2_PLACEMENT_3D('',#71220,#41154,#41155) ;
#34434 = AXIS2_PLACEMENT_3D('',#71221,#41156,#41157) ;
#34435 = AXIS2_PLACEMENT_3D('',#71224,#41158,#41159) ;
#34436 = AXIS2_PLACEMENT_3D('',#71227,#41162,#41163) ;
#34437 = AXIS2_PLACEMENT_3D('',#71230,#41164,#41165) ;
#34438 = AXIS2_PLACEMENT_3D('',#71231,#41166,#41167) ;
#34439 = AXIS2_PLACEMENT_3D('',#71232,#41168,#41169) ;
#34440 = AXIS2_PLACEMENT_3D('',#71233,#41170,#41171) ;
#34441 = AXIS2_PLACEMENT_3D('',#71236,#41172,#41173) ;
#34442 = AXIS2_PLACEMENT_3D('',#71239,#41176,#41177) ;
#34443 = AXIS2_PLACEMENT_3D('',#71241,#41178,#41179) ;
#34444 = AXIS2_PLACEMENT_3D('',#71242,#41180,#41181) ;
#34445 = AXIS2_PLACEMENT_3D('',#71243,#41182,#41183) ;
#34446 = AXIS2_PLACEMENT_3D('',#71244,#41184,#41185) ;
#34447 = AXIS2_PLACEMENT_3D('',#71246,#41186,#41187) ;
#34448 = AXIS2_PLACEMENT_3D('',#71248,#41189,#41190) ;
#34449 = AXIS2_PLACEMENT_3D('',#71249,#41191,#41192) ;
#34450 = AXIS2_PLACEMENT_3D('',#71250,#41193,#41194) ;
#34451 = AXIS2_PLACEMENT_3D('',#71251,#41195,#41196) ;
#34452 = AXIS2_PLACEMENT_3D('',#71255,#41198,#41199) ;
#34453 = AXIS2_PLACEMENT_3D('',#71257,#41201,#41202) ;
#34454 = AXIS2_PLACEMENT_3D('',#71261,#41204,#41205) ;
#34455 = AXIS2_PLACEMENT_3D('',#71268,#41209,#41210) ;
#34456 = AXIS2_PLACEMENT_3D('',#71270,#41212,#41213) ;
#34457 = AXIS2_PLACEMENT_3D('',#71273,#41215,#41216) ;
#34458 = AXIS2_PLACEMENT_3D('',#71274,#41217,#41218) ;
#34459 = AXIS2_PLACEMENT_3D('',#71278,#41221,#41222) ;
#34460 = AXIS2_PLACEMENT_3D('',#71281,#41223,#41224) ;
#34461 = AXIS2_PLACEMENT_3D('',#71285,#41226,#41227) ;
#34462 = AXIS2_PLACEMENT_3D('',#71287,#41229,#41230) ;
#34463 = AXIS2_PLACEMENT_3D('',#71290,#41231,#41232) ;
#34464 = AXIS2_PLACEMENT_3D('',#71291,#41233,#41234) ;
#34465 = AXIS2_PLACEMENT_3D('',#71292,#41235,#41236) ;
#34466 = AXIS2_PLACEMENT_3D('',#71293,#41237,#41238) ;
#34467 = AXIS2_PLACEMENT_3D('',#71296,#41239,#41240) ;
#34468 = AXIS2_PLACEMENT_3D('',#71299,#41243,#41244) ;
#34469 = AXIS2_PLACEMENT_3D('',#71302,#41245,#41246) ;
#34470 = AXIS2_PLACEMENT_3D('',#71303,#41247,#41248) ;
#34471 = AXIS2_PLACEMENT_3D('',#71304,#41249,#41250) ;
#34472 = AXIS2_PLACEMENT_3D('',#71305,#41251,#41252) ;
#34473 = AXIS2_PLACEMENT_3D('',#71308,#41253,#41254) ;
#34474 = AXIS2_PLACEMENT_3D('',#71311,#41257,#41258) ;
#34475 = AXIS2_PLACEMENT_3D('',#71313,#41259,#41260) ;
#34476 = AXIS2_PLACEMENT_3D('',#71314,#41261,#41262) ;
#34477 = AXIS2_PLACEMENT_3D('',#71315,#41263,#41264) ;
#34478 = AXIS2_PLACEMENT_3D('',#71316,#41265,#41266) ;
#34479 = AXIS2_PLACEMENT_3D('',#71318,#41267,#41268) ;
#34480 = AXIS2_PLACEMENT_3D('',#71320,#41270,#41271) ;
#34481 = AXIS2_PLACEMENT_3D('',#71321,#41272,#41273) ;
#34482 = AXIS2_PLACEMENT_3D('',#71322,#41274,#41275) ;
#34483 = AXIS2_PLACEMENT_3D('',#71323,#41276,#41277) ;
#34484 = AXIS2_PLACEMENT_3D('',#71327,#41279,#41280) ;
#34485 = AXIS2_PLACEMENT_3D('',#71329,#41282,#41283) ;
#34486 = AXIS2_PLACEMENT_3D('',#71333,#41285,#41286) ;
#34487 = AXIS2_PLACEMENT_3D('',#71340,#41290,#41291) ;
#34488 = AXIS2_PLACEMENT_3D('',#71342,#41293,#41294) ;
#34489 = AXIS2_PLACEMENT_3D('',#71345,#41296,#41297) ;
#34490 = AXIS2_PLACEMENT_3D('',#71346,#41298,#41299) ;
#34491 = AXIS2_PLACEMENT_3D('',#71350,#41302,#41303) ;
#34492 = AXIS2_PLACEMENT_3D('',#71353,#41304,#41305) ;
#34493 = AXIS2_PLACEMENT_3D('',#71357,#41307,#41308) ;
#34494 = AXIS2_PLACEMENT_3D('',#71359,#41310,#41311) ;
#34495 = AXIS2_PLACEMENT_3D('',#71362,#41312,#41313) ;
#34496 = AXIS2_PLACEMENT_3D('',#71363,#41314,#41315) ;
#34497 = AXIS2_PLACEMENT_3D('',#71364,#41316,#41317) ;
#34498 = AXIS2_PLACEMENT_3D('',#71365,#41318,#41319) ;
#34499 = AXIS2_PLACEMENT_3D('',#71368,#41320,#41321) ;
#34500 = AXIS2_PLACEMENT_3D('',#71371,#41324,#41325) ;
#34501 = AXIS2_PLACEMENT_3D('',#71374,#41326,#41327) ;
#34502 = AXIS2_PLACEMENT_3D('',#71375,#41328,#41329) ;
#34503 = AXIS2_PLACEMENT_3D('',#71376,#41330,#41331) ;
#34504 = AXIS2_PLACEMENT_3D('',#71377,#41332,#41333) ;
#34505 = AXIS2_PLACEMENT_3D('',#71380,#41334,#41335) ;
#34506 = AXIS2_PLACEMENT_3D('',#71383,#41338,#41339) ;
#34507 = AXIS2_PLACEMENT_3D('',#71385,#41340,#41341) ;
#34508 = AXIS2_PLACEMENT_3D('',#71386,#41342,#41343) ;
#34509 = AXIS2_PLACEMENT_3D('',#71387,#41344,#41345) ;
#34510 = AXIS2_PLACEMENT_3D('',#71388,#41346,#41347) ;
#34511 = AXIS2_PLACEMENT_3D('',#71390,#41348,#41349) ;
#34512 = AXIS2_PLACEMENT_3D('',#71392,#41351,#41352) ;
#34513 = AXIS2_PLACEMENT_3D('',#71393,#41353,#41354) ;
#34514 = AXIS2_PLACEMENT_3D('',#71394,#41355,#41356) ;
#34515 = AXIS2_PLACEMENT_3D('',#71395,#41357,#41358) ;
#34516 = AXIS2_PLACEMENT_3D('',#71399,#41360,#41361) ;
#34517 = AXIS2_PLACEMENT_3D('',#71401,#41363,#41364) ;
#34518 = AXIS2_PLACEMENT_3D('',#71405,#41366,#41367) ;
#34519 = AXIS2_PLACEMENT_3D('',#71412,#41371,#41372) ;
#34520 = AXIS2_PLACEMENT_3D('',#71414,#41374,#41375) ;
#34521 = AXIS2_PLACEMENT_3D('',#71417,#41377,#41378) ;
#34522 = AXIS2_PLACEMENT_3D('',#71418,#41379,#41380) ;
#34523 = AXIS2_PLACEMENT_3D('',#71422,#41383,#41384) ;
#34524 = AXIS2_PLACEMENT_3D('',#71425,#41385,#41386) ;
#34525 = AXIS2_PLACEMENT_3D('',#71429,#41388,#41389) ;
#34526 = AXIS2_PLACEMENT_3D('',#71431,#41391,#41392) ;
#34527 = AXIS2_PLACEMENT_3D('',#71434,#41393,#41394) ;
#34528 = AXIS2_PLACEMENT_3D('',#71435,#41395,#41396) ;
#34529 = AXIS2_PLACEMENT_3D('',#71436,#41397,#41398) ;
#34530 = AXIS2_PLACEMENT_3D('',#71437,#41399,#41400) ;
#34531 = AXIS2_PLACEMENT_3D('',#71440,#41401,#41402) ;
#34532 = AXIS2_PLACEMENT_3D('',#71443,#41405,#41406) ;
#34533 = AXIS2_PLACEMENT_3D('',#71446,#41407,#41408) ;
#34534 = AXIS2_PLACEMENT_3D('',#71447,#41409,#41410) ;
#34535 = AXIS2_PLACEMENT_3D('',#71448,#41411,#41412) ;
#34536 = AXIS2_PLACEMENT_3D('',#71449,#41413,#41414) ;
#34537 = AXIS2_PLACEMENT_3D('',#71452,#41415,#41416) ;
#34538 = AXIS2_PLACEMENT_3D('',#71455,#41419,#41420) ;
#34539 = AXIS2_PLACEMENT_3D('',#71457,#41421,#41422) ;
#34540 = AXIS2_PLACEMENT_3D('',#71458,#41423,#41424) ;
#34541 = AXIS2_PLACEMENT_3D('',#71459,#41425,#41426) ;
#34542 = AXIS2_PLACEMENT_3D('',#71460,#41427,#41428) ;
#34543 = AXIS2_PLACEMENT_3D('',#71462,#41429,#41430) ;
#34544 = AXIS2_PLACEMENT_3D('',#71464,#41432,#41433) ;
#34545 = AXIS2_PLACEMENT_3D('',#71465,#41434,#41435) ;
#34546 = AXIS2_PLACEMENT_3D('',#71466,#41436,#41437) ;
#34547 = AXIS2_PLACEMENT_3D('',#71467,#41438,#41439) ;
#34548 = AXIS2_PLACEMENT_3D('',#71471,#41441,#41442) ;
#34549 = AXIS2_PLACEMENT_3D('',#71473,#41444,#41445) ;
#34550 = AXIS2_PLACEMENT_3D('',#71477,#41447,#41448) ;
#34551 = AXIS2_PLACEMENT_3D('',#71484,#41452,#41453) ;
#34552 = AXIS2_PLACEMENT_3D('',#71486,#41455,#41456) ;
#34553 = AXIS2_PLACEMENT_3D('',#71489,#41458,#41459) ;
#34554 = AXIS2_PLACEMENT_3D('',#71490,#41460,#41461) ;
#34555 = AXIS2_PLACEMENT_3D('',#71494,#41464,#41465) ;
#34556 = AXIS2_PLACEMENT_3D('',#71497,#41466,#41467) ;
#34557 = AXIS2_PLACEMENT_3D('',#71501,#41469,#41470) ;
#34558 = AXIS2_PLACEMENT_3D('',#71503,#41472,#41473) ;
#34559 = AXIS2_PLACEMENT_3D('',#71506,#41474,#41475) ;
#34560 = AXIS2_PLACEMENT_3D('',#71507,#41476,#41477) ;
#34561 = AXIS2_PLACEMENT_3D('',#71508,#41478,#41479) ;
#34562 = AXIS2_PLACEMENT_3D('',#71509,#41480,#41481) ;
#34563 = AXIS2_PLACEMENT_3D('',#71512,#41482,#41483) ;
#34564 = AXIS2_PLACEMENT_3D('',#71515,#41486,#41487) ;
#34565 = AXIS2_PLACEMENT_3D('',#71518,#41488,#41489) ;
#34566 = AXIS2_PLACEMENT_3D('',#71519,#41490,#41491) ;
#34567 = AXIS2_PLACEMENT_3D('',#71520,#41492,#41493) ;
#34568 = AXIS2_PLACEMENT_3D('',#71521,#41494,#41495) ;
#34569 = AXIS2_PLACEMENT_3D('',#71524,#41496,#41497) ;
#34570 = AXIS2_PLACEMENT_3D('',#71527,#41500,#41501) ;
#34571 = AXIS2_PLACEMENT_3D('',#71529,#41502,#41503) ;
#34572 = AXIS2_PLACEMENT_3D('',#71530,#41504,#41505) ;
#34573 = AXIS2_PLACEMENT_3D('',#71531,#41506,#41507) ;
#34574 = AXIS2_PLACEMENT_3D('',#71532,#41508,#41509) ;
#34575 = AXIS2_PLACEMENT_3D('',#71534,#41510,#41511) ;
#34576 = AXIS2_PLACEMENT_3D('',#71536,#41513,#41514) ;
#34577 = AXIS2_PLACEMENT_3D('',#71537,#41515,#41516) ;
#34578 = AXIS2_PLACEMENT_3D('',#71538,#41517,#41518) ;
#34579 = AXIS2_PLACEMENT_3D('',#71539,#41519,#41520) ;
#34580 = AXIS2_PLACEMENT_3D('',#71543,#41522,#41523) ;
#34581 = AXIS2_PLACEMENT_3D('',#71545,#41525,#41526) ;
#34582 = AXIS2_PLACEMENT_3D('',#71549,#41528,#41529) ;
#34583 = AXIS2_PLACEMENT_3D('',#71556,#41533,#41534) ;
#34584 = AXIS2_PLACEMENT_3D('',#71558,#41536,#41537) ;
#34585 = AXIS2_PLACEMENT_3D('',#71561,#41539,#41540) ;
#34586 = AXIS2_PLACEMENT_3D('',#71562,#41541,#41542) ;
#34587 = AXIS2_PLACEMENT_3D('',#71566,#41545,#41546) ;
#34588 = AXIS2_PLACEMENT_3D('',#71569,#41547,#41548) ;
#34589 = AXIS2_PLACEMENT_3D('',#71573,#41550,#41551) ;
#34590 = AXIS2_PLACEMENT_3D('',#71575,#41553,#41554) ;
#34591 = AXIS2_PLACEMENT_3D('',#71578,#41555,#41556) ;
#34592 = AXIS2_PLACEMENT_3D('',#71579,#41557,#41558) ;
#34593 = AXIS2_PLACEMENT_3D('',#71580,#41559,#41560) ;
#34594 = AXIS2_PLACEMENT_3D('',#71581,#41561,#41562) ;
#34595 = AXIS2_PLACEMENT_3D('',#71584,#41563,#41564) ;
#34596 = AXIS2_PLACEMENT_3D('',#71587,#41567,#41568) ;
#34597 = AXIS2_PLACEMENT_3D('',#71590,#41569,#41570) ;
#34598 = AXIS2_PLACEMENT_3D('',#71591,#41571,#41572) ;
#34599 = AXIS2_PLACEMENT_3D('',#71592,#41573,#41574) ;
#34600 = AXIS2_PLACEMENT_3D('',#71593,#41575,#41576) ;
#34601 = AXIS2_PLACEMENT_3D('',#71596,#41577,#41578) ;
#34602 = AXIS2_PLACEMENT_3D('',#71599,#41581,#41582) ;
#34603 = AXIS2_PLACEMENT_3D('',#71601,#41583,#41584) ;
#34604 = AXIS2_PLACEMENT_3D('',#71602,#41585,#41586) ;
#34605 = AXIS2_PLACEMENT_3D('',#71603,#41587,#41588) ;
#34606 = AXIS2_PLACEMENT_3D('',#71604,#41589,#41590) ;
#34607 = AXIS2_PLACEMENT_3D('',#71606,#41591,#41592) ;
#34608 = AXIS2_PLACEMENT_3D('',#71608,#41594,#41595) ;
#34609 = AXIS2_PLACEMENT_3D('',#71609,#41596,#41597) ;
#34610 = AXIS2_PLACEMENT_3D('',#71610,#41598,#41599) ;
#34611 = AXIS2_PLACEMENT_3D('',#71611,#41600,#41601) ;
#34612 = AXIS2_PLACEMENT_3D('',#71615,#41603,#41604) ;
#34613 = AXIS2_PLACEMENT_3D('',#71617,#41606,#41607) ;
#34614 = AXIS2_PLACEMENT_3D('',#71621,#41609,#41610) ;
#34615 = AXIS2_PLACEMENT_3D('',#71628,#41614,#41615) ;
#34616 = AXIS2_PLACEMENT_3D('',#71630,#41617,#41618) ;
#34617 = AXIS2_PLACEMENT_3D('',#71633,#41620,#41621) ;
#34618 = AXIS2_PLACEMENT_3D('',#71634,#41622,#41623) ;
#34619 = AXIS2_PLACEMENT_3D('',#71638,#41626,#41627) ;
#34620 = AXIS2_PLACEMENT_3D('',#71641,#41628,#41629) ;
#34621 = AXIS2_PLACEMENT_3D('',#71645,#41631,#41632) ;
#34622 = AXIS2_PLACEMENT_3D('',#71647,#41634,#41635) ;
#34623 = AXIS2_PLACEMENT_3D('',#71650,#41636,#41637) ;
#34624 = AXIS2_PLACEMENT_3D('',#71651,#41638,#41639) ;
#34625 = AXIS2_PLACEMENT_3D('',#71652,#41640,#41641) ;
#34626 = AXIS2_PLACEMENT_3D('',#71653,#41642,#41643) ;
#34627 = AXIS2_PLACEMENT_3D('',#71656,#41644,#41645) ;
#34628 = AXIS2_PLACEMENT_3D('',#71659,#41648,#41649) ;
#34629 = AXIS2_PLACEMENT_3D('',#71662,#41650,#41651) ;
#34630 = AXIS2_PLACEMENT_3D('',#71663,#41652,#41653) ;
#34631 = AXIS2_PLACEMENT_3D('',#71664,#41654,#41655) ;
#34632 = AXIS2_PLACEMENT_3D('',#71665,#41656,#41657) ;
#34633 = AXIS2_PLACEMENT_3D('',#71668,#41658,#41659) ;
#34634 = AXIS2_PLACEMENT_3D('',#71671,#41662,#41663) ;
#34635 = AXIS2_PLACEMENT_3D('',#71674,#41664,#41665) ;
#34636 = AXIS2_PLACEMENT_3D('',#71675,#41666,#41667) ;
#34637 = AXIS2_PLACEMENT_3D('',#71676,#41668,#41669) ;
#34638 = AXIS2_PLACEMENT_3D('',#71677,#41670,#41671) ;
#34639 = AXIS2_PLACEMENT_3D('',#71680,#41672,#41673) ;
#34640 = AXIS2_PLACEMENT_3D('',#71683,#41676,#41677) ;
#34641 = AXIS2_PLACEMENT_3D('',#71684,#41678,#41679) ;
#34642 = AXIS2_PLACEMENT_3D('',#71685,#41680,#41681) ;
#34643 = AXIS2_PLACEMENT_3D('',#71686,#41682,#41683) ;
#34644 = AXIS2_PLACEMENT_3D('',#71690,#41685,#41686) ;
#34645 = AXIS2_PLACEMENT_3D('',#71692,#41688,#41689) ;
#34646 = AXIS2_PLACEMENT_3D('',#71696,#41692,#41693) ;
#34647 = AXIS2_PLACEMENT_3D('',#71699,#41695,#41696) ;
#34648 = AXIS2_PLACEMENT_3D('',#71700,#41697,#41698) ;
#34649 = AXIS2_PLACEMENT_3D('',#71704,#41701,#41702) ;
#34650 = AXIS2_PLACEMENT_3D('',#71717,#41708,#41709) ;
#34651 = AXIS2_PLACEMENT_3D('',#71721,#41711,#41712) ;
#34652 = AXIS2_PLACEMENT_3D('',#71725,#41714,#41715) ;
#34653 = AXIS2_PLACEMENT_3D('',#71728,#41717,#41718) ;
#34654 = AXIS2_PLACEMENT_3D('',#71730,#41719,#41720) ;
#34655 = AXIS2_PLACEMENT_3D('',#71731,#41721,#41722) ;
#34656 = AXIS2_PLACEMENT_3D('',#71733,#41723,#41724) ;
#34657 = AXIS2_PLACEMENT_3D('',#71736,#41726,#41727) ;
#34658 = AXIS2_PLACEMENT_3D('',#71737,#41728,#41729) ;
#34659 = AXIS2_PLACEMENT_3D('',#71739,#41730,#41731) ;
#34660 = AXIS2_PLACEMENT_3D('',#71740,#41732,#41733) ;
#34661 = AXIS2_PLACEMENT_3D('',#71741,#41734,#41735) ;
#34662 = AXIS2_PLACEMENT_3D('',#71743,#41736,#41737) ;
#34663 = AXIS2_PLACEMENT_3D('',#71745,#41739,#41740) ;
#34664 = AXIS2_PLACEMENT_3D('',#71747,#41741,#41742) ;
#34665 = AXIS2_PLACEMENT_3D('',#71748,#41743,#41744) ;
#34666 = AXIS2_PLACEMENT_3D('',#71749,#41745,#41746) ;
#34667 = AXIS2_PLACEMENT_3D('',#71751,#41747,#41748) ;
#34668 = AXIS2_PLACEMENT_3D('',#71753,#41750,#41751) ;
#34669 = AXIS2_PLACEMENT_3D('',#71754,#41752,#41753) ;
#34670 = AXIS2_PLACEMENT_3D('',#71755,#41754,#41755) ;
#34671 = AXIS2_PLACEMENT_3D('',#71756,#41756,#41757) ;
#34672 = AXIS2_PLACEMENT_3D('',#71757,#41758,#41759) ;
#34673 = AXIS2_PLACEMENT_3D('',#71758,#41760,#41761) ;
#34674 = AXIS2_PLACEMENT_3D('',#71759,#41762,#41763) ;
#34675 = AXIS2_PLACEMENT_3D('',#71760,#41764,#41765) ;
#34676 = AXIS2_PLACEMENT_3D('',#71764,#41767,#41768) ;
#34677 = AXIS2_PLACEMENT_3D('',#71766,#41770,#41771) ;
#34678 = AXIS2_PLACEMENT_3D('',#71772,#41774,#41775) ;
#34679 = AXIS2_PLACEMENT_3D('',#71777,#41778,#41779) ;
#34680 = AXIS2_PLACEMENT_3D('',#71779,#41781,#41782) ;
#34681 = AXIS2_PLACEMENT_3D('',#71782,#41784,#41785) ;
#34682 = AXIS2_PLACEMENT_3D('',#71783,#41786,#41787) ;
#34683 = AXIS2_PLACEMENT_3D('',#71787,#41790,#41791) ;
#34684 = AXIS2_PLACEMENT_3D('',#71791,#41794,#41795) ;
#34685 = AXIS2_PLACEMENT_3D('',#71792,#41796,#41797) ;
#34686 = AXIS2_PLACEMENT_3D('',#71793,#41798,#41799) ;
#34687 = AXIS2_PLACEMENT_3D('',#71794,#41800,#41801) ;
#34688 = AXIS2_PLACEMENT_3D('',#71795,#41802,#41803) ;
#34689 = AXIS2_PLACEMENT_3D('',#71799,#41806,#41807) ;
#34690 = AXIS2_PLACEMENT_3D('',#71801,#41808,#41809) ;
#34691 = AXIS2_PLACEMENT_3D('',#71803,#41811,#41812) ;
#34692 = AXIS2_PLACEMENT_3D('',#71806,#41814,#41815) ;
#34693 = AXIS2_PLACEMENT_3D('',#71807,#41816,#41817) ;
#34694 = AXIS2_PLACEMENT_3D('',#71809,#41819,#41820) ;
#34695 = AXIS2_PLACEMENT_3D('',#71811,#41821,#41822) ;
#34696 = AXIS2_PLACEMENT_3D('',#71812,#41823,#41824) ;
#34697 = AXIS2_PLACEMENT_3D('',#71813,#41825,#41826) ;
#34698 = AXIS2_PLACEMENT_3D('',#71814,#41827,#41828) ;
#34699 = AXIS2_PLACEMENT_3D('',#71816,#41829,#41830) ;
#34700 = AXIS2_PLACEMENT_3D('',#71818,#41831,#41832) ;
#34701 = AXIS2_PLACEMENT_3D('',#71820,#41834,#41835) ;
#34702 = AXIS2_PLACEMENT_3D('',#71822,#41836,#41837) ;
#34703 = AXIS2_PLACEMENT_3D('',#71823,#41838,#41839) ;
#34704 = AXIS2_PLACEMENT_3D('',#71824,#41840,#41841) ;
#34705 = AXIS2_PLACEMENT_3D('',#71826,#41842,#41843) ;
#34706 = AXIS2_PLACEMENT_3D('',#71828,#41845,#41846) ;
#34707 = AXIS2_PLACEMENT_3D('',#71830,#41847,#41848) ;
#34708 = AXIS2_PLACEMENT_3D('',#71831,#41849,#41850) ;
#34709 = AXIS2_PLACEMENT_3D('',#71832,#41851,#41852) ;
#34710 = AXIS2_PLACEMENT_3D('',#71835,#41853,#41854) ;
#34711 = AXIS2_PLACEMENT_3D('',#71836,#41855,#41856) ;
#34712 = AXIS2_PLACEMENT_3D('',#71837,#41857,#41858) ;
#34713 = AXIS2_PLACEMENT_3D('',#71838,#41859,#41860) ;
#34714 = AXIS2_PLACEMENT_3D('',#71840,#41862,#41863) ;
#34715 = AXIS2_PLACEMENT_3D('',#71841,#41864,#41865) ;
#34716 = AXIS2_PLACEMENT_3D('',#71843,#41867,#41868) ;
#34717 = AXIS2_PLACEMENT_3D('',#71845,#41869,#41870) ;
#34718 = AXIS2_PLACEMENT_3D('',#71846,#41871,#41872) ;
#34719 = AXIS2_PLACEMENT_3D('',#71847,#41873,#41874) ;
#34720 = AXIS2_PLACEMENT_3D('',#71848,#41875,#41876) ;
#34721 = AXIS2_PLACEMENT_3D('',#71850,#41878,#41879) ;
#34722 = AXIS2_PLACEMENT_3D('',#71853,#41882,#41883) ;
#34723 = AXIS2_PLACEMENT_3D('',#71855,#41884,#41885) ;
#34724 = AXIS2_PLACEMENT_3D('',#71857,#41887,#41888) ;
#34725 = AXIS2_PLACEMENT_3D('',#71859,#41890,#41891) ;
#34726 = AXIS2_PLACEMENT_3D('',#71860,#41892,#41893) ;
#34727 = AXIS2_PLACEMENT_3D('',#71861,#41894,#41895) ;
#34728 = AXIS2_PLACEMENT_3D('',#71862,#41896,#41897) ;
#34729 = AXIS2_PLACEMENT_3D('',#71864,#41899,#41900) ;
#34730 = AXIS2_PLACEMENT_3D('',#71865,#41901,#41902) ;
#34731 = AXIS2_PLACEMENT_3D('',#71866,#41903,#41904) ;
#34732 = AXIS2_PLACEMENT_3D('',#71867,#41905,#41906) ;
#34733 = AXIS2_PLACEMENT_3D('',#71868,#41907,#41908) ;
#34734 = AXIS2_PLACEMENT_3D('',#71869,#41909,#41910) ;
#34735 = AXIS2_PLACEMENT_3D('',#71870,#41911,#41912) ;
#34736 = AXIS2_PLACEMENT_3D('',#71879,#41917,#41918) ;
#34737 = AXIS2_PLACEMENT_3D('',#71880,#41919,#41920) ;
#34738 = AXIS2_PLACEMENT_3D('',#71881,#41921,#41922) ;
#34739 = AXIS2_PLACEMENT_3D('',#71882,#41923,#41924) ;
#34740 = AXIS2_PLACEMENT_3D('',#71883,#41925,#41926) ;
#34741 = AXIS2_PLACEMENT_3D('',#71884,#41927,#41928) ;
#34742 = AXIS2_PLACEMENT_3D('',#71885,#41929,#41930) ;
#34743 = AXIS2_PLACEMENT_3D('',#71886,#41931,#41932) ;
#34744 = AXIS2_PLACEMENT_3D('',#71887,#41933,#41934) ;
#34745 = AXIS2_PLACEMENT_3D('',#71888,#41935,#41936) ;
#34746 = AXIS2_PLACEMENT_3D('',#71889,#41937,#41938) ;
#34747 = AXIS2_PLACEMENT_3D('',#71890,#41939,#41940) ;
#34748 = AXIS2_PLACEMENT_3D('',#71891,#41941,#41942) ;
#34749 = AXIS2_PLACEMENT_3D('',#71892,#41943,#41944) ;
#34750 = AXIS2_PLACEMENT_3D('',#71893,#41945,#41946) ;
#34751 = AXIS2_PLACEMENT_3D('',#71894,#41947,#41948) ;
#34752 = AXIS2_PLACEMENT_3D('',#71895,#41949,#41950) ;
#34753 = AXIS2_PLACEMENT_3D('',#71896,#41951,#41952) ;
#34754 = AXIS2_PLACEMENT_3D('',#71897,#41953,#41954) ;
#34755 = AXIS2_PLACEMENT_3D('',#71900,#41955,#41956) ;
#34756 = AXIS2_PLACEMENT_3D('',#71903,#41958,#41959) ;
#34757 = AXIS2_PLACEMENT_3D('',#71905,#41961,#41962) ;
#34758 = AXIS2_PLACEMENT_3D('',#71907,#41963,#41964) ;
#34759 = AXIS2_PLACEMENT_3D('',#71908,#41965,#41966) ;
#34760 = AXIS2_PLACEMENT_3D('',#71909,#41967,#41968) ;
#34761 = AXIS2_PLACEMENT_3D('',#71911,#41969,#41970) ;
#34762 = AXIS2_PLACEMENT_3D('',#71913,#41972,#41973) ;
#34763 = AXIS2_PLACEMENT_3D('',#71915,#41974,#41975) ;
#34764 = AXIS2_PLACEMENT_3D('',#71916,#41976,#41977) ;
#34765 = AXIS2_PLACEMENT_3D('',#71917,#41978,#41979) ;
#34766 = AXIS2_PLACEMENT_3D('',#71920,#41980,#41981) ;
#34767 = AXIS2_PLACEMENT_3D('',#71921,#41982,#41983) ;
#34768 = AXIS2_PLACEMENT_3D('',#71922,#41984,#41985) ;
#34769 = AXIS2_PLACEMENT_3D('',#71923,#41986,#41987) ;
#34770 = AXIS2_PLACEMENT_3D('',#71925,#41989,#41990) ;
#34771 = AXIS2_PLACEMENT_3D('',#71926,#41991,#41992) ;
#34772 = AXIS2_PLACEMENT_3D('',#71928,#41994,#41995) ;
#34773 = AXIS2_PLACEMENT_3D('',#71930,#41996,#41997) ;
#34774 = AXIS2_PLACEMENT_3D('',#71931,#41998,#41999) ;
#34775 = AXIS2_PLACEMENT_3D('',#71932,#42000,#42001) ;
#34776 = AXIS2_PLACEMENT_3D('',#71933,#42002,#42003) ;
#34777 = AXIS2_PLACEMENT_3D('',#71935,#42005,#42006) ;
#34778 = AXIS2_PLACEMENT_3D('',#71938,#42009,#42010) ;
#34779 = AXIS2_PLACEMENT_3D('',#71940,#42011,#42012) ;
#34780 = AXIS2_PLACEMENT_3D('',#71942,#42014,#42015) ;
#34781 = AXIS2_PLACEMENT_3D('',#71944,#42017,#42018) ;
#34782 = AXIS2_PLACEMENT_3D('',#71945,#42019,#42020) ;
#34783 = AXIS2_PLACEMENT_3D('',#71946,#42021,#42022) ;
#34784 = AXIS2_PLACEMENT_3D('',#71947,#42023,#42024) ;
#34785 = AXIS2_PLACEMENT_3D('',#71948,#42025,#42026) ;
#34786 = AXIS2_PLACEMENT_3D('',#71950,#42028,#42029) ;
#34787 = AXIS2_PLACEMENT_3D('',#71951,#42030,#42031) ;
#34788 = AXIS2_PLACEMENT_3D('',#71952,#42032,#42033) ;
#34789 = AXIS2_PLACEMENT_3D('',#71953,#42034,#42035) ;
#34790 = AXIS2_PLACEMENT_3D('',#71954,#42036,#42037) ;
#34791 = AXIS2_PLACEMENT_3D('',#71955,#42038,#42039) ;
#34792 = AXIS2_PLACEMENT_3D('',#71956,#42040,#42041) ;
#34793 = AXIS2_PLACEMENT_3D('',#71957,#42042,#42043) ;
#34794 = AXIS2_PLACEMENT_3D('',#71966,#42048,#42049) ;
#34795 = AXIS2_PLACEMENT_3D('',#71968,#42050,#42051) ;
#34796 = AXIS2_PLACEMENT_3D('',#71970,#42052,#42053) ;
#34797 = AXIS2_PLACEMENT_3D('',#71971,#42054,#42055) ;
#34798 = AXIS2_PLACEMENT_3D('',#71972,#42056,#42057) ;
#34799 = AXIS2_PLACEMENT_3D('',#71974,#42058,#42059) ;
#34800 = AXIS2_PLACEMENT_3D('',#71975,#42060,#42061) ;
#34801 = AXIS2_PLACEMENT_3D('',#71976,#42062,#42063) ;
#34802 = AXIS2_PLACEMENT_3D('',#71977,#42064,#42065) ;
#34803 = AXIS2_PLACEMENT_3D('',#71979,#42067,#42068) ;
#34804 = AXIS2_PLACEMENT_3D('',#71980,#42069,#42070) ;
#34805 = AXIS2_PLACEMENT_3D('',#71981,#42071,#42072) ;
#34806 = AXIS2_PLACEMENT_3D('',#71983,#42074,#42075) ;
#34807 = AXIS2_PLACEMENT_3D('',#71984,#42076,#42077) ;
#34808 = AXIS2_PLACEMENT_3D('',#71985,#42078,#42079) ;
#34809 = AXIS2_PLACEMENT_3D('',#71986,#42080,#42081) ;
#34810 = AXIS2_PLACEMENT_3D('',#71987,#42082,#42083) ;
#34811 = AXIS2_PLACEMENT_3D('',#71988,#42084,#42085) ;
#34812 = AXIS2_PLACEMENT_3D('',#71989,#42086,#42087) ;
#34813 = AXIS2_PLACEMENT_3D('',#71990,#42088,#42089) ;
#34814 = AXIS2_PLACEMENT_3D('',#71991,#42090,#42091) ;
#34815 = AXIS2_PLACEMENT_3D('',#71994,#42092,#42093) ;
#34816 = AXIS2_PLACEMENT_3D('',#71997,#42095,#42096) ;
#34817 = AXIS2_PLACEMENT_3D('',#71999,#42098,#42099) ;
#34818 = AXIS2_PLACEMENT_3D('',#72001,#42100,#42101) ;
#34819 = AXIS2_PLACEMENT_3D('',#72002,#42102,#42103) ;
#34820 = AXIS2_PLACEMENT_3D('',#72003,#42104,#42105) ;
#34821 = AXIS2_PLACEMENT_3D('',#72005,#42106,#42107) ;
#34822 = AXIS2_PLACEMENT_3D('',#72007,#42109,#42110) ;
#34823 = AXIS2_PLACEMENT_3D('',#72009,#42111,#42112) ;
#34824 = AXIS2_PLACEMENT_3D('',#72010,#42113,#42114) ;
#34825 = AXIS2_PLACEMENT_3D('',#72011,#42115,#42116) ;
#34826 = AXIS2_PLACEMENT_3D('',#72014,#42117,#42118) ;
#34827 = AXIS2_PLACEMENT_3D('',#72015,#42119,#42120) ;
#34828 = AXIS2_PLACEMENT_3D('',#72016,#42121,#42122) ;
#34829 = AXIS2_PLACEMENT_3D('',#72017,#42123,#42124) ;
#34830 = AXIS2_PLACEMENT_3D('',#72019,#42126,#42127) ;
#34831 = AXIS2_PLACEMENT_3D('',#72020,#42128,#42129) ;
#34832 = AXIS2_PLACEMENT_3D('',#72022,#42131,#42132) ;
#34833 = AXIS2_PLACEMENT_3D('',#72024,#42133,#42134) ;
#34834 = AXIS2_PLACEMENT_3D('',#72025,#42135,#42136) ;
#34835 = AXIS2_PLACEMENT_3D('',#72026,#42137,#42138) ;
#34836 = AXIS2_PLACEMENT_3D('',#72027,#42139,#42140) ;
#34837 = AXIS2_PLACEMENT_3D('',#72029,#42142,#42143) ;
#34838 = AXIS2_PLACEMENT_3D('',#72032,#42146,#42147) ;
#34839 = AXIS2_PLACEMENT_3D('',#72034,#42148,#42149) ;
#34840 = AXIS2_PLACEMENT_3D('',#72036,#42151,#42152) ;
#34841 = AXIS2_PLACEMENT_3D('',#72038,#42154,#42155) ;
#34842 = AXIS2_PLACEMENT_3D('',#72039,#42156,#42157) ;
#34843 = AXIS2_PLACEMENT_3D('',#72040,#42158,#42159) ;
#34844 = AXIS2_PLACEMENT_3D('',#72041,#42160,#42161) ;
#34845 = AXIS2_PLACEMENT_3D('',#72042,#42162,#42163) ;
#34846 = AXIS2_PLACEMENT_3D('',#72044,#42165,#42166) ;
#34847 = AXIS2_PLACEMENT_3D('',#72045,#42167,#42168) ;
#34848 = AXIS2_PLACEMENT_3D('',#72046,#42169,#42170) ;
#34849 = AXIS2_PLACEMENT_3D('',#72047,#42171,#42172) ;
#34850 = AXIS2_PLACEMENT_3D('',#72048,#42173,#42174) ;
#34851 = AXIS2_PLACEMENT_3D('',#72049,#42175,#42176) ;
#34852 = AXIS2_PLACEMENT_3D('',#72050,#42177,#42178) ;
#34853 = AXIS2_PLACEMENT_3D('',#72051,#42179,#42180) ;
#34854 = AXIS2_PLACEMENT_3D('',#72060,#42185,#42186) ;
#34855 = AXIS2_PLACEMENT_3D('',#72062,#42187,#42188) ;
#34856 = AXIS2_PLACEMENT_3D('',#72064,#42189,#42190) ;
#34857 = AXIS2_PLACEMENT_3D('',#72065,#42191,#42192) ;
#34858 = AXIS2_PLACEMENT_3D('',#72066,#42193,#42194) ;
#34859 = AXIS2_PLACEMENT_3D('',#72068,#42195,#42196) ;
#34860 = AXIS2_PLACEMENT_3D('',#72069,#42197,#42198) ;
#34861 = AXIS2_PLACEMENT_3D('',#72070,#42199,#42200) ;
#34862 = AXIS2_PLACEMENT_3D('',#72071,#42201,#42202) ;
#34863 = AXIS2_PLACEMENT_3D('',#72073,#42204,#42205) ;
#34864 = AXIS2_PLACEMENT_3D('',#72074,#42206,#42207) ;
#34865 = AXIS2_PLACEMENT_3D('',#72075,#42208,#42209) ;
#34866 = AXIS2_PLACEMENT_3D('',#72077,#42211,#42212) ;
#34867 = AXIS2_PLACEMENT_3D('',#72078,#42213,#42214) ;
#34868 = AXIS2_PLACEMENT_3D('',#72079,#42215,#42216) ;
#34869 = AXIS2_PLACEMENT_3D('',#72080,#42217,#42218) ;
#34870 = AXIS2_PLACEMENT_3D('',#72081,#42219,#42220) ;
#34871 = AXIS2_PLACEMENT_3D('',#72082,#42221,#42222) ;
#34872 = AXIS2_PLACEMENT_3D('',#72083,#42223,#42224) ;
#34873 = AXIS2_PLACEMENT_3D('',#72084,#42225,#42226) ;
#34874 = AXIS2_PLACEMENT_3D('',#72085,#42227,#42228) ;
#34875 = AXIS2_PLACEMENT_3D('',#72088,#42229,#42230) ;
#34876 = AXIS2_PLACEMENT_3D('',#72091,#42232,#42233) ;
#34877 = AXIS2_PLACEMENT_3D('',#72093,#42235,#42236) ;
#34878 = AXIS2_PLACEMENT_3D('',#72095,#42237,#42238) ;
#34879 = AXIS2_PLACEMENT_3D('',#72096,#42239,#42240) ;
#34880 = AXIS2_PLACEMENT_3D('',#72097,#42241,#42242) ;
#34881 = AXIS2_PLACEMENT_3D('',#72099,#42243,#42244) ;
#34882 = AXIS2_PLACEMENT_3D('',#72101,#42246,#42247) ;
#34883 = AXIS2_PLACEMENT_3D('',#72103,#42248,#42249) ;
#34884 = AXIS2_PLACEMENT_3D('',#72104,#42250,#42251) ;
#34885 = AXIS2_PLACEMENT_3D('',#72105,#42252,#42253) ;
#34886 = AXIS2_PLACEMENT_3D('',#72108,#42254,#42255) ;
#34887 = AXIS2_PLACEMENT_3D('',#72109,#42256,#42257) ;
#34888 = AXIS2_PLACEMENT_3D('',#72110,#42258,#42259) ;
#34889 = AXIS2_PLACEMENT_3D('',#72111,#42260,#42261) ;
#34890 = AXIS2_PLACEMENT_3D('',#72113,#42263,#42264) ;
#34891 = AXIS2_PLACEMENT_3D('',#72114,#42265,#42266) ;
#34892 = AXIS2_PLACEMENT_3D('',#72116,#42268,#42269) ;
#34893 = AXIS2_PLACEMENT_3D('',#72118,#42270,#42271) ;
#34894 = AXIS2_PLACEMENT_3D('',#72119,#42272,#42273) ;
#34895 = AXIS2_PLACEMENT_3D('',#72120,#42274,#42275) ;
#34896 = AXIS2_PLACEMENT_3D('',#72121,#42276,#42277) ;
#34897 = AXIS2_PLACEMENT_3D('',#72123,#42279,#42280) ;
#34898 = AXIS2_PLACEMENT_3D('',#72126,#42283,#42284) ;
#34899 = AXIS2_PLACEMENT_3D('',#72128,#42285,#42286) ;
#34900 = AXIS2_PLACEMENT_3D('',#72130,#42288,#42289) ;
#34901 = AXIS2_PLACEMENT_3D('',#72132,#42291,#42292) ;
#34902 = AXIS2_PLACEMENT_3D('',#72133,#42293,#42294) ;
#34903 = AXIS2_PLACEMENT_3D('',#72134,#42295,#42296) ;
#34904 = AXIS2_PLACEMENT_3D('',#72135,#42297,#42298) ;
#34905 = AXIS2_PLACEMENT_3D('',#72136,#42299,#42300) ;
#34906 = AXIS2_PLACEMENT_3D('',#72138,#42302,#42303) ;
#34907 = AXIS2_PLACEMENT_3D('',#72139,#42304,#42305) ;
#34908 = AXIS2_PLACEMENT_3D('',#72140,#42306,#42307) ;
#34909 = AXIS2_PLACEMENT_3D('',#72141,#42308,#42309) ;
#34910 = AXIS2_PLACEMENT_3D('',#72142,#42310,#42311) ;
#34911 = AXIS2_PLACEMENT_3D('',#72143,#42312,#42313) ;
#34912 = AXIS2_PLACEMENT_3D('',#72144,#42314,#42315) ;
#34913 = AXIS2_PLACEMENT_3D('',#72145,#42316,#42317) ;
#34914 = AXIS2_PLACEMENT_3D('',#72154,#42322,#42323) ;
#34915 = AXIS2_PLACEMENT_3D('',#72156,#42324,#42325) ;
#34916 = AXIS2_PLACEMENT_3D('',#72158,#42326,#42327) ;
#34917 = AXIS2_PLACEMENT_3D('',#72159,#42328,#42329) ;
#34918 = AXIS2_PLACEMENT_3D('',#72160,#42330,#42331) ;
#34919 = AXIS2_PLACEMENT_3D('',#72162,#42332,#42333) ;
#34920 = AXIS2_PLACEMENT_3D('',#72163,#42334,#42335) ;
#34921 = AXIS2_PLACEMENT_3D('',#72164,#42336,#42337) ;
#34922 = AXIS2_PLACEMENT_3D('',#72165,#42338,#42339) ;
#34923 = AXIS2_PLACEMENT_3D('',#72167,#42341,#42342) ;
#34924 = AXIS2_PLACEMENT_3D('',#72168,#42343,#42344) ;
#34925 = AXIS2_PLACEMENT_3D('',#72169,#42345,#42346) ;
#34926 = AXIS2_PLACEMENT_3D('',#72171,#42348,#42349) ;
#34927 = AXIS2_PLACEMENT_3D('',#72172,#42350,#42351) ;
#34928 = AXIS2_PLACEMENT_3D('',#72173,#42352,#42353) ;
#34929 = AXIS2_PLACEMENT_3D('',#72174,#42354,#42355) ;
#34930 = AXIS2_PLACEMENT_3D('',#72175,#42356,#42357) ;
#34931 = AXIS2_PLACEMENT_3D('',#72176,#42358,#42359) ;
#34932 = AXIS2_PLACEMENT_3D('',#72177,#42360,#42361) ;
#34933 = AXIS2_PLACEMENT_3D('',#72178,#42362,#42363) ;
#34934 = AXIS2_PLACEMENT_3D('',#72179,#42364,#42365) ;
#34935 = AXIS2_PLACEMENT_3D('',#72182,#42366,#42367) ;
#34936 = AXIS2_PLACEMENT_3D('',#72185,#42369,#42370) ;
#34937 = AXIS2_PLACEMENT_3D('',#72187,#42372,#42373) ;
#34938 = AXIS2_PLACEMENT_3D('',#72189,#42374,#42375) ;
#34939 = AXIS2_PLACEMENT_3D('',#72190,#42376,#42377) ;
#34940 = AXIS2_PLACEMENT_3D('',#72191,#42378,#42379) ;
#34941 = AXIS2_PLACEMENT_3D('',#72193,#42380,#42381) ;
#34942 = AXIS2_PLACEMENT_3D('',#72195,#42383,#42384) ;
#34943 = AXIS2_PLACEMENT_3D('',#72197,#42385,#42386) ;
#34944 = AXIS2_PLACEMENT_3D('',#72198,#42387,#42388) ;
#34945 = AXIS2_PLACEMENT_3D('',#72199,#42389,#42390) ;
#34946 = AXIS2_PLACEMENT_3D('',#72202,#42391,#42392) ;
#34947 = AXIS2_PLACEMENT_3D('',#72203,#42393,#42394) ;
#34948 = AXIS2_PLACEMENT_3D('',#72204,#42395,#42396) ;
#34949 = AXIS2_PLACEMENT_3D('',#72205,#42397,#42398) ;
#34950 = AXIS2_PLACEMENT_3D('',#72207,#42400,#42401) ;
#34951 = AXIS2_PLACEMENT_3D('',#72208,#42402,#42403) ;
#34952 = AXIS2_PLACEMENT_3D('',#72210,#42405,#42406) ;
#34953 = AXIS2_PLACEMENT_3D('',#72212,#42407,#42408) ;
#34954 = AXIS2_PLACEMENT_3D('',#72213,#42409,#42410) ;
#34955 = AXIS2_PLACEMENT_3D('',#72214,#42411,#42412) ;
#34956 = AXIS2_PLACEMENT_3D('',#72215,#42413,#42414) ;
#34957 = AXIS2_PLACEMENT_3D('',#72217,#42416,#42417) ;
#34958 = AXIS2_PLACEMENT_3D('',#72220,#42420,#42421) ;
#34959 = AXIS2_PLACEMENT_3D('',#72222,#42422,#42423) ;
#34960 = AXIS2_PLACEMENT_3D('',#72224,#42425,#42426) ;
#34961 = AXIS2_PLACEMENT_3D('',#72226,#42428,#42429) ;
#34962 = AXIS2_PLACEMENT_3D('',#72227,#42430,#42431) ;
#34963 = AXIS2_PLACEMENT_3D('',#72228,#42432,#42433) ;
#34964 = AXIS2_PLACEMENT_3D('',#72229,#42434,#42435) ;
#34965 = AXIS2_PLACEMENT_3D('',#72230,#42436,#42437) ;
#34966 = AXIS2_PLACEMENT_3D('',#72232,#42439,#42440) ;
#34967 = AXIS2_PLACEMENT_3D('',#72233,#42441,#42442) ;
#34968 = AXIS2_PLACEMENT_3D('',#72234,#42443,#42444) ;
#34969 = AXIS2_PLACEMENT_3D('',#72235,#42445,#42446) ;
#34970 = AXIS2_PLACEMENT_3D('',#72236,#42447,#42448) ;
#34971 = AXIS2_PLACEMENT_3D('',#72237,#42449,#42450) ;
#34972 = AXIS2_PLACEMENT_3D('',#72238,#42451,#42452) ;
#34973 = AXIS2_PLACEMENT_3D('',#72239,#42453,#42454) ;
#34974 = AXIS2_PLACEMENT_3D('',#72248,#42459,#42460) ;
#34975 = AXIS2_PLACEMENT_3D('',#72250,#42461,#42462) ;
#34976 = AXIS2_PLACEMENT_3D('',#72252,#42463,#42464) ;
#34977 = AXIS2_PLACEMENT_3D('',#72253,#42465,#42466) ;
#34978 = AXIS2_PLACEMENT_3D('',#72254,#42467,#42468) ;
#34979 = AXIS2_PLACEMENT_3D('',#72256,#42469,#42470) ;
#34980 = AXIS2_PLACEMENT_3D('',#72257,#42471,#42472) ;
#34981 = AXIS2_PLACEMENT_3D('',#72258,#42473,#42474) ;
#34982 = AXIS2_PLACEMENT_3D('',#72259,#42475,#42476) ;
#34983 = AXIS2_PLACEMENT_3D('',#72261,#42478,#42479) ;
#34984 = AXIS2_PLACEMENT_3D('',#72262,#42480,#42481) ;
#34985 = AXIS2_PLACEMENT_3D('',#72263,#42482,#42483) ;
#34986 = AXIS2_PLACEMENT_3D('',#72265,#42485,#42486) ;
#34987 = AXIS2_PLACEMENT_3D('',#72266,#42487,#42488) ;
#34988 = AXIS2_PLACEMENT_3D('',#72267,#42489,#42490) ;
#34989 = AXIS2_PLACEMENT_3D('',#72268,#42491,#42492) ;
#34990 = AXIS2_PLACEMENT_3D('',#72269,#42493,#42494) ;
#34991 = AXIS2_PLACEMENT_3D('',#72270,#42495,#42496) ;
#34992 = AXIS2_PLACEMENT_3D('',#72271,#42497,#42498) ;
#34993 = AXIS2_PLACEMENT_3D('',#72272,#42499,#42500) ;
#34994 = AXIS2_PLACEMENT_3D('',#72273,#42501,#42502) ;
#34995 = AXIS2_PLACEMENT_3D('',#72276,#42503,#42504) ;
#34996 = AXIS2_PLACEMENT_3D('',#72279,#42506,#42507) ;
#34997 = AXIS2_PLACEMENT_3D('',#72281,#42509,#42510) ;
#34998 = AXIS2_PLACEMENT_3D('',#72283,#42511,#42512) ;
#34999 = AXIS2_PLACEMENT_3D('',#72284,#42513,#42514) ;
#35000 = AXIS2_PLACEMENT_3D('',#72285,#42515,#42516) ;
#35001 = AXIS2_PLACEMENT_3D('',#72287,#42517,#42518) ;
#35002 = AXIS2_PLACEMENT_3D('',#72289,#42520,#42521) ;
#35003 = AXIS2_PLACEMENT_3D('',#72291,#42522,#42523) ;
#35004 = AXIS2_PLACEMENT_3D('',#72292,#42524,#42525) ;
#35005 = AXIS2_PLACEMENT_3D('',#72293,#42526,#42527) ;
#35006 = AXIS2_PLACEMENT_3D('',#72296,#42528,#42529) ;
#35007 = AXIS2_PLACEMENT_3D('',#72297,#42530,#42531) ;
#35008 = AXIS2_PLACEMENT_3D('',#72298,#42532,#42533) ;
#35009 = AXIS2_PLACEMENT_3D('',#72299,#42534,#42535) ;
#35010 = AXIS2_PLACEMENT_3D('',#72301,#42537,#42538) ;
#35011 = AXIS2_PLACEMENT_3D('',#72302,#42539,#42540) ;
#35012 = AXIS2_PLACEMENT_3D('',#72304,#42542,#42543) ;
#35013 = AXIS2_PLACEMENT_3D('',#72306,#42544,#42545) ;
#35014 = AXIS2_PLACEMENT_3D('',#72307,#42546,#42547) ;
#35015 = AXIS2_PLACEMENT_3D('',#72308,#42548,#42549) ;
#35016 = AXIS2_PLACEMENT_3D('',#72309,#42550,#42551) ;
#35017 = AXIS2_PLACEMENT_3D('',#72311,#42553,#42554) ;
#35018 = AXIS2_PLACEMENT_3D('',#72314,#42557,#42558) ;
#35019 = AXIS2_PLACEMENT_3D('',#72316,#42559,#42560) ;
#35020 = AXIS2_PLACEMENT_3D('',#72318,#42562,#42563) ;
#35021 = AXIS2_PLACEMENT_3D('',#72320,#42565,#42566) ;
#35022 = AXIS2_PLACEMENT_3D('',#72321,#42567,#42568) ;
#35023 = AXIS2_PLACEMENT_3D('',#72322,#42569,#42570) ;
#35024 = AXIS2_PLACEMENT_3D('',#72323,#42571,#42572) ;
#35025 = AXIS2_PLACEMENT_3D('',#72324,#42573,#42574) ;
#35026 = AXIS2_PLACEMENT_3D('',#72326,#42576,#42577) ;
#35027 = AXIS2_PLACEMENT_3D('',#72327,#42578,#42579) ;
#35028 = AXIS2_PLACEMENT_3D('',#72328,#42580,#42581) ;
#35029 = AXIS2_PLACEMENT_3D('',#72329,#42582,#42583) ;
#35030 = AXIS2_PLACEMENT_3D('',#72330,#42584,#42585) ;
#35031 = AXIS2_PLACEMENT_3D('',#72331,#42586,#42587) ;
#35032 = AXIS2_PLACEMENT_3D('',#72332,#42588,#42589) ;
#35033 = AXIS2_PLACEMENT_3D('',#72333,#42590,#42591) ;
#35034 = AXIS2_PLACEMENT_3D('',#72342,#42596,#42597) ;
#35035 = AXIS2_PLACEMENT_3D('',#72344,#42598,#42599) ;
#35036 = AXIS2_PLACEMENT_3D('',#72346,#42600,#42601) ;
#35037 = AXIS2_PLACEMENT_3D('',#72347,#42602,#42603) ;
#35038 = AXIS2_PLACEMENT_3D('',#72348,#42604,#42605) ;
#35039 = AXIS2_PLACEMENT_3D('',#72350,#42606,#42607) ;
#35040 = AXIS2_PLACEMENT_3D('',#72351,#42608,#42609) ;
#35041 = AXIS2_PLACEMENT_3D('',#72352,#42610,#42611) ;
#35042 = AXIS2_PLACEMENT_3D('',#72353,#42612,#42613) ;
#35043 = AXIS2_PLACEMENT_3D('',#72355,#42615,#42616) ;
#35044 = AXIS2_PLACEMENT_3D('',#72356,#42617,#42618) ;
#35045 = AXIS2_PLACEMENT_3D('',#72357,#42619,#42620) ;
#35046 = AXIS2_PLACEMENT_3D('',#72359,#42622,#42623) ;
#35047 = AXIS2_PLACEMENT_3D('',#72360,#42624,#42625) ;
#35048 = AXIS2_PLACEMENT_3D('',#72361,#42626,#42627) ;
#35049 = AXIS2_PLACEMENT_3D('',#72362,#42628,#42629) ;
#35050 = AXIS2_PLACEMENT_3D('',#72363,#42630,#42631) ;
#35051 = AXIS2_PLACEMENT_3D('',#72364,#42632,#42633) ;
#35052 = AXIS2_PLACEMENT_3D('',#72365,#42634,#42635) ;
#35053 = AXIS2_PLACEMENT_3D('',#72366,#42636,#42637) ;
#35054 = AXIS2_PLACEMENT_3D('',#72367,#42638,#42639) ;
#35055 = AXIS2_PLACEMENT_3D('',#72370,#42640,#42641) ;
#35056 = AXIS2_PLACEMENT_3D('',#72373,#42643,#42644) ;
#35057 = AXIS2_PLACEMENT_3D('',#72375,#42646,#42647) ;
#35058 = AXIS2_PLACEMENT_3D('',#72377,#42648,#42649) ;
#35059 = AXIS2_PLACEMENT_3D('',#72378,#42650,#42651) ;
#35060 = AXIS2_PLACEMENT_3D('',#72379,#42652,#42653) ;
#35061 = AXIS2_PLACEMENT_3D('',#72381,#42654,#42655) ;
#35062 = AXIS2_PLACEMENT_3D('',#72383,#42657,#42658) ;
#35063 = AXIS2_PLACEMENT_3D('',#72385,#42659,#42660) ;
#35064 = AXIS2_PLACEMENT_3D('',#72386,#42661,#42662) ;
#35065 = AXIS2_PLACEMENT_3D('',#72387,#42663,#42664) ;
#35066 = AXIS2_PLACEMENT_3D('',#72390,#42665,#42666) ;
#35067 = AXIS2_PLACEMENT_3D('',#72391,#42667,#42668) ;
#35068 = AXIS2_PLACEMENT_3D('',#72392,#42669,#42670) ;
#35069 = AXIS2_PLACEMENT_3D('',#72393,#42671,#42672) ;
#35070 = AXIS2_PLACEMENT_3D('',#72395,#42674,#42675) ;
#35071 = AXIS2_PLACEMENT_3D('',#72396,#42676,#42677) ;
#35072 = AXIS2_PLACEMENT_3D('',#72398,#42679,#42680) ;
#35073 = AXIS2_PLACEMENT_3D('',#72400,#42681,#42682) ;
#35074 = AXIS2_PLACEMENT_3D('',#72401,#42683,#42684) ;
#35075 = AXIS2_PLACEMENT_3D('',#72402,#42685,#42686) ;
#35076 = AXIS2_PLACEMENT_3D('',#72403,#42687,#42688) ;
#35077 = AXIS2_PLACEMENT_3D('',#72405,#42690,#42691) ;
#35078 = AXIS2_PLACEMENT_3D('',#72408,#42694,#42695) ;
#35079 = AXIS2_PLACEMENT_3D('',#72410,#42696,#42697) ;
#35080 = AXIS2_PLACEMENT_3D('',#72412,#42699,#42700) ;
#35081 = AXIS2_PLACEMENT_3D('',#72414,#42702,#42703) ;
#35082 = AXIS2_PLACEMENT_3D('',#72415,#42704,#42705) ;
#35083 = AXIS2_PLACEMENT_3D('',#72416,#42706,#42707) ;
#35084 = AXIS2_PLACEMENT_3D('',#72417,#42708,#42709) ;
#35085 = AXIS2_PLACEMENT_3D('',#72418,#42710,#42711) ;
#35086 = AXIS2_PLACEMENT_3D('',#72420,#42713,#42714) ;
#35087 = AXIS2_PLACEMENT_3D('',#72421,#42715,#42716) ;
#35088 = AXIS2_PLACEMENT_3D('',#72422,#42717,#42718) ;
#35089 = AXIS2_PLACEMENT_3D('',#72423,#42719,#42720) ;
#35090 = AXIS2_PLACEMENT_3D('',#72424,#42721,#42722) ;
#35091 = AXIS2_PLACEMENT_3D('',#72425,#42723,#42724) ;
#35092 = AXIS2_PLACEMENT_3D('',#72426,#42725,#42726) ;
#35093 = AXIS2_PLACEMENT_3D('',#72427,#42727,#42728) ;
#35094 = AXIS2_PLACEMENT_3D('',#72436,#42733,#42734) ;
#35095 = AXIS2_PLACEMENT_3D('',#72438,#42735,#42736) ;
#35096 = AXIS2_PLACEMENT_3D('',#72440,#42737,#42738) ;
#35097 = AXIS2_PLACEMENT_3D('',#72441,#42739,#42740) ;
#35098 = AXIS2_PLACEMENT_3D('',#72442,#42741,#42742) ;
#35099 = AXIS2_PLACEMENT_3D('',#72444,#42743,#42744) ;
#35100 = AXIS2_PLACEMENT_3D('',#72445,#42745,#42746) ;
#35101 = AXIS2_PLACEMENT_3D('',#72446,#42747,#42748) ;
#35102 = AXIS2_PLACEMENT_3D('',#72447,#42749,#42750) ;
#35103 = AXIS2_PLACEMENT_3D('',#72449,#42752,#42753) ;
#35104 = AXIS2_PLACEMENT_3D('',#72450,#42754,#42755) ;
#35105 = AXIS2_PLACEMENT_3D('',#72451,#42756,#42757) ;
#35106 = AXIS2_PLACEMENT_3D('',#72453,#42759,#42760) ;
#35107 = AXIS2_PLACEMENT_3D('',#72454,#42761,#42762) ;
#35108 = AXIS2_PLACEMENT_3D('',#72455,#42763,#42764) ;
#35109 = AXIS2_PLACEMENT_3D('',#72456,#42765,#42766) ;
#35110 = AXIS2_PLACEMENT_3D('',#72457,#42767,#42768) ;
#35111 = AXIS2_PLACEMENT_3D('',#72458,#42769,#42770) ;
#35112 = AXIS2_PLACEMENT_3D('',#72459,#42771,#42772) ;
#35113 = AXIS2_PLACEMENT_3D('',#72460,#42773,#42774) ;
#35114 = AXIS2_PLACEMENT_3D('',#72461,#42775,#42776) ;
#35115 = AXIS2_PLACEMENT_3D('',#72464,#42777,#42778) ;
#35116 = AXIS2_PLACEMENT_3D('',#72467,#42780,#42781) ;
#35117 = AXIS2_PLACEMENT_3D('',#72469,#42783,#42784) ;
#35118 = AXIS2_PLACEMENT_3D('',#72471,#42785,#42786) ;
#35119 = AXIS2_PLACEMENT_3D('',#72472,#42787,#42788) ;
#35120 = AXIS2_PLACEMENT_3D('',#72473,#42789,#42790) ;
#35121 = AXIS2_PLACEMENT_3D('',#72475,#42791,#42792) ;
#35122 = AXIS2_PLACEMENT_3D('',#72477,#42794,#42795) ;
#35123 = AXIS2_PLACEMENT_3D('',#72479,#42796,#42797) ;
#35124 = AXIS2_PLACEMENT_3D('',#72480,#42798,#42799) ;
#35125 = AXIS2_PLACEMENT_3D('',#72481,#42800,#42801) ;
#35126 = AXIS2_PLACEMENT_3D('',#72484,#42802,#42803) ;
#35127 = AXIS2_PLACEMENT_3D('',#72485,#42804,#42805) ;
#35128 = AXIS2_PLACEMENT_3D('',#72486,#42806,#42807) ;
#35129 = AXIS2_PLACEMENT_3D('',#72487,#42808,#42809) ;
#35130 = AXIS2_PLACEMENT_3D('',#72489,#42811,#42812) ;
#35131 = AXIS2_PLACEMENT_3D('',#72490,#42813,#42814) ;
#35132 = AXIS2_PLACEMENT_3D('',#72492,#42816,#42817) ;
#35133 = AXIS2_PLACEMENT_3D('',#72494,#42818,#42819) ;
#35134 = AXIS2_PLACEMENT_3D('',#72495,#42820,#42821) ;
#35135 = AXIS2_PLACEMENT_3D('',#72496,#42822,#42823) ;
#35136 = AXIS2_PLACEMENT_3D('',#72497,#42824,#42825) ;
#35137 = AXIS2_PLACEMENT_3D('',#72499,#42827,#42828) ;
#35138 = AXIS2_PLACEMENT_3D('',#72502,#42831,#42832) ;
#35139 = AXIS2_PLACEMENT_3D('',#72504,#42833,#42834) ;
#35140 = AXIS2_PLACEMENT_3D('',#72506,#42836,#42837) ;
#35141 = AXIS2_PLACEMENT_3D('',#72508,#42839,#42840) ;
#35142 = AXIS2_PLACEMENT_3D('',#72509,#42841,#42842) ;
#35143 = AXIS2_PLACEMENT_3D('',#72510,#42843,#42844) ;
#35144 = AXIS2_PLACEMENT_3D('',#72511,#42845,#42846) ;
#35145 = AXIS2_PLACEMENT_3D('',#72512,#42847,#42848) ;
#35146 = AXIS2_PLACEMENT_3D('',#72514,#42850,#42851) ;
#35147 = AXIS2_PLACEMENT_3D('',#72515,#42852,#42853) ;
#35148 = AXIS2_PLACEMENT_3D('',#72516,#42854,#42855) ;
#35149 = AXIS2_PLACEMENT_3D('',#72517,#42856,#42857) ;
#35150 = AXIS2_PLACEMENT_3D('',#72518,#42858,#42859) ;
#35151 = AXIS2_PLACEMENT_3D('',#72519,#42860,#42861) ;
#35152 = AXIS2_PLACEMENT_3D('',#72520,#42862,#42863) ;
#35153 = AXIS2_PLACEMENT_3D('',#72521,#42864,#42865) ;
#35154 = AXIS2_PLACEMENT_3D('',#72530,#42870,#42871) ;
#35155 = AXIS2_PLACEMENT_3D('',#72532,#42872,#42873) ;
#35156 = AXIS2_PLACEMENT_3D('',#72534,#42874,#42875) ;
#35157 = AXIS2_PLACEMENT_3D('',#72535,#42876,#42877) ;
#35158 = AXIS2_PLACEMENT_3D('',#72536,#42878,#42879) ;
#35159 = AXIS2_PLACEMENT_3D('',#72538,#42880,#42881) ;
#35160 = AXIS2_PLACEMENT_3D('',#72539,#42882,#42883) ;
#35161 = AXIS2_PLACEMENT_3D('',#72540,#42884,#42885) ;
#35162 = AXIS2_PLACEMENT_3D('',#72541,#42886,#42887) ;
#35163 = AXIS2_PLACEMENT_3D('',#72543,#42889,#42890) ;
#35164 = AXIS2_PLACEMENT_3D('',#72544,#42891,#42892) ;
#35165 = AXIS2_PLACEMENT_3D('',#72545,#42893,#42894) ;
#35166 = AXIS2_PLACEMENT_3D('',#72547,#42896,#42897) ;
#35167 = AXIS2_PLACEMENT_3D('',#72548,#42898,#42899) ;
#35168 = AXIS2_PLACEMENT_3D('',#72549,#42900,#42901) ;
#35169 = AXIS2_PLACEMENT_3D('',#72550,#42902,#42903) ;
#35170 = AXIS2_PLACEMENT_3D('',#72551,#42904,#42905) ;
#35171 = AXIS2_PLACEMENT_3D('',#72552,#42906,#42907) ;
#35172 = AXIS2_PLACEMENT_3D('',#72553,#42908,#42909) ;
#35173 = AXIS2_PLACEMENT_3D('',#72554,#42910,#42911) ;
#35174 = AXIS2_PLACEMENT_3D('',#72555,#42912,#42913) ;
#35175 = AXIS2_PLACEMENT_3D('',#72558,#42914,#42915) ;
#35176 = AXIS2_PLACEMENT_3D('',#72561,#42917,#42918) ;
#35177 = AXIS2_PLACEMENT_3D('',#72563,#42920,#42921) ;
#35178 = AXIS2_PLACEMENT_3D('',#72565,#42922,#42923) ;
#35179 = AXIS2_PLACEMENT_3D('',#72566,#42924,#42925) ;
#35180 = AXIS2_PLACEMENT_3D('',#72567,#42926,#42927) ;
#35181 = AXIS2_PLACEMENT_3D('',#72569,#42928,#42929) ;
#35182 = AXIS2_PLACEMENT_3D('',#72571,#42931,#42932) ;
#35183 = AXIS2_PLACEMENT_3D('',#72573,#42933,#42934) ;
#35184 = AXIS2_PLACEMENT_3D('',#72574,#42935,#42936) ;
#35185 = AXIS2_PLACEMENT_3D('',#72575,#42937,#42938) ;
#35186 = AXIS2_PLACEMENT_3D('',#72578,#42939,#42940) ;
#35187 = AXIS2_PLACEMENT_3D('',#72579,#42941,#42942) ;
#35188 = AXIS2_PLACEMENT_3D('',#72580,#42943,#42944) ;
#35189 = AXIS2_PLACEMENT_3D('',#72581,#42945,#42946) ;
#35190 = AXIS2_PLACEMENT_3D('',#72583,#42948,#42949) ;
#35191 = AXIS2_PLACEMENT_3D('',#72584,#42950,#42951) ;
#35192 = AXIS2_PLACEMENT_3D('',#72586,#42953,#42954) ;
#35193 = AXIS2_PLACEMENT_3D('',#72588,#42955,#42956) ;
#35194 = AXIS2_PLACEMENT_3D('',#72589,#42957,#42958) ;
#35195 = AXIS2_PLACEMENT_3D('',#72590,#42959,#42960) ;
#35196 = AXIS2_PLACEMENT_3D('',#72591,#42961,#42962) ;
#35197 = AXIS2_PLACEMENT_3D('',#72593,#42964,#42965) ;
#35198 = AXIS2_PLACEMENT_3D('',#72596,#42968,#42969) ;
#35199 = AXIS2_PLACEMENT_3D('',#72598,#42970,#42971) ;
#35200 = AXIS2_PLACEMENT_3D('',#72600,#42973,#42974) ;
#35201 = AXIS2_PLACEMENT_3D('',#72602,#42976,#42977) ;
#35202 = AXIS2_PLACEMENT_3D('',#72603,#42978,#42979) ;
#35203 = AXIS2_PLACEMENT_3D('',#72604,#42980,#42981) ;
#35204 = AXIS2_PLACEMENT_3D('',#72605,#42982,#42983) ;
#35205 = AXIS2_PLACEMENT_3D('',#72606,#42984,#42985) ;
#35206 = AXIS2_PLACEMENT_3D('',#72608,#42987,#42988) ;
#35207 = AXIS2_PLACEMENT_3D('',#72609,#42989,#42990) ;
#35208 = AXIS2_PLACEMENT_3D('',#72610,#42991,#42992) ;
#35209 = AXIS2_PLACEMENT_3D('',#72611,#42993,#42994) ;
#35210 = AXIS2_PLACEMENT_3D('',#72612,#42995,#42996) ;
#35211 = AXIS2_PLACEMENT_3D('',#72613,#42997,#42998) ;
#35212 = AXIS2_PLACEMENT_3D('',#72614,#42999,#43000) ;
#35213 = AXIS2_PLACEMENT_3D('',#72615,#43001,#43002) ;
#35214 = AXIS2_PLACEMENT_3D('',#72624,#43007,#43008) ;
#35215 = AXIS2_PLACEMENT_3D('',#72626,#43009,#43010) ;
#35216 = AXIS2_PLACEMENT_3D('',#72628,#43011,#43012) ;
#35217 = AXIS2_PLACEMENT_3D('',#72629,#43013,#43014) ;
#35218 = AXIS2_PLACEMENT_3D('',#72630,#43015,#43016) ;
#35219 = AXIS2_PLACEMENT_3D('',#72632,#43017,#43018) ;
#35220 = AXIS2_PLACEMENT_3D('',#72633,#43019,#43020) ;
#35221 = AXIS2_PLACEMENT_3D('',#72634,#43021,#43022) ;
#35222 = AXIS2_PLACEMENT_3D('',#72635,#43023,#43024) ;
#35223 = AXIS2_PLACEMENT_3D('',#72637,#43026,#43027) ;
#35224 = AXIS2_PLACEMENT_3D('',#72638,#43028,#43029) ;
#35225 = AXIS2_PLACEMENT_3D('',#72639,#43030,#43031) ;
#35226 = AXIS2_PLACEMENT_3D('',#72641,#43033,#43034) ;
#35227 = AXIS2_PLACEMENT_3D('',#72642,#43035,#43036) ;
#35228 = AXIS2_PLACEMENT_3D('',#72643,#43037,#43038) ;
#35229 = AXIS2_PLACEMENT_3D('',#72644,#43039,#43040) ;
#35230 = AXIS2_PLACEMENT_3D('',#72645,#43041,#43042) ;
#35231 = AXIS2_PLACEMENT_3D('',#72646,#43043,#43044) ;
#35232 = AXIS2_PLACEMENT_3D('',#72647,#43045,#43046) ;
#35233 = AXIS2_PLACEMENT_3D('',#72650,#43049,#43050) ;
#35234 = AXIS2_PLACEMENT_3D('',#72653,#43053,#43054) ;
#35235 = AXIS2_PLACEMENT_3D('',#72656,#43057,#43058) ;
#35236 = AXIS2_PLACEMENT_3D('',#72659,#43061,#43062) ;
#35237 = AXIS2_PLACEMENT_3D('',#72662,#43065,#43066) ;
#35238 = AXIS2_PLACEMENT_3D('',#72665,#43069,#43070) ;
#35239 = AXIS2_PLACEMENT_3D('',#72668,#43073,#43074) ;
#35240 = AXIS2_PLACEMENT_3D('',#72671,#43077,#43078) ;
#35241 = AXIS2_PLACEMENT_3D('',#72674,#43081,#43082) ;
#35242 = AXIS2_PLACEMENT_3D('',#72676,#43084,#43085) ;
#35243 = AXIS2_PLACEMENT_3D('',#72678,#43087,#43088) ;
#35244 = AXIS2_PLACEMENT_3D('',#72680,#43090,#43091) ;
#35245 = AXIS2_PLACEMENT_3D('',#72682,#43093,#43094) ;
#35246 = AXIS2_PLACEMENT_3D('',#72684,#43096,#43097) ;
#35247 = AXIS2_PLACEMENT_3D('',#72686,#43099,#43100) ;
#35248 = AXIS2_PLACEMENT_3D('',#72688,#43102,#43103) ;
#35249 = AXIS2_PLACEMENT_3D('',#72690,#43105,#43106) ;
#35250 = AXIS2_PLACEMENT_3D('',#72692,#43108,#43109) ;
#35251 = AXIS2_PLACEMENT_3D('',#72694,#43111,#43112) ;
#35252 = AXIS2_PLACEMENT_3D('',#72696,#43114,#43115) ;
#35253 = AXIS2_PLACEMENT_3D('',#72698,#43117,#43118) ;
#35254 = AXIS2_PLACEMENT_3D('',#72700,#43120,#43121) ;
#35255 = AXIS2_PLACEMENT_3D('',#72702,#43123,#43124) ;
#35256 = AXIS2_PLACEMENT_3D('',#72704,#43126,#43127) ;
#35257 = AXIS2_PLACEMENT_3D('',#72706,#43129,#43130) ;
#35258 = AXIS2_PLACEMENT_3D('',#72708,#43132,#43133) ;
#35259 = AXIS2_PLACEMENT_3D('',#72710,#43135,#43136) ;
#35260 = AXIS2_PLACEMENT_3D('',#72791,#43177,#43178) ;
#35261 = AXIS2_PLACEMENT_3D('',#72793,#43179,#43180) ;
#35262 = AXIS2_PLACEMENT_3D('',#72796,#43182,#43183) ;
#35263 = AXIS2_PLACEMENT_3D('',#72797,#43184,#43185) ;
#35264 = AXIS2_PLACEMENT_3D('',#72802,#43189,#43190) ;
#35265 = AXIS2_PLACEMENT_3D('',#72806,#43192,#43193) ;
#35266 = AXIS2_PLACEMENT_3D('',#72807,#43194,#43195) ;
#35267 = AXIS2_PLACEMENT_3D('',#72808,#43196,#43197) ;
#35268 = AXIS2_PLACEMENT_3D('',#72810,#43198,#43199) ;
#35269 = AXIS2_PLACEMENT_3D('',#72813,#43201,#43202) ;
#35270 = AXIS2_PLACEMENT_3D('',#72814,#43203,#43204) ;
#35271 = AXIS2_PLACEMENT_3D('',#72816,#43205,#43206) ;
#35272 = AXIS2_PLACEMENT_3D('',#72819,#43208,#43209) ;
#35273 = AXIS2_PLACEMENT_3D('',#72820,#43210,#43211) ;
#35274 = AXIS2_PLACEMENT_3D('',#72824,#43213,#43214) ;
#35275 = AXIS2_PLACEMENT_3D('',#72825,#43215,#43216) ;
#35276 = AXIS2_PLACEMENT_3D('',#72826,#43217,#43218) ;
#35277 = AXIS2_PLACEMENT_3D('',#72830,#43220,#43221) ;
#35278 = AXIS2_PLACEMENT_3D('',#72831,#43222,#43223) ;
#35279 = AXIS2_PLACEMENT_3D('',#72832,#43224,#43225) ;
#35280 = AXIS2_PLACEMENT_3D('',#72836,#43227,#43228) ;
#35281 = AXIS2_PLACEMENT_3D('',#72837,#43229,#43230) ;
#35282 = AXIS2_PLACEMENT_3D('',#72838,#43231,#43232) ;
#35283 = AXIS2_PLACEMENT_3D('',#72840,#43233,#43234) ;
#35284 = AXIS2_PLACEMENT_3D('',#72843,#43236,#43237) ;
#35285 = AXIS2_PLACEMENT_3D('',#72844,#43238,#43239) ;
#35286 = AXIS2_PLACEMENT_3D('',#72848,#43241,#43242) ;
#35287 = AXIS2_PLACEMENT_3D('',#72849,#43243,#43244) ;
#35288 = AXIS2_PLACEMENT_3D('',#72850,#43245,#43246) ;
#35289 = AXIS2_PLACEMENT_3D('',#72852,#43247,#43248) ;
#35290 = AXIS2_PLACEMENT_3D('',#72857,#43252,#43253) ;
#35291 = AXIS2_PLACEMENT_3D('',#72860,#43255,#43256) ;
#35292 = AXIS2_PLACEMENT_3D('',#72861,#43257,#43258) ;
#35293 = AXIS2_PLACEMENT_3D('',#72863,#43260,#43261) ;
#35294 = AXIS2_PLACEMENT_3D('',#72872,#43266,#43267) ;
#35295 = AXIS2_PLACEMENT_3D('',#72881,#43272,#43273) ;
#35296 = AXIS2_PLACEMENT_3D('',#72890,#43278,#43279) ;
#35297 = AXIS2_PLACEMENT_3D('',#72899,#43284,#43285) ;
#35298 = AXIS2_PLACEMENT_3D('',#72908,#43290,#43291) ;
#35299 = AXIS2_PLACEMENT_3D('',#72917,#43296,#43297) ;
#35300 = AXIS2_PLACEMENT_3D('',#72926,#43302,#43303) ;
#35301 = AXIS2_PLACEMENT_3D('',#72935,#43308,#43309) ;
#35302 = AXIS2_PLACEMENT_3D('',#72938,#43312,#43313) ;
#35303 = AXIS2_PLACEMENT_3D('',#72943,#43317,#43318) ;
#35304 = AXIS2_PLACEMENT_3D('',#72948,#43322,#43323) ;
#35305 = AXIS2_PLACEMENT_3D('',#72953,#43327,#43328) ;
#35306 = AXIS2_PLACEMENT_3D('',#72958,#43332,#43333) ;
#35307 = AXIS2_PLACEMENT_3D('',#72963,#43337,#43338) ;
#35308 = AXIS2_PLACEMENT_3D('',#72968,#43342,#43343) ;
#35309 = AXIS2_PLACEMENT_3D('',#72973,#43347,#43348) ;
#35310 = AXIS2_PLACEMENT_3D('',#72978,#43352,#43353) ;
#35311 = AXIS2_PLACEMENT_3D('',#72983,#43357,#43358) ;
#35312 = AXIS2_PLACEMENT_3D('',#72988,#43362,#43363) ;
#35313 = AXIS2_PLACEMENT_3D('',#72993,#43367,#43368) ;
#35314 = AXIS2_PLACEMENT_3D('',#72998,#43372,#43373) ;
#35315 = AXIS2_PLACEMENT_3D('',#73003,#43377,#43378) ;
#35316 = AXIS2_PLACEMENT_3D('',#73008,#43382,#43383) ;
#35317 = AXIS2_PLACEMENT_3D('',#73013,#43387,#43388) ;
#35318 = AXIS2_PLACEMENT_3D('',#73018,#43392,#43393) ;
#35319 = AXIS2_PLACEMENT_3D('',#73019,#43394,#43395) ;
#35320 = AXIS2_PLACEMENT_3D('',#73021,#43397,#43398) ;
#35321 = AXIS2_PLACEMENT_3D('',#73023,#43400,#43401) ;
#35322 = AXIS2_PLACEMENT_3D('',#73025,#43403,#43404) ;
#35323 = AXIS2_PLACEMENT_3D('',#73027,#43406,#43407) ;
#35324 = AXIS2_PLACEMENT_3D('',#73029,#43409,#43410) ;
#35325 = AXIS2_PLACEMENT_3D('',#73031,#43412,#43413) ;
#35326 = AXIS2_PLACEMENT_3D('',#73033,#43415,#43416) ;
#35327 = AXIS2_PLACEMENT_3D('',#73035,#43418,#43419) ;
#35328 = AXIS2_PLACEMENT_3D('',#73037,#43421,#43422) ;
#35329 = AXIS2_PLACEMENT_3D('',#73039,#43423,#43424) ;
#35330 = AXIS2_PLACEMENT_3D('',#73040,#43425,#43426) ;
#35331 = AXIS2_PLACEMENT_3D('',#73043,#43427,#43428) ;
#35332 = AXIS2_PLACEMENT_3D('',#73044,#43429,#43430) ;
#35333 = AXIS2_PLACEMENT_3D('',#73045,#43431,#43432) ;
#35334 = AXIS2_PLACEMENT_3D('',#73046,#43433,#43434) ;
#35335 = AXIS2_PLACEMENT_3D('',#73048,#43435,#43436) ;
#35336 = AXIS2_PLACEMENT_3D('',#73050,#43438,#43439) ;
#35337 = AXIS2_PLACEMENT_3D('',#73051,#43440,#43441) ;
#35338 = AXIS2_PLACEMENT_3D('',#73052,#43442,#43443) ;
#35339 = AXIS2_PLACEMENT_3D('',#73054,#43445,#43446) ;
#35340 = AXIS2_PLACEMENT_3D('',#73055,#43447,#43448) ;
#35341 = AXIS2_PLACEMENT_3D('',#73057,#43449,#43450) ;
#35342 = AXIS2_PLACEMENT_3D('',#73058,#43451,#43452) ;
#35343 = AXIS2_PLACEMENT_3D('',#73061,#43453,#43454) ;
#35344 = AXIS2_PLACEMENT_3D('',#73062,#43455,#43456) ;
#35345 = AXIS2_PLACEMENT_3D('',#73063,#43457,#43458) ;
#35346 = AXIS2_PLACEMENT_3D('',#73064,#43459,#43460) ;
#35347 = AXIS2_PLACEMENT_3D('',#73066,#43461,#43462) ;
#35348 = AXIS2_PLACEMENT_3D('',#73068,#43464,#43465) ;
#35349 = AXIS2_PLACEMENT_3D('',#73069,#43466,#43467) ;
#35350 = AXIS2_PLACEMENT_3D('',#73070,#43468,#43469) ;
#35351 = AXIS2_PLACEMENT_3D('',#73072,#43471,#43472) ;
#35352 = AXIS2_PLACEMENT_3D('',#73073,#43473,#43474) ;
#35353 = AXIS2_PLACEMENT_3D('',#73075,#43475,#43476) ;
#35354 = AXIS2_PLACEMENT_3D('',#73076,#43477,#43478) ;
#35355 = AXIS2_PLACEMENT_3D('',#73079,#43479,#43480) ;
#35356 = AXIS2_PLACEMENT_3D('',#73080,#43481,#43482) ;
#35357 = AXIS2_PLACEMENT_3D('',#73081,#43483,#43484) ;
#35358 = AXIS2_PLACEMENT_3D('',#73082,#43485,#43486) ;
#35359 = AXIS2_PLACEMENT_3D('',#73084,#43487,#43488) ;
#35360 = AXIS2_PLACEMENT_3D('',#73086,#43490,#43491) ;
#35361 = AXIS2_PLACEMENT_3D('',#73087,#43492,#43493) ;
#35362 = AXIS2_PLACEMENT_3D('',#73088,#43494,#43495) ;
#35363 = AXIS2_PLACEMENT_3D('',#73090,#43497,#43498) ;
#35364 = AXIS2_PLACEMENT_3D('',#73091,#43499,#43500) ;
#35365 = AXIS2_PLACEMENT_3D('',#73093,#43501,#43502) ;
#35366 = AXIS2_PLACEMENT_3D('',#73094,#43503,#43504) ;
#35367 = AXIS2_PLACEMENT_3D('',#73097,#43505,#43506) ;
#35368 = AXIS2_PLACEMENT_3D('',#73098,#43507,#43508) ;
#35369 = AXIS2_PLACEMENT_3D('',#73099,#43509,#43510) ;
#35370 = AXIS2_PLACEMENT_3D('',#73100,#43511,#43512) ;
#35371 = AXIS2_PLACEMENT_3D('',#73102,#43513,#43514) ;
#35372 = AXIS2_PLACEMENT_3D('',#73104,#43516,#43517) ;
#35373 = AXIS2_PLACEMENT_3D('',#73105,#43518,#43519) ;
#35374 = AXIS2_PLACEMENT_3D('',#73106,#43520,#43521) ;
#35375 = AXIS2_PLACEMENT_3D('',#73108,#43523,#43524) ;
#35376 = AXIS2_PLACEMENT_3D('',#73109,#43525,#43526) ;
#35377 = AXIS2_PLACEMENT_3D('',#73111,#43527,#43528) ;
#35378 = AXIS2_PLACEMENT_3D('',#73112,#43529,#43530) ;
#35379 = AXIS2_PLACEMENT_3D('',#73115,#43531,#43532) ;
#35380 = AXIS2_PLACEMENT_3D('',#73116,#43533,#43534) ;
#35381 = AXIS2_PLACEMENT_3D('',#73117,#43535,#43536) ;
#35382 = AXIS2_PLACEMENT_3D('',#73118,#43537,#43538) ;
#35383 = AXIS2_PLACEMENT_3D('',#73120,#43539,#43540) ;
#35384 = AXIS2_PLACEMENT_3D('',#73122,#43542,#43543) ;
#35385 = AXIS2_PLACEMENT_3D('',#73123,#43544,#43545) ;
#35386 = AXIS2_PLACEMENT_3D('',#73124,#43546,#43547) ;
#35387 = AXIS2_PLACEMENT_3D('',#73126,#43549,#43550) ;
#35388 = AXIS2_PLACEMENT_3D('',#73127,#43551,#43552) ;
#35389 = AXIS2_PLACEMENT_3D('',#73129,#43553,#43554) ;
#35390 = AXIS2_PLACEMENT_3D('',#73130,#43555,#43556) ;
#35391 = AXIS2_PLACEMENT_3D('',#73133,#43557,#43558) ;
#35392 = AXIS2_PLACEMENT_3D('',#73134,#43559,#43560) ;
#35393 = AXIS2_PLACEMENT_3D('',#73135,#43561,#43562) ;
#35394 = AXIS2_PLACEMENT_3D('',#73136,#43563,#43564) ;
#35395 = AXIS2_PLACEMENT_3D('',#73138,#43565,#43566) ;
#35396 = AXIS2_PLACEMENT_3D('',#73140,#43568,#43569) ;
#35397 = AXIS2_PLACEMENT_3D('',#73141,#43570,#43571) ;
#35398 = AXIS2_PLACEMENT_3D('',#73142,#43572,#43573) ;
#35399 = AXIS2_PLACEMENT_3D('',#73144,#43575,#43576) ;
#35400 = AXIS2_PLACEMENT_3D('',#73145,#43577,#43578) ;
#35401 = AXIS2_PLACEMENT_3D('',#73147,#43579,#43580) ;
#35402 = AXIS2_PLACEMENT_3D('',#73148,#43581,#43582) ;
#35403 = AXIS2_PLACEMENT_3D('',#73151,#43583,#43584) ;
#35404 = AXIS2_PLACEMENT_3D('',#73152,#43585,#43586) ;
#35405 = AXIS2_PLACEMENT_3D('',#73153,#43587,#43588) ;
#35406 = AXIS2_PLACEMENT_3D('',#73154,#43589,#43590) ;
#35407 = AXIS2_PLACEMENT_3D('',#73156,#43591,#43592) ;
#35408 = AXIS2_PLACEMENT_3D('',#73158,#43594,#43595) ;
#35409 = AXIS2_PLACEMENT_3D('',#73159,#43596,#43597) ;
#35410 = AXIS2_PLACEMENT_3D('',#73160,#43598,#43599) ;
#35411 = AXIS2_PLACEMENT_3D('',#73162,#43601,#43602) ;
#35412 = AXIS2_PLACEMENT_3D('',#73163,#43603,#43604) ;
#35413 = AXIS2_PLACEMENT_3D('',#73165,#43605,#43606) ;
#35414 = AXIS2_PLACEMENT_3D('',#73166,#43607,#43608) ;
#35415 = AXIS2_PLACEMENT_3D('',#73169,#43609,#43610) ;
#35416 = AXIS2_PLACEMENT_3D('',#73170,#43611,#43612) ;
#35417 = AXIS2_PLACEMENT_3D('',#73171,#43613,#43614) ;
#35418 = AXIS2_PLACEMENT_3D('',#73172,#43615,#43616) ;
#35419 = AXIS2_PLACEMENT_3D('',#73174,#43617,#43618) ;
#35420 = AXIS2_PLACEMENT_3D('',#73176,#43620,#43621) ;
#35421 = AXIS2_PLACEMENT_3D('',#73177,#43622,#43623) ;
#35422 = AXIS2_PLACEMENT_3D('',#73178,#43624,#43625) ;
#35423 = AXIS2_PLACEMENT_3D('',#73180,#43627,#43628) ;
#35424 = AXIS2_PLACEMENT_3D('',#73181,#43629,#43630) ;
#35425 = AXIS2_PLACEMENT_3D('',#73184,#43631,#43632) ;
#35426 = AXIS2_PLACEMENT_3D('',#73185,#43633,#43634) ;
#35427 = AXIS2_PLACEMENT_3D('',#73186,#43635,#43636) ;
#35428 = AXIS2_PLACEMENT_3D('',#73187,#43637,#43638) ;
#35429 = AXIS2_PLACEMENT_3D('',#73189,#43639,#43640) ;
#35430 = AXIS2_PLACEMENT_3D('',#73191,#43642,#43643) ;
#35431 = AXIS2_PLACEMENT_3D('',#73192,#43644,#43645) ;
#35432 = AXIS2_PLACEMENT_3D('',#73193,#43646,#43647) ;
#35433 = AXIS2_PLACEMENT_3D('',#73195,#43649,#43650) ;
#35434 = AXIS2_PLACEMENT_3D('',#73196,#43651,#43652) ;
#35435 = AXIS2_PLACEMENT_3D('',#73198,#43654,#43655) ;
#35436 = AXIS2_PLACEMENT_3D('',#73200,#43657,#43658) ;
#35437 = AXIS2_PLACEMENT_3D('',#73202,#43660,#43661) ;
#35438 = AXIS2_PLACEMENT_3D('',#73203,#43662,#43663) ;
#35439 = AXIS2_PLACEMENT_3D('',#73204,#43664,#43665) ;
#35440 = AXIS2_PLACEMENT_3D('',#73206,#43667,#43668) ;
#35441 = AXIS2_PLACEMENT_3D('',#73208,#43670,#43671) ;
#35442 = AXIS2_PLACEMENT_3D('',#73210,#43673,#43674) ;
#35443 = AXIS2_PLACEMENT_3D('',#73211,#43675,#43676) ;
#35444 = AXIS2_PLACEMENT_3D('',#73212,#43677,#43678) ;
#35445 = AXIS2_PLACEMENT_3D('',#73214,#43680,#43681) ;
#35446 = AXIS2_PLACEMENT_3D('',#73216,#43683,#43684) ;
#35447 = AXIS2_PLACEMENT_3D('',#73218,#43686,#43687) ;
#35448 = AXIS2_PLACEMENT_3D('',#73219,#43688,#43689) ;
#35449 = AXIS2_PLACEMENT_3D('',#73220,#43690,#43691) ;
#35450 = AXIS2_PLACEMENT_3D('',#73222,#43693,#43694) ;
#35451 = AXIS2_PLACEMENT_3D('',#73224,#43696,#43697) ;
#35452 = AXIS2_PLACEMENT_3D('',#73226,#43699,#43700) ;
#35453 = AXIS2_PLACEMENT_3D('',#73227,#43701,#43702) ;
#35454 = AXIS2_PLACEMENT_3D('',#73228,#43703,#43704) ;
#35455 = AXIS2_PLACEMENT_3D('',#73230,#43706,#43707) ;
#35456 = AXIS2_PLACEMENT_3D('',#73232,#43709,#43710) ;
#35457 = AXIS2_PLACEMENT_3D('',#73234,#43712,#43713) ;
#35458 = AXIS2_PLACEMENT_3D('',#73235,#43714,#43715) ;
#35459 = AXIS2_PLACEMENT_3D('',#73236,#43716,#43717) ;
#35460 = AXIS2_PLACEMENT_3D('',#73238,#43719,#43720) ;
#35461 = AXIS2_PLACEMENT_3D('',#73240,#43722,#43723) ;
#35462 = AXIS2_PLACEMENT_3D('',#73242,#43725,#43726) ;
#35463 = AXIS2_PLACEMENT_3D('',#73243,#43727,#43728) ;
#35464 = AXIS2_PLACEMENT_3D('',#73244,#43729,#43730) ;
#35465 = AXIS2_PLACEMENT_3D('',#73246,#43732,#43733) ;
#35466 = AXIS2_PLACEMENT_3D('',#73248,#43735,#43736) ;
#35467 = AXIS2_PLACEMENT_3D('',#73250,#43738,#43739) ;
#35468 = AXIS2_PLACEMENT_3D('',#73251,#43740,#43741) ;
#35469 = AXIS2_PLACEMENT_3D('',#73252,#43742,#43743) ;
#35470 = AXIS2_PLACEMENT_3D('',#73254,#43745,#43746) ;
#35471 = AXIS2_PLACEMENT_3D('',#73256,#43748,#43749) ;
#35472 = AXIS2_PLACEMENT_3D('',#73258,#43751,#43752) ;
#35473 = AXIS2_PLACEMENT_3D('',#73259,#43753,#43754) ;
#35474 = AXIS2_PLACEMENT_3D('',#73260,#43755,#43756) ;
#35475 = AXIS2_PLACEMENT_3D('',#73261,#43757,#43758) ;
#35476 = AXIS2_PLACEMENT_3D('',#73262,#43759,#43760) ;
#35477 = AXIS2_PLACEMENT_3D('',#73333,#43762,#43763) ;
#35478 = AXIS2_PLACEMENT_3D('',#73409,#43765,#43766) ;
#35479 = AXIS2_PLACEMENT_3D('',#73485,#43768,#43769) ;
#35480 = AXIS2_PLACEMENT_3D('',#73561,#43771,#43772) ;
#35481 = AXIS2_PLACEMENT_3D('',#73637,#43774,#43775) ;
#35482 = AXIS2_PLACEMENT_3D('',#73713,#43777,#43778) ;
#35483 = AXIS2_PLACEMENT_3D('',#73789,#43780,#43781) ;
#35484 = AXIS2_PLACEMENT_3D('',#73794,#43783,#43784) ;
#35485 = AXIS2_PLACEMENT_3D('',#73865,#43785,#43786) ;
#35486 = AXIS2_PLACEMENT_3D('',#73895,#43788,#43789) ;
#35487 = AXIS2_PLACEMENT_3D('',#73916,#43790,#43791) ;
#35488 = AXIS2_PLACEMENT_3D('',#73992,#43793,#43794) ;
#35489 = AXIS2_PLACEMENT_3D('',#74068,#43796,#43797) ;
#35490 = AXIS2_PLACEMENT_3D('',#74144,#43799,#43800) ;
#35491 = AXIS2_PLACEMENT_3D('',#74220,#43802,#43803) ;
#35492 = AXIS2_PLACEMENT_3D('',#74296,#43805,#43806) ;
#35493 = AXIS2_PLACEMENT_3D('',#74372,#43808,#43809) ;
#35494 = AXIS2_PLACEMENT_3D('',#74399,#43810,#43811) ;
#35495 = AXIS2_PLACEMENT_3D('',#74431,#43812,#43813) ;
#35496 = AXIS2_PLACEMENT_3D('',#74437,#43814,#43815) ;
#35497 = AXIS2_PLACEMENT_3D('',#74464,#43816,#43817) ;
#35498 = AXIS2_PLACEMENT_3D('',#74504,#43818,#43819) ;
#35499 = AXIS2_PLACEMENT_3D('',#74540,#43820,#43821) ;
#35500 = AXIS2_PLACEMENT_3D('',#74573,#43822,#43823) ;
#35501 = AXIS2_PLACEMENT_3D('',#74574,#43824,#43825) ;
#35502 = AXIS2_PLACEMENT_3D('',#74575,#43826,#43827) ;
#35503 = AXIS2_PLACEMENT_3D('',#74650,#43828,#43829) ;
#35504 = AXIS2_PLACEMENT_3D('',#74683,#43831,#43832) ;
#35505 = AXIS2_PLACEMENT_3D('',#74772,#43835,#43836) ;
#35506 = AXIS2_PLACEMENT_3D('',#74773,#43837,#43838) ;
#35507 = AXIS2_PLACEMENT_3D('',#74774,#43839,#43840) ;
#35508 = AXIS2_PLACEMENT_3D('',#74777,#43841,#43842) ;
#35509 = AXIS2_PLACEMENT_3D('',#74786,#43843,#43844) ;
#35510 = AXIS2_PLACEMENT_3D('',#74788,#43845,#43846) ;
#35511 = AXIS2_PLACEMENT_3D('',#74790,#43847,#43848) ;
#35512 = AXIS2_PLACEMENT_3D('',#74798,#43849,#43850) ;
#35513 = AXIS2_PLACEMENT_3D('',#74800,#43851,#43852) ;
#35514 = AXIS2_PLACEMENT_3D('',#74802,#43853,#43854) ;
#35515 = AXIS2_PLACEMENT_3D('',#74810,#43855,#43856) ;
#35516 = AXIS2_PLACEMENT_3D('',#74812,#43857,#43858) ;
#35517 = AXIS2_PLACEMENT_3D('',#74813,#43859,#43860) ;
#35518 = AXIS2_PLACEMENT_3D('',#74814,#43861,#43862) ;
#35519 = AXIS2_PLACEMENT_3D('',#74816,#43863,#43864) ;
#35520 = AXIS2_PLACEMENT_3D('',#74818,#43865,#43866) ;
#35521 = AXIS2_PLACEMENT_3D('',#74825,#43867,#43868) ;
#35522 = AXIS2_PLACEMENT_3D('',#74851,#43869,#43870) ;
#35523 = AXIS2_PLACEMENT_3D('',#74879,#43871,#43872) ;
#35524 = AXIS2_PLACEMENT_3D('',#74916,#43873,#43874) ;
#35525 = AXIS2_PLACEMENT_3D('',#74943,#43875,#43876) ;
#35526 = AXIS2_PLACEMENT_3D('',#74944,#43877,#43878) ;
#35527 = AXIS2_PLACEMENT_3D('',#75016,#43880,#43881) ;
#35528 = AXIS2_PLACEMENT_3D('',#75040,#43883,#43884) ;
#35529 = AXIS2_PLACEMENT_3D('',#75111,#43886,#43887) ;
#35530 = AXIS2_PLACEMENT_3D('',#75115,#43889,#43890) ;
#35531 = AXIS2_PLACEMENT_3D('',#75117,#43892,#43893) ;
#35532 = AXIS2_PLACEMENT_3D('',#75123,#43896,#43897) ;
#35533 = AXIS2_PLACEMENT_3D('',#75154,#43898,#43899) ;
#35534 = AXIS2_PLACEMENT_3D('',#75187,#43900,#43901) ;
#35535 = AXIS2_PLACEMENT_3D('',#75223,#43902,#43903) ;
#35536 = AXIS2_PLACEMENT_3D('',#75256,#43904,#43905) ;
#35537 = AXIS2_PLACEMENT_3D('',#75257,#43906,#43907) ;
#35538 = AXIS2_PLACEMENT_3D('',#75258,#43908,#43909) ;
#35539 = AXIS2_PLACEMENT_3D('',#75306,#43910,#43911) ;
#35540 = AXIS2_PLACEMENT_3D('',#75392,#43913,#43914) ;
#35541 = AXIS2_PLACEMENT_3D('',#75478,#43917,#43918) ;
#35542 = AXIS2_PLACEMENT_3D('',#75479,#43919,#43920) ;
#35543 = AXIS2_PLACEMENT_3D('',#75481,#43921,#43922) ;
#35544 = AXIS2_PLACEMENT_3D('',#75483,#43923,#43924) ;
#35545 = AXIS2_PLACEMENT_3D('',#75490,#43925,#43926) ;
#35546 = AXIS2_PLACEMENT_3D('',#75516,#43927,#43928) ;
#35547 = AXIS2_PLACEMENT_3D('',#75544,#43929,#43930) ;
#35548 = AXIS2_PLACEMENT_3D('',#75581,#43931,#43932) ;
#35549 = AXIS2_PLACEMENT_3D('',#75608,#43933,#43934) ;
#35550 = AXIS2_PLACEMENT_3D('',#75609,#43935,#43936) ;
#35551 = AXIS2_PLACEMENT_3D('',#75681,#43938,#43939) ;
#35552 = AXIS2_PLACEMENT_3D('',#75705,#43941,#43942) ;
#35553 = AXIS2_PLACEMENT_3D('',#75776,#43944,#43945) ;
#35554 = AXIS2_PLACEMENT_3D('',#75780,#43947,#43948) ;
#35555 = AXIS2_PLACEMENT_3D('',#75782,#43950,#43951) ;
#35556 = AXIS2_PLACEMENT_3D('',#75788,#43954,#43955) ;
#35557 = AXIS2_PLACEMENT_3D('',#75789,#43956,#43957) ;
#35558 = AXIS2_PLACEMENT_3D('',#75808,#43958,#43959) ;
#35559 = AXIS2_PLACEMENT_3D('',#75810,#43960,#43961) ;
#35560 = AXIS2_PLACEMENT_3D('',#75811,#43962,#43963) ;
#35561 = AXIS2_PLACEMENT_3D('',#75812,#43964,#43965) ;
#35562 = AXIS2_PLACEMENT_3D('',#75816,#43967,#43968) ;
#35563 = AXIS2_PLACEMENT_3D('',#75818,#43970,#43971) ;
#35564 = AXIS2_PLACEMENT_3D('',#75820,#43972,#43973) ;
#35565 = AXIS2_PLACEMENT_3D('',#75821,#43974,#43975) ;
#35566 = AXIS2_PLACEMENT_3D('',#75822,#43976,#43977) ;
#35567 = AXIS2_PLACEMENT_3D('',#75824,#43978,#43979) ;
#35568 = AXIS2_PLACEMENT_3D('',#75832,#43980,#43981) ;
#35569 = AXIS2_PLACEMENT_3D('',#75833,#43982,#43983) ;
#35570 = AXIS2_PLACEMENT_3D('',#75841,#43985,#43986) ;
#35571 = AXIS2_PLACEMENT_3D('',#75842,#43987,#43988) ;
#35572 = AXIS2_PLACEMENT_3D('',#75845,#43990,#43991) ;
#35573 = AXIS2_PLACEMENT_3D('',#75883,#43992,#43993) ;
#35574 = AXIS2_PLACEMENT_3D('',#75905,#43994,#43995) ;
#35575 = AXIS2_PLACEMENT_3D('',#75906,#43996,#43997) ;
#35576 = AXIS2_PLACEMENT_3D('',#75928,#43998,#43999) ;
#35577 = AXIS2_PLACEMENT_3D('',#75937,#44000,#44001) ;
#35578 = AXIS2_PLACEMENT_3D('',#75938,#44002,#44003) ;
#35579 = AXIS2_PLACEMENT_3D('',#75939,#44004,#44005) ;
#35580 = AXIS2_PLACEMENT_3D('',#75942,#44006,#44007) ;
#35581 = AXIS2_PLACEMENT_3D('',#75944,#44008,#44009) ;
#35582 = AXIS2_PLACEMENT_3D('',#75945,#44010,#44011) ;
#35583 = AXIS2_PLACEMENT_3D('',#75968,#44012,#44013) ;
#35584 = AXIS2_PLACEMENT_3D('',#76003,#44014,#44015) ;
#35585 = AXIS2_PLACEMENT_3D('',#76004,#44016,#44017) ;
#35586 = AXIS2_PLACEMENT_3D('',#76005,#44018,#44019) ;
#35587 = AXIS2_PLACEMENT_3D('',#76049,#44020,#44021) ;
#35588 = AXIS2_PLACEMENT_3D('',#76051,#44022,#44023) ;
#35589 = AXIS2_PLACEMENT_3D('',#76053,#44024,#44025) ;
#35590 = AXIS2_PLACEMENT_3D('',#76054,#44026,#44027) ;
#35591 = AXIS2_PLACEMENT_3D('',#76055,#44028,#44029) ;
#35592 = AXIS2_PLACEMENT_3D('',#76059,#44032,#44033) ;
#35593 = AXIS2_PLACEMENT_3D('',#76062,#44035,#44036) ;
#35594 = AXIS2_PLACEMENT_3D('',#76080,#44037,#44038) ;
#35595 = AXIS2_PLACEMENT_3D('',#76081,#44039,#44040) ;
#35596 = AXIS2_PLACEMENT_3D('',#76082,#44041,#44042) ;
#35597 = AXIS2_PLACEMENT_3D('',#76085,#44044,#44045) ;
#35598 = AXIS2_PLACEMENT_3D('',#76086,#44046,#44047) ;
#35599 = AXIS2_PLACEMENT_3D('',#76087,#44048,#44049) ;
#35600 = AXIS2_PLACEMENT_3D('',#76088,#44050,#44051) ;
#35601 = AXIS2_PLACEMENT_3D('',#76094,#44054,#44055) ;
#35602 = AXIS2_PLACEMENT_3D('',#76097,#44057,#44058) ;
#35603 = AXIS2_PLACEMENT_3D('',#76098,#44059,#44060) ;
#35604 = AXIS2_PLACEMENT_3D('',#76101,#44062,#44063) ;
#35605 = AXIS2_PLACEMENT_3D('',#76102,#44064,#44065) ;
#35606 = AXIS2_PLACEMENT_3D('',#76105,#44066,#44067) ;
#35607 = AXIS2_PLACEMENT_3D('',#76107,#44068,#44069) ;
#35608 = AXIS2_PLACEMENT_3D('',#76108,#44070,#44071) ;
#35609 = AXIS2_PLACEMENT_3D('',#76131,#44072,#44073) ;
#35610 = AXIS2_PLACEMENT_3D('',#76165,#44074,#44075) ;
#35611 = AXIS2_PLACEMENT_3D('',#76167,#44076,#44077) ;
#35612 = AXIS2_PLACEMENT_3D('',#76168,#44078,#44079) ;
#35613 = AXIS2_PLACEMENT_3D('',#76212,#44080,#44081) ;
#35614 = AXIS2_PLACEMENT_3D('',#76214,#44082,#44083) ;
#35615 = AXIS2_PLACEMENT_3D('',#76216,#44084,#44085) ;
#35616 = AXIS2_PLACEMENT_3D('',#76224,#44086,#44087) ;
#35617 = AXIS2_PLACEMENT_3D('',#76225,#44088,#44089) ;
#35618 = AXIS2_PLACEMENT_3D('',#76227,#44090,#44091) ;
#35619 = AXIS2_PLACEMENT_3D('',#76236,#44092,#44093) ;
#35620 = AXIS2_PLACEMENT_3D('',#76238,#44094,#44095) ;
#35621 = AXIS2_PLACEMENT_3D('',#76239,#44096,#44097) ;
#35622 = AXIS2_PLACEMENT_3D('',#76240,#44098,#44099) ;
#35623 = AXIS2_PLACEMENT_3D('',#76244,#44101,#44102) ;
#35624 = AXIS2_PLACEMENT_3D('',#76246,#44104,#44105) ;
#35625 = AXIS2_PLACEMENT_3D('',#76248,#44106,#44107) ;
#35626 = AXIS2_PLACEMENT_3D('',#76249,#44108,#44109) ;
#35627 = AXIS2_PLACEMENT_3D('',#76271,#44110,#44111) ;
#35628 = AXIS2_PLACEMENT_3D('',#76297,#44112,#44113) ;
#35629 = AXIS2_PLACEMENT_3D('',#76298,#44114,#44115) ;
#35630 = AXIS2_PLACEMENT_3D('',#76335,#44116,#44117) ;
#35631 = AXIS2_PLACEMENT_3D('',#76337,#44118,#44119) ;
#35632 = AXIS2_PLACEMENT_3D('',#76339,#44120,#44121) ;
#35633 = AXIS2_PLACEMENT_3D('',#76340,#44122,#44123) ;
#35634 = AXIS2_PLACEMENT_3D('',#76341,#44124,#44125) ;
#35635 = AXIS2_PLACEMENT_3D('',#76345,#44128,#44129) ;
#35636 = AXIS2_PLACEMENT_3D('',#76348,#44131,#44132) ;
#35637 = AXIS2_PLACEMENT_3D('',#76366,#44133,#44134) ;
#35638 = AXIS2_PLACEMENT_3D('',#76367,#44135,#44136) ;
#35639 = AXIS2_PLACEMENT_3D('',#76368,#44137,#44138) ;
#35640 = AXIS2_PLACEMENT_3D('',#76371,#44140,#44141) ;
#35641 = AXIS2_PLACEMENT_3D('',#76372,#44142,#44143) ;
#35642 = AXIS2_PLACEMENT_3D('',#76373,#44144,#44145) ;
#35643 = AXIS2_PLACEMENT_3D('',#76374,#44146,#44147) ;
#35644 = AXIS2_PLACEMENT_3D('',#76380,#44150,#44151) ;
#35645 = AXIS2_PLACEMENT_3D('',#76383,#44153,#44154) ;
#35646 = AXIS2_PLACEMENT_3D('',#76384,#44155,#44156) ;
#35647 = AXIS2_PLACEMENT_3D('',#76387,#44158,#44159) ;
#35648 = AXIS2_PLACEMENT_3D('',#76405,#44160,#44161) ;
#35649 = AXIS2_PLACEMENT_3D('',#76406,#44162,#44163) ;
#35650 = AXIS2_PLACEMENT_3D('',#76407,#44164,#44165) ;
#35651 = AXIS2_PLACEMENT_3D('',#76411,#44167,#44168) ;
#35652 = AXIS2_PLACEMENT_3D('',#76413,#44170,#44171) ;
#35653 = AXIS2_PLACEMENT_3D('',#76415,#44172,#44173) ;
#35654 = AXIS2_PLACEMENT_3D('',#76416,#44174,#44175) ;
#35655 = AXIS2_PLACEMENT_3D('',#76417,#44176,#44177) ;
#35656 = AXIS2_PLACEMENT_3D('',#76418,#44178,#44179) ;
#35657 = AXIS2_PLACEMENT_3D('',#76419,#44180,#44181) ;
#35658 = AXIS2_PLACEMENT_3D('',#76423,#44183,#44184) ;
#35659 = AXIS2_PLACEMENT_3D('',#76495,#44186,#44187) ;
#35660 = AXIS2_PLACEMENT_3D('',#76497,#44188,#44189) ;
#35661 = AXIS2_PLACEMENT_3D('',#76544,#44190,#44191) ;
#35662 = AXIS2_PLACEMENT_3D('',#76564,#44192,#44193) ;
#35663 = AXIS2_PLACEMENT_3D('',#76694,#44194,#44195) ;
#35664 = AXIS2_PLACEMENT_3D('',#76695,#44196,#44197) ;
#35665 = AXIS2_PLACEMENT_3D('',#77298,#44198,#44199) ;
#35666 = AXIS2_PLACEMENT_3D('',#77325,#44200,#44201) ;
#35667 = AXIS2_PLACEMENT_3D('',#77327,#44202,#44203) ;
#35668 = AXIS2_PLACEMENT_3D('',#77329,#44204,#44205) ;
#35669 = AXIS2_PLACEMENT_3D('',#77331,#44206,#44207) ;
#35670 = AXIS2_PLACEMENT_3D('',#77337,#44210,#44211) ;
#35671 = AXIS2_PLACEMENT_3D('',#77339,#44212,#44213) ;
#35672 = AXIS2_PLACEMENT_3D('',#77340,#44214,#44215) ;
#35673 = AXIS2_PLACEMENT_3D('',#77363,#44216,#44217) ;
#35674 = AXIS2_PLACEMENT_3D('',#77364,#44218,#44219) ;
#35675 = AXIS2_PLACEMENT_3D('',#77365,#44220,#44221) ;
#35676 = AXIS2_PLACEMENT_3D('',#77389,#44223,#44224) ;
#35677 = AXIS2_PLACEMENT_3D('',#77391,#44226,#44227) ;
#35678 = AXIS2_PLACEMENT_3D('',#77393,#44228,#44229) ;
#35679 = AXIS2_PLACEMENT_3D('',#77394,#44230,#44231) ;
#35680 = AXIS2_PLACEMENT_3D('',#77395,#44232,#44233) ;
#35681 = AXIS2_PLACEMENT_3D('',#77401,#44237,#44238) ;
#35682 = AXIS2_PLACEMENT_3D('',#77404,#44240,#44241) ;
#35683 = AXIS2_PLACEMENT_3D('',#77405,#44242,#44243) ;
#35684 = AXIS2_PLACEMENT_3D('',#77407,#44244,#44245) ;
#35685 = AXIS2_PLACEMENT_3D('',#77420,#44246,#44247) ;
#35686 = AXIS2_PLACEMENT_3D('',#77421,#44248,#44249) ;
#35687 = AXIS2_PLACEMENT_3D('',#77424,#44250,#44251) ;
#35688 = AXIS2_PLACEMENT_3D('',#77426,#44252,#44253) ;
#35689 = AXIS2_PLACEMENT_3D('',#77427,#44254,#44255) ;
#35690 = AXIS2_PLACEMENT_3D('',#77450,#44256,#44257) ;
#35691 = AXIS2_PLACEMENT_3D('',#77474,#44260,#44261) ;
#35692 = AXIS2_PLACEMENT_3D('',#77475,#44262,#44263) ;
#35693 = AXIS2_PLACEMENT_3D('',#77476,#44264,#44265) ;
#35694 = AXIS2_PLACEMENT_3D('',#77518,#44266,#44267) ;
#35695 = AXIS2_PLACEMENT_3D('',#77522,#44269,#44270) ;
#35696 = AXIS2_PLACEMENT_3D('',#77524,#44272,#44273) ;
#35697 = AXIS2_PLACEMENT_3D('',#77528,#44276,#44277) ;
#35698 = AXIS2_PLACEMENT_3D('',#77531,#44279,#44280) ;
#35699 = AXIS2_PLACEMENT_3D('',#77532,#44281,#44282) ;
#35700 = AXIS2_PLACEMENT_3D('',#77556,#44287,#44288) ;
#35701 = AXIS2_PLACEMENT_3D('',#77557,#44289,#44290) ;
#35702 = AXIS2_PLACEMENT_3D('',#77558,#44291,#44292) ;
#35703 = AXIS2_PLACEMENT_3D('',#77561,#44293,#44294) ;
#35704 = AXIS2_PLACEMENT_3D('',#77589,#44297,#44298) ;
#35705 = AXIS2_PLACEMENT_3D('',#77591,#44299,#44300) ;
#35706 = AXIS2_PLACEMENT_3D('',#77592,#44301,#44302) ;
#35707 = AXIS2_PLACEMENT_3D('',#77593,#44303,#44304) ;
#35708 = AXIS2_PLACEMENT_3D('',#77594,#44305,#44306) ;
#35709 = AXIS2_PLACEMENT_3D('',#77596,#44307,#44308) ;
#35710 = AXIS2_PLACEMENT_3D('',#77598,#44310,#44311) ;
#35711 = AXIS2_PLACEMENT_3D('',#77600,#44312,#44313) ;
#35712 = AXIS2_PLACEMENT_3D('',#77601,#44314,#44315) ;
#35713 = AXIS2_PLACEMENT_3D('',#77602,#44316,#44317) ;
#35714 = AXIS2_PLACEMENT_3D('',#77603,#44318,#44319) ;
#35715 = AXIS2_PLACEMENT_3D('',#77604,#44320,#44321) ;
#35716 = AXIS2_PLACEMENT_3D('',#77607,#44323,#44324) ;
#35717 = AXIS2_PLACEMENT_3D('',#77609,#44326,#44327) ;
#35718 = AXIS2_PLACEMENT_3D('',#77613,#44330,#44331) ;
#35719 = AXIS2_PLACEMENT_3D('',#77614,#44332,#44333) ;
#35720 = AXIS2_PLACEMENT_3D('',#77615,#44334,#44335) ;
#35721 = AXIS2_PLACEMENT_3D('',#77616,#44336,#44337) ;
#35722 = AXIS2_PLACEMENT_3D('',#77617,#44338,#44339) ;
#35723 = AXIS2_PLACEMENT_3D('',#77618,#44340,#44341) ;
#35724 = AXIS2_PLACEMENT_3D('',#77619,#44342,#44343) ;
#35725 = AXIS2_PLACEMENT_3D('',#77662,#44344,#44345) ;
#35726 = AXIS2_PLACEMENT_3D('',#77663,#44346,#44347) ;
#35727 = AXIS2_PLACEMENT_3D('',#77664,#44348,#44349) ;
#35728 = AXIS2_PLACEMENT_3D('',#77665,#44350,#44351) ;
#35729 = AXIS2_PLACEMENT_3D('',#77667,#44352,#44353) ;
#35730 = AXIS2_PLACEMENT_3D('',#77669,#44355,#44356) ;
#35731 = AXIS2_PLACEMENT_3D('',#77671,#44357,#44358) ;
#35732 = AXIS2_PLACEMENT_3D('',#77672,#44359,#44360) ;
#35733 = AXIS2_PLACEMENT_3D('',#77673,#44361,#44362) ;
#35734 = AXIS2_PLACEMENT_3D('',#77675,#44363,#44364) ;
#35735 = AXIS2_PLACEMENT_3D('',#77677,#44365,#44366) ;
#35736 = AXIS2_PLACEMENT_3D('',#77695,#44368,#44369) ;
#35737 = AXIS2_PLACEMENT_3D('',#77696,#44370,#44371) ;
#35738 = AXIS2_PLACEMENT_3D('',#77697,#44372,#44373) ;
#35739 = AXIS2_PLACEMENT_3D('',#77698,#44374,#44375) ;
#35740 = AXIS2_PLACEMENT_3D('',#77699,#44376,#44377) ;
#35741 = AXIS2_PLACEMENT_3D('',#77700,#44378,#44379) ;
#35742 = AXIS2_PLACEMENT_3D('',#77702,#44380,#44381) ;
#35743 = AXIS2_PLACEMENT_3D('',#77704,#44382,#44383) ;
#35744 = AXIS2_PLACEMENT_3D('',#77705,#44384,#44385) ;
#35745 = AXIS2_PLACEMENT_3D('',#77706,#44386,#44387) ;
#35746 = AXIS2_PLACEMENT_3D('',#77709,#44389,#44390) ;
#35747 = AXIS2_PLACEMENT_3D('',#77711,#44392,#44393) ;
#35748 = AXIS2_PLACEMENT_3D('',#77712,#44394,#44395) ;
#35749 = AXIS2_PLACEMENT_3D('',#77718,#44399,#44400) ;
#35750 = AXIS2_PLACEMENT_3D('',#77719,#44401,#44402) ;
#35751 = AXIS2_PLACEMENT_3D('',#77720,#44403,#44404) ;
#35752 = AXIS2_PLACEMENT_3D('',#77721,#44405,#44406) ;
#35753 = AXIS2_PLACEMENT_3D('',#77722,#44407,#44408) ;
#35754 = AXIS2_PLACEMENT_3D('',#77723,#44409,#44410) ;
#35755 = AXIS2_PLACEMENT_3D('',#77741,#44411,#44412) ;
#35756 = AXIS2_PLACEMENT_3D('',#77742,#44413,#44414) ;
#35757 = AXIS2_PLACEMENT_3D('',#77743,#44415,#44416) ;
#35758 = AXIS2_PLACEMENT_3D('',#77745,#44418,#44419) ;
#35759 = AXIS2_PLACEMENT_3D('',#77779,#44421,#44422) ;
#35760 = AXIS2_PLACEMENT_3D('',#77784,#44425,#44426) ;
#35761 = AXIS2_PLACEMENT_3D('',#77811,#44427,#44428) ;
#35762 = AXIS2_PLACEMENT_3D('',#77813,#44429,#44430) ;
#35763 = AXIS2_PLACEMENT_3D('',#77815,#44431,#44432) ;
#35764 = AXIS2_PLACEMENT_3D('',#77817,#44433,#44434) ;
#35765 = AXIS2_PLACEMENT_3D('',#77823,#44437,#44438) ;
#35766 = AXIS2_PLACEMENT_3D('',#77825,#44439,#44440) ;
#35767 = AXIS2_PLACEMENT_3D('',#77826,#44441,#44442) ;
#35768 = AXIS2_PLACEMENT_3D('',#77849,#44443,#44444) ;
#35769 = AXIS2_PLACEMENT_3D('',#77850,#44445,#44446) ;
#35770 = AXIS2_PLACEMENT_3D('',#77851,#44447,#44448) ;
#35771 = AXIS2_PLACEMENT_3D('',#77875,#44450,#44451) ;
#35772 = AXIS2_PLACEMENT_3D('',#77877,#44453,#44454) ;
#35773 = AXIS2_PLACEMENT_3D('',#77879,#44455,#44456) ;
#35774 = AXIS2_PLACEMENT_3D('',#77880,#44457,#44458) ;
#35775 = AXIS2_PLACEMENT_3D('',#77881,#44459,#44460) ;
#35776 = AXIS2_PLACEMENT_3D('',#77887,#44464,#44465) ;
#35777 = AXIS2_PLACEMENT_3D('',#77890,#44467,#44468) ;
#35778 = AXIS2_PLACEMENT_3D('',#77891,#44469,#44470) ;
#35779 = AXIS2_PLACEMENT_3D('',#77893,#44471,#44472) ;
#35780 = AXIS2_PLACEMENT_3D('',#77906,#44473,#44474) ;
#35781 = AXIS2_PLACEMENT_3D('',#77907,#44475,#44476) ;
#35782 = AXIS2_PLACEMENT_3D('',#77910,#44477,#44478) ;
#35783 = AXIS2_PLACEMENT_3D('',#77912,#44479,#44480) ;
#35784 = AXIS2_PLACEMENT_3D('',#77913,#44481,#44482) ;
#35785 = AXIS2_PLACEMENT_3D('',#77936,#44483,#44484) ;
#35786 = AXIS2_PLACEMENT_3D('',#77960,#44487,#44488) ;
#35787 = AXIS2_PLACEMENT_3D('',#77961,#44489,#44490) ;
#35788 = AXIS2_PLACEMENT_3D('',#77962,#44491,#44492) ;
#35789 = AXIS2_PLACEMENT_3D('',#78004,#44493,#44494) ;
#35790 = AXIS2_PLACEMENT_3D('',#78008,#44496,#44497) ;
#35791 = AXIS2_PLACEMENT_3D('',#78010,#44499,#44500) ;
#35792 = AXIS2_PLACEMENT_3D('',#78014,#44503,#44504) ;
#35793 = AXIS2_PLACEMENT_3D('',#78017,#44506,#44507) ;
#35794 = AXIS2_PLACEMENT_3D('',#78018,#44508,#44509) ;
#35795 = AXIS2_PLACEMENT_3D('',#78023,#44513,#44514) ;
#35796 = AXIS2_PLACEMENT_3D('',#78026,#44515,#44516) ;
#35797 = AXIS2_PLACEMENT_3D('',#78030,#44518,#44519) ;
#35798 = AXIS2_PLACEMENT_3D('',#78049,#44521,#44522) ;
#35799 = AXIS2_PLACEMENT_3D('',#78050,#44523,#44524) ;
#35800 = AXIS2_PLACEMENT_3D('',#78076,#44525,#44526) ;
#35801 = AXIS2_PLACEMENT_3D('',#78078,#44527,#44528) ;
#35802 = AXIS2_PLACEMENT_3D('',#78079,#44529,#44530) ;
#35803 = AXIS2_PLACEMENT_3D('',#78080,#44531,#44532) ;
#35804 = AXIS2_PLACEMENT_3D('',#78081,#44533,#44534) ;
#35805 = AXIS2_PLACEMENT_3D('',#78083,#44535,#44536) ;
#35806 = AXIS2_PLACEMENT_3D('',#78085,#44538,#44539) ;
#35807 = AXIS2_PLACEMENT_3D('',#78087,#44540,#44541) ;
#35808 = AXIS2_PLACEMENT_3D('',#78088,#44542,#44543) ;
#35809 = AXIS2_PLACEMENT_3D('',#78089,#44544,#44545) ;
#35810 = AXIS2_PLACEMENT_3D('',#78090,#44546,#44547) ;
#35811 = AXIS2_PLACEMENT_3D('',#78091,#44548,#44549) ;
#35812 = AXIS2_PLACEMENT_3D('',#78094,#44552,#44553) ;
#35813 = AXIS2_PLACEMENT_3D('',#78097,#44555,#44556) ;
#35814 = AXIS2_PLACEMENT_3D('',#78099,#44558,#44559) ;
#35815 = AXIS2_PLACEMENT_3D('',#78103,#44562,#44563) ;
#35816 = AXIS2_PLACEMENT_3D('',#78104,#44564,#44565) ;
#35817 = AXIS2_PLACEMENT_3D('',#78105,#44566,#44567) ;
#35818 = AXIS2_PLACEMENT_3D('',#78106,#44568,#44569) ;
#35819 = AXIS2_PLACEMENT_3D('',#78107,#44570,#44571) ;
#35820 = AXIS2_PLACEMENT_3D('',#78124,#44572,#44573) ;
#35821 = AXIS2_PLACEMENT_3D('',#78125,#44574,#44575) ;
#35822 = AXIS2_PLACEMENT_3D('',#78126,#44576,#44577) ;
#35823 = AXIS2_PLACEMENT_3D('',#78127,#44578,#44579) ;
#35824 = AXIS2_PLACEMENT_3D('',#78153,#44580,#44581) ;
#35825 = AXIS2_PLACEMENT_3D('',#78154,#44582,#44583) ;
#35826 = AXIS2_PLACEMENT_3D('',#78155,#44584,#44585) ;
#35827 = AXIS2_PLACEMENT_3D('',#78157,#44586,#44587) ;
#35828 = AXIS2_PLACEMENT_3D('',#78159,#44589,#44590) ;
#35829 = AXIS2_PLACEMENT_3D('',#78161,#44591,#44592) ;
#35830 = AXIS2_PLACEMENT_3D('',#78162,#44593,#44594) ;
#35831 = AXIS2_PLACEMENT_3D('',#78163,#44595,#44596) ;
#35832 = AXIS2_PLACEMENT_3D('',#78165,#44597,#44598) ;
#35833 = AXIS2_PLACEMENT_3D('',#78167,#44599,#44600) ;
#35834 = AXIS2_PLACEMENT_3D('',#78185,#44602,#44603) ;
#35835 = AXIS2_PLACEMENT_3D('',#78186,#44604,#44605) ;
#35836 = AXIS2_PLACEMENT_3D('',#78187,#44606,#44607) ;
#35837 = AXIS2_PLACEMENT_3D('',#78188,#44608,#44609) ;
#35838 = AXIS2_PLACEMENT_3D('',#78189,#44610,#44611) ;
#35839 = AXIS2_PLACEMENT_3D('',#78190,#44612,#44613) ;
#35840 = AXIS2_PLACEMENT_3D('',#78192,#44614,#44615) ;
#35841 = AXIS2_PLACEMENT_3D('',#78194,#44616,#44617) ;
#35842 = AXIS2_PLACEMENT_3D('',#78195,#44618,#44619) ;
#35843 = AXIS2_PLACEMENT_3D('',#78196,#44620,#44621) ;
#35844 = AXIS2_PLACEMENT_3D('',#78204,#44623,#44624) ;
#35845 = AXIS2_PLACEMENT_3D('',#78210,#44628,#44629) ;
#35846 = AXIS2_PLACEMENT_3D('',#78211,#44630,#44631) ;
#35847 = AXIS2_PLACEMENT_3D('',#78212,#44632,#44633) ;
#35848 = AXIS2_PLACEMENT_3D('',#78213,#44634,#44635) ;
#35849 = AXIS2_PLACEMENT_3D('',#78214,#44636,#44637) ;
#35850 = AXIS2_PLACEMENT_3D('',#78215,#44638,#44639) ;
#35851 = AXIS2_PLACEMENT_3D('',#78233,#44640,#44641) ;
#35852 = AXIS2_PLACEMENT_3D('',#78234,#44642,#44643) ;
#35853 = AXIS2_PLACEMENT_3D('',#78235,#44644,#44645) ;
#35854 = AXIS2_PLACEMENT_3D('',#78237,#44647,#44648) ;
#35855 = AXIS2_PLACEMENT_3D('',#78239,#44650,#44651) ;
#35856 = AXIS2_PLACEMENT_3D('',#78240,#44652,#44653) ;
#35857 = AXIS2_PLACEMENT_3D('',#78241,#44654,#44655) ;
#35858 = AXIS2_PLACEMENT_3D('',#78242,#44656,#44657) ;
#35859 = AXIS2_PLACEMENT_3D('',#78243,#44658,#44659) ;
#35860 = AXIS2_PLACEMENT_3D('',#78244,#44660,#44661) ;
#35861 = AXIS2_PLACEMENT_3D('',#78245,#44662,#44663) ;
#35862 = AXIS2_PLACEMENT_3D('',#78246,#44664,#44665) ;
#35863 = AXIS2_PLACEMENT_3D('',#78247,#44666,#44667) ;
#35864 = AXIS2_PLACEMENT_3D('',#78248,#44668,#44669) ;
#35865 = AXIS2_PLACEMENT_3D('',#78249,#44670,#44671) ;
#35866 = AXIS2_PLACEMENT_3D('',#78250,#44672,#44673) ;
#35867 = AXIS2_PLACEMENT_3D('',#78251,#44674,#44675) ;
#35868 = AXIS2_PLACEMENT_3D('',#78252,#44676,#44677) ;
#35869 = AXIS2_PLACEMENT_3D('',#78254,#44678,#44679) ;
#35870 = AXIS2_PLACEMENT_3D('',#78255,#44680,#44681) ;
#35871 = AXIS2_PLACEMENT_3D('',#78284,#44682,#44683) ;
#35872 = AXIS2_PLACEMENT_3D('',#78285,#44684,#44685) ;
#35873 = AXIS2_PLACEMENT_3D('',#78286,#44686,#44687) ;
#35874 = AXIS2_PLACEMENT_3D('',#78287,#44688,#44689) ;
#35875 = AXIS2_PLACEMENT_3D('',#78288,#44690,#44691) ;
#35876 = AXIS2_PLACEMENT_3D('',#78289,#44692,#44693) ;
#35877 = AXIS2_PLACEMENT_3D('',#78292,#44695,#44696) ;
#35878 = AXIS2_PLACEMENT_3D('',#78321,#44697,#44698) ;
#35879 = AXIS2_PLACEMENT_3D('',#78322,#44699,#44700) ;
#35880 = AXIS2_PLACEMENT_3D('',#78323,#44701,#44702) ;
#35881 = AXIS2_PLACEMENT_3D('',#78324,#44703,#44704) ;
#35882 = AXIS2_PLACEMENT_3D('',#78325,#44705,#44706) ;
#35883 = AXIS2_PLACEMENT_3D('',#78357,#44707,#44708) ;
#35884 = AXIS2_PLACEMENT_3D('',#78374,#44709,#44710) ;
#35885 = AXIS2_PLACEMENT_3D('',#78375,#44711,#44712) ;
#35886 = AXIS2_PLACEMENT_3D('',#78376,#44713,#44714) ;
#35887 = AXIS2_PLACEMENT_3D('',#78377,#44715,#44716) ;
#35888 = AXIS2_PLACEMENT_3D('',#78378,#44717,#44718) ;
#35889 = AXIS2_PLACEMENT_3D('',#78379,#44719,#44720) ;
#35890 = AXIS2_PLACEMENT_3D('',#78411,#44721,#44722) ;
#35891 = AXIS2_PLACEMENT_3D('',#78428,#44723,#44724) ;
#35892 = AXIS2_PLACEMENT_3D('',#78430,#44726,#44727) ;
#35893 = AXIS2_PLACEMENT_3D('',#78431,#44728,#44729) ;
#35894 = AXIS2_PLACEMENT_3D('',#78432,#44730,#44731) ;
#35895 = AXIS2_PLACEMENT_3D('',#78433,#44732,#44733) ;
#35896 = AXIS2_PLACEMENT_3D('',#78434,#44734,#44735) ;
#35897 = AXIS2_PLACEMENT_3D('',#78435,#44736,#44737) ;
#35898 = AXIS2_PLACEMENT_3D('',#78459,#44739,#44740) ;
#35899 = AXIS2_PLACEMENT_3D('',#78484,#44741,#44742) ;
#35900 = AXIS2_PLACEMENT_3D('',#78485,#44743,#44744) ;
#35901 = AXIS2_PLACEMENT_3D('',#78486,#44745,#44746) ;
#35902 = AXIS2_PLACEMENT_3D('',#78777,#44747,#44748) ;
#35903 = AXIS2_PLACEMENT_3D('',#78778,#44749,#44750) ;
#35904 = AXIS2_PLACEMENT_3D('',#78779,#44751,#44752) ;
#35905 = AXIS2_PLACEMENT_3D('',#78780,#44753,#44754) ;
#35906 = AXIS2_PLACEMENT_3D('',#78781,#44755,#44756) ;
#35907 = AXIS2_PLACEMENT_3D('',#78782,#44757,#44758) ;
#35908 = AXIS2_PLACEMENT_3D('',#78783,#44759,#44760) ;
#35909 = AXIS2_PLACEMENT_3D('',#78784,#44761,#44762) ;
#35910 = AXIS2_PLACEMENT_3D('',#78785,#44763,#44764) ;
#35911 = AXIS2_PLACEMENT_3D('',#78786,#44765,#44766) ;
#35912 = AXIS2_PLACEMENT_3D('',#78787,#44767,#44768) ;
#35913 = AXIS2_PLACEMENT_3D('',#78788,#44769,#44770) ;
#35914 = AXIS2_PLACEMENT_3D('',#78810,#44772,#44773) ;
#35915 = AXIS2_PLACEMENT_3D('',#78831,#44774,#44775) ;
#35916 = AXIS2_PLACEMENT_3D('',#78907,#44777,#44778) ;
#35917 = AXIS2_PLACEMENT_3D('',#78983,#44780,#44781) ;
#35918 = AXIS2_PLACEMENT_3D('',#79003,#44783,#44784) ;
#35919 = AXIS2_PLACEMENT_3D('',#79022,#44785,#44786) ;
#35920 = AXIS2_PLACEMENT_3D('',#79038,#44788,#44789) ;
#35921 = AXIS2_PLACEMENT_3D('',#79065,#44790,#44791) ;
#35922 = AXIS2_PLACEMENT_3D('',#79141,#44793,#44794) ;
#35923 = AXIS2_PLACEMENT_3D('',#79217,#44796,#44797) ;
#35924 = AXIS2_PLACEMENT_3D('',#79231,#44799,#44800) ;
#35925 = AXIS2_PLACEMENT_3D('',#79256,#44801,#44802) ;
#35926 = AXIS2_PLACEMENT_3D('',#79329,#44803,#44804) ;
#35927 = AXIS2_PLACEMENT_3D('',#79402,#44805,#44806) ;
#35928 = AXIS2_PLACEMENT_3D('',#79405,#44807,#44808) ;
#35929 = AXIS2_PLACEMENT_3D('',#79409,#44810,#44811) ;
#35930 = AXIS2_PLACEMENT_3D('',#79411,#44813,#44814) ;
#35931 = AXIS2_PLACEMENT_3D('',#79414,#44815,#44816) ;
#35932 = AXIS2_PLACEMENT_3D('',#79416,#44817,#44818) ;
#35933 = AXIS2_PLACEMENT_3D('',#79418,#44819,#44820) ;
#35934 = AXIS2_PLACEMENT_3D('',#79419,#44821,#44822) ;
#35935 = AXIS2_PLACEMENT_3D('',#79420,#44823,#44824) ;
#35936 = AXIS2_PLACEMENT_3D('',#79423,#44825,#44826) ;
#35937 = AXIS2_PLACEMENT_3D('',#79426,#44829,#44830) ;
#35938 = AXIS2_PLACEMENT_3D('',#79429,#44831,#44832) ;
#35939 = AXIS2_PLACEMENT_3D('',#79431,#44833,#44834) ;
#35940 = AXIS2_PLACEMENT_3D('',#79433,#44835,#44836) ;
#35941 = AXIS2_PLACEMENT_3D('',#79434,#44837,#44838) ;
#35942 = AXIS2_PLACEMENT_3D('',#79435,#44839,#44840) ;
#35943 = AXIS2_PLACEMENT_3D('',#79438,#44841,#44842) ;
#35944 = AXIS2_PLACEMENT_3D('',#79440,#44843,#44844) ;
#35945 = AXIS2_PLACEMENT_3D('',#79442,#44845,#44846) ;
#35946 = AXIS2_PLACEMENT_3D('',#79443,#44847,#44848) ;
#35947 = AXIS2_PLACEMENT_3D('',#79444,#44849,#44850) ;
#35948 = AXIS2_PLACEMENT_3D('',#79447,#44851,#44852) ;
#35949 = AXIS2_PLACEMENT_3D('',#79450,#44855,#44856) ;
#35950 = AXIS2_PLACEMENT_3D('',#79453,#44857,#44858) ;
#35951 = AXIS2_PLACEMENT_3D('',#79454,#44859,#44860) ;
#35952 = AXIS2_PLACEMENT_3D('',#79455,#44861,#44862) ;
#35953 = AXIS2_PLACEMENT_3D('',#79456,#44863,#44864) ;
#35954 = AXIS2_PLACEMENT_3D('',#79459,#44867,#44868) ;
#35955 = AXIS2_PLACEMENT_3D('',#79461,#44869,#44870) ;
#35956 = AXIS2_PLACEMENT_3D('',#79464,#44873,#44874) ;
#35957 = AXIS2_PLACEMENT_3D('',#79467,#44875,#44876) ;
#35958 = AXIS2_PLACEMENT_3D('',#79469,#44877,#44878) ;
#35959 = AXIS2_PLACEMENT_3D('',#79471,#44879,#44880) ;
#35960 = AXIS2_PLACEMENT_3D('',#79472,#44881,#44882) ;
#35961 = AXIS2_PLACEMENT_3D('',#79473,#44883,#44884) ;
#35962 = AXIS2_PLACEMENT_3D('',#79475,#44885,#44886) ;
#35963 = AXIS2_PLACEMENT_3D('',#79478,#44889,#44890) ;
#35964 = AXIS2_PLACEMENT_3D('',#79481,#44891,#44892) ;
#35965 = AXIS2_PLACEMENT_3D('',#79484,#44895,#44896) ;
#35966 = AXIS2_PLACEMENT_3D('',#79487,#44897,#44898) ;
#35967 = AXIS2_PLACEMENT_3D('',#79488,#44899,#44900) ;
#35968 = AXIS2_PLACEMENT_3D('',#79489,#44901,#44902) ;
#35969 = AXIS2_PLACEMENT_3D('',#79490,#44903,#44904) ;
#35970 = AXIS2_PLACEMENT_3D('',#79493,#44907,#44908) ;
#35971 = AXIS2_PLACEMENT_3D('',#79496,#44911,#44912) ;
#35972 = AXIS2_PLACEMENT_3D('',#79499,#44913,#44914) ;
#35973 = AXIS2_PLACEMENT_3D('',#79502,#44917,#44918) ;
#35974 = AXIS2_PLACEMENT_3D('',#79505,#44921,#44922) ;
#35975 = AXIS2_PLACEMENT_3D('',#79506,#44923,#44924) ;
#35976 = AXIS2_PLACEMENT_3D('',#79507,#44925,#44926) ;
#35977 = AXIS2_PLACEMENT_3D('',#79508,#44927,#44928) ;
#35978 = AXIS2_PLACEMENT_3D('',#79509,#44929,#44930) ;
#35979 = AXIS2_PLACEMENT_3D('',#79511,#44931,#44932) ;
#35980 = AXIS2_PLACEMENT_3D('',#79514,#44934,#44935) ;
#35981 = AXIS2_PLACEMENT_3D('',#79516,#44937,#44938) ;
#35982 = AXIS2_PLACEMENT_3D('',#79517,#44939,#44940) ;
#35983 = AXIS2_PLACEMENT_3D('',#79518,#44941,#44942) ;
#35984 = AXIS2_PLACEMENT_3D('',#79519,#44943,#44944) ;
#35985 = AXIS2_PLACEMENT_3D('',#79520,#44945,#44946) ;
#35986 = AXIS2_PLACEMENT_3D('',#79522,#44948,#44949) ;
#35987 = AXIS2_PLACEMENT_3D('',#79526,#44951,#44952) ;
#35988 = AXIS2_PLACEMENT_3D('',#79528,#44954,#44955) ;
#35989 = AXIS2_PLACEMENT_3D('',#79542,#44958,#44959) ;
#35990 = AXIS2_PLACEMENT_3D('',#79545,#44961,#44962) ;
#35991 = AXIS2_PLACEMENT_3D('',#79546,#44963,#44964) ;
#35992 = AXIS2_PLACEMENT_3D('',#79550,#44967,#44968) ;
#35993 = AXIS2_PLACEMENT_3D('',#79551,#44969,#44970) ;
#35994 = AXIS2_PLACEMENT_3D('',#79552,#44971,#44972) ;
#35995 = AXIS2_PLACEMENT_3D('',#79554,#44974,#44975) ;
#35996 = AXIS2_PLACEMENT_3D('',#79555,#44976,#44977) ;
#35997 = AXIS2_PLACEMENT_3D('',#79558,#44979,#44980) ;
#35998 = AXIS2_PLACEMENT_3D('',#79559,#44981,#44982) ;
#35999 = AXIS2_PLACEMENT_3D('',#79563,#44984,#44985) ;
#36000 = AXIS2_PLACEMENT_3D('',#79565,#44987,#44988) ;
#36001 = AXIS2_PLACEMENT_3D('',#79567,#44989,#44990) ;
#36002 = AXIS2_PLACEMENT_3D('',#79578,#44996,#44997) ;
#36003 = AXIS2_PLACEMENT_3D('',#79579,#44998,#44999) ;
#36004 = AXIS2_PLACEMENT_3D('',#79581,#45001,#45002) ;
#36005 = AXIS2_PLACEMENT_3D('',#79600,#45007,#45008) ;
#36006 = AXIS2_PLACEMENT_3D('',#79609,#45013,#45014) ;
#36007 = AXIS2_PLACEMENT_3D('',#79616,#45017,#45018) ;
#36008 = AXIS2_PLACEMENT_3D('',#79628,#45024,#45025) ;
#36009 = AXIS2_PLACEMENT_3D('',#79630,#45027,#45028) ;
#36010 = AXIS2_PLACEMENT_3D('',#79661,#45033,#45034) ;
#36011 = AXIS2_PLACEMENT_3D('',#79662,#45035,#45036) ;
#36012 = AXIS2_PLACEMENT_3D('',#79663,#45037,#45038) ;
#36013 = AXIS2_PLACEMENT_3D('',#79664,#45039,#45040) ;
#36014 = AXIS2_PLACEMENT_3D('',#79665,#45041,#45042) ;
#36015 = AXIS2_PLACEMENT_3D('',#79666,#45043,#45044) ;
#36016 = AXIS2_PLACEMENT_3D('',#79667,#45045,#45046) ;
#36017 = AXIS2_PLACEMENT_3D('',#79695,#45048,#45049) ;
#36018 = AXIS2_PLACEMENT_3D('',#79723,#45051,#45052) ;
#36019 = AXIS2_PLACEMENT_3D('',#79732,#45057,#45058) ;
#36020 = AXIS2_PLACEMENT_3D('',#79733,#45059,#45060) ;
#36021 = AXIS2_PLACEMENT_3D('',#79734,#45061,#45062) ;
#36022 = AXIS2_PLACEMENT_3D('',#79735,#45063,#45064) ;
#36023 = AXIS2_PLACEMENT_3D('',#79742,#45067,#45068) ;
#36024 = AXIS2_PLACEMENT_3D('',#79746,#45070,#45071) ;
#36025 = AXIS2_PLACEMENT_3D('',#79748,#45073,#45074) ;
#36026 = AXIS2_PLACEMENT_3D('',#79753,#45076,#45077) ;
#36027 = AXIS2_PLACEMENT_3D('',#79757,#45079,#45080) ;
#36028 = AXIS2_PLACEMENT_3D('',#79761,#45083,#45084) ;
#36029 = AXIS2_PLACEMENT_3D('',#79763,#45085,#45086) ;
#36030 = AXIS2_PLACEMENT_3D('',#79766,#45088,#45089) ;
#36031 = AXIS2_PLACEMENT_3D('',#79767,#45090,#45091) ;
#36032 = AXIS2_PLACEMENT_3D('',#79773,#45095,#45096) ;
#36033 = AXIS2_PLACEMENT_3D('',#79775,#45097,#45098) ;
#36034 = AXIS2_PLACEMENT_3D('',#79776,#45099,#45100) ;
#36035 = AXIS2_PLACEMENT_3D('',#79777,#45101,#45102) ;
#36036 = AXIS2_PLACEMENT_3D('',#79779,#45103,#45104) ;
#36037 = AXIS2_PLACEMENT_3D('',#79780,#45105,#45106) ;
#36038 = AXIS2_PLACEMENT_3D('',#79781,#45107,#45108) ;
#36039 = AXIS2_PLACEMENT_3D('',#79783,#45109,#45110) ;
#36040 = AXIS2_PLACEMENT_3D('',#79784,#45111,#45112) ;
#36041 = AXIS2_PLACEMENT_3D('',#79785,#45113,#45114) ;
#36042 = AXIS2_PLACEMENT_3D('',#79786,#45115,#45116) ;
#36043 = AXIS2_PLACEMENT_3D('',#79787,#45117,#45118) ;
#36044 = AXIS2_PLACEMENT_3D('',#79788,#45119,#45120) ;
#36045 = AXIS2_PLACEMENT_3D('',#79790,#45121,#45122) ;
#36046 = AXIS2_PLACEMENT_3D('',#79791,#45123,#45124) ;
#36047 = AXIS2_PLACEMENT_3D('',#79792,#45125,#45126) ;
#36048 = AXIS2_PLACEMENT_3D('',#79793,#45127,#45128) ;
#36049 = AXIS2_PLACEMENT_3D('',#79794,#45129,#45130) ;
#36050 = AXIS2_PLACEMENT_3D('',#79795,#45131,#45132) ;
#36051 = AXIS2_PLACEMENT_3D('',#79796,#45133,#45134) ;
#36052 = AXIS2_PLACEMENT_3D('',#79798,#45135,#45136) ;
#36053 = AXIS2_PLACEMENT_3D('',#79800,#45138,#45139) ;
#36054 = AXIS2_PLACEMENT_3D('',#79803,#45141,#45142) ;
#36055 = AXIS2_PLACEMENT_3D('',#79804,#45143,#45144) ;
#36056 = AXIS2_PLACEMENT_3D('',#79806,#45145,#45146) ;
#36057 = AXIS2_PLACEMENT_3D('',#79808,#45148,#45149) ;
#36058 = AXIS2_PLACEMENT_3D('',#79809,#45150,#45151) ;
#36059 = AXIS2_PLACEMENT_3D('',#79810,#45152,#45153) ;
#36060 = AXIS2_PLACEMENT_3D('',#79813,#45155,#45156) ;
#36061 = AXIS2_PLACEMENT_3D('',#79814,#45157,#45158) ;
#36062 = AXIS2_PLACEMENT_3D('',#79815,#45159,#45160) ;
#36063 = AXIS2_PLACEMENT_3D('',#79816,#45161,#45162) ;
#36064 = AXIS2_PLACEMENT_3D('',#79817,#45163,#45164) ;
#36065 = AXIS2_PLACEMENT_3D('',#79818,#45165,#45166) ;
#36066 = AXIS2_PLACEMENT_3D('',#79819,#45167,#45168) ;
#36067 = AXIS2_PLACEMENT_3D('',#79820,#45169,#45170) ;
#36068 = AXIS2_PLACEMENT_3D('',#79821,#45171,#45172) ;
#36069 = AXIS2_PLACEMENT_3D('',#79822,#45173,#45174) ;
#36070 = AXIS2_PLACEMENT_3D('',#79823,#45175,#45176) ;
#36071 = AXIS2_PLACEMENT_3D('',#79824,#45177,#45178) ;
#36072 = AXIS2_PLACEMENT_3D('',#79825,#45179,#45180) ;
#36073 = AXIS2_PLACEMENT_3D('',#79827,#45181,#45182) ;
#36074 = AXIS2_PLACEMENT_3D('',#79829,#45184,#45185) ;
#36075 = AXIS2_PLACEMENT_3D('',#79830,#45186,#45187) ;
#36076 = AXIS2_PLACEMENT_3D('',#79831,#45188,#45189) ;
#36077 = AXIS2_PLACEMENT_3D('',#79834,#45191,#45192) ;
#36078 = AXIS2_PLACEMENT_3D('',#79835,#45193,#45194) ;
#36079 = AXIS2_PLACEMENT_3D('',#79836,#45195,#45196) ;
#36080 = AXIS2_PLACEMENT_3D('',#79837,#45197,#45198) ;
#36081 = AXIS2_PLACEMENT_3D('',#79838,#45199,#45200) ;
#36082 = AXIS2_PLACEMENT_3D('',#79839,#45201,#45202) ;
#36083 = AXIS2_PLACEMENT_3D('',#79840,#45203,#45204) ;
#36084 = AXIS2_PLACEMENT_3D('',#79841,#45205,#45206) ;
#36085 = AXIS2_PLACEMENT_3D('',#79842,#45207,#45208) ;
#36086 = AXIS2_PLACEMENT_3D('',#79843,#45209,#45210) ;
#36087 = AXIS2_PLACEMENT_3D('',#79844,#45211,#45212) ;
#36088 = AXIS2_PLACEMENT_3D('',#79845,#45213,#45214) ;
#36089 = AXIS2_PLACEMENT_3D('',#79846,#45215,#45216) ;
#36090 = AXIS2_PLACEMENT_3D('',#79849,#45218,#45219) ;
#36091 = AXIS2_PLACEMENT_3D('',#79850,#45220,#45221) ;
#36092 = AXIS2_PLACEMENT_3D('',#79851,#45222,#45223) ;
#36093 = AXIS2_PLACEMENT_3D('',#79852,#45224,#45225) ;
#36094 = AXIS2_PLACEMENT_3D('',#79853,#45226,#45227) ;
#36095 = AXIS2_PLACEMENT_3D('',#79854,#45228,#45229) ;
#36096 = AXIS2_PLACEMENT_3D('',#79855,#45230,#45231) ;
#36097 = AXIS2_PLACEMENT_3D('',#79856,#45232,#45233) ;
#36098 = AXIS2_PLACEMENT_3D('',#79857,#45234,#45235) ;
#36099 = AXIS2_PLACEMENT_3D('',#79858,#45236,#45237) ;
#36100 = AXIS2_PLACEMENT_3D('',#79859,#45238,#45239) ;
#36101 = AXIS2_PLACEMENT_3D('',#79860,#45240,#45241) ;
#36102 = AXIS2_PLACEMENT_3D('',#79861,#45242,#45243) ;
#36103 = AXIS2_PLACEMENT_3D('',#79862,#45244,#45245) ;
#36104 = AXIS2_PLACEMENT_3D('',#79863,#45246,#45247) ;
#36105 = AXIS2_PLACEMENT_3D('',#79864,#45248,#45249) ;
#36106 = AXIS2_PLACEMENT_3D('',#79865,#45250,#45251) ;
#36107 = AXIS2_PLACEMENT_3D('',#79867,#45252,#45253) ;
#36108 = AXIS2_PLACEMENT_3D('',#79869,#45255,#45256) ;
#36109 = AXIS2_PLACEMENT_3D('',#79870,#45257,#45258) ;
#36110 = AXIS2_PLACEMENT_3D('',#79872,#45260,#45261) ;
#36111 = AXIS2_PLACEMENT_3D('',#79873,#45262,#45263) ;
#36112 = AXIS2_PLACEMENT_3D('',#79874,#45264,#45265) ;
#36113 = AXIS2_PLACEMENT_3D('',#79875,#45266,#45267) ;
#36114 = AXIS2_PLACEMENT_3D('',#79877,#45269,#45270) ;
#36115 = AXIS2_PLACEMENT_3D('',#79878,#45271,#45272) ;
#36116 = AXIS2_PLACEMENT_3D('',#79879,#45273,#45274) ;
#36117 = AXIS2_PLACEMENT_3D('',#79880,#45275,#45276) ;
#36118 = AXIS2_PLACEMENT_3D('',#79881,#45277,#45278) ;
#36119 = AXIS2_PLACEMENT_3D('',#79882,#45279,#45280) ;
#36120 = AXIS2_PLACEMENT_3D('',#79883,#45281,#45282) ;
#36121 = AXIS2_PLACEMENT_3D('',#79884,#45283,#45284) ;
#36122 = AXIS2_PLACEMENT_3D('',#79885,#45285,#45286) ;
#36123 = AXIS2_PLACEMENT_3D('',#79887,#45287,#45288) ;
#36124 = AXIS2_PLACEMENT_3D('',#79889,#45289,#45290) ;
#36125 = AXIS2_PLACEMENT_3D('',#79890,#45291,#45292) ;
#36126 = AXIS2_PLACEMENT_3D('',#79891,#45293,#45294) ;
#36127 = AXIS2_PLACEMENT_3D('',#79893,#45295,#45296) ;
#36128 = AXIS2_PLACEMENT_3D('',#79894,#45297,#45298) ;
#36129 = AXIS2_PLACEMENT_3D('',#79897,#45299,#45300) ;
#36130 = AXIS2_PLACEMENT_3D('',#79898,#45301,#45302) ;
#36131 = AXIS2_PLACEMENT_3D('',#79900,#45304,#45305) ;
#36132 = AXIS2_PLACEMENT_3D('',#79901,#45306,#45307) ;
#36133 = AXIS2_PLACEMENT_3D('',#79902,#45308,#45309) ;
#36134 = AXIS2_PLACEMENT_3D('',#80793,#45310,#45311) ;
#36135 = AXIS2_PLACEMENT_3D('',#80794,#45312,#45313) ;
#36136 = AXIS2_PLACEMENT_3D('',#80795,#45314,#45315) ;
#36137 = AXIS2_PLACEMENT_3D('',#80796,#45316,#45317) ;
#36138 = AXIS2_PLACEMENT_3D('',#80797,#45318,#45319) ;
#36139 = AXIS2_PLACEMENT_3D('',#80798,#45320,#45321) ;
#36140 = AXIS2_PLACEMENT_3D('',#80799,#45322,#45323) ;
#36141 = AXIS2_PLACEMENT_3D('',#80800,#45324,#45325) ;
#36142 = AXIS2_PLACEMENT_3D('',#80801,#45326,#45327) ;
#36143 = AXIS2_PLACEMENT_3D('',#80802,#45328,#45329) ;
#36144 = AXIS2_PLACEMENT_3D('',#80803,#45330,#45331) ;
#36145 = AXIS2_PLACEMENT_3D('',#80840,#45332,#45333) ;
#36146 = AXIS2_PLACEMENT_3D('',#80846,#45334,#45335) ;
#36147 = AXIS2_PLACEMENT_3D('',#80883,#45336,#45337) ;
#36148 = AXIS2_PLACEMENT_3D('',#80891,#45338,#45339) ;
#36149 = AXIS2_PLACEMENT_3D('',#80920,#45340,#45341) ;
#36150 = AXIS2_PLACEMENT_3D('',#80928,#45342,#45343) ;
#36151 = AXIS2_PLACEMENT_3D('',#80965,#45344,#45345) ;
#36152 = AXIS2_PLACEMENT_3D('',#80973,#45346,#45347) ;
#36153 = AXIS2_PLACEMENT_3D('',#81010,#45348,#45349) ;
#36154 = AXIS2_PLACEMENT_3D('',#81018,#45350,#45351) ;
#36155 = AXIS2_PLACEMENT_3D('',#81019,#45352,#45353) ;
#36156 = AXIS2_PLACEMENT_3D('',#81021,#45354,#45355) ;
#36157 = AXIS2_PLACEMENT_3D('',#81024,#45357,#45358) ;
#36158 = AXIS2_PLACEMENT_3D('',#81025,#45359,#45360) ;
#36159 = AXIS2_PLACEMENT_3D('',#81031,#45363,#45364) ;
#36160 = AXIS2_PLACEMENT_3D('',#81040,#45369,#45370) ;
#36161 = AXIS2_PLACEMENT_3D('',#81049,#45375,#45376) ;
#36162 = AXIS2_PLACEMENT_3D('',#81058,#45381,#45382) ;
#36163 = AXIS2_PLACEMENT_3D('',#81062,#45385,#45386) ;
#36164 = AXIS2_PLACEMENT_3D('',#81070,#45390,#45391) ;
#36165 = AXIS2_PLACEMENT_3D('',#81071,#45392,#45393) ;
#36166 = AXIS2_PLACEMENT_3D('',#81078,#45396,#45397) ;
#36167 = AXIS2_PLACEMENT_3D('',#81080,#45399,#45400) ;
#36168 = AXIS2_PLACEMENT_3D('',#81088,#45404,#45405) ;
#36169 = AXIS2_PLACEMENT_3D('',#81089,#45406,#45407) ;
#36170 = AXIS2_PLACEMENT_3D('',#81096,#45410,#45411) ;
#36171 = AXIS2_PLACEMENT_3D('',#81098,#45413,#45414) ;
#36172 = AXIS2_PLACEMENT_3D('',#81100,#45415,#45416) ;
#36173 = AXIS2_PLACEMENT_3D('',#81102,#45417,#45418) ;
#36174 = AXIS2_PLACEMENT_3D('',#81103,#45419,#45420) ;
#36175 = AXIS2_PLACEMENT_3D('',#81104,#45421,#45422) ;
#36176 = AXIS2_PLACEMENT_3D('',#81107,#45424,#45425) ;
#36177 = AXIS2_PLACEMENT_3D('',#81108,#45426,#45427) ;
#36178 = AXIS2_PLACEMENT_3D('',#81110,#45428,#45429) ;
#36179 = AXIS2_PLACEMENT_3D('',#81112,#45431,#45432) ;
#36180 = AXIS2_PLACEMENT_3D('',#81114,#45433,#45434) ;
#36181 = AXIS2_PLACEMENT_3D('',#81116,#45435,#45436) ;
#36182 = AXIS2_PLACEMENT_3D('',#81117,#45437,#45438) ;
#36183 = AXIS2_PLACEMENT_3D('',#81118,#45439,#45440) ;
#36184 = AXIS2_PLACEMENT_3D('',#81121,#45442,#45443) ;
#36185 = AXIS2_PLACEMENT_3D('',#81122,#45444,#45445) ;
#36186 = AXIS2_PLACEMENT_3D('',#81124,#45446,#45447) ;
#36187 = AXIS2_PLACEMENT_3D('',#81126,#45449,#45450) ;
#36188 = AXIS2_PLACEMENT_3D('',#81128,#45451,#45452) ;
#36189 = AXIS2_PLACEMENT_3D('',#81130,#45453,#45454) ;
#36190 = AXIS2_PLACEMENT_3D('',#81131,#45455,#45456) ;
#36191 = AXIS2_PLACEMENT_3D('',#81132,#45457,#45458) ;
#36192 = AXIS2_PLACEMENT_3D('',#81135,#45460,#45461) ;
#36193 = AXIS2_PLACEMENT_3D('',#81136,#45462,#45463) ;
#36194 = AXIS2_PLACEMENT_3D('',#81138,#45464,#45465) ;
#36195 = AXIS2_PLACEMENT_3D('',#81140,#45467,#45468) ;
#36196 = AXIS2_PLACEMENT_3D('',#81146,#45472,#45473) ;
#36197 = AXIS2_PLACEMENT_3D('',#81152,#45477,#45478) ;
#36198 = AXIS2_PLACEMENT_3D('',#81153,#45479,#45480) ;
#36199 = AXIS2_PLACEMENT_3D('',#81154,#45481,#45482) ;
#36200 = AXIS2_PLACEMENT_3D('',#81155,#45483,#45484) ;
#36201 = AXIS2_PLACEMENT_3D('',#81156,#45485,#45486) ;
#36202 = AXIS2_PLACEMENT_3D('',#81157,#45487,#45488) ;
#36203 = AXIS2_PLACEMENT_3D('',#81158,#45489,#45490) ;
#36204 = AXIS2_PLACEMENT_3D('',#81159,#45491,#45492) ;
#36205 = AXIS2_PLACEMENT_3D('',#81160,#45493,#45494) ;
#36206 = AXIS2_PLACEMENT_3D('',#81161,#45495,#45496) ;
#36207 = AXIS2_PLACEMENT_3D('',#81170,#45501,#45502) ;
#36208 = AXIS2_PLACEMENT_3D('',#81179,#45507,#45508) ;
#36209 = AXIS2_PLACEMENT_3D('',#81180,#45509,#45510) ;
#36210 = AXIS2_PLACEMENT_3D('',#81181,#45511,#45512) ;
#36211 = AXIS2_PLACEMENT_3D('',#81182,#45513,#45514) ;
#36212 = AXIS2_PLACEMENT_3D('',#81183,#45515,#45516) ;
#36213 = AXIS2_PLACEMENT_3D('',#81184,#45517,#45518) ;
#36214 = AXIS2_PLACEMENT_3D('',#81185,#45519,#45520) ;
#36215 = AXIS2_PLACEMENT_3D('',#81186,#45521,#45522) ;
#36216 = AXIS2_PLACEMENT_3D('',#81187,#45523,#45524) ;
#36217 = AXIS2_PLACEMENT_3D('',#81193,#45528,#45529) ;
#36218 = AXIS2_PLACEMENT_3D('',#81199,#45533,#45534) ;
#36219 = AXIS2_PLACEMENT_3D('',#81200,#45535,#45536) ;
#36220 = AXIS2_PLACEMENT_3D('',#81201,#45537,#45538) ;
#36221 = AXIS2_PLACEMENT_3D('',#81202,#45539,#45540) ;
#36222 = AXIS2_PLACEMENT_3D('',#81203,#45541,#45542) ;
#36223 = AXIS2_PLACEMENT_3D('',#81204,#45543,#45544) ;
#36224 = AXIS2_PLACEMENT_3D('',#81205,#45545,#45546) ;
#36225 = AXIS2_PLACEMENT_3D('',#81206,#45547,#45548) ;
#36226 = AXIS2_PLACEMENT_3D('',#81207,#45549,#45550) ;
#36227 = AXIS2_PLACEMENT_3D('',#81208,#45551,#45552) ;
#36228 = AXIS2_PLACEMENT_3D('',#81214,#45556,#45557) ;
#36229 = AXIS2_PLACEMENT_3D('',#81220,#45561,#45562) ;
#36230 = AXIS2_PLACEMENT_3D('',#81221,#45563,#45564) ;
#36231 = AXIS2_PLACEMENT_3D('',#81222,#45565,#45566) ;
#36232 = AXIS2_PLACEMENT_3D('',#81223,#45567,#45568) ;
#36233 = AXIS2_PLACEMENT_3D('',#81224,#45569,#45570) ;
#36234 = AXIS2_PLACEMENT_3D('',#81225,#45571,#45572) ;
#36235 = AXIS2_PLACEMENT_3D('',#81226,#45573,#45574) ;
#36236 = AXIS2_PLACEMENT_3D('',#81227,#45575,#45576) ;
#36237 = AXIS2_PLACEMENT_3D('',#81228,#45577,#45578) ;
#36238 = AXIS2_PLACEMENT_3D('',#81229,#45579,#45580) ;
#36239 = AXIS2_PLACEMENT_3D('',#81230,#45581,#45582) ;
#36240 = AXIS2_PLACEMENT_3D('',#81231,#45583,#45584) ;
#36241 = AXIS2_PLACEMENT_3D('',#81232,#45585,#45586) ;
#36242 = AXIS2_PLACEMENT_3D('',#81233,#45587,#45588) ;
#36243 = AXIS2_PLACEMENT_3D('',#81234,#45589,#45590) ;
#36244 = AXIS2_PLACEMENT_3D('',#81235,#45591,#45592) ;
#36245 = AXIS2_PLACEMENT_3D('',#81236,#45593,#45594) ;
#36246 = AXIS2_PLACEMENT_3D('',#81237,#45595,#45596) ;
#36247 = AXIS2_PLACEMENT_3D('',#81238,#45597,#45598) ;
#36248 = AXIS2_PLACEMENT_3D('',#81241,#45599,#45600) ;
#36249 = AXIS2_PLACEMENT_3D('',#81247,#45604,#45605) ;
#36250 = AXIS2_PLACEMENT_3D('',#81254,#45609,#45610) ;
#36251 = AXIS2_PLACEMENT_3D('',#81263,#45615,#45616) ;
#36252 = AXIS2_PLACEMENT_3D('',#81264,#45617,#45618) ;
#36253 = AXIS2_PLACEMENT_3D('',#81265,#45619,#45620) ;
#36254 = AXIS2_PLACEMENT_3D('',#81266,#45621,#45622) ;
#36255 = AXIS2_PLACEMENT_3D('',#81267,#45623,#45624) ;
#36256 = AXIS2_PLACEMENT_3D('',#81268,#45625,#45626) ;
#36257 = AXIS2_PLACEMENT_3D('',#81269,#45627,#45628) ;
#36258 = AXIS2_PLACEMENT_3D('',#81270,#45629,#45630) ;
#36259 = AXIS2_PLACEMENT_3D('',#81271,#45631,#45632) ;
#36260 = AXIS2_PLACEMENT_3D('',#81272,#45633,#45634) ;
#36261 = AXIS2_PLACEMENT_3D('',#81273,#45635,#45636) ;
#36262 = AXIS2_PLACEMENT_3D('',#81276,#45637,#45638) ;
#36263 = AXIS2_PLACEMENT_3D('',#81282,#45642,#45643) ;
#36264 = AXIS2_PLACEMENT_3D('',#81289,#45647,#45648) ;
#36265 = AXIS2_PLACEMENT_3D('',#81298,#45653,#45654) ;
#36266 = AXIS2_PLACEMENT_3D('',#81299,#45655,#45656) ;
#36267 = AXIS2_PLACEMENT_3D('',#81300,#45657,#45658) ;
#36268 = AXIS2_PLACEMENT_3D('',#81301,#45659,#45660) ;
#36269 = AXIS2_PLACEMENT_3D('',#81302,#45661,#45662) ;
#36270 = AXIS2_PLACEMENT_3D('',#81303,#45663,#45664) ;
#36271 = AXIS2_PLACEMENT_3D('',#81304,#45665,#45666) ;
#36272 = AXIS2_PLACEMENT_3D('',#81305,#45667,#45668) ;
#36273 = AXIS2_PLACEMENT_3D('',#81306,#45669,#45670) ;
#36274 = AXIS2_PLACEMENT_3D('',#81307,#45671,#45672) ;
#36275 = AXIS2_PLACEMENT_3D('',#81308,#45673,#45674) ;
#36276 = AXIS2_PLACEMENT_3D('',#81316,#45678,#45679) ;
#36277 = AXIS2_PLACEMENT_3D('',#81317,#45680,#45681) ;
#36278 = AXIS2_PLACEMENT_3D('',#81324,#45685,#45686) ;
#36279 = AXIS2_PLACEMENT_3D('',#81333,#45691,#45692) ;
#36280 = AXIS2_PLACEMENT_3D('',#81334,#45693,#45694) ;
#36281 = AXIS2_PLACEMENT_3D('',#81335,#45695,#45696) ;
#36282 = AXIS2_PLACEMENT_3D('',#81336,#45697,#45698) ;
#36283 = AXIS2_PLACEMENT_3D('',#81337,#45699,#45700) ;
#36284 = AXIS2_PLACEMENT_3D('',#81338,#45701,#45702) ;
#36285 = AXIS2_PLACEMENT_3D('',#81339,#45703,#45704) ;
#36286 = AXIS2_PLACEMENT_3D('',#81340,#45705,#45706) ;
#36287 = AXIS2_PLACEMENT_3D('',#81341,#45707,#45708) ;
#36288 = AXIS2_PLACEMENT_3D('',#81342,#45709,#45710) ;
#36289 = AXIS2_PLACEMENT_3D('',#81343,#45711,#45712) ;
#36290 = AXIS2_PLACEMENT_3D('',#81351,#45716,#45717) ;
#36291 = AXIS2_PLACEMENT_3D('',#81352,#45718,#45719) ;
#36292 = AXIS2_PLACEMENT_3D('',#81359,#45723,#45724) ;
#36293 = AXIS2_PLACEMENT_3D('',#81368,#45729,#45730) ;
#36294 = AXIS2_PLACEMENT_3D('',#81369,#45731,#45732) ;
#36295 = AXIS2_PLACEMENT_3D('',#81370,#45733,#45734) ;
#36296 = AXIS2_PLACEMENT_3D('',#81371,#45735,#45736) ;
#36297 = AXIS2_PLACEMENT_3D('',#81372,#45737,#45738) ;
#36298 = AXIS2_PLACEMENT_3D('',#81373,#45739,#45740) ;
#36299 = AXIS2_PLACEMENT_3D('',#81374,#45741,#45742) ;
#36300 = AXIS2_PLACEMENT_3D('',#81375,#45743,#45744) ;
#36301 = AXIS2_PLACEMENT_3D('',#81376,#45745,#45746) ;
#36302 = AXIS2_PLACEMENT_3D('',#81377,#45747,#45748) ;
#36303 = AXIS2_PLACEMENT_3D('',#81378,#45749,#45750) ;
#36304 = AXIS2_PLACEMENT_3D('',#81389,#45757,#45758) ;
#36305 = AXIS2_PLACEMENT_3D('',#81400,#45765,#45766) ;
#36306 = AXIS2_PLACEMENT_3D('',#81411,#45773,#45774) ;
#36307 = AXIS2_PLACEMENT_3D('',#81422,#45781,#45782) ;
#36308 = AXIS2_PLACEMENT_3D('',#81423,#45783,#45784) ;
#36309 = AXIS2_PLACEMENT_3D('',#81425,#45785,#45786) ;
#36310 = AXIS2_PLACEMENT_3D('',#81426,#45787,#45788) ;
#36311 = AXIS2_PLACEMENT_3D('',#81427,#45789,#45790) ;
#36312 = AXIS2_PLACEMENT_3D('',#81428,#45791,#45792) ;
#36313 = AXIS2_PLACEMENT_3D('',#81458,#45793,#45794) ;
#36314 = AXIS2_PLACEMENT_3D('',#81471,#45795,#45796) ;
#36315 = AXIS2_PLACEMENT_3D('',#81473,#45798,#45799) ;
#36316 = AXIS2_PLACEMENT_3D('',#81504,#45801,#45802) ;
#36317 = AXIS2_PLACEMENT_3D('',#81517,#45803,#45804) ;
#36318 = AXIS2_PLACEMENT_3D('',#81519,#45806,#45807) ;
#36319 = AXIS2_PLACEMENT_3D('',#81550,#45809,#45810) ;
#36320 = AXIS2_PLACEMENT_3D('',#81589,#45811,#45812) ;
#36321 = AXIS2_PLACEMENT_3D('',#81596,#45813,#45814) ;
#36322 = AXIS2_PLACEMENT_3D('',#81598,#45816,#45817) ;
#36323 = AXIS2_PLACEMENT_3D('',#81629,#45819,#45820) ;
#36324 = AXIS2_PLACEMENT_3D('',#81642,#45821,#45822) ;
#36325 = AXIS2_PLACEMENT_3D('',#81644,#45824,#45825) ;
#36326 = AXIS2_PLACEMENT_3D('',#81646,#45827,#45828) ;
#36327 = AXIS2_PLACEMENT_3D('',#81647,#45829,#45830) ;
#36328 = AXIS2_PLACEMENT_3D('',#81648,#45831,#45832) ;
#36329 = AXIS2_PLACEMENT_3D('',#81649,#45833,#45834) ;
#36330 = AXIS2_PLACEMENT_3D('',#81650,#45835,#45836) ;
#36331 = AXIS2_PLACEMENT_3D('',#81651,#45837,#45838) ;
#36332 = AXIS2_PLACEMENT_3D('',#81652,#45839,#45840) ;
#36333 = AXIS2_PLACEMENT_3D('',#81653,#45841,#45842) ;
#36334 = AXIS2_PLACEMENT_3D('',#81654,#45843,#45844) ;
#36335 = AXIS2_PLACEMENT_3D('',#81655,#45845,#45846) ;
#36336 = AXIS2_PLACEMENT_3D('',#81656,#45847,#45848) ;
#36337 = AXIS2_PLACEMENT_3D('',#81657,#45849,#45850) ;
#36338 = AXIS2_PLACEMENT_3D('',#81658,#45851,#45852) ;
#36339 = AXIS2_PLACEMENT_3D('',#81659,#45853,#45854) ;
#36340 = AXIS2_PLACEMENT_3D('',#81660,#45855,#45856) ;
#36341 = AXIS2_PLACEMENT_3D('',#81661,#45857,#45858) ;
#36342 = AXIS2_PLACEMENT_3D('',#81662,#45859,#45860) ;
#36343 = AXIS2_PLACEMENT_3D('',#81663,#45861,#45862) ;
#36344 = AXIS2_PLACEMENT_3D('',#81664,#45863,#45864) ;
#36345 = AXIS2_PLACEMENT_3D('',#81677,#45871,#45872) ;
#36346 = AXIS2_PLACEMENT_3D('',#81687,#45878,#45879) ;
#36347 = AXIS2_PLACEMENT_3D('',#81695,#45884,#45885) ;
#36348 = AXIS2_PLACEMENT_3D('',#81699,#45888,#45889) ;
#36349 = AXIS2_PLACEMENT_3D('',#81707,#45894,#45895) ;
#36350 = AXIS2_PLACEMENT_3D('',#81715,#45900,#45901) ;
#36351 = AXIS2_PLACEMENT_3D('',#81725,#45907,#45908) ;
#36352 = AXIS2_PLACEMENT_3D('',#81730,#45912,#45913) ;
#36353 = AXIS2_PLACEMENT_3D('',#81734,#45916,#45917) ;
#36354 = AXIS2_PLACEMENT_3D('',#81742,#45922,#45923) ;
#36355 = AXIS2_PLACEMENT_3D('',#81746,#45926,#45927) ;
#36356 = AXIS2_PLACEMENT_3D('',#81747,#45928,#45929) ;
#36357 = AXIS2_PLACEMENT_3D('',#81750,#45931,#45932) ;
#36358 = AXIS2_PLACEMENT_3D('',#81752,#45933,#45934) ;
#36359 = AXIS2_PLACEMENT_3D('',#81754,#45935,#45936) ;
#36360 = AXIS2_PLACEMENT_3D('',#81756,#45937,#45938) ;
#36361 = AXIS2_PLACEMENT_3D('',#81758,#45939,#45940) ;
#36362 = AXIS2_PLACEMENT_3D('',#81759,#45941,#45942) ;
#36363 = AXIS2_PLACEMENT_3D('',#81762,#45944,#45945) ;
#36364 = AXIS2_PLACEMENT_3D('',#81764,#45946,#45947) ;
#36365 = AXIS2_PLACEMENT_3D('',#81766,#45948,#45949) ;
#36366 = AXIS2_PLACEMENT_3D('',#81768,#45950,#45951) ;
#36367 = AXIS2_PLACEMENT_3D('',#81770,#45952,#45953) ;
#36368 = AXIS2_PLACEMENT_3D('',#81771,#45954,#45955) ;
#36369 = AXIS2_PLACEMENT_3D('',#81775,#45958,#45959) ;
#36370 = AXIS2_PLACEMENT_3D('',#81779,#45962,#45963) ;
#36371 = AXIS2_PLACEMENT_3D('',#81781,#45965,#45966) ;
#36372 = AXIS2_PLACEMENT_3D('',#81782,#45967,#45968) ;
#36373 = AXIS2_PLACEMENT_3D('',#81784,#45970,#45971) ;
#36374 = AXIS2_PLACEMENT_3D('',#81786,#45973,#45974) ;
#36375 = AXIS2_PLACEMENT_3D('',#81788,#45976,#45977) ;
#36376 = AXIS2_PLACEMENT_3D('',#81790,#45979,#45980) ;
#36377 = AXIS2_PLACEMENT_3D('',#81792,#45982,#45983) ;
#36378 = AXIS2_PLACEMENT_3D('',#81793,#45984,#45985) ;
#36379 = AXIS2_PLACEMENT_3D('',#81794,#45986,#45987) ;
#36380 = AXIS2_PLACEMENT_3D('',#81795,#45988,#45989) ;
#36381 = AXIS2_PLACEMENT_3D('',#81796,#45990,#45991) ;
#36382 = AXIS2_PLACEMENT_3D('',#81797,#45992,#45993) ;
#36383 = AXIS2_PLACEMENT_3D('',#81827,#45995,#45996) ;
#36384 = AXIS2_PLACEMENT_3D('',#81850,#45997,#45998) ;
#36385 = AXIS2_PLACEMENT_3D('',#81926,#46000,#46001) ;
#36386 = AXIS2_PLACEMENT_3D('',#82004,#46003,#46004) ;
#36387 = AXIS2_PLACEMENT_3D('',#82082,#46006,#46007) ;
#36388 = AXIS2_PLACEMENT_3D('',#82158,#46009,#46010) ;
#36389 = AXIS2_PLACEMENT_3D('',#82234,#46012,#46013) ;
#36390 = AXIS2_PLACEMENT_3D('',#82310,#46015,#46016) ;
#36391 = AXIS2_PLACEMENT_3D('',#82386,#46018,#46019) ;
#36392 = AXIS2_PLACEMENT_3D('',#82464,#46021,#46022) ;
#36393 = AXIS2_PLACEMENT_3D('',#82540,#46024,#46025) ;
#36394 = AXIS2_PLACEMENT_3D('',#82618,#46027,#46028) ;
#36395 = AXIS2_PLACEMENT_3D('',#82694,#46030,#46031) ;
#36396 = AXIS2_PLACEMENT_3D('',#82770,#46033,#46034) ;
#36397 = AXIS2_PLACEMENT_3D('',#82846,#46036,#46037) ;
#36398 = AXIS2_PLACEMENT_3D('',#82922,#46039,#46040) ;
#36399 = AXIS2_PLACEMENT_3D('',#82960,#46042,#46043) ;
#36400 = AXIS2_PLACEMENT_3D('',#83071,#46044,#46045) ;
#36401 = AXIS2_PLACEMENT_3D('',#83147,#46047,#46048) ;
#36402 = AXIS2_PLACEMENT_3D('',#83223,#46050,#46051) ;
#36403 = AXIS2_PLACEMENT_3D('',#83299,#46053,#46054) ;
#36404 = AXIS2_PLACEMENT_3D('',#83375,#46056,#46057) ;
#36405 = AXIS2_PLACEMENT_3D('',#83453,#46059,#46060) ;
#36406 = AXIS2_PLACEMENT_3D('',#83529,#46062,#46063) ;
#36407 = AXIS2_PLACEMENT_3D('',#83605,#46065,#46066) ;
#36408 = AXIS2_PLACEMENT_3D('',#83683,#46068,#46069) ;
#36409 = AXIS2_PLACEMENT_3D('',#83759,#46071,#46072) ;
#36410 = AXIS2_PLACEMENT_3D('',#83835,#46074,#46075) ;
#36411 = AXIS2_PLACEMENT_3D('',#83911,#46077,#46078) ;
#36412 = AXIS2_PLACEMENT_3D('',#83987,#46080,#46081) ;
#36413 = AXIS2_PLACEMENT_3D('',#84065,#46083,#46084) ;
#36414 = AXIS2_PLACEMENT_3D('',#84141,#46086,#46087) ;
#36415 = AXIS2_PLACEMENT_3D('',#84219,#46089,#46090) ;
#36416 = AXIS2_PLACEMENT_3D('',#84256,#46092,#46093) ;
#36417 = AXIS2_PLACEMENT_3D('',#84257,#46094,#46095) ;
#36418 = AXIS2_PLACEMENT_3D('',#84258,#46096,#46097) ;
#36419 = AXIS2_PLACEMENT_3D('',#84285,#46098,#46099) ;
#36420 = AXIS2_PLACEMENT_3D('',#84302,#46100,#46101) ;
#36421 = AXIS2_PLACEMENT_3D('',#84313,#46102,#46103) ;
#36422 = AXIS2_PLACEMENT_3D('',#84346,#46104,#46105) ;
#36423 = AXIS2_PLACEMENT_3D('',#84375,#46106,#46107) ;
#36424 = AXIS2_PLACEMENT_3D('',#84378,#46108,#46109) ;
#36425 = AXIS2_PLACEMENT_3D('',#84384,#46110,#46111) ;
#36426 = AXIS2_PLACEMENT_3D('',#84388,#46112,#46113) ;
#36427 = AXIS2_PLACEMENT_3D('',#84391,#46114,#46115) ;
#36428 = AXIS2_PLACEMENT_3D('',#84397,#46116,#46117) ;
#36429 = AXIS2_PLACEMENT_3D('',#84401,#46118,#46119) ;
#36430 = AXIS2_PLACEMENT_3D('',#84403,#46120,#46121) ;
#36431 = AXIS2_PLACEMENT_3D('',#84405,#46122,#46123) ;
#36432 = AXIS2_PLACEMENT_3D('',#84407,#46124,#46125) ;
#36433 = AXIS2_PLACEMENT_3D('',#84408,#46126,#46127) ;
#36434 = AXIS2_PLACEMENT_3D('',#84409,#46128,#46129) ;
#36435 = AXIS2_PLACEMENT_3D('',#84412,#46130,#46131) ;
#36436 = AXIS2_PLACEMENT_3D('',#84414,#46132,#46133) ;
#36437 = AXIS2_PLACEMENT_3D('',#84416,#46134,#46135) ;
#36438 = AXIS2_PLACEMENT_3D('',#84418,#46136,#46137) ;
#36439 = AXIS2_PLACEMENT_3D('',#84419,#46138,#46139) ;
#36440 = AXIS2_PLACEMENT_3D('',#84421,#46140,#46141) ;
#36441 = AXIS2_PLACEMENT_3D('',#84423,#46142,#46143) ;
#36442 = AXIS2_PLACEMENT_3D('',#84425,#46144,#46145) ;
#36443 = AXIS2_PLACEMENT_3D('',#84426,#46146,#46147) ;
#36444 = AXIS2_PLACEMENT_3D('',#84428,#46148,#46149) ;
#36445 = AXIS2_PLACEMENT_3D('',#84430,#46150,#46151) ;
#36446 = AXIS2_PLACEMENT_3D('',#84432,#46152,#46153) ;
#36447 = AXIS2_PLACEMENT_3D('',#84434,#46154,#46155) ;
#36448 = AXIS2_PLACEMENT_3D('',#84436,#46156,#46157) ;
#36449 = AXIS2_PLACEMENT_3D('',#84438,#46158,#46159) ;
#36450 = AXIS2_PLACEMENT_3D('',#84440,#46160,#46161) ;
#36451 = AXIS2_PLACEMENT_3D('',#84442,#46162,#46163) ;
#36452 = AXIS2_PLACEMENT_3D('',#84443,#46164,#46165) ;
#36453 = AXIS2_PLACEMENT_3D('',#84444,#46166,#46167) ;
#36454 = AXIS2_PLACEMENT_3D('',#84447,#46168,#46169) ;
#36455 = AXIS2_PLACEMENT_3D('',#84449,#46171,#46172) ;
#36456 = AXIS2_PLACEMENT_3D('',#84450,#46173,#46174) ;
#36457 = AXIS2_PLACEMENT_3D('',#84452,#46175,#46176) ;
#36458 = AXIS2_PLACEMENT_3D('',#84453,#46177,#46178) ;
#36459 = AXIS2_PLACEMENT_3D('',#84454,#46179,#46180) ;
#36460 = AXIS2_PLACEMENT_3D('',#85382,#46182,#46183) ;
#36461 = AXIS2_PLACEMENT_3D('',#85383,#46184,#46185) ;
#36462 = AXIS2_PLACEMENT_3D('',#85389,#46186,#46187) ;
#36463 = AXIS2_PLACEMENT_3D('',#85393,#46188,#46189) ;
#36464 = AXIS2_PLACEMENT_3D('',#85397,#46192,#46193) ;
#36465 = AXIS2_PLACEMENT_3D('',#85401,#46196,#46197) ;
#36466 = AXIS2_PLACEMENT_3D('',#85405,#46200,#46201) ;
#36467 = AXIS2_PLACEMENT_3D('',#85407,#46203,#46204) ;
#36468 = AXIS2_PLACEMENT_3D('',#85419,#46210,#46211) ;
#36469 = AXIS2_PLACEMENT_3D('',#85432,#46219,#46220) ;
#36470 = AXIS2_PLACEMENT_3D('',#85434,#46222,#46223) ;
#36471 = AXIS2_PLACEMENT_3D('',#85436,#46225,#46226) ;
#36472 = AXIS2_PLACEMENT_3D('',#85438,#46228,#46229) ;
#36473 = AXIS2_PLACEMENT_3D('',#85439,#46230,#46231) ;
#36474 = AXIS2_PLACEMENT_3D('',#85441,#46233,#46234) ;
#36475 = AXIS2_PLACEMENT_3D('',#85443,#46236,#46237) ;
#36476 = AXIS2_PLACEMENT_3D('',#85445,#46239,#46240) ;
#36477 = AXIS2_PLACEMENT_3D('',#85449,#46241,#46242) ;
#36478 = AXIS2_PLACEMENT_3D('',#85453,#46243,#46244) ;
#36479 = AXIS2_PLACEMENT_3D('',#85455,#46246,#46247) ;
#36480 = AXIS2_PLACEMENT_3D('',#85457,#46249,#46250) ;
#36481 = AXIS2_PLACEMENT_3D('',#85459,#46252,#46253) ;
#36482 = AXIS2_PLACEMENT_3D('',#85460,#46254,#46255) ;
#36483 = AXIS2_PLACEMENT_3D('',#85461,#46256,#46257) ;
#36484 = AXIS2_PLACEMENT_3D('',#85470,#46262,#46263) ;
#36485 = AXIS2_PLACEMENT_3D('',#85901,#46268,#46269) ;
#36486 = AXIS2_PLACEMENT_3D('',#86232,#46270,#46271) ;
#36487 = AXIS2_PLACEMENT_3D('',#86233,#46272,#46273) ;
#36488 = AXIS2_PLACEMENT_3D('',#86235,#46274,#46275) ;
#36489 = AXIS2_PLACEMENT_3D('',#86237,#46276,#46277) ;
#36490 = AXIS2_PLACEMENT_3D('',#86239,#46278,#46279) ;
#36491 = AXIS2_PLACEMENT_3D('',#86240,#46280,#46281) ;
#36492 = AXIS2_PLACEMENT_3D('',#86241,#46282,#46283) ;
#36493 = AXIS2_PLACEMENT_3D('',#86244,#46284,#46285) ;
#36494 = AXIS2_PLACEMENT_3D('',#86245,#46286,#46287) ;
#36495 = AXIS2_PLACEMENT_3D('',#86247,#46289,#46290) ;
#36496 = AXIS2_PLACEMENT_3D('',#86249,#46291,#46292) ;
#36497 = AXIS2_PLACEMENT_3D('',#86250,#46293,#46294) ;
#36498 = AXIS2_PLACEMENT_3D('',#86252,#46295,#46296) ;
#36499 = AXIS2_PLACEMENT_3D('',#86253,#46297,#46298) ;
#36500 = AXIS2_PLACEMENT_3D('',#86254,#46299,#46300) ;
#36501 = AXIS2_PLACEMENT_3D('',#86256,#46301,#46302) ;
#36502 = AXIS2_PLACEMENT_3D('',#86257,#46303,#46304) ;
#36503 = AXIS2_PLACEMENT_3D('',#86259,#46306,#46307) ;
#36504 = AXIS2_PLACEMENT_3D('',#86260,#46308,#46309) ;
#36505 = AXIS2_PLACEMENT_3D('',#86261,#46310,#46311) ;
#36506 = AXIS2_PLACEMENT_3D('',#86262,#46312,#46313) ;
#36507 = AXIS2_PLACEMENT_3D('',#86263,#46314,#46315) ;
#36508 = AXIS2_PLACEMENT_3D('',#86264,#46316,#46317) ;
#36509 = AXIS2_PLACEMENT_3D('',#86265,#46318,#46319) ;
#36510 = AXIS2_PLACEMENT_3D('',#86266,#46320,#46321) ;
#36511 = AXIS2_PLACEMENT_3D('',#86267,#46322,#46323) ;
#36512 = AXIS2_PLACEMENT_3D('',#86268,#46324,#46325) ;
#36513 = AXIS2_PLACEMENT_3D('',#86269,#46326,#46327) ;
#36514 = AXIS2_PLACEMENT_3D('',#86270,#46328,#46329) ;
#36515 = AXIS2_PLACEMENT_3D('',#86271,#46330,#46331) ;
#36516 = AXIS2_PLACEMENT_3D('',#86272,#46332,#46333) ;
#36517 = AXIS2_PLACEMENT_3D('',#86273,#46334,#46335) ;
#36518 = AXIS2_PLACEMENT_3D('',#86274,#46336,#46337) ;
#36519 = AXIS2_PLACEMENT_3D('',#86275,#46338,#46339) ;
#36520 = AXIS2_PLACEMENT_3D('',#86276,#46340,#46341) ;
#36521 = AXIS2_PLACEMENT_3D('',#86277,#46342,#46343) ;
#36522 = AXIS2_PLACEMENT_3D('',#86278,#46344,#46345) ;
#36523 = DIRECTION('axis',(0.,0.,1.)) ;
#36524 = DIRECTION('refdir',(1.,0.,0.)) ;
#36525 = DIRECTION('axis',(0.,0.,1.)) ;
#36526 = DIRECTION('refdir',(1.,0.,0.)) ;
#36527 = DIRECTION('axis',(0.,0.,1.)) ;
#36528 = DIRECTION('refdir',(1.,0.,0.)) ;
#36529 = DIRECTION('center_axis',(-1.,1.75658099177411E-13,4.54195640846217E-14)) ;
#36530 = DIRECTION('ref_axis',(1.56325514861445E-13,0.707106781186434,0.707106781186661)) ;
#36531 = DIRECTION('center_axis',(1.,-1.75658099177411E-13,-4.54195640846217E-14)) ;
#36532 = DIRECTION('ref_axis',(1.56325514861445E-13,0.707106781186434,0.707106781186661)) ;
#36533 = DIRECTION('',(-1.,1.75658099177411E-13,4.54195640846217E-14)) ;
#36534 = DIRECTION('center_axis',(-1.,1.75658099177411E-13,4.54195640846217E-14)) ;
#36535 = DIRECTION('ref_axis',(1.56325514861445E-13,0.707106781186434,0.707106781186661)) ;
#36536 = DIRECTION('',(1.,-1.75658099177411E-13,-4.54195640846217E-14)) ;
#36537 = DIRECTION('center_axis',(4.54195640846217E-14,-1.66321791214601E-16,
1.)) ;
#36538 = DIRECTION('ref_axis',(1.,-1.75658099177411E-13,-4.54195640846217E-14)) ;
#36539 = DIRECTION('',(1.75658099177411E-13,1.,1.66321791206623E-16)) ;
#36540 = DIRECTION('',(1.,-1.75658099177411E-13,-4.54195640846217E-14)) ;
#36541 = DIRECTION('',(1.75658099177411E-13,1.,1.66321791206623E-16)) ;
#36542 = DIRECTION('',(-1.75658099177411E-13,-1.,-1.66321791206623E-16)) ;
#36543 = DIRECTION('',(1.75658099177411E-13,1.,1.66321791206623E-16)) ;
#36544 = DIRECTION('center_axis',(4.54195640846217E-14,-1.66321791214601E-16,
1.)) ;
#36545 = DIRECTION('ref_axis',(-0.866025403784527,-0.499999999999848,3.92513354304944E-14)) ;
#36546 = DIRECTION('center_axis',(4.54195640846217E-14,-1.66321791214601E-16,
1.)) ;
#36547 = DIRECTION('ref_axis',(-1.,5.55236256206829E-46,4.54195640846217E-14)) ;
#36548 = DIRECTION('center_axis',(-4.54195640846217E-14,1.66321791214601E-16,
-1.)) ;
#36549 = DIRECTION('ref_axis',(0.156304737392435,0.987708878702972,-6.93501552682122E-15)) ;
#36550 = DIRECTION('center_axis',(4.54195640846217E-14,-1.66321791214601E-16,
1.)) ;
#36551 = DIRECTION('ref_axis',(-1.,5.55236256206829E-46,4.54195640846217E-14)) ;
#36552 = DIRECTION('center_axis',(-4.54195640846217E-14,1.66321791214601E-16,
-1.)) ;
#36553 = DIRECTION('ref_axis',(0.987708878702962,-0.1563047373925,-4.48873035970975E-14)) ;
#36554 = DIRECTION('center_axis',(4.54195640846217E-14,-1.66321791214601E-16,
1.)) ;
#36555 = DIRECTION('ref_axis',(-0.499999999999848,0.866025403784526,2.28538209386987E-14)) ;
#36556 = DIRECTION('center_axis',(-4.54195640846217E-14,1.66321791214601E-16,
-1.)) ;
#36557 = DIRECTION('ref_axis',(0.987707474797848,0.156313608583704,-4.48352445890699E-14)) ;
#36558 = DIRECTION('center_axis',(4.54195640846217E-14,-1.66321791214601E-16,
1.)) ;
#36559 = DIRECTION('ref_axis',(-1.,5.55236256206829E-46,4.54195640846217E-14)) ;
#36560 = DIRECTION('center_axis',(-4.54195640846217E-14,1.66321791214601E-16,
-1.)) ;
#36561 = DIRECTION('ref_axis',(-0.156304737392422,-0.987708878702974,6.93501552682063E-15)) ;
#36562 = DIRECTION('center_axis',(4.54195640846217E-14,-1.66321791214601E-16,
1.)) ;
#36563 = DIRECTION('ref_axis',(0.866025403784527,0.499999999999848,-3.92513354304944E-14)) ;
#36564 = DIRECTION('center_axis',(4.54195640846217E-14,-1.66321791214601E-16,
1.)) ;
#36565 = DIRECTION('ref_axis',(-1.,1.75719331517368E-13,4.54195640846217E-14)) ;
#36566 = DIRECTION('center_axis',(4.54195640846217E-14,-1.66321791214601E-16,
1.)) ;
#36567 = DIRECTION('ref_axis',(-0.965925826289023,0.25881904510269,4.39149772153074E-14)) ;
#36568 = DIRECTION('center_axis',(4.54195640846217E-14,-1.66321791214601E-16,
1.)) ;
#36569 = DIRECTION('ref_axis',(-1.,1.75719331517368E-13,4.54195640846217E-14)) ;
#36570 = DIRECTION('center_axis',(4.54195640846217E-14,-1.66321791214601E-16,
1.)) ;
#36571 = DIRECTION('ref_axis',(-0.965925826289114,-0.258819045102351,4.38288827209477E-14)) ;
#36572 = DIRECTION('',(-1.75658099177411E-13,-1.,-1.66321791206623E-16)) ;
#36573 = DIRECTION('center_axis',(4.54195640846217E-14,-1.66321791214601E-16,
1.)) ;
#36574 = DIRECTION('ref_axis',(1.75658099177411E-13,1.,1.66321791206623E-16)) ;
#36575 = DIRECTION('',(1.75658099177411E-13,1.,1.66321791206623E-16)) ;
#36576 = DIRECTION('center_axis',(4.54195640846217E-14,-1.66321791214601E-16,
1.)) ;
#36577 = DIRECTION('ref_axis',(1.75658099177411E-13,1.,1.66321791206623E-16)) ;
#36578 = DIRECTION('',(-1.75658099177411E-13,-1.,-1.66321791206623E-16)) ;
#36579 = DIRECTION('center_axis',(4.54195640846217E-14,-1.66321791214601E-16,
1.)) ;
#36580 = DIRECTION('ref_axis',(1.75658099177411E-13,1.,1.66321791206623E-16)) ;
#36581 = DIRECTION('',(1.75658099177411E-13,1.,1.66321791206623E-16)) ;
#36582 = DIRECTION('center_axis',(4.54195640846217E-14,-1.66321791214601E-16,
1.)) ;
#36583 = DIRECTION('ref_axis',(1.75658099177411E-13,1.,1.66321791206623E-16)) ;
#36584 = DIRECTION('',(-1.75658099177411E-13,-1.,-1.66321791206623E-16)) ;
#36585 = DIRECTION('center_axis',(4.54195640846217E-14,-1.66321791214601E-16,
1.)) ;
#36586 = DIRECTION('ref_axis',(1.75658099177411E-13,1.,1.66321791206623E-16)) ;
#36587 = DIRECTION('',(1.75658099177411E-13,1.,1.66321791206623E-16)) ;
#36588 = DIRECTION('center_axis',(4.54195640846217E-14,-1.66321791214601E-16,
1.)) ;
#36589 = DIRECTION('ref_axis',(1.75658099177411E-13,1.,1.66321791206623E-16)) ;
#36590 = DIRECTION('',(-1.75658099177411E-13,-1.,-1.66321791206623E-16)) ;
#36591 = DIRECTION('center_axis',(4.54195640846217E-14,-1.66321791214601E-16,
1.)) ;
#36592 = DIRECTION('ref_axis',(1.75658099177411E-13,1.,1.66321791206623E-16)) ;
#36593 = DIRECTION('',(1.75658099177411E-13,1.,1.66321791206623E-16)) ;
#36594 = DIRECTION('center_axis',(4.54195640846217E-14,-1.66321791214601E-16,
1.)) ;
#36595 = DIRECTION('ref_axis',(1.75658099177411E-13,1.,1.66321791206623E-16)) ;
#36596 = DIRECTION('',(1.75658099177411E-13,1.,1.66321791206623E-16)) ;
#36597 = DIRECTION('center_axis',(4.54195640846217E-14,-1.66321791214601E-16,
1.)) ;
#36598 = DIRECTION('ref_axis',(1.75658099177411E-13,1.,1.66321791206623E-16)) ;
#36599 = DIRECTION('',(-1.75658099177411E-13,-1.,-1.66321791206623E-16)) ;
#36600 = DIRECTION('center_axis',(4.54195640846217E-14,-1.66321791214601E-16,
1.)) ;
#36601 = DIRECTION('ref_axis',(1.75658099177411E-13,1.,1.66321791206623E-16)) ;
#36602 = DIRECTION('',(-1.75658099177411E-13,-1.,-1.66321791206623E-16)) ;
#36603 = DIRECTION('center_axis',(4.54195640846217E-14,-1.66321791214601E-16,
1.)) ;
#36604 = DIRECTION('ref_axis',(1.75658099177411E-13,1.,1.66321791206623E-16)) ;
#36605 = DIRECTION('',(1.75658099177411E-13,1.,1.66321791206623E-16)) ;
#36606 = DIRECTION('center_axis',(4.54195640846217E-14,-1.66321791214601E-16,
1.)) ;
#36607 = DIRECTION('ref_axis',(1.75658099177411E-13,1.,1.66321791206623E-16)) ;
#36608 = DIRECTION('center_axis',(4.54195640846217E-14,-1.66321791214601E-16,
1.)) ;
#36609 = DIRECTION('ref_axis',(1.,-1.75824632631105E-13,-4.54195640846217E-14)) ;
#36610 = DIRECTION('center_axis',(4.54195640846217E-14,-1.66321791214601E-16,
1.)) ;
#36611 = DIRECTION('ref_axis',(1.,-1.75824632631105E-13,-4.54195640846217E-14)) ;
#36612 = DIRECTION('center_axis',(4.54195640846217E-14,-1.66321791214601E-16,
1.)) ;
#36613 = DIRECTION('ref_axis',(0.707106781186672,0.707106781186423,-3.19988744963517E-14)) ;
#36614 = DIRECTION('center_axis',(4.54195640846217E-14,-1.66321791214601E-16,
1.)) ;
#36615 = DIRECTION('ref_axis',(0.707106781186672,0.707106781186423,-3.19988744963517E-14)) ;
#36616 = DIRECTION('center_axis',(4.54195640846217E-14,-1.66321791214601E-16,
1.)) ;
#36617 = DIRECTION('ref_axis',(0.707106781186672,0.707106781186423,-3.19988744963517E-14)) ;
#36618 = DIRECTION('center_axis',(4.54195640846217E-14,-1.66321791214601E-16,
1.)) ;
#36619 = DIRECTION('ref_axis',(0.707106781186672,0.707106781186423,-3.19988744963517E-14)) ;
#36620 = DIRECTION('center_axis',(4.54195640846217E-14,-1.66321791214601E-16,
1.)) ;
#36621 = DIRECTION('ref_axis',(-0.258819045102691,-0.965925826289023,1.15947936917534E-14)) ;
#36622 = DIRECTION('center_axis',(4.54195640846217E-14,-1.66321791214601E-16,
1.)) ;
#36623 = DIRECTION('ref_axis',(-1.75780563857326E-13,-1.,-1.66321791206617E-16)) ;
#36624 = DIRECTION('center_axis',(4.54195640846217E-14,-1.66321791214601E-16,
1.)) ;
#36625 = DIRECTION('ref_axis',(0.258819045102351,-0.965925826289114,-1.19161027189557E-14)) ;
#36626 = DIRECTION('center_axis',(4.54195640846217E-14,-1.66321791214601E-16,
1.)) ;
#36627 = DIRECTION('ref_axis',(-1.75780563857326E-13,-1.,-1.66321791206617E-16)) ;
#36628 = DIRECTION('center_axis',(4.54195640846217E-14,-1.66321791214601E-16,
1.)) ;
#36629 = DIRECTION('ref_axis',(0.965925826289023,-0.258819045102691,-4.39149772153074E-14)) ;
#36630 = DIRECTION('center_axis',(4.54195640846217E-14,-1.66321791214601E-16,
1.)) ;
#36631 = DIRECTION('ref_axis',(1.,-1.75841796197283E-13,-4.54195640846217E-14)) ;
#36632 = DIRECTION('center_axis',(4.54195640846217E-14,-1.66321791214601E-16,
1.)) ;
#36633 = DIRECTION('ref_axis',(0.965925826289114,0.258819045102351,-4.38288827209477E-14)) ;
#36634 = DIRECTION('center_axis',(4.54195640846217E-14,-1.66321791214601E-16,
1.)) ;
#36635 = DIRECTION('ref_axis',(1.,-1.75841796197283E-13,-4.54195640846217E-14)) ;
#36636 = DIRECTION('center_axis',(4.54195640846217E-14,-1.66321791214601E-16,
1.)) ;
#36637 = DIRECTION('ref_axis',(0.258819045102691,0.965925826289023,-1.15947936917534E-14)) ;
#36638 = DIRECTION('center_axis',(4.54195640846217E-14,-1.66321791214601E-16,
1.)) ;
#36639 = DIRECTION('ref_axis',(1.7590302853724E-13,1.,1.66321791206612E-16)) ;
#36640 = DIRECTION('center_axis',(4.54195640846217E-14,-1.66321791214601E-16,
1.)) ;
#36641 = DIRECTION('ref_axis',(-0.258819045102351,0.965925826289114,1.19161027189557E-14)) ;
#36642 = DIRECTION('center_axis',(4.54195640846217E-14,-1.66321791214601E-16,
1.)) ;
#36643 = DIRECTION('ref_axis',(1.7590302853724E-13,1.,1.66321791206612E-16)) ;
#36644 = DIRECTION('center_axis',(4.54195640846217E-14,-1.66321791214601E-16,
1.)) ;
#36645 = DIRECTION('ref_axis',(0.499999999999848,-0.866025403784527,-2.28538209386987E-14)) ;
#36646 = DIRECTION('center_axis',(-4.54195640846217E-14,1.66321791214601E-16,
-1.)) ;
#36647 = DIRECTION('ref_axis',(0.156305321293456,-0.987708786300572,-7.26359705179142E-15)) ;
#36648 = DIRECTION('center_axis',(4.54195640846217E-14,-1.66321791214601E-16,
1.)) ;
#36649 = DIRECTION('ref_axis',(-1.,5.55236256206829E-46,4.54195640846217E-14)) ;
#36650 = DIRECTION('center_axis',(-4.54195640846217E-14,1.66321791214601E-16,
-1.)) ;
#36651 = DIRECTION('ref_axis',(-0.987708878702966,0.156304737392474,4.48873035970976E-14)) ;
#36652 = DIRECTION('center_axis',(-1.75658099177411E-13,-1.,-1.66321791206623E-16)) ;
#36653 = DIRECTION('ref_axis',(-0.707106781186542,1.24091425832264E-13,0.707106781186553)) ;
#36654 = DIRECTION('center_axis',(1.75658099177411E-13,1.,1.66321791206623E-16)) ;
#36655 = DIRECTION('ref_axis',(-0.707106781186542,1.24091425832264E-13,0.707106781186553)) ;
#36656 = DIRECTION('center_axis',(-1.75658099177411E-13,-1.,-1.66321791206623E-16)) ;
#36657 = DIRECTION('ref_axis',(-0.707106781186542,1.24091425832264E-13,0.707106781186553)) ;
#36658 = DIRECTION('',(1.75658099177411E-13,1.,1.66321791206623E-16)) ;
#36659 = DIRECTION('center_axis',(-1.,1.75658099177411E-13,4.54195640846217E-14)) ;
#36660 = DIRECTION('ref_axis',(-9.20925513358884E-14,-0.707106781186434,0.707106781186661)) ;
#36661 = DIRECTION('center_axis',(1.,-1.75658099177411E-13,-4.54195640846217E-14)) ;
#36662 = DIRECTION('ref_axis',(-9.20925513358884E-14,-0.707106781186434,0.707106781186661)) ;
#36663 = DIRECTION('',(-1.,1.75658099177411E-13,4.54195640846217E-14)) ;
#36664 = DIRECTION('center_axis',(-1.,1.75658099177411E-13,4.54195640846217E-14)) ;
#36665 = DIRECTION('ref_axis',(-9.20925513358884E-14,-0.707106781186434,0.707106781186661)) ;
#36666 = DIRECTION('center_axis',(1.75658099177411E-13,1.,1.66321791206623E-16)) ;
#36667 = DIRECTION('ref_axis',(-4.54195640846217E-14,1.66321791214601E-16,
-1.)) ;
#36668 = DIRECTION('',(4.54195640846217E-14,-1.66321791214601E-16,1.)) ;
#36669 = DIRECTION('center_axis',(-1.75658099177411E-13,-1.,-1.66321791206623E-16)) ;
#36670 = DIRECTION('ref_axis',(0.70710678118651,-1.24091425832259E-13,-0.707106781186585)) ;
#36671 = DIRECTION('',(1.,-1.75658099177411E-13,-4.53796366499639E-14)) ;
#36672 = DIRECTION('center_axis',(1.75658099177411E-13,1.,1.66321791206623E-16)) ;
#36673 = DIRECTION('ref_axis',(-0.707106781186529,1.24091425832262E-13,0.707106781186566)) ;
#36674 = DIRECTION('',(-2.98822568073276E-29,-1.66321791206623E-16,1.)) ;
#36675 = DIRECTION('center_axis',(-1.75658099177411E-13,-1.,-1.66321791206623E-16)) ;
#36676 = DIRECTION('ref_axis',(0.707106781186551,-1.24091425832266E-13,-0.707106781186544)) ;
#36677 = DIRECTION('',(1.,-1.75658099177411E-13,-4.54195640846217E-14)) ;
#36678 = DIRECTION('center_axis',(-1.75658099177411E-13,-1.,-1.66321791206623E-16)) ;
#36679 = DIRECTION('ref_axis',(-0.707106781186579,1.24326640365113E-13,-0.707106781186516)) ;
#36680 = DIRECTION('',(2.92172610985041E-29,1.66321791206623E-16,-1.)) ;
#36681 = DIRECTION('center_axis',(1.75658099177411E-13,1.,1.66321791206623E-16)) ;
#36682 = DIRECTION('ref_axis',(0.707106781186554,-1.24326640365109E-13,0.707106781186541)) ;
#36683 = DIRECTION('',(1.,-1.75658099177411E-13,-4.54224185797219E-14)) ;
#36684 = DIRECTION('center_axis',(1.75658099177411E-13,1.,1.66321791206623E-16)) ;
#36685 = DIRECTION('ref_axis',(-0.707106781186538,1.24091425832263E-13,0.707106781186557)) ;
#36686 = DIRECTION('',(-2.92157696951376E-29,-1.66321791206623E-16,1.)) ;
#36687 = DIRECTION('center_axis',(-1.75658099177411E-13,-1.,-1.66321791206623E-16)) ;
#36688 = DIRECTION('ref_axis',(0.707106781186529,-1.24091425832262E-13,-0.707106781186566)) ;
#36689 = DIRECTION('',(1.,-1.75658099177411E-13,-4.54195640846217E-14)) ;
#36690 = DIRECTION('center_axis',(-1.75658099177411E-13,-1.,-1.66321791206623E-16)) ;
#36691 = DIRECTION('ref_axis',(-0.70710678118658,1.24326640365113E-13,-0.707106781186515)) ;
#36692 = DIRECTION('',(-4.54195640846217E-14,1.66321791214601E-16,-1.)) ;
#36693 = DIRECTION('center_axis',(1.75658099177411E-13,1.,1.66321791206623E-16)) ;
#36694 = DIRECTION('ref_axis',(-1.,1.75658099177411E-13,1.34042507393854E-33)) ;
#36695 = DIRECTION('center_axis',(1.75658099177411E-13,1.,1.66321791206623E-16)) ;
#36696 = DIRECTION('ref_axis',(-1.,1.75658099177411E-13,6.92942826962939E-35)) ;
#36697 = DIRECTION('center_axis',(-1.,1.75658099177411E-13,4.54195640846217E-14)) ;
#36698 = DIRECTION('ref_axis',(1.56325514861461E-13,0.70710678118656,0.707106781186535)) ;
#36699 = DIRECTION('center_axis',(1.,-1.75658099177411E-13,-4.54195640846217E-14)) ;
#36700 = DIRECTION('ref_axis',(1.56325514861461E-13,0.70710678118656,0.707106781186535)) ;
#36701 = DIRECTION('',(1.,-1.75658099177411E-13,-4.54195640846217E-14)) ;
#36702 = DIRECTION('center_axis',(-1.,1.75658099177411E-13,4.54195640846217E-14)) ;
#36703 = DIRECTION('ref_axis',(1.56325514861461E-13,0.70710678118656,0.707106781186535)) ;
#36704 = DIRECTION('',(-1.,1.75658099177411E-13,4.54195640846217E-14)) ;
#36705 = DIRECTION('center_axis',(1.,-1.75658099177411E-13,-4.54195640846217E-14)) ;
#36706 = DIRECTION('ref_axis',(1.75658099177411E-13,1.,1.66321791206623E-16)) ;
#36707 = DIRECTION('',(4.54195640846217E-14,-1.66321791214601E-16,1.)) ;
#36708 = DIRECTION('',(1.75658099177411E-13,1.,0.)) ;
#36709 = DIRECTION('',(-4.54195640846217E-14,1.66321791214601E-16,-1.)) ;
#36710 = DIRECTION('',(4.54195640846217E-14,-1.66321791214601E-16,1.)) ;
#36711 = DIRECTION('',(-1.75658099177411E-13,-1.,-1.66321791206623E-16)) ;
#36712 = DIRECTION('center_axis',(-1.75658099177411E-13,-1.,-1.66321791206623E-16)) ;
#36713 = DIRECTION('ref_axis',(-2.33866651370291E-30,1.66321791206623E-16,
-1.)) ;
#36714 = DIRECTION('',(-4.54195640846217E-14,1.66321791214601E-16,-1.)) ;
#36715 = DIRECTION('center_axis',(-1.75658099177411E-13,-1.,-1.66321791206623E-16)) ;
#36716 = DIRECTION('ref_axis',(0.70710678118651,-1.24091425832259E-13,-0.707106781186585)) ;
#36717 = DIRECTION('',(1.,-1.75658099177411E-13,-4.54195640846217E-14)) ;
#36718 = DIRECTION('center_axis',(1.75658099177411E-13,1.,1.66321791206623E-16)) ;
#36719 = DIRECTION('ref_axis',(-0.707106781186529,1.24091425832262E-13,0.707106781186566)) ;
#36720 = DIRECTION('',(1.32744277756511E-27,7.55696881488181E-15,1.)) ;
#36721 = DIRECTION('center_axis',(-1.75658099177411E-13,-1.,-1.66321791206623E-16)) ;
#36722 = DIRECTION('ref_axis',(0.707106781186551,-1.24091425832266E-13,-0.707106781186544)) ;
#36723 = DIRECTION('',(-1.,1.75658099177411E-13,0.)) ;
#36724 = DIRECTION('center_axis',(-1.75658099177411E-13,-1.,-1.66321791206623E-16)) ;
#36725 = DIRECTION('ref_axis',(-0.707106781186551,1.24326640365108E-13,-0.707106781186544)) ;
#36726 = DIRECTION('',(-1.32744277756505E-27,-7.55696881488144E-15,-1.)) ;
#36727 = DIRECTION('center_axis',(1.75658099177411E-13,1.,1.66321791206623E-16)) ;
#36728 = DIRECTION('ref_axis',(0.707106781186551,-1.24326640365108E-13,0.707106781186544)) ;
#36729 = DIRECTION('',(1.,-1.75658099177411E-13,-4.54195640846217E-14)) ;
#36730 = DIRECTION('center_axis',(1.75658099177411E-13,1.,1.66321791206623E-16)) ;
#36731 = DIRECTION('ref_axis',(-0.707106781186535,1.24091425832263E-13,0.70710678118656)) ;
#36732 = DIRECTION('',(2.92157696951376E-29,1.66321791206623E-16,-1.)) ;
#36733 = DIRECTION('center_axis',(-1.75658099177411E-13,-1.,-1.66321791206623E-16)) ;
#36734 = DIRECTION('ref_axis',(0.707106781186549,-1.24091425832265E-13,-0.707106781186546)) ;
#36735 = DIRECTION('',(1.,-1.75658099177411E-13,-4.54195640846217E-14)) ;
#36736 = DIRECTION('center_axis',(-1.75658099177411E-13,-1.,-1.66321791206623E-16)) ;
#36737 = DIRECTION('ref_axis',(-0.707106781186561,1.2432664036511E-13,-0.707106781186534)) ;
#36738 = DIRECTION('center_axis',(1.75658099177411E-13,1.,1.66321791206623E-16)) ;
#36739 = DIRECTION('ref_axis',(0.99999997726804,-1.75658059720777E-13,-0.000213222701069828)) ;
#36740 = DIRECTION('center_axis',(-1.75658099177411E-13,-1.,-1.66321791206623E-16)) ;
#36741 = DIRECTION('ref_axis',(-1.,1.75658099177411E-13,-8.27097305203856E-32)) ;
#36742 = DIRECTION('center_axis',(1.,-1.75658099177411E-13,-4.54195640846217E-14)) ;
#36743 = DIRECTION('ref_axis',(-9.20925513359162E-14,-0.70710678118656,0.707106781186535)) ;
#36744 = DIRECTION('center_axis',(-1.,1.75658099177411E-13,4.54195640846217E-14)) ;
#36745 = DIRECTION('ref_axis',(-9.20925513359162E-14,-0.70710678118656,0.707106781186535)) ;
#36746 = DIRECTION('',(-1.,1.75658099177411E-13,4.54195640846217E-14)) ;
#36747 = DIRECTION('center_axis',(1.,-1.75658099177411E-13,-4.54195640846217E-14)) ;
#36748 = DIRECTION('ref_axis',(-9.20925513359162E-14,-0.70710678118656,0.707106781186535)) ;
#36749 = DIRECTION('',(1.,-1.75658099177411E-13,-4.54195640846217E-14)) ;
#36750 = DIRECTION('center_axis',(-1.,1.75658099177411E-13,4.54195640846217E-14)) ;
#36751 = DIRECTION('ref_axis',(-1.75658099177411E-13,-1.,-1.66321791206623E-16)) ;
#36752 = DIRECTION('',(4.54195640846217E-14,-1.66321791214601E-16,1.)) ;
#36753 = DIRECTION('',(-1.75658099177411E-13,-1.,-1.81854713288318E-16)) ;
#36754 = DIRECTION('',(-4.54195640846217E-14,1.66321791214601E-16,-1.)) ;
#36755 = DIRECTION('',(1.75658099177411E-13,1.,1.66321791206623E-16)) ;
#36756 = DIRECTION('center_axis',(1.75658099177411E-13,1.,1.66321791206623E-16)) ;
#36757 = DIRECTION('ref_axis',(-4.54195640846217E-14,1.66321791214601E-16,
-1.)) ;
#36758 = DIRECTION('',(4.54195640846217E-14,-1.66321791214601E-16,1.)) ;
#36759 = DIRECTION('center_axis',(1.75658099177411E-13,1.,1.66321791206623E-16)) ;
#36760 = DIRECTION('ref_axis',(-0.70710678118658,1.24326640365113E-13,-0.707106781186515)) ;
#36761 = DIRECTION('',(-1.,1.75658099177411E-13,4.54195640846217E-14)) ;
#36762 = DIRECTION('center_axis',(1.75658099177411E-13,1.,1.66321791206623E-16)) ;
#36763 = DIRECTION('ref_axis',(0.707106781186529,-1.24091425832262E-13,-0.707106781186566)) ;
#36764 = DIRECTION('',(-2.92157696951376E-29,-1.66321791206623E-16,1.)) ;
#36765 = DIRECTION('center_axis',(-1.75658099177411E-13,-1.,-1.66321791206623E-16)) ;
#36766 = DIRECTION('ref_axis',(-0.707106781186538,1.24091425832263E-13,0.707106781186557)) ;
#36767 = DIRECTION('',(1.,-1.75658099177411E-13,-4.54224185797219E-14)) ;
#36768 = DIRECTION('center_axis',(-1.75658099177411E-13,-1.,-1.66321791206623E-16)) ;
#36769 = DIRECTION('ref_axis',(0.707106781186554,-1.24326640365109E-13,0.707106781186541)) ;
#36770 = DIRECTION('',(2.92172610985041E-29,1.66321791206623E-16,-1.)) ;
#36771 = DIRECTION('center_axis',(1.75658099177411E-13,1.,1.66321791206623E-16)) ;
#36772 = DIRECTION('ref_axis',(-0.707106781186579,1.24326640365113E-13,-0.707106781186516)) ;
#36773 = DIRECTION('',(-1.,1.75658099177411E-13,4.54195640846217E-14)) ;
#36774 = DIRECTION('center_axis',(1.75658099177411E-13,1.,1.66321791206623E-16)) ;
#36775 = DIRECTION('ref_axis',(0.707106781186551,-1.24091425832266E-13,-0.707106781186544)) ;
#36776 = DIRECTION('',(-2.98822568073276E-29,-1.66321791206623E-16,1.)) ;
#36777 = DIRECTION('center_axis',(-1.75658099177411E-13,-1.,-1.66321791206623E-16)) ;
#36778 = DIRECTION('ref_axis',(-0.707106781186529,1.24091425832262E-13,0.707106781186566)) ;
#36779 = DIRECTION('',(1.,-1.75658099177411E-13,-4.53796366499639E-14)) ;
#36780 = DIRECTION('center_axis',(1.75658099177411E-13,1.,1.66321791206623E-16)) ;
#36781 = DIRECTION('ref_axis',(0.70710678118651,-1.24091425832259E-13,-0.707106781186585)) ;
#36782 = DIRECTION('center_axis',(1.75658099177411E-13,1.,1.66321791206623E-16)) ;
#36783 = DIRECTION('ref_axis',(-1.,1.75658099177411E-13,1.34042507393854E-33)) ;
#36784 = DIRECTION('center_axis',(1.75658099177411E-13,1.,1.66321791206623E-16)) ;
#36785 = DIRECTION('ref_axis',(-1.,1.75658099177411E-13,6.92942826962939E-35)) ;
#36786 = DIRECTION('center_axis',(-1.75744394921826E-13,-1.,-1.81854713288314E-16)) ;
#36787 = DIRECTION('ref_axis',(-0.707106781186529,1.2414146270379E-13,0.707106781186566)) ;
#36788 = DIRECTION('',(-1.75744394921826E-13,-1.,-1.81854713288314E-16)) ;
#36789 = DIRECTION('center_axis',(-1.75658099177411E-13,-1.,-1.66321791206623E-16)) ;
#36790 = DIRECTION('ref_axis',(-0.707106781186529,1.24091425832262E-13,0.707106781186566)) ;
#36791 = DIRECTION('',(1.75744394921826E-13,1.,1.81854713288314E-16)) ;
#36792 = DIRECTION('center_axis',(4.53796366499638E-14,-1.81854713296289E-16,
1.)) ;
#36793 = DIRECTION('ref_axis',(-1.,1.75658099177411E-13,4.53796366499638E-14)) ;
#36794 = DIRECTION('',(1.75658099177411E-13,1.,1.66321791206623E-16)) ;
#36795 = DIRECTION('',(1.,-1.75658099177411E-13,-4.54195640846217E-14)) ;
#36796 = DIRECTION('center_axis',(-1.75744394921826E-13,-1.,-1.81854713288314E-16)) ;
#36797 = DIRECTION('ref_axis',(-0.707106781186529,1.2414146270379E-13,0.707106781186566)) ;
#36798 = DIRECTION('',(-1.75744394921826E-13,-1.,-1.81854713288314E-16)) ;
#36799 = DIRECTION('',(1.75744394921826E-13,1.,1.81854713288314E-16)) ;
#36800 = DIRECTION('center_axis',(4.53796366499638E-14,-1.81854713296289E-16,
1.)) ;
#36801 = DIRECTION('ref_axis',(-1.,1.75658099177411E-13,4.53796366499638E-14)) ;
#36802 = DIRECTION('',(1.75658099177411E-13,1.,1.81854713288318E-16)) ;
#36803 = DIRECTION('center_axis',(-1.75658099177411E-13,-1.,-1.66321791206623E-16)) ;
#36804 = DIRECTION('ref_axis',(-0.707106781186507,1.24091425832258E-13,0.707106781186588)) ;
#36805 = DIRECTION('center_axis',(1.75658099177411E-13,1.,1.66321791206623E-16)) ;
#36806 = DIRECTION('ref_axis',(-0.707106781186507,1.24091425832258E-13,0.707106781186588)) ;
#36807 = DIRECTION('',(1.75658099177411E-13,1.,1.66321791206623E-16)) ;
#36808 = DIRECTION('center_axis',(-1.75658099177411E-13,-1.,-1.66321791206623E-16)) ;
#36809 = DIRECTION('ref_axis',(-0.707106781186507,1.24091425832258E-13,0.707106781186588)) ;
#36810 = DIRECTION('',(-1.75658099177411E-13,-1.,-1.66321791206623E-16)) ;
#36811 = DIRECTION('center_axis',(-1.75658099177411E-13,-1.,-1.66321791206623E-16)) ;
#36812 = DIRECTION('ref_axis',(1.,-1.75658099177411E-13,-4.54195640846217E-14)) ;
#36813 = DIRECTION('',(-1.,1.75658099177411E-13,4.54195640846217E-14)) ;
#36814 = DIRECTION('',(-4.54195640846217E-14,1.66321791214601E-16,-1.)) ;
#36815 = DIRECTION('',(1.,-1.75658099177411E-13,-4.54195640846217E-14)) ;
#36816 = DIRECTION('',(4.54195640846217E-14,-1.66321791214601E-16,1.)) ;
#36817 = DIRECTION('center_axis',(4.54195640846217E-14,-1.66321791214601E-16,
1.)) ;
#36818 = DIRECTION('ref_axis',(1.,-1.75658099177411E-13,-4.54195640846217E-14)) ;
#36819 = DIRECTION('',(1.,-1.75658099177411E-13,-4.54195640846217E-14)) ;
#36820 = DIRECTION('',(1.35690070290911E-13,1.,1.66321791208438E-16)) ;
#36821 = DIRECTION('',(-1.,5.13165898663611E-13,4.00690931964822E-13)) ;
#36822 = DIRECTION('',(-1.75658099177411E-13,-1.,-1.66321791206623E-16)) ;
#36823 = DIRECTION('',(1.,-1.75658099177411E-13,-4.36218068752822E-13)) ;
#36824 = DIRECTION('',(-4.59875193481411E-13,-1.,-1.66321791193714E-16)) ;
#36825 = DIRECTION('center_axis',(4.54195640846217E-14,-1.66321791214601E-16,
1.)) ;
#36826 = DIRECTION('ref_axis',(0.707106781186423,-0.707106781186672,-3.22340890291943E-14)) ;
#36827 = DIRECTION('center_axis',(4.54195640846217E-14,-1.66321791214601E-16,
1.)) ;
#36828 = DIRECTION('ref_axis',(-0.987708878702966,0.156304737392474,4.48873035970976E-14)) ;
#36829 = DIRECTION('center_axis',(4.54195640846217E-14,-1.66321791214601E-16,
1.)) ;
#36830 = DIRECTION('ref_axis',(-1.,5.55236256206829E-46,4.54195640846217E-14)) ;
#36831 = DIRECTION('center_axis',(4.54195640846217E-14,-1.66321791214601E-16,
1.)) ;
#36832 = DIRECTION('ref_axis',(0.156305321293456,-0.987708786300572,-7.26359705179142E-15)) ;
#36833 = DIRECTION('center_axis',(-4.54195640846217E-14,1.66321791214621E-16,
-1.)) ;
#36834 = DIRECTION('ref_axis',(1.,1.87077983243537E-9,-4.54195640843106E-14)) ;
#36835 = DIRECTION('center_axis',(-4.54195640846217E-14,1.66321791214621E-16,
-1.)) ;
#36836 = DIRECTION('ref_axis',(1.,1.75488086631674E-8,-4.54195640817029E-14)) ;
#36837 = DIRECTION('center_axis',(-4.54195640846217E-14,1.66321791214601E-16,
-1.)) ;
#36838 = DIRECTION('ref_axis',(-1.,2.41975421181691E-13,4.54195640846217E-14)) ;
#36839 = DIRECTION('',(1.75658099177411E-13,1.,1.66321791206623E-16)) ;
#36840 = DIRECTION('center_axis',(-4.54195640846217E-14,1.66321791214601E-16,
-1.)) ;
#36841 = DIRECTION('ref_axis',(1.,-9.98668740296709E-14,-4.54195640846217E-14)) ;
#36842 = DIRECTION('',(-1.75658099177411E-13,-1.,-1.66321791206623E-16)) ;
#36843 = DIRECTION('center_axis',(-4.54195640846217E-14,1.66321791214601E-16,
-1.)) ;
#36844 = DIRECTION('ref_axis',(-1.,2.41975421181691E-13,4.54195640846217E-14)) ;
#36845 = DIRECTION('',(1.75658099177411E-13,1.,1.66321791206623E-16)) ;
#36846 = DIRECTION('center_axis',(-4.54195640846217E-14,1.66321791214601E-16,
-1.)) ;
#36847 = DIRECTION('ref_axis',(1.,-9.98668740296709E-14,-4.54195640846217E-14)) ;
#36848 = DIRECTION('',(-1.75658099177411E-13,-1.,-1.66321791206623E-16)) ;
#36849 = DIRECTION('center_axis',(-4.54195640846217E-14,1.66321791214601E-16,
-1.)) ;
#36850 = DIRECTION('ref_axis',(-1.,2.41975421181691E-13,4.54195640846217E-14)) ;
#36851 = DIRECTION('',(1.75658099177411E-13,1.,1.66321791206623E-16)) ;
#36852 = DIRECTION('center_axis',(-4.54195640846217E-14,1.66321791214601E-16,
-1.)) ;
#36853 = DIRECTION('ref_axis',(1.,-9.98668740296709E-14,-4.54195640846217E-14)) ;
#36854 = DIRECTION('',(-1.75658099177411E-13,-1.,-1.66321791206623E-16)) ;
#36855 = DIRECTION('center_axis',(-4.54195640846217E-14,1.66321791214601E-16,
-1.)) ;
#36856 = DIRECTION('ref_axis',(-1.,2.41975421181691E-13,4.54195640846217E-14)) ;
#36857 = DIRECTION('',(1.75658099177411E-13,1.,1.66321791206623E-16)) ;
#36858 = DIRECTION('center_axis',(-4.54195640846217E-14,1.66321791214601E-16,
-1.)) ;
#36859 = DIRECTION('ref_axis',(1.,-1.09340777173131E-13,-4.54195640846217E-14)) ;
#36860 = DIRECTION('',(-1.75658099177411E-13,-1.,-1.66321791206623E-16)) ;
#36861 = DIRECTION('center_axis',(-4.54195640846217E-14,1.66321791214601E-16,
-1.)) ;
#36862 = DIRECTION('ref_axis',(1.,-1.09340777173131E-13,-4.54195640846217E-14)) ;
#36863 = DIRECTION('',(-1.75658099177411E-13,-1.,-1.66321791206623E-16)) ;
#36864 = DIRECTION('center_axis',(-4.54195640846217E-14,1.66321791214601E-16,
-1.)) ;
#36865 = DIRECTION('ref_axis',(-1.,2.41975421181691E-13,4.54195640846217E-14)) ;
#36866 = DIRECTION('',(1.75658099177411E-13,1.,1.66321791206623E-16)) ;
#36867 = DIRECTION('center_axis',(-4.54195640846217E-14,1.66321791214601E-16,
-1.)) ;
#36868 = DIRECTION('ref_axis',(-1.,2.41975421181691E-13,4.54195640846217E-14)) ;
#36869 = DIRECTION('',(1.75658099177411E-13,1.,1.66321791206623E-16)) ;
#36870 = DIRECTION('center_axis',(-4.54195640846217E-14,1.66321791214601E-16,
-1.)) ;
#36871 = DIRECTION('ref_axis',(1.,-1.09340777173131E-13,-4.54195640846217E-14)) ;
#36872 = DIRECTION('',(-1.75658099177411E-13,-1.,-1.66321791206623E-16)) ;
#36873 = DIRECTION('center_axis',(-4.54195640846217E-14,1.66321791214608E-16,
-1.)) ;
#36874 = DIRECTION('ref_axis',(0.707106781186672,0.707106781186423,-3.19988744963517E-14)) ;
#36875 = DIRECTION('center_axis',(-4.54195640846217E-14,1.66321791214608E-16,
-1.)) ;
#36876 = DIRECTION('ref_axis',(0.707106781186679,0.707106781186416,-3.1998874496352E-14)) ;
#36877 = DIRECTION('center_axis',(-4.54195640846217E-14,1.66321791214608E-16,
-1.)) ;
#36878 = DIRECTION('ref_axis',(-0.707106781186672,-0.707106781186423,3.19988744963517E-14)) ;
#36879 = DIRECTION('center_axis',(-4.54195640846217E-14,1.66321791214608E-16,
-1.)) ;
#36880 = DIRECTION('ref_axis',(-0.707106781186649,-0.707106781186446,3.19988744963507E-14)) ;
#36881 = DIRECTION('center_axis',(1.10810639983346E-16,4.54750752358529E-14,
1.)) ;
#36882 = DIRECTION('ref_axis',(-1.,1.75719331517368E-13,1.10810639975355E-16)) ;
#36883 = DIRECTION('center_axis',(4.54195640846217E-14,-1.66321791214601E-16,
1.)) ;
#36884 = DIRECTION('ref_axis',(-0.965925826289114,-0.258819045102351,4.38288827209477E-14)) ;
#36885 = DIRECTION('center_axis',(-4.54195640846217E-14,1.66321791214601E-16,
-1.)) ;
#36886 = DIRECTION('ref_axis',(-1.,1.75719331517368E-13,4.54195640846217E-14)) ;
#36887 = DIRECTION('center_axis',(4.54195640846217E-14,-1.66321791214601E-16,
1.)) ;
#36888 = DIRECTION('ref_axis',(-0.965925826289023,0.25881904510269,4.39149772153074E-14)) ;
#36889 = DIRECTION('center_axis',(4.54195640846217E-14,-1.66321791214602E-16,
1.)) ;
#36890 = DIRECTION('ref_axis',(-0.258819045102691,-0.965925826289023,1.15947936917534E-14)) ;
#36891 = DIRECTION('center_axis',(-2.21832942445859E-16,-4.54750752358529E-14,
1.)) ;
#36892 = DIRECTION('ref_axis',(-1.75780563857328E-13,-1.,-4.54750752358529E-14)) ;
#36893 = DIRECTION('center_axis',(4.54195640846217E-14,-1.66321791214602E-16,
1.)) ;
#36894 = DIRECTION('ref_axis',(0.258819045102351,-0.965925826289114,-1.19161027189557E-14)) ;
#36895 = DIRECTION('center_axis',(-4.54195640846217E-14,1.66321791214602E-16,
-1.)) ;
#36896 = DIRECTION('ref_axis',(-1.75780563857326E-13,-1.,-1.66321791206618E-16)) ;
#36897 = DIRECTION('center_axis',(4.54195640846217E-14,-1.66321791214601E-16,
1.)) ;
#36898 = DIRECTION('ref_axis',(0.965925826289023,-0.258819045102691,-4.39149772153074E-14)) ;
#36899 = DIRECTION('center_axis',(9.072831752926E-14,-4.58077188182821E-14,
1.)) ;
#36900 = DIRECTION('ref_axis',(1.,-1.75841796197283E-13,-9.07283175292681E-14)) ;
#36901 = DIRECTION('center_axis',(4.54195640846217E-14,-1.66321791214601E-16,
1.)) ;
#36902 = DIRECTION('ref_axis',(0.965925826289114,0.258819045102351,-4.38288827209477E-14)) ;
#36903 = DIRECTION('center_axis',(-4.54195640846217E-14,1.66321791214601E-16,
-1.)) ;
#36904 = DIRECTION('ref_axis',(1.,-1.75841796197283E-13,-4.54195640846217E-14)) ;
#36905 = DIRECTION('center_axis',(4.54195640846217E-14,-1.66321791214602E-16,
1.)) ;
#36906 = DIRECTION('ref_axis',(0.258819045102691,0.965925826289023,-1.15947936917534E-14)) ;
#36907 = DIRECTION('center_axis',(9.10609611116892E-14,4.51424316534237E-14,
1.)) ;
#36908 = DIRECTION('ref_axis',(1.75903028537238E-13,1.,-4.51424316534397E-14)) ;
#36909 = DIRECTION('center_axis',(4.54195640846217E-14,-1.66321791214602E-16,
1.)) ;
#36910 = DIRECTION('ref_axis',(-0.258819045102351,0.965925826289114,1.19161027189557E-14)) ;
#36911 = DIRECTION('center_axis',(-4.54195640846217E-14,1.66321791214602E-16,
-1.)) ;
#36912 = DIRECTION('ref_axis',(1.7590302853724E-13,1.,1.66321791206613E-16)) ;
#36913 = DIRECTION('center_axis',(4.54195640846217E-14,-1.66321791214602E-16,
1.)) ;
#36914 = DIRECTION('ref_axis',(0.707106781186672,0.707106781186423,-3.19988744963517E-14)) ;
#36915 = DIRECTION('center_axis',(4.54195640846217E-14,-1.66321791214601E-16,
1.)) ;
#36916 = DIRECTION('ref_axis',(-0.156304737392422,-0.987708878702974,6.93501552682063E-15)) ;
#36917 = DIRECTION('center_axis',(4.54195640846217E-14,-1.66321791214601E-16,
1.)) ;
#36918 = DIRECTION('ref_axis',(-1.,5.55236256206829E-46,4.54195640846217E-14)) ;
#36919 = DIRECTION('center_axis',(4.54195640846217E-14,-1.66321791214601E-16,
1.)) ;
#36920 = DIRECTION('ref_axis',(0.987707474797848,0.156313608583704,-4.48352445890699E-14)) ;
#36921 = DIRECTION('center_axis',(4.54195640846217E-14,-1.66321791214601E-16,
1.)) ;
#36922 = DIRECTION('ref_axis',(-0.707106781186423,0.707106781186672,3.22340890291943E-14)) ;
#36923 = DIRECTION('center_axis',(4.54195640846217E-14,-1.66321791214601E-16,
1.)) ;
#36924 = DIRECTION('ref_axis',(0.987708878702962,-0.1563047373925,-4.48873035970975E-14)) ;
#36925 = DIRECTION('center_axis',(4.54195640846217E-14,-1.66321791214601E-16,
1.)) ;
#36926 = DIRECTION('ref_axis',(-1.,5.55236256206829E-46,4.54195640846217E-14)) ;
#36927 = DIRECTION('center_axis',(4.54195640846217E-14,-1.66321791214602E-16,
1.)) ;
#36928 = DIRECTION('ref_axis',(-0.707106781186672,-0.707106781186423,3.19988744963517E-14)) ;
#36929 = DIRECTION('center_axis',(4.54195640846217E-14,-1.66321791214601E-16,
1.)) ;
#36930 = DIRECTION('ref_axis',(0.156304737392435,0.987708878702972,-6.93501552682122E-15)) ;
#36931 = DIRECTION('center_axis',(4.54195640846217E-14,-1.66321791214601E-16,
1.)) ;
#36932 = DIRECTION('ref_axis',(-1.,5.55236256206829E-46,4.54195640846217E-14)) ;
#36933 = DIRECTION('center_axis',(1.75658099177411E-13,1.,1.66321791206623E-16)) ;
#36934 = DIRECTION('ref_axis',(-4.54195640846217E-14,1.66321791214601E-16,
-1.)) ;
#36935 = DIRECTION('center_axis',(1.75658099177411E-13,1.,1.66321791206623E-16)) ;
#36936 = DIRECTION('ref_axis',(-0.707106781186561,1.2432664036511E-13,-0.707106781186534)) ;
#36937 = DIRECTION('',(-1.,1.75658099177411E-13,0.)) ;
#36938 = DIRECTION('center_axis',(1.75658099177411E-13,1.,1.66321791206623E-16)) ;
#36939 = DIRECTION('ref_axis',(0.707106781186549,-1.24091425832265E-13,-0.707106781186546)) ;
#36940 = DIRECTION('',(2.92157696951376E-29,1.66321791206623E-16,-1.)) ;
#36941 = DIRECTION('center_axis',(-1.75658099177411E-13,-1.,-1.66321791206623E-16)) ;
#36942 = DIRECTION('ref_axis',(-0.707106781186535,1.24091425832263E-13,0.70710678118656)) ;
#36943 = DIRECTION('',(1.,-1.75658099177411E-13,-4.54195640846217E-14)) ;
#36944 = DIRECTION('center_axis',(-1.75658099177411E-13,-1.,-1.66321791206623E-16)) ;
#36945 = DIRECTION('ref_axis',(0.707106781186551,-1.24326640365108E-13,0.707106781186544)) ;
#36946 = DIRECTION('',(-1.35951365453452E-28,-1.66321791206623E-16,1.)) ;
#36947 = DIRECTION('center_axis',(1.75658099177411E-13,1.,1.66321791206623E-16)) ;
#36948 = DIRECTION('ref_axis',(-0.707106781186551,1.24326640365108E-13,-0.707106781186544)) ;
#36949 = DIRECTION('',(-1.,1.75658099177411E-13,0.)) ;
#36950 = DIRECTION('center_axis',(1.75658099177411E-13,1.,1.66321791206623E-16)) ;
#36951 = DIRECTION('ref_axis',(0.707106781186551,-1.24091425832266E-13,-0.707106781186544)) ;
#36952 = DIRECTION('',(1.35951365453457E-28,1.66321791206623E-16,-1.)) ;
#36953 = DIRECTION('center_axis',(1.75658099177411E-13,1.,1.66321791206623E-16)) ;
#36954 = DIRECTION('ref_axis',(0.70710678118651,-1.24091425832259E-13,-0.707106781186585)) ;
#36955 = DIRECTION('',(4.54195640846217E-14,-1.66321791214601E-16,1.)) ;
#36956 = DIRECTION('center_axis',(1.75658099177411E-13,1.,1.66321791206623E-16)) ;
#36957 = DIRECTION('ref_axis',(0.99999997726804,-1.75658059720777E-13,-0.000213222701069828)) ;
#36958 = DIRECTION('center_axis',(1.75658099177411E-13,1.,1.66321791206623E-16)) ;
#36959 = DIRECTION('ref_axis',(-1.,1.75658099177411E-13,-8.27097305203856E-32)) ;
#36960 = DIRECTION('center_axis',(1.,-1.75658099177411E-13,-4.54195640846217E-14)) ;
#36961 = DIRECTION('ref_axis',(-4.54195640846217E-14,1.66321791214601E-16,
-1.)) ;
#36962 = DIRECTION('',(4.54195640846217E-14,-1.66321791214601E-16,1.)) ;
#36963 = DIRECTION('center_axis',(-1.,1.75658099177411E-13,4.54195640846217E-14)) ;
#36964 = DIRECTION('ref_axis',(-1.56325514861457E-13,-0.707106781186529,-0.707106781186566)) ;
#36965 = DIRECTION('',(-1.75658099177411E-13,-1.,-1.66321791206623E-16)) ;
#36966 = DIRECTION('center_axis',(-1.,1.75658099177411E-13,4.54195640846217E-14)) ;
#36967 = DIRECTION('ref_axis',(9.20925513359107E-14,0.707106781186535,-0.70710678118656)) ;
#36968 = DIRECTION('center_axis',(6.65065844402311E-14,-2.78565702539647E-14,
1.)) ;
#36969 = DIRECTION('ref_axis',(-0.987708878702966,0.156304737392474,7.00432578420257E-14)) ;
#36970 = DIRECTION('',(4.44089209850064E-14,0.,1.)) ;
#36971 = DIRECTION('',(5.41996232473793E-14,-2.07511428963625E-14,1.)) ;
#36972 = DIRECTION('center_axis',(-4.44089209850064E-14,0.,-1.)) ;
#36973 = DIRECTION('ref_axis',(-1.,0.,4.44089209850064E-14)) ;
#36974 = DIRECTION('',(-4.44089209850064E-14,0.,-1.)) ;
#36975 = DIRECTION('center_axis',(-5.83947887444131E-11,-9.23392314221282E-12,
-1.)) ;
#36976 = DIRECTION('ref_axis',(0.987707474797848,0.156313608583704,-5.91203571798419E-11)) ;
#36977 = DIRECTION('',(-4.44089209850062E-14,0.,-1.)) ;
#36978 = DIRECTION('',(7.99435328682709E-14,4.25044929548771E-15,1.)) ;
#36979 = DIRECTION('center_axis',(-4.44089209850062E-14,0.,-1.)) ;
#36980 = DIRECTION('ref_axis',(-1.,0.,4.44089209850062E-14)) ;
#36981 = DIRECTION('',(4.44089209850062E-14,0.,1.)) ;
#36982 = DIRECTION('center_axis',(7.31098125473717E-14,2.09206985643948E-14,
1.)) ;
#36983 = DIRECTION('ref_axis',(-0.156304737392422,-0.987708878702974,3.20909697717474E-14)) ;
#36984 = DIRECTION('',(6.60043851897696E-14,8.613737371543E-15,1.)) ;
#36985 = DIRECTION('',(-6.91631936757579E-11,4.36746934819318E-10,-1.)) ;
#36986 = DIRECTION('',(6.94007814181027E-10,-4.38310128933186E-9,1.)) ;
#36987 = DIRECTION('center_axis',(-4.44089209850062E-14,0.,-1.)) ;
#36988 = DIRECTION('ref_axis',(-1.,0.,4.44089209850062E-14)) ;
#36989 = DIRECTION('',(4.44089209850062E-14,0.,1.)) ;
#36990 = DIRECTION('center_axis',(2.43325437290122E-14,2.75239266715355E-14,
1.)) ;
#36991 = DIRECTION('ref_axis',(0.987708878702962,-0.1563047373925,-1.97313493521686E-14)) ;
#36992 = DIRECTION('',(3.66395049218641E-14,2.04184993139333E-14,1.)) ;
#36993 = DIRECTION('',(6.34499860060004E-10,1.00068101952864E-10,-1.)) ;
#36994 = DIRECTION('',(5.64924462358365E-13,1.34783525161202E-13,1.)) ;
#36995 = DIRECTION('center_axis',(-4.44089209850062E-14,0.,-1.)) ;
#36996 = DIRECTION('ref_axis',(-1.,0.,4.44089209850062E-14)) ;
#36997 = DIRECTION('',(4.44089209850062E-14,0.,1.)) ;
#36998 = DIRECTION('center_axis',(1.77293156218716E-14,-2.1253342146824E-14,
1.)) ;
#36999 = DIRECTION('ref_axis',(0.156304737392435,0.987708878702972,1.82209387181059E-14)) ;
#37000 = DIRECTION('',(2.48347429794738E-14,-8.94638095397221E-15,1.)) ;
#37001 = DIRECTION('center_axis',(-8.03175469292822E-12,5.04730250306102E-11,
-1.)) ;
#37002 = DIRECTION('ref_axis',(0.156305321293456,-0.987708786300572,-5.11080562917308E-11)) ;
#37003 = DIRECTION('',(-8.95302828677947E-14,5.19338576482528E-13,1.)) ;
#37004 = DIRECTION('center_axis',(1.,-1.75658099177411E-13,-4.54195640846217E-14)) ;
#37005 = DIRECTION('ref_axis',(9.20925513359107E-14,0.707106781186535,-0.70710678118656)) ;
#37006 = DIRECTION('',(-1.,1.75658099177411E-13,4.54195640846217E-14)) ;
#37007 = DIRECTION('center_axis',(1.,-1.75658099177411E-13,-4.54195640846217E-14)) ;
#37008 = DIRECTION('ref_axis',(9.20925513359107E-14,0.707106781186535,-0.70710678118656)) ;
#37009 = DIRECTION('center_axis',(4.54195640846217E-14,-1.66321791214601E-16,
1.)) ;
#37010 = DIRECTION('ref_axis',(-1.,1.75658099177411E-13,4.54195640846217E-14)) ;
#37011 = DIRECTION('',(1.,-1.75658099177411E-13,-4.54195640846217E-14)) ;
#37012 = DIRECTION('',(1.75658099177411E-13,1.,1.66321791206623E-16)) ;
#37013 = DIRECTION('center_axis',(1.,-1.75658099177411E-13,-4.54195640846217E-14)) ;
#37014 = DIRECTION('ref_axis',(-1.56325514861457E-13,-0.707106781186529,-0.707106781186566)) ;
#37015 = DIRECTION('',(-1.,1.75658099177411E-13,4.54195640846217E-14)) ;
#37016 = DIRECTION('center_axis',(1.,-1.75658099177411E-13,-4.54195640846217E-14)) ;
#37017 = DIRECTION('ref_axis',(-1.56325514861457E-13,-0.707106781186529,-0.707106781186566)) ;
#37018 = DIRECTION('center_axis',(1.75658099177411E-13,1.,1.66321791206623E-16)) ;
#37019 = DIRECTION('ref_axis',(-1.,1.75658099177411E-13,4.54195640846217E-14)) ;
#37020 = DIRECTION('',(-4.54195640846217E-14,1.66321791214601E-16,-1.)) ;
#37021 = DIRECTION('',(-4.54195640846217E-14,1.66321791214601E-16,-1.)) ;
#37022 = DIRECTION('center_axis',(1.75658099177411E-13,1.,1.81854713288318E-16)) ;
#37023 = DIRECTION('ref_axis',(0.70710678118651,-1.24080442397723E-13,-0.707106781186585)) ;
#37024 = DIRECTION('center_axis',(-1.,1.75658099177411E-13,4.54195640846217E-14)) ;
#37025 = DIRECTION('ref_axis',(-1.56325514861457E-13,-0.707106781186529,-0.707106781186566)) ;
#37026 = DIRECTION('center_axis',(1.,-1.75658099177411E-13,-4.54195640846217E-14)) ;
#37027 = DIRECTION('ref_axis',(-1.56325514861457E-13,-0.707106781186529,-0.707106781186566)) ;
#37028 = DIRECTION('',(1.,-1.75658099177411E-13,-4.54195640846217E-14)) ;
#37029 = DIRECTION('center_axis',(-1.,1.75658099177411E-13,4.54195640846217E-14)) ;
#37030 = DIRECTION('ref_axis',(-1.56325514861457E-13,-0.707106781186529,-0.707106781186566)) ;
#37031 = DIRECTION('',(-1.,1.75658099177411E-13,4.54195640846217E-14)) ;
#37032 = DIRECTION('center_axis',(4.54195640846217E-14,-1.66321791214601E-16,
1.)) ;
#37033 = DIRECTION('ref_axis',(-1.75658099177411E-13,-1.,-1.66321791206623E-16)) ;
#37034 = DIRECTION('',(-1.75658099177411E-13,-1.,-1.66321791206623E-16)) ;
#37035 = DIRECTION('',(-1.,1.75658099177411E-13,4.54195640846217E-14)) ;
#37036 = DIRECTION('',(-1.75658099177411E-13,-1.,-1.66321791206623E-16)) ;
#37037 = DIRECTION('center_axis',(1.,-1.75658099177411E-13,-4.54195640846217E-14)) ;
#37038 = DIRECTION('ref_axis',(-4.54195640846217E-14,1.66321791214601E-16,
-1.)) ;
#37039 = DIRECTION('',(4.54195640846217E-14,-1.66321791214601E-16,1.)) ;
#37040 = DIRECTION('',(-1.75658099177411E-13,-1.,-1.66321791206623E-16)) ;
#37041 = DIRECTION('',(-4.54195640846217E-14,1.66321791214601E-16,-1.)) ;
#37042 = DIRECTION('center_axis',(1.,-1.75658099177411E-13,-4.54195640846217E-14)) ;
#37043 = DIRECTION('ref_axis',(9.20925513359094E-14,0.707106781186529,-0.707106781186566)) ;
#37044 = DIRECTION('center_axis',(1.,-1.75658099177411E-13,-4.54195640846217E-14)) ;
#37045 = DIRECTION('ref_axis',(9.20925513359094E-14,0.707106781186529,-0.707106781186566)) ;
#37046 = DIRECTION('center_axis',(-1.,1.75658099177411E-13,4.54195640846217E-14)) ;
#37047 = DIRECTION('ref_axis',(9.20925513359094E-14,0.707106781186529,-0.707106781186566)) ;
#37048 = DIRECTION('',(1.,-1.75658099177411E-13,-4.54195640846217E-14)) ;
#37049 = DIRECTION('center_axis',(-1.75658099177411E-13,-1.,-1.66321791206623E-16)) ;
#37050 = DIRECTION('ref_axis',(1.,-1.75658099177411E-13,-4.54195640846217E-14)) ;
#37051 = DIRECTION('center_axis',(1.75658099177411E-13,1.,1.66321791206623E-16)) ;
#37052 = DIRECTION('ref_axis',(8.33151766584917E-14,-1.66321791221258E-16,
1.)) ;
#37053 = DIRECTION('',(-4.54195640846217E-14,1.66321791214601E-16,-1.)) ;
#37054 = DIRECTION('center_axis',(1.75658099177411E-13,1.,1.66321791206623E-16)) ;
#37055 = DIRECTION('ref_axis',(0.707106781186548,-1.24326640365108E-13,0.707106781186548)) ;
#37056 = DIRECTION('',(4.54195640846217E-14,-1.66321791214601E-16,1.)) ;
#37057 = DIRECTION('center_axis',(-1.75658099177411E-13,-1.,-1.66321791206623E-16)) ;
#37058 = DIRECTION('ref_axis',(0.70710678118651,-1.24091425832259E-13,-0.707106781186585)) ;
#37059 = DIRECTION('',(-1.75658099177411E-13,-1.,-1.66321791206623E-16)) ;
#37060 = DIRECTION('center_axis',(-1.,1.75658099177411E-13,4.54195640846217E-14)) ;
#37061 = DIRECTION('ref_axis',(-1.75658099177411E-13,-1.,-1.66321791206623E-16)) ;
#37062 = DIRECTION('center_axis',(-1.75744394921826E-13,-1.,-1.66321791206619E-16)) ;
#37063 = DIRECTION('ref_axis',(0.707106781186551,-1.24152446138329E-13,-0.707106781186544)) ;
#37064 = DIRECTION('',(1.75744394921826E-13,1.,1.66321791206619E-16)) ;
#37065 = DIRECTION('',(-1.75744394921826E-13,-1.,-1.66321791206619E-16)) ;
#37066 = DIRECTION('center_axis',(4.54195640846217E-14,-1.66321791214601E-16,
1.)) ;
#37067 = DIRECTION('ref_axis',(-1.,1.75658099177411E-13,4.54195640846217E-14)) ;
#37068 = DIRECTION('',(-1.72252784426699E-13,-1.,-1.66321791206777E-16)) ;
#37069 = DIRECTION('center_axis',(-1.72252784426699E-13,-1.,0.)) ;
#37070 = DIRECTION('ref_axis',(0.707106781186554,-1.21801111946385E-13,0.707106781186541)) ;
#37071 = DIRECTION('',(-1.72252784426699E-13,-1.,0.)) ;
#37072 = DIRECTION('',(1.72252784426699E-13,1.,0.)) ;
#37073 = DIRECTION('center_axis',(1.,-1.72252784426699E-13,5.67869452327227E-31)) ;
#37074 = DIRECTION('ref_axis',(-2.92172610985041E-29,-1.66321791206623E-16,
1.)) ;
#37075 = DIRECTION('',(1.72252784426699E-13,1.,1.66321791206777E-16)) ;
#37076 = DIRECTION('center_axis',(1.72252784426699E-13,1.,1.66321791206777E-16)) ;
#37077 = DIRECTION('ref_axis',(-0.707106781186579,1.2191871921281E-13,-0.707106781186516)) ;
#37078 = DIRECTION('center_axis',(-1.72252784426699E-13,-1.,-1.66321791206777E-16)) ;
#37079 = DIRECTION('ref_axis',(0.707106781186529,-1.21683504679959E-13,-0.707106781186566)) ;
#37080 = DIRECTION('',(1.72252784426699E-13,1.,1.66321791206777E-16)) ;
#37081 = DIRECTION('',(-1.72252784426699E-13,-1.,-1.66321791206777E-16)) ;
#37082 = DIRECTION('center_axis',(4.54195640846217E-14,-1.66321791214601E-16,
1.)) ;
#37083 = DIRECTION('ref_axis',(-1.,1.75658099177411E-13,4.54195640846217E-14)) ;
#37084 = DIRECTION('',(-1.75658099177411E-13,-1.,-1.66321791206623E-16)) ;
#37085 = DIRECTION('center_axis',(-1.72252784426699E-13,-1.,0.)) ;
#37086 = DIRECTION('ref_axis',(-0.707106781186538,1.21801111946382E-13,0.707106781186557)) ;
#37087 = DIRECTION('',(-1.72252784426699E-13,-1.,0.)) ;
#37088 = DIRECTION('',(1.72252784426699E-13,1.,0.)) ;
#37089 = DIRECTION('center_axis',(4.54224185797219E-14,-7.82413807575213E-27,
1.)) ;
#37090 = DIRECTION('ref_axis',(-1.,1.75658099177411E-13,4.54224185797219E-14)) ;
#37091 = DIRECTION('center_axis',(1.75658099177411E-13,1.,1.66321791206623E-16)) ;
#37092 = DIRECTION('ref_axis',(-0.70710678118658,1.24326640365113E-13,-0.707106781186515)) ;
#37093 = DIRECTION('',(1.75658099177411E-13,1.,1.66321791206623E-16)) ;
#37094 = DIRECTION('center_axis',(1.7578531223231E-13,1.,1.66321791206617E-16)) ;
#37095 = DIRECTION('ref_axis',(-0.707106781186535,1.24181379046037E-13,0.70710678118656)) ;
#37096 = DIRECTION('',(1.7578531223231E-13,1.,1.66321791206617E-16)) ;
#37097 = DIRECTION('',(-1.7578531223231E-13,-1.,-1.66321791206617E-16)) ;
#37098 = DIRECTION('center_axis',(1.,-1.7578531223231E-13,-2.11583031556481E-32)) ;
#37099 = DIRECTION('ref_axis',(-2.92157696951377E-29,-1.66321791206623E-16,
1.)) ;
#37100 = DIRECTION('',(-1.7578531223231E-13,-1.,0.)) ;
#37101 = DIRECTION('center_axis',(-1.7578531223231E-13,-1.,0.)) ;
#37102 = DIRECTION('ref_axis',(0.707106781186549,-1.24298986312461E-13,-0.707106781186546)) ;
#37103 = DIRECTION('',(1.7578531223231E-13,1.,0.)) ;
#37104 = DIRECTION('center_axis',(0.,0.,-1.)) ;
#37105 = DIRECTION('ref_axis',(1.,-1.75658099177411E-13,0.)) ;
#37106 = DIRECTION('',(-1.75658099177411E-13,-1.,0.)) ;
#37107 = DIRECTION('center_axis',(1.75658099177411E-13,1.,0.)) ;
#37108 = DIRECTION('ref_axis',(-0.707106781186561,1.24209033098689E-13,-0.707106781186534)) ;
#37109 = DIRECTION('center_axis',(-1.89478062869335E-13,-1.,-1.66321791205995E-16)) ;
#37110 = DIRECTION('ref_axis',(0.707106781186551,-1.34098830407419E-13,0.707106781186544)) ;
#37111 = DIRECTION('',(-1.89478062869335E-13,-1.,-1.66321791205995E-16)) ;
#37112 = DIRECTION('',(1.89478062869335E-13,1.,1.66321791205995E-16)) ;
#37113 = DIRECTION('center_axis',(-1.,1.89478062869335E-13,-1.04437034642664E-28)) ;
#37114 = DIRECTION('ref_axis',(-1.32744277756505E-27,-7.55696881488144E-15,
-1.)) ;
#37115 = DIRECTION('',(1.89478062869335E-13,1.,0.)) ;
#37116 = DIRECTION('center_axis',(-1.89478062869335E-13,-1.,0.)) ;
#37117 = DIRECTION('ref_axis',(-0.707106781186551,1.33981223140998E-13,-0.707106781186544)) ;
#37118 = DIRECTION('',(-1.89478062869335E-13,-1.,0.)) ;
#37119 = DIRECTION('center_axis',(-1.,1.75744394921826E-13,-6.52134249405362E-31)) ;
#37120 = DIRECTION('ref_axis',(-1.32744277756511E-27,-7.55696881488181E-15,
-1.)) ;
#37121 = DIRECTION('',(-1.89478062869335E-13,-1.,0.)) ;
#37122 = DIRECTION('center_axis',(-1.89478062869335E-13,-1.,0.)) ;
#37123 = DIRECTION('ref_axis',(0.707106781186551,-1.33981223140998E-13,-0.707106781186544)) ;
#37124 = DIRECTION('',(1.89478062869335E-13,1.,0.)) ;
#37125 = DIRECTION('center_axis',(0.,0.,-1.)) ;
#37126 = DIRECTION('ref_axis',(1.,-1.75658099177411E-13,0.)) ;
#37127 = DIRECTION('center_axis',(-1.75658099177411E-13,-1.,-1.66321791206623E-16)) ;
#37128 = DIRECTION('ref_axis',(0.707106781186548,-1.24326640365108E-13,0.707106781186548)) ;
#37129 = DIRECTION('center_axis',(-1.75658099177411E-13,-1.,-1.66321791206623E-16)) ;
#37130 = DIRECTION('ref_axis',(0.707106781186548,-1.24326640365108E-13,0.707106781186548)) ;
#37131 = DIRECTION('center_axis',(1.75658099177411E-13,1.,1.66321791206623E-16)) ;
#37132 = DIRECTION('ref_axis',(-1.,1.75658099177411E-13,4.54195640846217E-14)) ;
#37133 = DIRECTION('',(-4.54195640846217E-14,1.66321791214601E-16,-1.)) ;
#37134 = DIRECTION('center_axis',(-1.75658099177411E-13,-1.,-1.66321791206623E-16)) ;
#37135 = DIRECTION('ref_axis',(1.,-1.75658099177411E-13,9.19520314956783E-14)) ;
#37136 = DIRECTION('center_axis',(1.,-1.75658099177411E-13,-4.54195640846217E-14)) ;
#37137 = DIRECTION('ref_axis',(1.75658099177411E-13,1.,1.66321791206623E-16)) ;
#37138 = DIRECTION('center_axis',(-1.,1.75744394921826E-13,-6.52134249405362E-31)) ;
#37139 = DIRECTION('ref_axis',(-1.32744277756511E-27,-7.55696881488181E-15,
-1.)) ;
#37140 = DIRECTION('center_axis',(-1.75662560300847E-13,-1.,-1.81854713288314E-16)) ;
#37141 = DIRECTION('ref_axis',(-1.,1.75662560300847E-13,8.11276323366632E-34)) ;
#37142 = DIRECTION('',(-1.75662560300847E-13,-1.,-1.81854713288314E-16)) ;
#37143 = DIRECTION('center_axis',(-1.75744394921827E-13,-1.,-1.81854713288314E-16)) ;
#37144 = DIRECTION('ref_axis',(-1.,1.75744394921827E-13,1.5693287858714E-32)) ;
#37145 = DIRECTION('',(-1.75744394921827E-13,-1.,-1.81854713288314E-16)) ;
#37146 = DIRECTION('center_axis',(-1.,1.72252784426699E-13,-5.66378048960696E-31)) ;
#37147 = DIRECTION('ref_axis',(2.92157696951376E-29,1.66321791206623E-16,
-1.)) ;
#37148 = DIRECTION('center_axis',(-1.76155386573851E-13,-1.,0.)) ;
#37149 = DIRECTION('ref_axis',(-1.,1.76155386573851E-13,-4.62820191398731E-45)) ;
#37150 = DIRECTION('',(-1.76155386573851E-13,-1.,0.)) ;
#37151 = DIRECTION('center_axis',(1.34675317711724E-14,5.56466506464699E-14,
1.)) ;
#37152 = DIRECTION('ref_axis',(0.529493733640589,0.848313848782011,-5.43367980621762E-14)) ;
#37153 = DIRECTION('',(-7.72202224608625E-14,-2.9357493141945E-13,-1.)) ;
#37154 = DIRECTION('',(2.44508561928056E-14,1.26579979998417E-14,-1.)) ;
#37155 = DIRECTION('center_axis',(-1.01581938202089E-14,3.21931140438162E-14,
1.)) ;
#37156 = DIRECTION('ref_axis',(0.52949373364028,-0.848313848782204,3.26885644516982E-14)) ;
#37157 = DIRECTION('',(7.61868634881669E-14,-1.32198060448311E-13,-1.)) ;
#37158 = DIRECTION('',(1.05568025685331E-13,-2.8988996425453E-13,1.)) ;
#37159 = DIRECTION('center_axis',(1.10810639983346E-16,4.54750752358529E-14,
1.)) ;
#37160 = DIRECTION('ref_axis',(-1.,1.75719331517368E-13,1.10810639975355E-16)) ;
#37161 = DIRECTION('center_axis',(1.10810639983346E-16,4.54750752358529E-14,
1.)) ;
#37162 = DIRECTION('ref_axis',(-1.,1.75719331517368E-13,1.10810639975355E-16)) ;
#37163 = DIRECTION('center_axis',(4.10027929979194E-14,3.43576469924347E-14,
1.)) ;
#37164 = DIRECTION('ref_axis',(-0.499999999999848,0.866025403784526,-9.253198610756E-15)) ;
#37165 = DIRECTION('center_axis',(4.54195640846217E-14,-1.66321791214621E-16,
1.)) ;
#37166 = DIRECTION('ref_axis',(1.,-1.75824632631105E-13,-4.54195640846217E-14)) ;
#37167 = DIRECTION('',(-0.707106781186515,1.24122587161037E-13,0.70710678118658)) ;
#37168 = DIRECTION('center_axis',(4.54195640846217E-14,-1.66321791214621E-16,
1.)) ;
#37169 = DIRECTION('ref_axis',(1.,-1.75824632631105E-13,-4.54195640846217E-14)) ;
#37170 = DIRECTION('',(-0.707106781186515,1.24122587161037E-13,0.70710678118658)) ;
#37171 = DIRECTION('center_axis',(4.54195640846217E-14,-1.66321791214601E-16,
1.)) ;
#37172 = DIRECTION('ref_axis',(-1.,1.75658099177411E-13,4.54195640846217E-14)) ;
#37173 = DIRECTION('center_axis',(1.,-1.75658099177411E-13,-4.54195640846217E-14)) ;
#37174 = DIRECTION('ref_axis',(-4.54195640846217E-14,0.,-1.)) ;
#37175 = DIRECTION('center_axis',(4.54195640846217E-14,-1.66321791214608E-16,
1.)) ;
#37176 = DIRECTION('ref_axis',(0.707106781186672,0.707106781186423,-3.19988744963517E-14)) ;
#37177 = DIRECTION('',(4.54195640846217E-14,-1.66321791214608E-16,1.)) ;
#37178 = DIRECTION('center_axis',(4.54195640846217E-14,-1.66321791214608E-16,
1.)) ;
#37179 = DIRECTION('ref_axis',(0.707106781186672,0.707106781186423,-3.19988744963517E-14)) ;
#37180 = DIRECTION('',(4.54195640846217E-14,-1.66321791214608E-16,1.)) ;
#37181 = DIRECTION('center_axis',(4.54195640846217E-14,-1.66321791214608E-16,
1.)) ;
#37182 = DIRECTION('ref_axis',(0.707106781186672,0.707106781186423,-3.19988744963517E-14)) ;
#37183 = DIRECTION('',(4.54195640846217E-14,-1.66321791214608E-16,1.)) ;
#37184 = DIRECTION('center_axis',(4.54195640846217E-14,-1.66321791214608E-16,
1.)) ;
#37185 = DIRECTION('ref_axis',(0.707106781186672,0.707106781186423,-3.19988744963517E-14)) ;
#37186 = DIRECTION('',(4.54195640846217E-14,-1.66321791214608E-16,1.)) ;
#37187 = DIRECTION('center_axis',(4.54195640846217E-14,-1.66321791214601E-16,
1.)) ;
#37188 = DIRECTION('ref_axis',(-1.89547329362678E-13,-1.,-1.66321791205992E-16)) ;
#37189 = DIRECTION('',(-4.54195640846217E-14,1.66321791214602E-16,-1.)) ;
#37190 = DIRECTION('',(4.54195640846217E-14,-1.66321791214602E-16,1.)) ;
#37191 = DIRECTION('center_axis',(1.,-1.75658099177411E-13,-4.54195640846217E-14)) ;
#37192 = DIRECTION('ref_axis',(-4.54195640846217E-14,1.66321791214601E-16,
-1.)) ;
#37193 = DIRECTION('',(4.54195640846217E-14,-1.66321791214602E-16,1.)) ;
#37194 = DIRECTION('center_axis',(4.54195640846217E-14,-1.66321791214601E-16,
1.)) ;
#37195 = DIRECTION('ref_axis',(1.75658099177411E-13,1.,1.66321791206623E-16)) ;
#37196 = DIRECTION('',(-4.54195640846217E-14,1.66321791214602E-16,-1.)) ;
#37197 = DIRECTION('center_axis',(-1.,1.75658099177411E-13,4.54195640846217E-14)) ;
#37198 = DIRECTION('ref_axis',(4.54195640846217E-14,-1.66321791214601E-16,
1.)) ;
#37199 = DIRECTION('center_axis',(4.54195640846217E-14,-1.66321791214601E-16,
1.)) ;
#37200 = DIRECTION('ref_axis',(1.75658099177411E-13,1.,1.66321791206623E-16)) ;
#37201 = DIRECTION('',(-4.54195640846217E-14,1.66321791214602E-16,-1.)) ;
#37202 = DIRECTION('',(4.54195640846217E-14,-1.66321791214602E-16,1.)) ;
#37203 = DIRECTION('center_axis',(-1.,1.75658099177411E-13,4.54195640846217E-14)) ;
#37204 = DIRECTION('ref_axis',(4.54195640846217E-14,-1.66321791214601E-16,
1.)) ;
#37205 = DIRECTION('',(4.54195640846217E-14,-1.66321791214602E-16,1.)) ;
#37206 = DIRECTION('center_axis',(4.54195640846217E-14,-1.66321791214601E-16,
1.)) ;
#37207 = DIRECTION('ref_axis',(-1.66010601240624E-13,-1.,-1.66321791207061E-16)) ;
#37208 = DIRECTION('',(-4.54195640846217E-14,1.66321791214602E-16,-1.)) ;
#37209 = DIRECTION('center_axis',(1.,-1.75658099177411E-13,-4.54195640846217E-14)) ;
#37210 = DIRECTION('ref_axis',(-4.54195640846217E-14,1.66321791214601E-16,
-1.)) ;
#37211 = DIRECTION('center_axis',(4.54195640846217E-14,-1.66321791214601E-16,
1.)) ;
#37212 = DIRECTION('ref_axis',(-1.89547329362678E-13,-1.,-1.66321791205992E-16)) ;
#37213 = DIRECTION('',(-4.54195640846217E-14,1.66321791214602E-16,-1.)) ;
#37214 = DIRECTION('',(4.54195640846217E-14,-1.66321791214602E-16,1.)) ;
#37215 = DIRECTION('center_axis',(1.,-1.75658099177411E-13,-4.54195640846217E-14)) ;
#37216 = DIRECTION('ref_axis',(-4.54195640846217E-14,1.66321791214601E-16,
-1.)) ;
#37217 = DIRECTION('',(4.54195640846217E-14,-1.66321791214602E-16,1.)) ;
#37218 = DIRECTION('center_axis',(4.54195640846217E-14,-1.66321791214601E-16,
1.)) ;
#37219 = DIRECTION('ref_axis',(1.75658099177411E-13,1.,1.66321791206623E-16)) ;
#37220 = DIRECTION('',(-4.54195640846217E-14,1.66321791214602E-16,-1.)) ;
#37221 = DIRECTION('center_axis',(-1.,1.75658099177411E-13,4.54195640846217E-14)) ;
#37222 = DIRECTION('ref_axis',(4.54195640846217E-14,-1.66321791214601E-16,
1.)) ;
#37223 = DIRECTION('center_axis',(4.54195640846217E-14,-1.66321791214601E-16,
1.)) ;
#37224 = DIRECTION('ref_axis',(-1.66010601240624E-13,-1.,-1.66321791207061E-16)) ;
#37225 = DIRECTION('',(-4.54195640846217E-14,1.66321791214602E-16,-1.)) ;
#37226 = DIRECTION('',(4.54195640846217E-14,-1.66321791214602E-16,1.)) ;
#37227 = DIRECTION('center_axis',(1.,-1.75658099177411E-13,-4.54195640846217E-14)) ;
#37228 = DIRECTION('ref_axis',(-4.54195640846217E-14,1.66321791214601E-16,
-1.)) ;
#37229 = DIRECTION('',(4.54195640846217E-14,-1.66321791214602E-16,1.)) ;
#37230 = DIRECTION('center_axis',(4.54195640846217E-14,-1.66321791214601E-16,
1.)) ;
#37231 = DIRECTION('ref_axis',(1.75658099177411E-13,1.,1.66321791206623E-16)) ;
#37232 = DIRECTION('',(-4.54195640846217E-14,1.66321791214602E-16,-1.)) ;
#37233 = DIRECTION('center_axis',(-1.,1.75658099177411E-13,4.54195640846217E-14)) ;
#37234 = DIRECTION('ref_axis',(4.54195640846217E-14,-1.66321791214601E-16,
1.)) ;
#37235 = DIRECTION('center_axis',(4.54195640846217E-14,-1.66321791214601E-16,
1.)) ;
#37236 = DIRECTION('ref_axis',(-1.66010601240624E-13,-1.,-1.66321791207061E-16)) ;
#37237 = DIRECTION('',(-4.54195640846217E-14,1.66321791214602E-16,-1.)) ;
#37238 = DIRECTION('',(4.54195640846217E-14,-1.66321791214602E-16,1.)) ;
#37239 = DIRECTION('center_axis',(1.,-1.75658099177411E-13,-4.54195640846217E-14)) ;
#37240 = DIRECTION('ref_axis',(-4.54195640846217E-14,1.66321791214601E-16,
-1.)) ;
#37241 = DIRECTION('',(4.54195640846217E-14,-1.66321791214602E-16,1.)) ;
#37242 = DIRECTION('center_axis',(4.54195640846217E-14,-1.66321791214601E-16,
1.)) ;
#37243 = DIRECTION('ref_axis',(1.75658099177411E-13,1.,1.66321791206623E-16)) ;
#37244 = DIRECTION('',(-4.54195640846217E-14,1.66321791214602E-16,-1.)) ;
#37245 = DIRECTION('center_axis',(-1.,1.75658099177411E-13,4.54195640846217E-14)) ;
#37246 = DIRECTION('ref_axis',(4.54195640846217E-14,-1.66321791214601E-16,
1.)) ;
#37247 = DIRECTION('center_axis',(4.54195640846217E-14,-1.66321791214601E-16,
1.)) ;
#37248 = DIRECTION('ref_axis',(-1.89547329362678E-13,-1.,-1.66321791205992E-16)) ;
#37249 = DIRECTION('',(-4.54195640846217E-14,1.66321791214602E-16,-1.)) ;
#37250 = DIRECTION('',(4.54195640846217E-14,-1.66321791214602E-16,1.)) ;
#37251 = DIRECTION('center_axis',(1.,-1.75658099177411E-13,-4.54195640846217E-14)) ;
#37252 = DIRECTION('ref_axis',(-4.54195640846217E-14,1.66321791214601E-16,
-1.)) ;
#37253 = DIRECTION('',(4.54195640846217E-14,-1.66321791214602E-16,1.)) ;
#37254 = DIRECTION('center_axis',(4.54195640846217E-14,-1.66321791214601E-16,
1.)) ;
#37255 = DIRECTION('ref_axis',(1.75658099177411E-13,1.,1.66321791206623E-16)) ;
#37256 = DIRECTION('',(-4.54195640846217E-14,1.66321791214602E-16,-1.)) ;
#37257 = DIRECTION('center_axis',(-1.,1.75658099177411E-13,4.54195640846217E-14)) ;
#37258 = DIRECTION('ref_axis',(4.54195640846217E-14,-1.66321791214601E-16,
1.)) ;
#37259 = DIRECTION('center_axis',(-1.75658099177411E-13,-1.,-1.66321791206623E-16)) ;
#37260 = DIRECTION('ref_axis',(1.,-1.75658099177411E-13,-4.54195640846217E-14)) ;
#37261 = DIRECTION('',(1.75658099177411E-13,1.,1.66321791206623E-16)) ;
#37262 = DIRECTION('center_axis',(-1.,1.75658099177411E-13,4.54195640846217E-14)) ;
#37263 = DIRECTION('ref_axis',(4.54195640846217E-14,-1.66321791214601E-16,
1.)) ;
#37264 = DIRECTION('center_axis',(-1.75658099177411E-13,-1.,-1.66321791206623E-16)) ;
#37265 = DIRECTION('ref_axis',(0.99999997726804,-1.75658059720777E-13,-0.000213222701069828)) ;
#37266 = DIRECTION('',(-1.75658099177411E-13,-1.,-1.66321791206623E-16)) ;
#37267 = DIRECTION('center_axis',(1.08955953009724E-14,-4.58309287791692E-15,
1.)) ;
#37268 = DIRECTION('ref_axis',(-0.866025403784527,-0.499999999999848,7.14431588103965E-15)) ;
#37269 = DIRECTION('center_axis',(4.9836335171324E-14,-3.46902905748639E-14,
1.)) ;
#37270 = DIRECTION('ref_axis',(0.499999999999848,-0.866025403784527,-5.49608404881535E-14)) ;
#37271 = DIRECTION('center_axis',(7.99435328682709E-14,4.25044929548771E-15,
1.)) ;
#37272 = DIRECTION('ref_axis',(0.866025403784527,0.499999999999848,-7.13583549799491E-14)) ;
#37273 = DIRECTION('center_axis',(-1.03934083530628E-14,-3.21183541046639E-14,
1.)) ;
#37274 = DIRECTION('ref_axis',(-0.848313848782009,0.529493733640593,8.18959499131937E-15)) ;
#37275 = DIRECTION('',(2.48321689126043E-13,-3.16343365850263E-14,-1.)) ;
#37276 = DIRECTION('',(-5.79112402932487E-14,7.00367420686418E-14,-1.)) ;
#37277 = DIRECTION('center_axis',(1.30601282495909E-14,-5.57440796960452E-14,
1.)) ;
#37278 = DIRECTION('ref_axis',(0.848313848782206,0.529493733640277,1.84370532256005E-14)) ;
#37279 = DIRECTION('',(8.69448181549043E-14,1.21772749364003E-13,-1.)) ;
#37280 = DIRECTION('',(3.35143206547937E-13,5.99821398094943E-14,1.)) ;
#37281 = DIRECTION('center_axis',(-2.21832942445859E-16,-4.54750752358529E-14,
1.)) ;
#37282 = DIRECTION('ref_axis',(-1.75780563857328E-13,-1.,-4.54750752358529E-14)) ;
#37283 = DIRECTION('center_axis',(-2.21832942445859E-16,-4.54750752358529E-14,
1.)) ;
#37284 = DIRECTION('ref_axis',(-1.75780563857328E-13,-1.,-4.54750752358529E-14)) ;
#37285 = DIRECTION('center_axis',(7.7371596398071E-14,-5.59792942288991E-14,
1.)) ;
#37286 = DIRECTION('ref_axis',(-0.529493733640591,-0.84831384878201,-6.52023508487044E-15)) ;
#37287 = DIRECTION('',(-1.36189057083808E-14,2.93907575001879E-13,-1.)) ;
#37288 = DIRECTION('',(-1.15289984362049E-13,-1.23253544174125E-14,-1.)) ;
#37289 = DIRECTION('center_axis',(1.00997321989452E-13,-3.25257576262454E-14,
1.)) ;
#37290 = DIRECTION('ref_axis',(-0.52949373364028,0.848313848782204,8.10694997443418E-14)) ;
#37291 = DIRECTION('',(-1.6702599165741E-13,1.32530704030741E-13,-1.)) ;
#37292 = DIRECTION('',(-1.47288975160872E-14,2.895573206721E-13,1.)) ;
#37293 = DIRECTION('center_axis',(9.072831752926E-14,-4.58077188182821E-14,
1.)) ;
#37294 = DIRECTION('ref_axis',(1.,-1.75841796197283E-13,-9.07283175292681E-14)) ;
#37295 = DIRECTION('center_axis',(9.072831752926E-14,-4.58077188182821E-14,
1.)) ;
#37296 = DIRECTION('ref_axis',(1.,-1.75841796197283E-13,-9.07283175292681E-14)) ;
#37297 = DIRECTION('center_axis',(1.01232536522306E-13,3.17857105222347E-14,
1.)) ;
#37298 = DIRECTION('ref_axis',(0.848313848782008,-0.529493733640594,-6.90466281383654E-14)) ;
#37299 = DIRECTION('',(-3.39160817295286E-13,3.19669801674555E-14,-1.)) ;
#37300 = DIRECTION('',(-3.29278878759946E-14,-6.97040984862126E-14,-1.)) ;
#37301 = DIRECTION('center_axis',(7.77789999196525E-14,5.5411436113616E-14,
1.)) ;
#37302 = DIRECTION('ref_axis',(-0.848313848782201,-0.529493733640285,9.53210109704396E-14)) ;
#37303 = DIRECTION('',(-1.77783946324148E-13,-1.21440105781574E-13,-1.)) ;
#37304 = DIRECTION('',(-2.44304078378693E-13,-6.03147833919235E-14,1.)) ;
#37305 = DIRECTION('center_axis',(9.10609611116892E-14,4.51424316534237E-14,
1.)) ;
#37306 = DIRECTION('ref_axis',(1.75903028537238E-13,1.,-4.51424316534397E-14)) ;
#37307 = DIRECTION('center_axis',(9.10609611116892E-14,4.51424316534237E-14,
1.)) ;
#37308 = DIRECTION('ref_axis',(1.75903028537238E-13,1.,-4.51424316534397E-14)) ;
#37309 = DIRECTION('axis',(0.,0.,1.)) ;
#37310 = DIRECTION('refdir',(1.,0.,0.)) ;
#37311 = DIRECTION('axis',(0.,0.,1.)) ;
#37312 = DIRECTION('refdir',(1.,0.,0.)) ;
#37313 = DIRECTION('axis',(0.,0.,1.)) ;
#37314 = DIRECTION('refdir',(1.,0.,0.)) ;
#37315 = DIRECTION('center_axis',(0.,-1.,0.)) ;
#37316 = DIRECTION('ref_axis',(-2.9521166348046E-16,0.,-1.)) ;
#37317 = DIRECTION('',(0.,-1.,0.)) ;
#37318 = DIRECTION('center_axis',(-7.50335137235545E-15,-1.,-1.88069991130403E-15)) ;
#37319 = DIRECTION('ref_axis',(-0.802795663530002,7.14503324610129E-15,-0.596254243269953)) ;
#37320 = DIRECTION('center_axis',(0.,-1.,0.)) ;
#37321 = DIRECTION('ref_axis',(-2.9521166348046E-16,0.,-1.)) ;
#37322 = DIRECTION('',(0.,-1.,0.)) ;
#37323 = DIRECTION('center_axis',(0.,-1.,0.)) ;
#37324 = DIRECTION('ref_axis',(-2.9521166348046E-16,0.,-1.)) ;
#37325 = DIRECTION('',(0.,-1.,0.)) ;
#37326 = DIRECTION('center_axis',(0.,-1.,0.)) ;
#37327 = DIRECTION('ref_axis',(-2.9521166348046E-16,0.,-1.)) ;
#37328 = DIRECTION('',(0.,-1.,0.)) ;
#37329 = DIRECTION('center_axis',(0.,-1.,0.)) ;
#37330 = DIRECTION('ref_axis',(-2.9521166348046E-16,0.,-1.)) ;
#37331 = DIRECTION('',(0.,-1.,0.)) ;
#37332 = DIRECTION('center_axis',(8.41776735018431E-16,-1.,-1.3808398081996E-15)) ;
#37333 = DIRECTION('ref_axis',(0.802795663530003,1.49910630744832E-15,-0.596254243269952)) ;
#37334 = DIRECTION('center_axis',(0.,-1.,0.)) ;
#37335 = DIRECTION('ref_axis',(0.,0.,-1.)) ;
#37336 = DIRECTION('',(0.,-1.,0.)) ;
#37337 = DIRECTION('center_axis',(0.,1.,0.)) ;
#37338 = DIRECTION('ref_axis',(0.,0.,1.)) ;
#37339 = DIRECTION('center_axis',(0.,-1.,0.)) ;
#37340 = DIRECTION('ref_axis',(0.,0.,-1.)) ;
#37341 = DIRECTION('',(0.,-1.,0.)) ;
#37342 = DIRECTION('center_axis',(0.,-1.,0.)) ;
#37343 = DIRECTION('ref_axis',(0.,0.,-1.)) ;
#37344 = DIRECTION('',(0.,-1.,0.)) ;
#37345 = DIRECTION('center_axis',(0.,-1.,0.)) ;
#37346 = DIRECTION('ref_axis',(0.,0.,-1.)) ;
#37347 = DIRECTION('',(0.,-1.,0.)) ;
#37348 = DIRECTION('center_axis',(0.,-1.,0.)) ;
#37349 = DIRECTION('ref_axis',(0.,0.,-1.)) ;
#37350 = DIRECTION('',(0.,-1.,0.)) ;
#37351 = DIRECTION('center_axis',(0.,-1.,0.)) ;
#37352 = DIRECTION('ref_axis',(0.,0.,-1.)) ;
#37353 = DIRECTION('',(0.,-1.,0.)) ;
#37354 = DIRECTION('center_axis',(0.,1.,0.)) ;
#37355 = DIRECTION('ref_axis',(0.,0.,1.)) ;
#37356 = DIRECTION('center_axis',(0.,1.,0.)) ;
#37357 = DIRECTION('ref_axis',(0.,0.,1.)) ;
#37358 = DIRECTION('',(-8.65956056235495E-17,0.707106781186546,-0.707106781186549)) ;
#37359 = DIRECTION('center_axis',(0.,-1.,0.)) ;
#37360 = DIRECTION('ref_axis',(0.,0.,1.)) ;
#37361 = DIRECTION('',(8.65956056235495E-17,-0.707106781186546,-0.707106781186549)) ;
#37362 = DIRECTION('center_axis',(0.,-1.,0.)) ;
#37363 = DIRECTION('ref_axis',(0.,0.,1.)) ;
#37364 = DIRECTION('center_axis',(0.,1.,0.)) ;
#37365 = DIRECTION('ref_axis',(0.,0.,1.)) ;
#37366 = DIRECTION('center_axis',(0.,1.,0.)) ;
#37367 = DIRECTION('ref_axis',(0.,0.,1.)) ;
#37368 = DIRECTION('center_axis',(0.,1.,0.)) ;
#37369 = DIRECTION('ref_axis',(0.,0.,1.)) ;
#37370 = DIRECTION('center_axis',(0.,-1.,0.)) ;
#37371 = DIRECTION('ref_axis',(0.,0.,-1.)) ;
#37372 = DIRECTION('center_axis',(0.,-1.,0.)) ;
#37373 = DIRECTION('ref_axis',(-2.9521166348046E-16,0.,-1.)) ;
#37374 = DIRECTION('center_axis',(0.,1.,0.)) ;
#37375 = DIRECTION('ref_axis',(0.,0.,1.)) ;
#37376 = DIRECTION('center_axis',(0.,-1.,0.)) ;
#37377 = DIRECTION('ref_axis',(0.,0.,1.)) ;
#37378 = DIRECTION('center_axis',(0.,-1.,0.)) ;
#37379 = DIRECTION('ref_axis',(0.,0.,1.)) ;
#37380 = DIRECTION('center_axis',(0.,1.,0.)) ;
#37381 = DIRECTION('ref_axis',(0.,0.,1.)) ;
#37382 = DIRECTION('center_axis',(0.,1.,0.)) ;
#37383 = DIRECTION('ref_axis',(0.,0.,1.)) ;
#37384 = DIRECTION('center_axis',(0.,1.,0.)) ;
#37385 = DIRECTION('ref_axis',(0.,0.,1.)) ;
#37386 = DIRECTION('center_axis',(0.,1.,0.)) ;
#37387 = DIRECTION('ref_axis',(0.,0.,1.)) ;
#37388 = DIRECTION('center_axis',(0.,1.,0.)) ;
#37389 = DIRECTION('ref_axis',(0.,0.,1.)) ;
#37390 = DIRECTION('center_axis',(0.,1.,0.)) ;
#37391 = DIRECTION('ref_axis',(0.,0.,1.)) ;
#37392 = DIRECTION('center_axis',(0.,1.,0.)) ;
#37393 = DIRECTION('ref_axis',(0.,0.,1.)) ;
#37394 = DIRECTION('center_axis',(0.5,0.,0.866025403784439)) ;
#37395 = DIRECTION('ref_axis',(0.866025403784439,0.,-0.5)) ;
#37396 = DIRECTION('',(0.,-1.,0.)) ;
#37397 = DIRECTION('',(0.,-1.,0.)) ;
#37398 = DIRECTION('center_axis',(1.,0.,-1.36574054430651E-16)) ;
#37399 = DIRECTION('ref_axis',(-1.36574054430651E-16,0.,-1.)) ;
#37400 = DIRECTION('',(0.,-1.,0.)) ;
#37401 = DIRECTION('center_axis',(0.5,0.,-0.866025403784439)) ;
#37402 = DIRECTION('ref_axis',(-0.866025403784439,0.,-0.5)) ;
#37403 = DIRECTION('',(0.,-1.,0.)) ;
#37404 = DIRECTION('center_axis',(-0.5,0.,-0.866025403784438)) ;
#37405 = DIRECTION('ref_axis',(-0.866025403784438,0.,0.5)) ;
#37406 = DIRECTION('',(0.,-1.,0.)) ;
#37407 = DIRECTION('center_axis',(-1.,0.,0.)) ;
#37408 = DIRECTION('ref_axis',(0.,0.,1.)) ;
#37409 = DIRECTION('',(0.,-1.,0.)) ;
#37410 = DIRECTION('center_axis',(-0.5,0.,0.866025403784439)) ;
#37411 = DIRECTION('ref_axis',(0.866025403784439,0.,0.5)) ;
#37412 = DIRECTION('center_axis',(0.,1.,0.)) ;
#37413 = DIRECTION('ref_axis',(0.,0.,1.)) ;
#37414 = DIRECTION('center_axis',(0.,-1.,0.)) ;
#37415 = DIRECTION('ref_axis',(0.,0.,1.)) ;
#37416 = DIRECTION('center_axis',(0.,-1.,0.)) ;
#37417 = DIRECTION('ref_axis',(0.,0.,1.)) ;
#37418 = DIRECTION('center_axis',(0.,-1.,0.)) ;
#37419 = DIRECTION('ref_axis',(1.77635683940025E-15,0.,1.)) ;
#37420 = DIRECTION('center_axis',(0.,-1.,0.)) ;
#37421 = DIRECTION('ref_axis',(0.,0.,1.)) ;
#37422 = DIRECTION('center_axis',(0.,1.,0.)) ;
#37423 = DIRECTION('ref_axis',(0.,0.,1.)) ;
#37424 = DIRECTION('center_axis',(0.,-1.,0.)) ;
#37425 = DIRECTION('ref_axis',(-1.01064309961486E-15,0.,-1.)) ;
#37426 = DIRECTION('center_axis',(0.,-1.,0.)) ;
#37427 = DIRECTION('ref_axis',(0.,0.,1.)) ;
#37428 = DIRECTION('center_axis',(0.,-1.,0.)) ;
#37429 = DIRECTION('ref_axis',(0.,0.,1.)) ;
#37430 = DIRECTION('center_axis',(0.,-1.,0.)) ;
#37431 = DIRECTION('ref_axis',(0.,0.,1.)) ;
#37432 = DIRECTION('center_axis',(0.,-1.,0.)) ;
#37433 = DIRECTION('ref_axis',(0.,0.,1.)) ;
#37434 = DIRECTION('center_axis',(0.,1.,0.)) ;
#37435 = DIRECTION('ref_axis',(0.,0.,1.)) ;
#37436 = DIRECTION('center_axis',(0.,1.,0.)) ;
#37437 = DIRECTION('ref_axis',(0.,0.,1.)) ;
#37438 = DIRECTION('center_axis',(0.,1.,0.)) ;
#37439 = DIRECTION('ref_axis',(1.22464679914735E-16,0.,-1.)) ;
#37440 = DIRECTION('center_axis',(0.,1.,0.)) ;
#37441 = DIRECTION('ref_axis',(0.,0.,1.)) ;
#37442 = DIRECTION('center_axis',(0.,1.,0.)) ;
#37443 = DIRECTION('ref_axis',(0.,0.,1.)) ;
#37444 = DIRECTION('',(-1.11022302462516E-16,-1.,-8.49927588852477E-14)) ;
#37445 = DIRECTION('',(1.,-1.11022302462511E-16,-5.70360434152645E-17)) ;
#37446 = DIRECTION('',(-1.11022302462516E-16,-1.,-8.49797573693038E-14)) ;
#37447 = DIRECTION('',(1.,-1.11022302462511E-16,-5.62735973232373E-17)) ;
#37448 = DIRECTION('',(-1.11022302462516E-16,-1.,-8.49806336411519E-14)) ;
#37449 = DIRECTION('',(1.,-1.11022302462511E-16,-5.55111512312665E-17)) ;
#37450 = DIRECTION('',(-1.11022302462516E-16,-1.,-8.49806336411598E-14)) ;
#37451 = DIRECTION('',(1.,-1.11022302462511E-16,-5.55111512312274E-17)) ;
#37452 = DIRECTION('',(-1.11022302462516E-16,-1.,-8.49806336411598E-14)) ;
#37453 = DIRECTION('',(1.,-1.11022302462511E-16,-5.55111512312602E-17)) ;
#37454 = DIRECTION('axis',(0.,0.,1.)) ;
#37455 = DIRECTION('refdir',(1.,0.,0.)) ;
#37456 = DIRECTION('axis',(0.,0.,1.)) ;
#37457 = DIRECTION('refdir',(1.,0.,0.)) ;
#37458 = DIRECTION('center_axis',(0.,0.,-1.)) ;
#37459 = DIRECTION('ref_axis',(-1.03057430466152E-16,1.,0.)) ;
#37460 = DIRECTION('',(0.,0.,1.)) ;
#37461 = DIRECTION('center_axis',(0.,9.04152290739048E-17,-1.)) ;
#37462 = DIRECTION('ref_axis',(-1.03057430466152E-16,1.,9.04152290739048E-17)) ;
#37463 = DIRECTION('center_axis',(0.,0.,-1.)) ;
#37464 = DIRECTION('ref_axis',(-1.03057430466152E-16,1.,0.)) ;
#37465 = DIRECTION('',(0.,0.,1.)) ;
#37466 = DIRECTION('center_axis',(0.,9.04152290739048E-17,-1.)) ;
#37467 = DIRECTION('ref_axis',(-1.03057430466152E-16,1.,9.04152290739048E-17)) ;
#37468 = DIRECTION('center_axis',(0.,0.,-1.)) ;
#37469 = DIRECTION('ref_axis',(-1.03057430466152E-16,1.,0.)) ;
#37470 = DIRECTION('',(0.,0.,1.)) ;
#37471 = DIRECTION('center_axis',(0.,0.,-1.)) ;
#37472 = DIRECTION('ref_axis',(-1.03057430466152E-16,1.,0.)) ;
#37473 = DIRECTION('',(0.,0.,1.)) ;
#37474 = DIRECTION('center_axis',(0.,0.,-1.)) ;
#37475 = DIRECTION('ref_axis',(-1.03057430466152E-16,1.,0.)) ;
#37476 = DIRECTION('',(0.,0.,1.)) ;
#37477 = DIRECTION('center_axis',(0.,0.,-1.)) ;
#37478 = DIRECTION('ref_axis',(-1.03057430466152E-16,1.,0.)) ;
#37479 = DIRECTION('',(0.,0.,1.)) ;
#37480 = DIRECTION('center_axis',(0.,1.42961865771945E-15,-1.)) ;
#37481 = DIRECTION('ref_axis',(0.,1.,1.42961865771945E-15)) ;
#37482 = DIRECTION('',(0.,-1.42961865771945E-15,1.)) ;
#37483 = DIRECTION('center_axis',(0.,-9.04152290739048E-17,1.)) ;
#37484 = DIRECTION('ref_axis',(8.88178419700125E-16,1.,9.04152290739048E-17)) ;
#37485 = DIRECTION('',(0.,-1.42961865771945E-15,1.)) ;
#37486 = DIRECTION('center_axis',(0.,1.42961865771945E-15,-1.)) ;
#37487 = DIRECTION('ref_axis',(0.,1.,1.42961865771945E-15)) ;
#37488 = DIRECTION('center_axis',(0.,1.42961865771945E-15,-1.)) ;
#37489 = DIRECTION('ref_axis',(0.,1.,1.42961865771945E-15)) ;
#37490 = DIRECTION('center_axis',(0.,-9.04152290739048E-17,1.)) ;
#37491 = DIRECTION('ref_axis',(8.88178419700125E-16,1.,9.04152290739048E-17)) ;
#37492 = DIRECTION('center_axis',(0.,1.42961865771945E-15,-1.)) ;
#37493 = DIRECTION('ref_axis',(0.,1.,1.42961865771945E-15)) ;
#37494 = DIRECTION('',(0.,-1.42961865771945E-15,1.)) ;
#37495 = DIRECTION('center_axis',(0.,1.42961865771945E-15,-1.)) ;
#37496 = DIRECTION('ref_axis',(0.,1.,1.42961865771945E-15)) ;
#37497 = DIRECTION('',(0.,-1.42961865771945E-15,1.)) ;
#37498 = DIRECTION('center_axis',(0.,1.42961865771945E-15,-1.)) ;
#37499 = DIRECTION('ref_axis',(0.,1.,1.42961865771945E-15)) ;
#37500 = DIRECTION('',(0.,-1.42961865771945E-15,1.)) ;
#37501 = DIRECTION('center_axis',(0.,1.42961865771945E-15,-1.)) ;
#37502 = DIRECTION('ref_axis',(0.,1.,1.42961865771945E-15)) ;
#37503 = DIRECTION('',(0.,-1.42961865771945E-15,1.)) ;
#37504 = DIRECTION('center_axis',(0.,1.42961865771945E-15,-1.)) ;
#37505 = DIRECTION('ref_axis',(0.,1.,1.42961865771945E-15)) ;
#37506 = DIRECTION('center_axis',(0.,1.42961865771945E-15,-1.)) ;
#37507 = DIRECTION('ref_axis',(0.,1.,1.42961865771945E-15)) ;
#37508 = DIRECTION('center_axis',(0.,0.,-1.)) ;
#37509 = DIRECTION('ref_axis',(-1.03057430466152E-16,1.,0.)) ;
#37510 = DIRECTION('center_axis',(1.12004190703271E-15,-3.6645376121857E-15,
-1.)) ;
#37511 = DIRECTION('ref_axis',(0.104117265609716,-0.99456502804088,3.76123665374887E-15)) ;
#37512 = DIRECTION('center_axis',(0.,-1.42652275615057E-16,1.)) ;
#37513 = DIRECTION('ref_axis',(1.,0.,0.)) ;
#37514 = DIRECTION('center_axis',(0.,1.42652275615057E-16,-1.)) ;
#37515 = DIRECTION('ref_axis',(1.22464679914735E-16,1.,1.42652275615057E-16)) ;
#37516 = DIRECTION('center_axis',(1.22464679914735E-16,-1.,-1.42652275615057E-16)) ;
#37517 = DIRECTION('ref_axis',(-1.,-1.22464679914735E-16,0.)) ;
#37518 = DIRECTION('center_axis',(-4.11797682050993E-32,-2.13305428978351E-16,
1.)) ;
#37519 = DIRECTION('ref_axis',(0.,1.,2.13305428978351E-16)) ;
#37520 = DIRECTION('center_axis',(-4.11797682050993E-32,-2.13305428978351E-16,
1.)) ;
#37521 = DIRECTION('ref_axis',(0.,1.,2.13305428978351E-16)) ;
#37522 = DIRECTION('center_axis',(0.,-1.42652275615057E-16,1.)) ;
#37523 = DIRECTION('ref_axis',(0.,-1.,-1.42652275615057E-16)) ;
#37524 = DIRECTION('',(8.03440589904947E-17,-0.656059028990509,-0.754709580222771)) ;
#37525 = DIRECTION('center_axis',(0.,1.42652275615057E-16,-1.)) ;
#37526 = DIRECTION('ref_axis',(0.,1.,1.42652275615057E-16)) ;
#37527 = DIRECTION('center_axis',(0.,0.,1.)) ;
#37528 = DIRECTION('ref_axis',(1.,0.,0.)) ;
#37529 = DIRECTION('',(-1.,3.18158468314499E-15,0.)) ;
#37530 = DIRECTION('',(-0.923879532511288,-0.382683432365087,0.)) ;
#37531 = DIRECTION('',(-0.382683432365093,-0.923879532511286,0.)) ;
#37532 = DIRECTION('',(3.33653301099406E-15,1.,0.)) ;
#37533 = DIRECTION('center_axis',(0.,0.,1.)) ;
#37534 = DIRECTION('ref_axis',(-3.49148133884313E-15,-1.,0.)) ;
#37535 = DIRECTION('',(-3.09896655698145E-16,1.,0.)) ;
#37536 = DIRECTION('',(-0.38268343236509,0.923879532511287,0.)) ;
#37537 = DIRECTION('',(-0.923879532511287,0.382683432365089,0.)) ;
#37538 = DIRECTION('',(1.,1.54948327849072E-16,0.)) ;
#37539 = DIRECTION('center_axis',(0.,0.,1.)) ;
#37540 = DIRECTION('ref_axis',(-1.,0.,0.)) ;
#37541 = DIRECTION('',(1.,-1.01645473608313E-14,0.)) ;
#37542 = DIRECTION('',(0.923879532511291,0.382683432365081,0.)) ;
#37543 = DIRECTION('',(0.382683432365099,0.923879532511283,0.)) ;
#37544 = DIRECTION('',(-1.03194956886803E-14,-1.,0.)) ;
#37545 = DIRECTION('center_axis',(0.,0.,-1.)) ;
#37546 = DIRECTION('ref_axis',(1.,-2.66453525910038E-15,0.)) ;
#37547 = DIRECTION('',(3.09896655698145E-16,-1.,0.)) ;
#37548 = DIRECTION('',(0.38268343236509,-0.923879532511287,0.)) ;
#37549 = DIRECTION('',(0.923879532511287,-0.382683432365089,0.)) ;
#37550 = DIRECTION('',(-1.,-1.54948327849072E-16,0.)) ;
#37551 = DIRECTION('center_axis',(0.,-1.42961865771945E-15,1.)) ;
#37552 = DIRECTION('ref_axis',(0.,-1.,-1.42961865771945E-15)) ;
#37553 = DIRECTION('',(8.65956056235495E-17,-0.707106781186548,-0.707106781186547)) ;
#37554 = DIRECTION('center_axis',(0.,1.42961865771945E-15,-1.)) ;
#37555 = DIRECTION('ref_axis',(0.,1.,1.42961865771945E-15)) ;
#37556 = DIRECTION('center_axis',(0.,-1.42652275615057E-16,1.)) ;
#37557 = DIRECTION('ref_axis',(0.,-1.,-1.42652275615057E-16)) ;
#37558 = DIRECTION('',(-8.03440589904947E-17,0.656059028990508,0.754709580222771)) ;
#37559 = DIRECTION('center_axis',(0.,-1.42652275615057E-16,1.)) ;
#37560 = DIRECTION('ref_axis',(0.,-1.,-1.42652275615057E-16)) ;
#37561 = DIRECTION('center_axis',(0.,-1.42652275615057E-16,-1.)) ;
#37562 = DIRECTION('ref_axis',(0.,1.,-1.42652275615057E-16)) ;
#37563 = DIRECTION('center_axis',(1.42652275615057E-16,-4.9806775825348E-31,
-1.)) ;
#37564 = DIRECTION('ref_axis',(-1.,3.49148133884313E-15,-1.42652275615057E-16)) ;
#37565 = DIRECTION('center_axis',(0.,1.42652275615057E-16,-1.)) ;
#37566 = DIRECTION('ref_axis',(0.,-1.,-1.42652275615057E-16)) ;
#37567 = DIRECTION('center_axis',(0.,-1.42652275615057E-16,1.)) ;
#37568 = DIRECTION('ref_axis',(0.,-1.,-1.42652275615057E-16)) ;
#37569 = DIRECTION('center_axis',(0.,0.,1.)) ;
#37570 = DIRECTION('ref_axis',(1.,0.,0.)) ;
#37571 = DIRECTION('center_axis',(-3.16947779287894E-15,-0.996194698091746,
-0.0871557427476585)) ;
#37572 = DIRECTION('ref_axis',(2.97883628356478E-31,0.0871557427476584,-0.996194698091746)) ;
#37573 = DIRECTION('center_axis',(1.54358702681427E-16,-0.996194698091746,
0.0871557427476582)) ;
#37574 = DIRECTION('ref_axis',(2.57763828956271E-33,0.0871557427476582,0.996194698091746)) ;
#37575 = DIRECTION('center_axis',(0.,0.,1.)) ;
#37576 = DIRECTION('ref_axis',(-1.,0.,0.)) ;
#37577 = DIRECTION('center_axis',(1.01258681893625E-14,0.996194698091746,
-0.0871557427476582)) ;
#37578 = DIRECTION('ref_axis',(7.19854450834723E-33,-0.0871557427476582,-0.996194698091746)) ;
#37579 = DIRECTION('center_axis',(-1.54358702681427E-16,0.996194698091746,
0.0871557427476585)) ;
#37580 = DIRECTION('ref_axis',(1.2014865513381E-32,-0.0871557427476584,0.996194698091746)) ;
#37581 = DIRECTION('center_axis',(0.,0.,1.)) ;
#37582 = DIRECTION('ref_axis',(-3.49148133884313E-15,-1.,0.)) ;
#37583 = DIRECTION('center_axis',(-0.996194698091746,-3.08717405362855E-16,
-0.0871557427476584)) ;
#37584 = DIRECTION('ref_axis',(0.0871557427476584,-3.04302649376462E-16,-0.996194698091746)) ;
#37585 = DIRECTION('center_axis',(-0.996194698091746,3.32383649556037E-15,
0.0871557427476584)) ;
#37586 = DIRECTION('ref_axis',(0.0871557427476584,-3.04302649376462E-16,0.996194698091746)) ;
#37587 = DIRECTION('center_axis',(-0.381227206369651,0.920363891963225,0.0871557427476585)) ;
#37588 = DIRECTION('ref_axis',(-0.923879532511288,-0.382683432365087,-7.3858143488638E-17)) ;
#37589 = DIRECTION('',(0.0666626913468322,-0.0666626913468327,0.995546167269401)) ;
#37590 = DIRECTION('',(0.01733375049386,-0.0871426484044399,0.996045029063886)) ;
#37591 = DIRECTION('center_axis',(-0.920363891963223,0.381227206369656,0.0871557427476584)) ;
#37592 = DIRECTION('ref_axis',(-0.382683432365092,-0.923879532511286,3.73934789043068E-19)) ;
#37593 = DIRECTION('',(0.0871426484044396,-0.0173337504938607,0.996045029063886)) ;
#37594 = DIRECTION('center_axis',(-0.996194698091746,3.32383649556037E-15,
0.0871557427476584)) ;
#37595 = DIRECTION('ref_axis',(0.0871557427476584,1.34784482901355E-31,0.996194698091746)) ;
#37596 = DIRECTION('center_axis',(0.996194698091746,3.08717405362855E-16,
0.0871557427476584)) ;
#37597 = DIRECTION('ref_axis',(0.0871557427476584,1.72317352807894E-33,-0.996194698091746)) ;
#37598 = DIRECTION('',(-0.0871426484044397,-0.0173337504938605,0.996045029063886)) ;
#37599 = DIRECTION('center_axis',(0.920363891963224,0.381227206369654,0.0871557427476584)) ;
#37600 = DIRECTION('ref_axis',(-0.38268343236509,0.923879532511287,-7.85426484421263E-17)) ;
#37601 = DIRECTION('',(-0.0666626913468323,-0.0666626913468325,0.995546167269401)) ;
#37602 = DIRECTION('center_axis',(0.381227206369653,0.920363891963225,0.0871557427476585)) ;
#37603 = DIRECTION('ref_axis',(-0.923879532511287,0.382683432365089,1.29793781600155E-17)) ;
#37604 = DIRECTION('',(-0.0173337504938602,-0.0871426484044398,0.996045029063886)) ;
#37605 = DIRECTION('center_axis',(-1.54358702681427E-16,0.996194698091746,
0.0871557427476585)) ;
#37606 = DIRECTION('ref_axis',(-3.11086130697268E-34,-0.0871557427476585,
0.996194698091746)) ;
#37607 = DIRECTION('center_axis',(-1.01258681893625E-14,-0.996194698091746,
0.0871557427476582)) ;
#37608 = DIRECTION('ref_axis',(-9.14090686442792E-32,-0.0871557427476582,
-0.996194698091746)) ;
#37609 = DIRECTION('',(-0.0173337504938594,0.0871426484044397,0.996045029063886)) ;
#37610 = DIRECTION('center_axis',(0.381227206369644,-0.920363891963228,0.0871557427476582)) ;
#37611 = DIRECTION('ref_axis',(0.923879532511291,0.38268343236508,5.52490330052255E-18)) ;
#37612 = DIRECTION('',(-0.0666626913468317,0.0666626913468329,0.995546167269401)) ;
#37613 = DIRECTION('center_axis',(0.920363891963221,-0.381227206369663,0.0871557427476583)) ;
#37614 = DIRECTION('ref_axis',(0.382683432365099,0.923879532511283,2.18567384430039E-17)) ;
#37615 = DIRECTION('',(-0.0871426484044395,0.017333750493861,0.996045029063886)) ;
#37616 = DIRECTION('center_axis',(0.996194698091746,-1.0280226892044E-14,
0.0871557427476584)) ;
#37617 = DIRECTION('ref_axis',(0.0871557427476584,3.23428151084849E-31,-0.996194698091746)) ;
#37618 = DIRECTION('center_axis',(0.996194698091746,-1.0280226892044E-14,
0.0871557427476584)) ;
#37619 = DIRECTION('ref_axis',(0.0871557427476584,3.23428151084849E-31,-0.996194698091746)) ;
#37620 = DIRECTION('center_axis',(0.,0.,1.)) ;
#37621 = DIRECTION('ref_axis',(1.,0.,0.)) ;
#37622 = DIRECTION('center_axis',(0.996194698091746,3.08717405362855E-16,
-0.0871557427476584)) ;
#37623 = DIRECTION('ref_axis',(0.0871557427476584,-1.34658839111257E-33,0.996194698091746)) ;
#37624 = DIRECTION('center_axis',(-0.996194698091746,-3.08717405362855E-16,
0.0871557427476584)) ;
#37625 = DIRECTION('ref_axis',(0.0871557427476584,1.72317352807894E-33,0.996194698091746)) ;
#37626 = DIRECTION('',(0.0871426484044397,0.0173337504938602,0.996045029063886)) ;
#37627 = DIRECTION('center_axis',(-0.920363891963224,-0.381227206369654,0.0871557427476583)) ;
#37628 = DIRECTION('ref_axis',(0.38268343236509,-0.923879532511287,-8.49630232542324E-17)) ;
#37629 = DIRECTION('',(0.0666626913468323,0.0666626913468322,0.995546167269401)) ;
#37630 = DIRECTION('center_axis',(-0.381227206369653,-0.920363891963225,0.0871557427476582)) ;
#37631 = DIRECTION('ref_axis',(0.923879532511287,-0.382683432365089,1.74631953898462E-17)) ;
#37632 = DIRECTION('',(0.0173337504938602,0.0871426484044396,0.996045029063886)) ;
#37633 = DIRECTION('center_axis',(1.54358702681427E-16,-0.996194698091746,
0.0871557427476582)) ;
#37634 = DIRECTION('ref_axis',(-1.03689433405292E-33,-0.0871557427476582,
-0.996194698091746)) ;
#37635 = DIRECTION('center_axis',(3.16947779287894E-15,0.996194698091746,
0.0871557427476585)) ;
#37636 = DIRECTION('ref_axis',(-5.1364595474912E-32,-0.0871557427476585,0.996194698091746)) ;
#37637 = DIRECTION('center_axis',(0.,9.04152290739048E-17,-1.)) ;
#37638 = DIRECTION('ref_axis',(0.,1.,9.04152290739048E-17)) ;
#37639 = DIRECTION('center_axis',(0.,1.42961865771945E-15,-1.)) ;
#37640 = DIRECTION('ref_axis',(0.,1.,1.42961865771945E-15)) ;
#37641 = DIRECTION('',(-1.75658099177411E-13,-1.,-2.36695155915651E-17)) ;
#37642 = DIRECTION('',(1.,-1.75658099177411E-13,-2.92157696951376E-29)) ;
#37643 = DIRECTION('',(-1.75658099177412E-13,-1.,-2.36695155915637E-17)) ;
#37644 = DIRECTION('',(1.,-1.75658099177412E-13,-2.92157696951376E-29)) ;
#37645 = DIRECTION('',(1.86593795969969E-13,1.,3.08974066821681E-16)) ;
#37646 = DIRECTION('',(-1.,1.86593795969969E-13,-1.22464679914704E-16)) ;
#37647 = DIRECTION('',(1.79994040505616E-13,1.,3.08974066821681E-16)) ;
#37648 = DIRECTION('',(-1.,1.79994040505616E-13,-1.22464679914705E-16)) ;
#37649 = DIRECTION('',(1.86593795969969E-13,1.,3.08974066821681E-16)) ;
#37650 = DIRECTION('',(-1.,1.86593795969969E-13,1.22464679914766E-16)) ;
#37651 = DIRECTION('',(-1.75658099177411E-13,-1.,-2.3669515591565E-17)) ;
#37652 = DIRECTION('',(1.,-1.75658099177411E-13,-2.92157696951375E-29)) ;
#37653 = DIRECTION('center_axis',(4.54195640846217E-14,-1.66321791214601E-16,
1.)) ;
#37654 = DIRECTION('ref_axis',(0.609352821942987,-0.792899198126797,-2.78084159612697E-14)) ;
#37655 = DIRECTION('',(4.54195640846217E-14,-1.66321791214601E-16,1.)) ;
#37656 = DIRECTION('center_axis',(-4.54195640846217E-14,1.66321791214601E-16,
-1.)) ;
#37657 = DIRECTION('ref_axis',(-1.,-3.64900768663075E-31,4.54195640846217E-14)) ;
#37658 = DIRECTION('center_axis',(4.54195640846217E-14,-1.66321791214601E-16,
1.)) ;
#37659 = DIRECTION('ref_axis',(0.609352821942987,-0.792899198126797,-2.78084159612697E-14)) ;
#37660 = DIRECTION('',(4.54195640846217E-14,-1.66321791214601E-16,1.)) ;
#37661 = DIRECTION('center_axis',(4.54195640846217E-14,-1.66321791214601E-16,
1.)) ;
#37662 = DIRECTION('ref_axis',(0.609352821942987,-0.792899198126797,-2.78084159612697E-14)) ;
#37663 = DIRECTION('',(4.54195640846217E-14,-1.66321791214601E-16,1.)) ;
#37664 = DIRECTION('center_axis',(4.54195640846217E-14,-1.66321791214601E-16,
1.)) ;
#37665 = DIRECTION('ref_axis',(-1.,-3.64900768663092E-31,4.54195640846217E-14)) ;
#37666 = DIRECTION('center_axis',(4.54195640846217E-14,-1.66321791214601E-16,
1.)) ;
#37667 = DIRECTION('ref_axis',(0.980619819129883,0.195920316275966,-4.45067388996815E-14)) ;
#37668 = DIRECTION('',(4.54195640846217E-14,-1.66321791214601E-16,1.)) ;
#37669 = DIRECTION('center_axis',(-4.54195640846217E-14,1.66321791214601E-16,
-1.)) ;
#37670 = DIRECTION('ref_axis',(-1.,3.4580495717732E-14,4.54195640846217E-14)) ;
#37671 = DIRECTION('center_axis',(4.54195640846217E-14,-1.66321791214601E-16,
1.)) ;
#37672 = DIRECTION('ref_axis',(0.980619819129883,0.195920316275966,-4.45067388996815E-14)) ;
#37673 = DIRECTION('',(4.54195640846217E-14,-1.66321791214601E-16,1.)) ;
#37674 = DIRECTION('center_axis',(4.54195640846217E-14,-1.66321791214601E-16,
1.)) ;
#37675 = DIRECTION('ref_axis',(0.980619819129883,0.195920316275966,-4.45067388996815E-14)) ;
#37676 = DIRECTION('',(4.54195640846217E-14,-1.66321791214601E-16,1.)) ;
#37677 = DIRECTION('center_axis',(4.54195640846217E-14,-1.66321791214601E-16,
1.)) ;
#37678 = DIRECTION('ref_axis',(-1.,3.4580495717732E-14,4.54195640846217E-14)) ;
#37679 = DIRECTION('center_axis',(4.54195640846217E-14,-1.66321791214601E-16,
1.)) ;
#37680 = DIRECTION('ref_axis',(0.609364319911517,-0.792890361663436,-2.78089367242917E-14)) ;
#37681 = DIRECTION('',(4.54195640846217E-14,-1.66321791214601E-16,1.)) ;
#37682 = DIRECTION('center_axis',(-4.54195640846217E-14,1.66321791214601E-16,
-1.)) ;
#37683 = DIRECTION('ref_axis',(-1.,3.4580495717732E-14,4.54195640846217E-14)) ;
#37684 = DIRECTION('center_axis',(4.54195640846217E-14,-1.66321791214601E-16,
1.)) ;
#37685 = DIRECTION('ref_axis',(0.609364319911517,-0.792890361663436,-2.78089367242917E-14)) ;
#37686 = DIRECTION('',(4.54195640846217E-14,-1.66321791214601E-16,1.)) ;
#37687 = DIRECTION('center_axis',(4.54195640846217E-14,-1.66321791214601E-16,
1.)) ;
#37688 = DIRECTION('ref_axis',(0.609364319911517,-0.792890361663436,-2.78089367242917E-14)) ;
#37689 = DIRECTION('',(4.54195640846217E-14,-1.66321791214601E-16,1.)) ;
#37690 = DIRECTION('center_axis',(4.54195640846217E-14,-1.66321791214601E-16,
1.)) ;
#37691 = DIRECTION('ref_axis',(-1.,3.4580495717732E-14,4.54195640846217E-14)) ;
#37692 = DIRECTION('center_axis',(4.54195640846217E-14,-1.66321791214601E-16,
1.)) ;
#37693 = DIRECTION('ref_axis',(0.609355676053996,-0.792897004699083,-2.78085452289327E-14)) ;
#37694 = DIRECTION('',(4.54195640846217E-14,-1.66321791214601E-16,1.)) ;
#37695 = DIRECTION('center_axis',(-4.54195640846217E-14,1.66321791214601E-16,
-1.)) ;
#37696 = DIRECTION('ref_axis',(-1.,3.54035479944944E-31,4.54195640846217E-14)) ;
#37697 = DIRECTION('center_axis',(4.54195640846217E-14,-1.66321791214601E-16,
1.)) ;
#37698 = DIRECTION('ref_axis',(0.609355676053996,-0.792897004699083,-2.78085452289327E-14)) ;
#37699 = DIRECTION('',(4.54195640846217E-14,-1.66321791214601E-16,1.)) ;
#37700 = DIRECTION('center_axis',(4.54195640846217E-14,-1.66321791214601E-16,
1.)) ;
#37701 = DIRECTION('ref_axis',(0.609355676053996,-0.792897004699083,-2.78085452289327E-14)) ;
#37702 = DIRECTION('',(4.54195640846217E-14,-1.66321791214601E-16,1.)) ;
#37703 = DIRECTION('center_axis',(4.54195640846217E-14,-1.66321791214601E-16,
1.)) ;
#37704 = DIRECTION('ref_axis',(-1.,3.54035479944944E-31,4.54195640846217E-14)) ;
#37705 = DIRECTION('center_axis',(4.54195640846217E-14,-1.66321791214601E-16,
1.)) ;
#37706 = DIRECTION('ref_axis',(-0.938429938932521,-0.345469607512881,4.25656196263415E-14)) ;
#37707 = DIRECTION('',(4.54195640846217E-14,-1.66321791214601E-16,1.)) ;
#37708 = DIRECTION('center_axis',(-4.54195640846217E-14,1.66321791214601E-16,
-1.)) ;
#37709 = DIRECTION('ref_axis',(-1.,5.55236256206829E-46,4.54195640846217E-14)) ;
#37710 = DIRECTION('center_axis',(4.54195640846217E-14,-1.66321791214601E-16,
1.)) ;
#37711 = DIRECTION('ref_axis',(-0.938429938932521,-0.345469607512881,4.25656196263415E-14)) ;
#37712 = DIRECTION('',(4.54195640846217E-14,-1.66321791214601E-16,1.)) ;
#37713 = DIRECTION('center_axis',(-4.54195640846217E-14,1.66321791214601E-16,
-1.)) ;
#37714 = DIRECTION('ref_axis',(-1.,5.55236256206829E-46,4.54195640846217E-14)) ;
#37715 = DIRECTION('center_axis',(4.54195640846217E-14,-1.66321791214601E-16,
1.)) ;
#37716 = DIRECTION('ref_axis',(-0.938429938932521,-0.345469607512881,4.25656196263415E-14)) ;
#37717 = DIRECTION('',(4.54195640846217E-14,-1.66321791214601E-16,1.)) ;
#37718 = DIRECTION('center_axis',(4.54195640846217E-14,-1.66321791214601E-16,
1.)) ;
#37719 = DIRECTION('ref_axis',(-1.,5.55236256206829E-46,4.54195640846217E-14)) ;
#37720 = DIRECTION('center_axis',(4.54195640846217E-14,-1.66321791214601E-16,
1.)) ;
#37721 = DIRECTION('ref_axis',(-0.938428681849293,-0.345473022221127,4.25655619622289E-14)) ;
#37722 = DIRECTION('',(4.54195640846217E-14,-1.66321791214601E-16,1.)) ;
#37723 = DIRECTION('center_axis',(-4.54195640846217E-14,1.66321791214601E-16,
-1.)) ;
#37724 = DIRECTION('ref_axis',(-1.,5.55236256206829E-46,4.54195640846217E-14)) ;
#37725 = DIRECTION('center_axis',(4.54195640846217E-14,-1.66321791214601E-16,
1.)) ;
#37726 = DIRECTION('ref_axis',(-0.938428681849293,-0.345473022221127,4.25655619622289E-14)) ;
#37727 = DIRECTION('',(4.54195640846217E-14,-1.66321791214601E-16,1.)) ;
#37728 = DIRECTION('center_axis',(-4.54195640846217E-14,1.66321791214601E-16,
-1.)) ;
#37729 = DIRECTION('ref_axis',(-1.,5.55236256206829E-46,4.54195640846217E-14)) ;
#37730 = DIRECTION('center_axis',(4.54195640846217E-14,-1.66321791214601E-16,
1.)) ;
#37731 = DIRECTION('ref_axis',(-0.938428681849293,-0.345473022221127,4.25655619622289E-14)) ;
#37732 = DIRECTION('',(4.54195640846217E-14,-1.66321791214601E-16,1.)) ;
#37733 = DIRECTION('center_axis',(4.54195640846217E-14,-1.66321791214601E-16,
1.)) ;
#37734 = DIRECTION('ref_axis',(-1.,5.55236256206829E-46,4.54195640846217E-14)) ;
#37735 = DIRECTION('center_axis',(4.54195640846217E-14,-1.66321791214601E-16,
1.)) ;
#37736 = DIRECTION('ref_axis',(-0.938433691542647,-0.345459413792185,4.25657917636955E-14)) ;
#37737 = DIRECTION('',(4.54195640846217E-14,-1.66321791214601E-16,1.)) ;
#37738 = DIRECTION('center_axis',(-4.54195640846217E-14,1.66321791214601E-16,
-1.)) ;
#37739 = DIRECTION('ref_axis',(-1.,5.55236256206829E-46,4.54195640846217E-14)) ;
#37740 = DIRECTION('center_axis',(4.54195640846217E-14,-1.66321791214601E-16,
1.)) ;
#37741 = DIRECTION('ref_axis',(-0.938433691542647,-0.345459413792185,4.25657917636955E-14)) ;
#37742 = DIRECTION('',(4.54195640846217E-14,-1.66321791214601E-16,1.)) ;
#37743 = DIRECTION('center_axis',(-4.54195640846217E-14,1.66321791214601E-16,
-1.)) ;
#37744 = DIRECTION('ref_axis',(-1.,5.55236256206829E-46,4.54195640846217E-14)) ;
#37745 = DIRECTION('center_axis',(4.54195640846217E-14,-1.66321791214601E-16,
1.)) ;
#37746 = DIRECTION('ref_axis',(-0.938433691542647,-0.345459413792185,4.25657917636955E-14)) ;
#37747 = DIRECTION('',(4.54195640846217E-14,-1.66321791214601E-16,1.)) ;
#37748 = DIRECTION('center_axis',(4.54195640846217E-14,-1.66321791214601E-16,
1.)) ;
#37749 = DIRECTION('ref_axis',(-1.,5.55236256206829E-46,4.54195640846217E-14)) ;
#37750 = DIRECTION('center_axis',(4.54195640846217E-14,-1.66321791214601E-16,
1.)) ;
#37751 = DIRECTION('ref_axis',(-0.938432448023048,-0.345462791769924,4.25657347217461E-14)) ;
#37752 = DIRECTION('',(4.54195640846217E-14,-1.66321791214601E-16,1.)) ;
#37753 = DIRECTION('center_axis',(-4.54195640846217E-14,1.66321791214601E-16,
-1.)) ;
#37754 = DIRECTION('ref_axis',(-1.,5.55236256206829E-46,4.54195640846217E-14)) ;
#37755 = DIRECTION('center_axis',(4.54195640846217E-14,-1.66321791214601E-16,
1.)) ;
#37756 = DIRECTION('ref_axis',(-0.938432448023048,-0.345462791769924,4.25657347217461E-14)) ;
#37757 = DIRECTION('',(4.54195640846217E-14,-1.66321791214601E-16,1.)) ;
#37758 = DIRECTION('center_axis',(-4.54195640846217E-14,1.66321791214601E-16,
-1.)) ;
#37759 = DIRECTION('ref_axis',(-1.,5.55236256206829E-46,4.54195640846217E-14)) ;
#37760 = DIRECTION('center_axis',(4.54195640846217E-14,-1.66321791214601E-16,
1.)) ;
#37761 = DIRECTION('ref_axis',(-0.938432448023048,-0.345462791769924,4.25657347217461E-14)) ;
#37762 = DIRECTION('',(4.54195640846217E-14,-1.66321791214601E-16,1.)) ;
#37763 = DIRECTION('center_axis',(4.54195640846217E-14,-1.66321791214601E-16,
1.)) ;
#37764 = DIRECTION('ref_axis',(-1.,5.55236256206829E-46,4.54195640846217E-14)) ;
#37765 = DIRECTION('center_axis',(1.75658099177411E-13,1.,1.66321791206623E-16)) ;
#37766 = DIRECTION('ref_axis',(-0.792895134159569,1.39177102581146E-13,0.609358110002713)) ;
#37767 = DIRECTION('',(1.75658099177411E-13,1.,1.66321791206623E-16)) ;
#37768 = DIRECTION('center_axis',(-1.75658099177411E-13,-1.,-1.66321791206623E-16)) ;
#37769 = DIRECTION('ref_axis',(1.72902478588661E-14,1.66321791203586E-16,
-1.)) ;
#37770 = DIRECTION('center_axis',(1.75658099177411E-13,1.,1.66321791206623E-16)) ;
#37771 = DIRECTION('ref_axis',(-0.792895134159569,1.39177102581146E-13,0.609358110002713)) ;
#37772 = DIRECTION('',(1.75658099177411E-13,1.,1.66321791206623E-16)) ;
#37773 = DIRECTION('center_axis',(1.75658099177411E-13,1.,1.66321791206623E-16)) ;
#37774 = DIRECTION('ref_axis',(0.195317858763442,-3.44722822381472E-14,0.980739993090964)) ;
#37775 = DIRECTION('',(1.75658099177411E-13,1.,1.66321791206623E-16)) ;
#37776 = DIRECTION('center_axis',(1.75658099177411E-13,1.,1.66321791206623E-16)) ;
#37777 = DIRECTION('ref_axis',(1.72902478588661E-14,1.66321791203586E-16,
-1.)) ;
#37778 = DIRECTION('center_axis',(1.75658099177411E-13,1.,1.66321791206623E-16)) ;
#37779 = DIRECTION('ref_axis',(-0.792888490970559,1.39175934213506E-13,0.609366754004868)) ;
#37780 = DIRECTION('',(1.75658099177411E-13,1.,1.66321791206623E-16)) ;
#37781 = DIRECTION('center_axis',(-1.75658099177411E-13,-1.,-1.66321791206623E-16)) ;
#37782 = DIRECTION('ref_axis',(2.16128098235828E-15,1.66321791206243E-16,
-1.)) ;
#37783 = DIRECTION('center_axis',(1.75658099177411E-13,1.,1.66321791206623E-16)) ;
#37784 = DIRECTION('ref_axis',(-0.792888490970559,1.39175934213506E-13,0.609366754004868)) ;
#37785 = DIRECTION('',(1.75658099177411E-13,1.,1.66321791206623E-16)) ;
#37786 = DIRECTION('center_axis',(1.75658099177411E-13,1.,1.66321791206623E-16)) ;
#37787 = DIRECTION('ref_axis',(-0.792888490970559,1.39175934213506E-13,0.609366754004868)) ;
#37788 = DIRECTION('',(1.75658099177411E-13,1.,1.66321791206623E-16)) ;
#37789 = DIRECTION('center_axis',(1.75658099177411E-13,1.,1.66321791206623E-16)) ;
#37790 = DIRECTION('ref_axis',(2.16128098235828E-15,1.66321791206243E-16,
-1.)) ;
#37791 = DIRECTION('center_axis',(1.75658099177411E-13,1.,1.66321791206623E-16)) ;
#37792 = DIRECTION('ref_axis',(-0.345475903104034,6.08417214137425E-14,-0.938427621276384)) ;
#37793 = DIRECTION('',(1.75658099177411E-13,1.,1.66321791206623E-16)) ;
#37794 = DIRECTION('center_axis',(-1.75658099177411E-13,-1.,-1.66321791206623E-16)) ;
#37795 = DIRECTION('ref_axis',(2.14929886997261E-46,1.66321791206623E-16,
-1.)) ;
#37796 = DIRECTION('center_axis',(1.75658099177411E-13,1.,1.66321791206623E-16)) ;
#37797 = DIRECTION('ref_axis',(-0.345475903104034,6.08417214137425E-14,-0.938427621276384)) ;
#37798 = DIRECTION('',(1.75658099177411E-13,1.,1.66321791206623E-16)) ;
#37799 = DIRECTION('center_axis',(-1.75658099177411E-13,-1.,-1.66321791206623E-16)) ;
#37800 = DIRECTION('ref_axis',(2.14929886997261E-46,1.66321791206623E-16,
-1.)) ;
#37801 = DIRECTION('center_axis',(1.75658099177411E-13,1.,1.66321791206623E-16)) ;
#37802 = DIRECTION('ref_axis',(-0.345475903104034,6.08417214137425E-14,-0.938427621276384)) ;
#37803 = DIRECTION('',(1.75658099177411E-13,1.,1.66321791206623E-16)) ;
#37804 = DIRECTION('center_axis',(1.75658099177411E-13,1.,1.66321791206623E-16)) ;
#37805 = DIRECTION('ref_axis',(2.14929886997261E-46,1.66321791206623E-16,
-1.)) ;
#37806 = DIRECTION('center_axis',(1.75658099177411E-13,1.,1.66321791206623E-16)) ;
#37807 = DIRECTION('ref_axis',(-0.345465672469094,6.08399249462695E-14,-0.938431387553441)) ;
#37808 = DIRECTION('',(1.75658099177411E-13,1.,1.66321791206623E-16)) ;
#37809 = DIRECTION('center_axis',(-1.75658099177411E-13,-1.,-1.66321791206623E-16)) ;
#37810 = DIRECTION('ref_axis',(2.14929886997261E-46,1.66321791206623E-16,
-1.)) ;
#37811 = DIRECTION('center_axis',(1.75658099177411E-13,1.,1.66321791206623E-16)) ;
#37812 = DIRECTION('ref_axis',(-0.345465672469094,6.08399249462695E-14,-0.938431387553441)) ;
#37813 = DIRECTION('',(1.75658099177411E-13,1.,1.66321791206623E-16)) ;
#37814 = DIRECTION('center_axis',(-1.75658099177411E-13,-1.,-1.66321791206623E-16)) ;
#37815 = DIRECTION('ref_axis',(2.14929886997261E-46,1.66321791206623E-16,
-1.)) ;
#37816 = DIRECTION('center_axis',(1.75658099177411E-13,1.,1.66321791206623E-16)) ;
#37817 = DIRECTION('ref_axis',(-0.345465672469094,6.08399249462695E-14,-0.938431387553441)) ;
#37818 = DIRECTION('',(1.75658099177411E-13,1.,1.66321791206623E-16)) ;
#37819 = DIRECTION('center_axis',(1.75658099177411E-13,1.,1.66321791206623E-16)) ;
#37820 = DIRECTION('ref_axis',(2.14929886997261E-46,1.66321791206623E-16,
-1.)) ;
#37821 = DIRECTION('center_axis',(-1.75658099177411E-13,-1.,-1.66321791206623E-16)) ;
#37822 = DIRECTION('ref_axis',(-0.792900091868732,1.39380671434654E-13,-0.609351658990567)) ;
#37823 = DIRECTION('',(-1.75658099177411E-13,-1.,-1.66321791206623E-16)) ;
#37824 = DIRECTION('center_axis',(1.75658099177411E-13,1.,1.66321791206623E-16)) ;
#37825 = DIRECTION('ref_axis',(-1.72902478588661E-14,-1.66321791203586E-16,
1.)) ;
#37826 = DIRECTION('center_axis',(-1.75658099177411E-13,-1.,-1.66321791206623E-16)) ;
#37827 = DIRECTION('ref_axis',(-0.792900091868732,1.39380671434654E-13,-0.609351658990567)) ;
#37828 = DIRECTION('',(-1.75658099177411E-13,-1.,-1.66321791206623E-16)) ;
#37829 = DIRECTION('center_axis',(-1.75658099177411E-13,-1.,-1.66321791206623E-16)) ;
#37830 = DIRECTION('ref_axis',(-0.792900091868732,1.39380671434654E-13,-0.609351658990567)) ;
#37831 = DIRECTION('',(-1.75658099177411E-13,-1.,-1.66321791206623E-16)) ;
#37832 = DIRECTION('center_axis',(-1.75658099177411E-13,-1.,-1.66321791206623E-16)) ;
#37833 = DIRECTION('ref_axis',(-1.72902478588661E-14,-1.66321791203586E-16,
1.)) ;
#37834 = DIRECTION('center_axis',(-1.75658099177411E-13,-1.,-1.66321791206623E-16)) ;
#37835 = DIRECTION('ref_axis',(-0.792893488573911,1.39379512941514E-13,-0.609360251228363)) ;
#37836 = DIRECTION('',(-1.75658099177411E-13,-1.,-1.66321791206623E-16)) ;
#37837 = DIRECTION('center_axis',(1.75658099177411E-13,1.,1.66321791206623E-16)) ;
#37838 = DIRECTION('ref_axis',(6.48384294707473E-15,-1.66321791207762E-16,
1.)) ;
#37839 = DIRECTION('center_axis',(-1.75658099177411E-13,-1.,-1.66321791206623E-16)) ;
#37840 = DIRECTION('ref_axis',(-0.792893488573911,1.39379512941514E-13,-0.609360251228363)) ;
#37841 = DIRECTION('',(-1.75658099177411E-13,-1.,-1.66321791206623E-16)) ;
#37842 = DIRECTION('center_axis',(-1.75658099177411E-13,-1.,-1.66321791206623E-16)) ;
#37843 = DIRECTION('ref_axis',(-0.792893488573911,1.39379512941514E-13,-0.609360251228363)) ;
#37844 = DIRECTION('',(-1.75658099177411E-13,-1.,-1.66321791206623E-16)) ;
#37845 = DIRECTION('center_axis',(-1.75658099177411E-13,-1.,-1.66321791206623E-16)) ;
#37846 = DIRECTION('ref_axis',(6.48384294707473E-15,-1.66321791207762E-16,
1.)) ;
#37847 = DIRECTION('center_axis',(-1.75658099177411E-13,-1.,-1.66321791206623E-16)) ;
#37848 = DIRECTION('ref_axis',(-0.345468206718894,6.05282070843357E-14,0.938430454613676)) ;
#37849 = DIRECTION('',(-1.75658099177411E-13,-1.,-1.66321791206623E-16)) ;
#37850 = DIRECTION('center_axis',(1.75658099177411E-13,1.,1.66321791206623E-16)) ;
#37851 = DIRECTION('ref_axis',(-2.14929886997261E-46,-1.66321791206623E-16,
1.)) ;
#37852 = DIRECTION('center_axis',(-1.75658099177411E-13,-1.,-1.66321791206623E-16)) ;
#37853 = DIRECTION('ref_axis',(-0.345468206718894,6.05282070843357E-14,0.938430454613676)) ;
#37854 = DIRECTION('',(-1.75658099177411E-13,-1.,-1.66321791206623E-16)) ;
#37855 = DIRECTION('center_axis',(1.75658099177411E-13,1.,1.66321791206623E-16)) ;
#37856 = DIRECTION('ref_axis',(-2.14929886997261E-46,-1.66321791206623E-16,
1.)) ;
#37857 = DIRECTION('center_axis',(-1.75658099177411E-13,-1.,-1.66321791206623E-16)) ;
#37858 = DIRECTION('ref_axis',(-0.345468206718894,6.05282070843357E-14,0.938430454613676)) ;
#37859 = DIRECTION('',(-1.75658099177411E-13,-1.,-1.66321791206623E-16)) ;
#37860 = DIRECTION('center_axis',(-1.75658099177411E-13,-1.,-1.66321791206623E-16)) ;
#37861 = DIRECTION('ref_axis',(-2.14929886997261E-46,-1.66321791206623E-16,
1.)) ;
#37862 = DIRECTION('center_axis',(-1.75658099177411E-13,-1.,-1.66321791206623E-16)) ;
#37863 = DIRECTION('ref_axis',(-0.345458037383117,6.05264201354982E-14,0.938434198229905)) ;
#37864 = DIRECTION('',(-1.75658099177411E-13,-1.,-1.66321791206623E-16)) ;
#37865 = DIRECTION('center_axis',(1.75658099177411E-13,1.,1.66321791206623E-16)) ;
#37866 = DIRECTION('ref_axis',(-2.14929886997261E-46,-1.66321791206623E-16,
1.)) ;
#37867 = DIRECTION('center_axis',(-1.75658099177411E-13,-1.,-1.66321791206623E-16)) ;
#37868 = DIRECTION('ref_axis',(-0.345458037383117,6.05264201354982E-14,0.938434198229905)) ;
#37869 = DIRECTION('',(-1.75658099177411E-13,-1.,-1.66321791206623E-16)) ;
#37870 = DIRECTION('center_axis',(1.75658099177411E-13,1.,1.66321791206623E-16)) ;
#37871 = DIRECTION('ref_axis',(-2.14929886997261E-46,-1.66321791206623E-16,
1.)) ;
#37872 = DIRECTION('center_axis',(-1.75658099177411E-13,-1.,-1.66321791206623E-16)) ;
#37873 = DIRECTION('ref_axis',(-0.345458037383117,6.05264201354982E-14,0.938434198229905)) ;
#37874 = DIRECTION('',(-1.75658099177411E-13,-1.,-1.66321791206623E-16)) ;
#37875 = DIRECTION('center_axis',(-1.75658099177411E-13,-1.,-1.66321791206623E-16)) ;
#37876 = DIRECTION('ref_axis',(-2.14929886997261E-46,-1.66321791206623E-16,
1.)) ;
#37877 = DIRECTION('center_axis',(-1.75658099177411E-13,-1.,-1.66321791206623E-16)) ;
#37878 = DIRECTION('ref_axis',(-0.345458037383117,6.05264201354982E-14,0.938434198229905)) ;
#37879 = DIRECTION('center_axis',(-1.75658099177411E-13,-1.,-1.66321791206623E-16)) ;
#37880 = DIRECTION('ref_axis',(-0.345468206718894,6.05282070843357E-14,0.938430454613676)) ;
#37881 = DIRECTION('center_axis',(-1.75658099177411E-13,-1.,-1.66321791206623E-16)) ;
#37882 = DIRECTION('ref_axis',(-0.792893488573911,1.39379512941514E-13,-0.609360251228363)) ;
#37883 = DIRECTION('center_axis',(-1.75658099177411E-13,-1.,-1.66321791206623E-16)) ;
#37884 = DIRECTION('ref_axis',(-0.792900091868732,1.39380671434654E-13,-0.609351658990567)) ;
#37885 = DIRECTION('center_axis',(1.75658099177411E-13,1.,1.66321791206623E-16)) ;
#37886 = DIRECTION('ref_axis',(-0.345465672469094,6.08399249462695E-14,-0.938431387553441)) ;
#37887 = DIRECTION('center_axis',(1.75658099177411E-13,1.,1.66321791206623E-16)) ;
#37888 = DIRECTION('ref_axis',(-0.345475903104034,6.08417214137425E-14,-0.938427621276384)) ;
#37889 = DIRECTION('center_axis',(1.75658099177411E-13,1.,1.66321791206623E-16)) ;
#37890 = DIRECTION('ref_axis',(-0.792888490970559,1.39175934213506E-13,0.609366754004868)) ;
#37891 = DIRECTION('center_axis',(1.75658099177411E-13,1.,1.66321791206623E-16)) ;
#37892 = DIRECTION('ref_axis',(-0.792895134159569,1.39177102581146E-13,0.609358110002713)) ;
#37893 = DIRECTION('center_axis',(4.54195640846217E-14,-1.66321791214601E-16,
1.)) ;
#37894 = DIRECTION('ref_axis',(-0.938432448023048,-0.345462791769924,4.25657347217461E-14)) ;
#37895 = DIRECTION('center_axis',(4.54195640846217E-14,-1.66321791214601E-16,
1.)) ;
#37896 = DIRECTION('ref_axis',(-0.938433691542647,-0.345459413792185,4.25657917636955E-14)) ;
#37897 = DIRECTION('center_axis',(4.54195640846217E-14,-1.66321791214601E-16,
1.)) ;
#37898 = DIRECTION('ref_axis',(-0.938428681849293,-0.345473022221127,4.25655619622289E-14)) ;
#37899 = DIRECTION('center_axis',(4.54195640846217E-14,-1.66321791214601E-16,
1.)) ;
#37900 = DIRECTION('ref_axis',(-0.938429938932521,-0.345469607512881,4.25656196263415E-14)) ;
#37901 = DIRECTION('center_axis',(4.54195640846217E-14,-1.66321791214601E-16,
1.)) ;
#37902 = DIRECTION('ref_axis',(0.609355676053996,-0.792897004699083,-2.78085452289327E-14)) ;
#37903 = DIRECTION('center_axis',(4.54195640846217E-14,-1.66321791214601E-16,
1.)) ;
#37904 = DIRECTION('ref_axis',(0.609364319911517,-0.792890361663436,-2.78089367242917E-14)) ;
#37905 = DIRECTION('center_axis',(4.54195640846217E-14,-1.66321791214601E-16,
1.)) ;
#37906 = DIRECTION('ref_axis',(0.980619819129883,0.195920316275966,-4.45067388996815E-14)) ;
#37907 = DIRECTION('center_axis',(4.54195640846217E-14,-1.66321791214601E-16,
1.)) ;
#37908 = DIRECTION('ref_axis',(0.609352821942987,-0.792899198126797,-2.78084159612697E-14)) ;
#37909 = DIRECTION('center_axis',(-1.,1.75658099177411E-13,4.54195640846217E-14)) ;
#37910 = DIRECTION('ref_axis',(9.20925513359107E-14,0.707106781186535,-0.70710678118656)) ;
#37911 = DIRECTION('center_axis',(-1.,1.75658099177411E-13,4.54195640846217E-14)) ;
#37912 = DIRECTION('ref_axis',(9.20925513359107E-14,0.707106781186535,-0.70710678118656)) ;
#37913 = DIRECTION('',(-1.,1.75658099177411E-13,4.54195640846217E-14)) ;
#37914 = DIRECTION('center_axis',(-1.,1.75658099177411E-13,4.54195640846217E-14)) ;
#37915 = DIRECTION('ref_axis',(9.20925513359107E-14,0.707106781186535,-0.70710678118656)) ;
#37916 = DIRECTION('',(1.,-1.75658099177411E-13,-4.54195640846217E-14)) ;
#37917 = DIRECTION('center_axis',(-1.75658099177411E-13,-1.,-1.66321791206623E-16)) ;
#37918 = DIRECTION('ref_axis',(4.54195640846217E-14,-1.66321791214601E-16,
1.)) ;
#37919 = DIRECTION('center_axis',(1.75658099177411E-13,1.,1.66321791206623E-16)) ;
#37920 = DIRECTION('ref_axis',(4.54195640846217E-14,-1.66321791214601E-16,
1.)) ;
#37921 = DIRECTION('',(-1.75658099177413E-13,-1.,-4.27988859368166E-14)) ;
#37922 = DIRECTION('center_axis',(-1.75658099177411E-13,-1.,-1.66321791206623E-16)) ;
#37923 = DIRECTION('ref_axis',(4.54195640846217E-14,-1.66321791214601E-16,
1.)) ;
#37924 = DIRECTION('',(1.63182045051861E-13,1.,1.66321791207189E-16)) ;
#37925 = DIRECTION('center_axis',(-1.75658099177411E-13,-1.,-1.66321791206623E-16)) ;
#37926 = DIRECTION('ref_axis',(1.,-1.75658099177411E-13,-4.54195640846217E-14)) ;
#37927 = DIRECTION('center_axis',(1.75658099177411E-13,1.,1.66321791206623E-16)) ;
#37928 = DIRECTION('ref_axis',(1.,-1.75658099177411E-13,-4.54195640846217E-14)) ;
#37929 = DIRECTION('',(-1.75658099177411E-13,-1.,-1.66321791206623E-16)) ;
#37930 = DIRECTION('center_axis',(-1.75658099177411E-13,-1.,-1.66321791206623E-16)) ;
#37931 = DIRECTION('ref_axis',(1.,-1.75658099177411E-13,-4.54195640846217E-14)) ;
#37932 = DIRECTION('',(1.75658099177411E-13,1.,1.66321791206623E-16)) ;
#37933 = DIRECTION('center_axis',(1.75658099177411E-13,1.,1.66321791206623E-16)) ;
#37934 = DIRECTION('ref_axis',(4.54195640846217E-14,-1.66321791214601E-16,
1.)) ;
#37935 = DIRECTION('center_axis',(-1.75658099177411E-13,-1.,-1.66321791206623E-16)) ;
#37936 = DIRECTION('ref_axis',(4.54195640846217E-14,-1.66321791214601E-16,
1.)) ;
#37937 = DIRECTION('',(1.75658099177411E-13,1.,1.66321791206623E-16)) ;
#37938 = DIRECTION('center_axis',(1.75658099177411E-13,1.,1.66321791206623E-16)) ;
#37939 = DIRECTION('ref_axis',(4.54195640846217E-14,-1.66321791214601E-16,
1.)) ;
#37940 = DIRECTION('',(-1.75658099177411E-13,-1.,-1.66321791206623E-16)) ;
#37941 = DIRECTION('center_axis',(1.75658099177411E-13,1.,1.66321791206623E-16)) ;
#37942 = DIRECTION('ref_axis',(-1.,1.75658099177411E-13,4.54195640846217E-14)) ;
#37943 = DIRECTION('center_axis',(-1.75658099177411E-13,-1.,-1.66321791206623E-16)) ;
#37944 = DIRECTION('ref_axis',(-1.,1.75658099177411E-13,4.54195640846217E-14)) ;
#37945 = DIRECTION('',(1.63182045051861E-13,1.,1.66321791207189E-16)) ;
#37946 = DIRECTION('center_axis',(1.75658099177411E-13,1.,1.66321791206623E-16)) ;
#37947 = DIRECTION('ref_axis',(-1.,1.75658099177411E-13,4.54195640846217E-14)) ;
#37948 = DIRECTION('',(-1.75658099177411E-13,-1.,-1.66321791206623E-16)) ;
#37949 = DIRECTION('center_axis',(1.,-1.75658099177411E-13,-4.54195640846217E-14)) ;
#37950 = DIRECTION('ref_axis',(4.54195640846217E-14,-1.66321791214601E-16,
1.)) ;
#37951 = DIRECTION('',(1.75658099177411E-13,1.,1.66321791206623E-16)) ;
#37952 = DIRECTION('center_axis',(1.,-1.75658099177411E-13,-4.54195640846217E-14)) ;
#37953 = DIRECTION('ref_axis',(-1.56325514861458E-13,-0.707106781186535,-0.70710678118656)) ;
#37954 = DIRECTION('',(-4.54195640846217E-14,1.66321791214601E-16,-1.)) ;
#37955 = DIRECTION('',(4.54195640846217E-14,-1.66321791214601E-16,1.)) ;
#37956 = DIRECTION('center_axis',(-1.,1.75658099177411E-13,4.54195640846217E-14)) ;
#37957 = DIRECTION('ref_axis',(-1.75658099177411E-13,-1.,-1.66321791206623E-16)) ;
#37958 = DIRECTION('',(-1.75658099177411E-13,-1.,-1.66321791206623E-16)) ;
#37959 = DIRECTION('center_axis',(-1.,1.75658099177411E-13,4.54195640846217E-14)) ;
#37960 = DIRECTION('ref_axis',(-4.54195640846217E-14,1.66321791214601E-16,
-1.)) ;
#37961 = DIRECTION('',(-4.54195640846217E-14,1.66321791214601E-16,-1.)) ;
#37962 = DIRECTION('',(4.54195640846217E-14,-1.66321791214601E-16,1.)) ;
#37963 = DIRECTION('center_axis',(1.75658099177411E-13,1.,1.66321791206623E-16)) ;
#37964 = DIRECTION('ref_axis',(-4.54195640846217E-14,1.66321791214601E-16,
-1.)) ;
#37965 = DIRECTION('center_axis',(-1.63182045051861E-13,-1.,0.)) ;
#37966 = DIRECTION('ref_axis',(-4.54195640846217E-14,7.41165735269263E-27,
-1.)) ;
#37967 = DIRECTION('',(1.75658099177411E-13,1.,1.66321791206623E-16)) ;
#37968 = DIRECTION('center_axis',(1.63182045051861E-13,1.,0.)) ;
#37969 = DIRECTION('ref_axis',(-4.54195640846217E-14,7.41165735269263E-27,
-1.)) ;
#37970 = DIRECTION('',(1.75658099177411E-13,1.,1.66321791206623E-16)) ;
#37971 = DIRECTION('center_axis',(-1.63182045051861E-13,-1.,-1.66321791207189E-16)) ;
#37972 = DIRECTION('ref_axis',(-0.707106781186566,1.15504737890484E-13,-0.707106781186529)) ;
#37973 = DIRECTION('center_axis',(-1.63182045051861E-13,-1.,0.)) ;
#37974 = DIRECTION('ref_axis',(-0.707106781186566,1.15387130624063E-13,-0.707106781186529)) ;
#37975 = DIRECTION('',(1.63182045051861E-13,1.,1.66321791207189E-16)) ;
#37976 = DIRECTION('center_axis',(-1.63182045051861E-13,-1.,0.)) ;
#37977 = DIRECTION('ref_axis',(-0.707106781186566,1.15387130624063E-13,-0.707106781186529)) ;
#37978 = DIRECTION('',(-1.63182045051861E-13,-1.,-1.66321791207189E-16)) ;
#37979 = DIRECTION('center_axis',(1.75658099177411E-13,1.,1.66321791206623E-16)) ;
#37980 = DIRECTION('ref_axis',(-4.54195640846217E-14,1.66321791214601E-16,
-1.)) ;
#37981 = DIRECTION('',(-1.,1.75658099177411E-13,4.54195640846217E-14)) ;
#37982 = DIRECTION('',(1.,-1.75658099177411E-13,-4.54195640846217E-14)) ;
#37983 = DIRECTION('',(-4.54195640846217E-14,1.66321791214601E-16,-1.)) ;
#37984 = DIRECTION('center_axis',(1.75658099177411E-13,1.,1.66321791206623E-16)) ;
#37985 = DIRECTION('ref_axis',(-1.,1.75658099177411E-13,4.54195640846217E-14)) ;
#37986 = DIRECTION('',(-4.54195640846217E-14,1.66321791214601E-16,-1.)) ;
#37987 = DIRECTION('',(1.,-1.75658099177411E-13,-4.54195640846217E-14)) ;
#37988 = DIRECTION('',(-4.54195640846217E-14,1.66321791214601E-16,-1.)) ;
#37989 = DIRECTION('center_axis',(1.75658099177411E-13,1.,1.66321791206623E-16)) ;
#37990 = DIRECTION('ref_axis',(-1.,1.75658099177411E-13,4.54195640846217E-14)) ;
#37991 = DIRECTION('',(-4.54195640846217E-14,1.66321791214601E-16,-1.)) ;
#37992 = DIRECTION('',(1.,-1.75658099177411E-13,-4.54195640846217E-14)) ;
#37993 = DIRECTION('',(2.71407300257853E-29,1.66321791206623E-16,-1.)) ;
#37994 = DIRECTION('',(1.,-1.75658099177411E-13,0.)) ;
#37995 = DIRECTION('',(-4.54195640846217E-14,1.66321791214601E-16,-1.)) ;
#37996 = DIRECTION('',(-1.,1.75658099177411E-13,4.54195640846217E-14)) ;
#37997 = DIRECTION('',(-4.54195640846217E-14,1.66321791214601E-16,-1.)) ;
#37998 = DIRECTION('',(-1.,1.75658099177411E-13,4.54195640846217E-14)) ;
#37999 = DIRECTION('',(4.54195640846217E-14,-1.66321791214601E-16,1.)) ;
#38000 = DIRECTION('',(-1.,1.75658099177411E-13,4.54195640846217E-14)) ;
#38001 = DIRECTION('',(4.54195640846217E-14,-1.66321791214601E-16,1.)) ;
#38002 = DIRECTION('center_axis',(1.75658099177411E-13,1.,1.66321791206623E-16)) ;
#38003 = DIRECTION('ref_axis',(-0.707106781186586,1.24326640365114E-13,-0.707106781186509)) ;
#38004 = DIRECTION('',(-1.,1.75658099177411E-13,4.54195640846217E-14)) ;
#38005 = DIRECTION('center_axis',(1.75658099177411E-13,1.,1.66321791206623E-16)) ;
#38006 = DIRECTION('ref_axis',(0.707106781186528,-1.24091425832262E-13,-0.707106781186567)) ;
#38007 = DIRECTION('',(-4.54195640846217E-14,1.66321791214601E-16,-1.)) ;
#38008 = DIRECTION('',(-1.,1.75658099177411E-13,4.54195640846217E-14)) ;
#38009 = DIRECTION('',(-4.54195640846217E-14,1.66321791214601E-16,-1.)) ;
#38010 = DIRECTION('',(1.,-1.75658099177411E-13,-4.54195640846217E-14)) ;
#38011 = DIRECTION('',(-4.54195640846217E-14,1.66321791214601E-16,-1.)) ;
#38012 = DIRECTION('center_axis',(1.75658099177411E-13,1.,1.66321791206623E-16)) ;
#38013 = DIRECTION('ref_axis',(1.,-1.75658099177411E-13,-4.54195640846217E-14)) ;
#38014 = DIRECTION('',(1.,-1.75658099177411E-13,-4.54195640846217E-14)) ;
#38015 = DIRECTION('',(4.54195640846217E-14,-1.66321791214601E-16,1.)) ;
#38016 = DIRECTION('',(-1.,1.75658099177411E-13,4.54195640846217E-14)) ;
#38017 = DIRECTION('',(-4.54195640846217E-14,1.66321791214601E-16,-1.)) ;
#38018 = DIRECTION('',(1.,-1.75658099177411E-13,-4.54195640846217E-14)) ;
#38019 = DIRECTION('',(4.54195640846217E-14,-1.66321791214601E-16,1.)) ;
#38020 = DIRECTION('',(-1.,1.75658099177411E-13,4.54195640846217E-14)) ;
#38021 = DIRECTION('',(-4.54195640846217E-14,1.66321791214601E-16,-1.)) ;
#38022 = DIRECTION('',(1.,-1.75658099177411E-13,-4.54195640846217E-14)) ;
#38023 = DIRECTION('',(4.54195640846217E-14,-1.66321791214601E-16,1.)) ;
#38024 = DIRECTION('',(-1.,1.75658099177411E-13,4.54195640846217E-14)) ;
#38025 = DIRECTION('',(-4.54195640846217E-14,1.66321791214601E-16,-1.)) ;
#38026 = DIRECTION('center_axis',(1.75658099177411E-13,1.,1.66321791206623E-16)) ;
#38027 = DIRECTION('ref_axis',(0.99999997726804,-1.75658059720776E-13,-0.000213222701069828)) ;
#38028 = DIRECTION('center_axis',(1.,-1.75658099177411E-13,-4.54195640846217E-14)) ;
#38029 = DIRECTION('ref_axis',(9.20925513359107E-14,0.707106781186535,-0.70710678118656)) ;
#38030 = DIRECTION('center_axis',(1.,-1.63182045051861E-13,0.)) ;
#38031 = DIRECTION('ref_axis',(1.15387130624058E-13,0.707106781186535,-0.70710678118656)) ;
#38032 = DIRECTION('',(1.,-1.75658099177411E-13,-4.54195640846217E-14)) ;
#38033 = DIRECTION('center_axis',(1.,-1.75658099177411E-13,-4.54195640846217E-14)) ;
#38034 = DIRECTION('ref_axis',(9.20925513359107E-14,0.707106781186535,-0.70710678118656)) ;
#38035 = DIRECTION('',(-1.,1.75658099177411E-13,4.54195640846217E-14)) ;
#38036 = DIRECTION('center_axis',(-1.75658099177411E-13,-1.,-1.66321791206623E-16)) ;
#38037 = DIRECTION('ref_axis',(4.54195640846217E-14,-1.66321791214601E-16,
1.)) ;
#38038 = DIRECTION('',(1.,-1.75658099177411E-13,-4.54195640846217E-14)) ;
#38039 = DIRECTION('',(4.54195640846217E-14,-1.66321791214601E-16,1.)) ;
#38040 = DIRECTION('',(-1.,1.75658099177411E-13,0.)) ;
#38041 = DIRECTION('',(-2.71407300257853E-29,-1.66321791206623E-16,1.)) ;
#38042 = DIRECTION('',(-4.54195640846217E-14,1.66321791214601E-16,-1.)) ;
#38043 = DIRECTION('center_axis',(-1.75658099177411E-13,-1.,-1.66321791206623E-16)) ;
#38044 = DIRECTION('ref_axis',(1.,-1.75658099177411E-13,-4.54195640846217E-14)) ;
#38045 = DIRECTION('',(4.54195640846217E-14,-1.66321791214601E-16,1.)) ;
#38046 = DIRECTION('',(-1.,1.75658099177411E-13,4.54195640846217E-14)) ;
#38047 = DIRECTION('',(-4.54195640846217E-14,1.66321791214601E-16,-1.)) ;
#38048 = DIRECTION('center_axis',(-1.75658099177411E-13,-1.,-1.66321791206623E-16)) ;
#38049 = DIRECTION('ref_axis',(1.,-1.75658099177411E-13,-4.54195640846217E-14)) ;
#38050 = DIRECTION('',(4.54195640846217E-14,-1.66321791214601E-16,1.)) ;
#38051 = DIRECTION('',(-1.,1.75658099177411E-13,4.54195640846217E-14)) ;
#38052 = DIRECTION('',(4.54195640846217E-14,-1.66321791214601E-16,1.)) ;
#38053 = DIRECTION('center_axis',(-1.75658099177411E-13,-1.,-1.66321791206623E-16)) ;
#38054 = DIRECTION('ref_axis',(-1.,1.75658099177411E-13,4.54195640846217E-14)) ;
#38055 = DIRECTION('',(4.54195640846217E-14,-1.66321791214601E-16,1.)) ;
#38056 = DIRECTION('',(-1.,1.75658099177411E-13,4.54195640846217E-14)) ;
#38057 = DIRECTION('',(4.54195640846217E-14,-1.66321791214601E-16,1.)) ;
#38058 = DIRECTION('center_axis',(-1.75658099177411E-13,-1.,-1.66321791206623E-16)) ;
#38059 = DIRECTION('ref_axis',(-1.,1.75658099177411E-13,4.54195640846217E-14)) ;
#38060 = DIRECTION('',(4.54195640846217E-14,-1.66321791214601E-16,1.)) ;
#38061 = DIRECTION('center_axis',(-1.75658099177411E-13,-1.,-1.66321791206623E-16)) ;
#38062 = DIRECTION('ref_axis',(1.,-1.75658099177411E-13,-4.54195640846217E-14)) ;
#38063 = DIRECTION('',(1.,-1.75658099177411E-13,-4.54195640846217E-14)) ;
#38064 = DIRECTION('',(-4.54195640846217E-14,1.66321791214601E-16,-1.)) ;
#38065 = DIRECTION('',(-1.,1.75658099177411E-13,4.54195640846217E-14)) ;
#38066 = DIRECTION('',(4.54195640846217E-14,-1.66321791214601E-16,1.)) ;
#38067 = DIRECTION('',(1.,-1.75658099177411E-13,-4.54195640846217E-14)) ;
#38068 = DIRECTION('',(-4.54195640846217E-14,1.66321791214601E-16,-1.)) ;
#38069 = DIRECTION('',(-1.,1.75658099177411E-13,4.54195640846217E-14)) ;
#38070 = DIRECTION('',(4.54195640846217E-14,-1.66321791214601E-16,1.)) ;
#38071 = DIRECTION('',(1.,-1.75658099177411E-13,-4.54195640846217E-14)) ;
#38072 = DIRECTION('',(-4.54195640846217E-14,1.66321791214601E-16,-1.)) ;
#38073 = DIRECTION('',(-1.,1.75658099177411E-13,4.54195640846217E-14)) ;
#38074 = DIRECTION('',(4.54195640846217E-14,-1.66321791214601E-16,1.)) ;
#38075 = DIRECTION('',(1.,-1.75658099177411E-13,-4.54195640846217E-14)) ;
#38076 = DIRECTION('',(-4.54195640846217E-14,1.66321791214601E-16,-1.)) ;
#38077 = DIRECTION('',(-1.,1.75658099177411E-13,4.54195640846217E-14)) ;
#38078 = DIRECTION('',(4.54195640846217E-14,-1.66321791214601E-16,1.)) ;
#38079 = DIRECTION('center_axis',(-1.75658099177411E-13,-1.,-1.66321791206623E-16)) ;
#38080 = DIRECTION('ref_axis',(0.00363593456997526,-8.05002047109562E-16,
0.999993389968055)) ;
#38081 = DIRECTION('',(2.92157696951376E-29,1.66321791206623E-16,-1.)) ;
#38082 = DIRECTION('center_axis',(-1.75658099177411E-13,-1.,-1.66321791206623E-16)) ;
#38083 = DIRECTION('ref_axis',(0.707106781186522,-1.24091425832261E-13,-0.707106781186573)) ;
#38084 = DIRECTION('',(-1.,1.75658099177411E-13,6.34413156928661E-16)) ;
#38085 = DIRECTION('center_axis',(-1.75658099177411E-13,-1.,-1.66321791206623E-16)) ;
#38086 = DIRECTION('ref_axis',(-0.707106781186573,1.24326640365112E-13,-0.707106781186523)) ;
#38087 = DIRECTION('',(-2.92157696951376E-29,-1.66321791206623E-16,1.)) ;
#38088 = DIRECTION('center_axis',(-1.75658099177411E-13,-1.,-1.66321791206623E-16)) ;
#38089 = DIRECTION('ref_axis',(-0.707106781186573,1.2409142583227E-13,0.707106781186523)) ;
#38090 = DIRECTION('',(1.,-1.75658099177411E-13,-3.1720657846433E-16)) ;
#38091 = DIRECTION('center_axis',(-1.75658099177411E-13,-1.,-1.66321791206623E-16)) ;
#38092 = DIRECTION('ref_axis',(0.707106781186522,-1.24326640365103E-13,0.707106781186573)) ;
#38093 = DIRECTION('',(1.,-1.75658099177411E-13,-4.54195640846217E-14)) ;
#38094 = DIRECTION('',(-4.54195640846217E-14,1.66321791214601E-16,-1.)) ;
#38095 = DIRECTION('',(1.,-1.75658099177411E-13,-4.54195640846217E-14)) ;
#38096 = DIRECTION('',(4.54195640846217E-14,-1.66321791214601E-16,1.)) ;
#38097 = DIRECTION('',(1.,-1.75658099177411E-13,-4.54195640846217E-14)) ;
#38098 = DIRECTION('',(4.54195640846217E-14,-1.66321791214601E-16,1.)) ;
#38099 = DIRECTION('center_axis',(-1.75658099177411E-13,-1.,-1.66321791206623E-16)) ;
#38100 = DIRECTION('ref_axis',(0.70710678118651,-1.24091425832259E-13,-0.707106781186585)) ;
#38101 = DIRECTION('',(1.,-1.75658099177411E-13,-4.54195640846217E-14)) ;
#38102 = DIRECTION('center_axis',(-1.75658099177411E-13,-1.,-1.66321791206623E-16)) ;
#38103 = DIRECTION('ref_axis',(-0.707106781186573,1.24326640365112E-13,-0.707106781186522)) ;
#38104 = DIRECTION('',(-4.54195640846217E-14,1.66321791214601E-16,-1.)) ;
#38105 = DIRECTION('center_axis',(1.75658099177411E-13,1.,1.66321791206623E-16)) ;
#38106 = DIRECTION('ref_axis',(-4.54195640846217E-14,1.66321791214601E-16,
-1.)) ;
#38107 = DIRECTION('',(4.54195640846217E-14,-1.66321791214601E-16,1.)) ;
#38108 = DIRECTION('',(-1.,1.75658099177411E-13,0.)) ;
#38109 = DIRECTION('',(-2.71407300257853E-29,-1.66321791206623E-16,1.)) ;
#38110 = DIRECTION('',(1.,-1.75658099177411E-13,-4.54195640846217E-14)) ;
#38111 = DIRECTION('',(4.54195640846217E-14,-1.66321791214601E-16,1.)) ;
#38112 = DIRECTION('center_axis',(1.75658099177411E-13,1.,1.66321791206623E-16)) ;
#38113 = DIRECTION('ref_axis',(-1.,1.75658099177411E-13,4.54195640846217E-14)) ;
#38114 = DIRECTION('',(4.54195640846217E-14,-1.66321791214601E-16,1.)) ;
#38115 = DIRECTION('',(-1.,1.75658099177411E-13,4.54195640846217E-14)) ;
#38116 = DIRECTION('',(4.54195640846217E-14,-1.66321791214601E-16,1.)) ;
#38117 = DIRECTION('center_axis',(1.75658099177411E-13,1.,1.66321791206623E-16)) ;
#38118 = DIRECTION('ref_axis',(-1.,1.75658099177411E-13,4.54195640846217E-14)) ;
#38119 = DIRECTION('',(-4.54195640846217E-14,1.66321791214601E-16,-1.)) ;
#38120 = DIRECTION('',(1.,-1.75658099177411E-13,-4.54195640846217E-14)) ;
#38121 = DIRECTION('',(1.,-1.75658099177411E-13,-4.54195640846217E-14)) ;
#38122 = DIRECTION('center_axis',(-1.75658099177411E-13,-1.,-1.66321791206623E-16)) ;
#38123 = DIRECTION('ref_axis',(1.,-1.75658099177411E-13,-4.54195640846217E-14)) ;
#38124 = DIRECTION('',(1.,-1.75658099177411E-13,-4.54195640846217E-14)) ;
#38125 = DIRECTION('',(-4.54195640846217E-14,1.66321791214601E-16,-1.)) ;
#38126 = DIRECTION('',(-1.,1.75658099177411E-13,4.54195640846217E-14)) ;
#38127 = DIRECTION('',(4.54195640846217E-14,-1.66321791214601E-16,1.)) ;
#38128 = DIRECTION('',(1.,-1.75658099177411E-13,-4.54195640846217E-14)) ;
#38129 = DIRECTION('',(-4.54195640846217E-14,1.66321791214601E-16,-1.)) ;
#38130 = DIRECTION('',(-1.,1.75658099177411E-13,4.54195640846217E-14)) ;
#38131 = DIRECTION('',(4.54195640846217E-14,-1.66321791214601E-16,1.)) ;
#38132 = DIRECTION('',(1.,-1.75658099177411E-13,-4.54195640846217E-14)) ;
#38133 = DIRECTION('',(-4.54195640846217E-14,1.66321791214601E-16,-1.)) ;
#38134 = DIRECTION('',(-1.,1.75658099177411E-13,4.54195640846217E-14)) ;
#38135 = DIRECTION('',(4.54195640846217E-14,-1.66321791214601E-16,1.)) ;
#38136 = DIRECTION('center_axis',(1.75658099177411E-13,1.,1.66321791206623E-16)) ;
#38137 = DIRECTION('ref_axis',(1.,-1.75658099177411E-13,-4.54195640846217E-14)) ;
#38138 = DIRECTION('',(1.,-1.75658099177411E-13,-4.54195640846217E-14)) ;
#38139 = DIRECTION('center_axis',(1.75658099177411E-13,1.,1.66321791206623E-16)) ;
#38140 = DIRECTION('ref_axis',(-8.60220061280517E-14,1.66321791221733E-16,
-1.)) ;
#38141 = DIRECTION('',(-4.54195640846217E-14,1.66321791214602E-16,-1.)) ;
#38142 = DIRECTION('',(-1.,1.75658099177411E-13,4.54195640846217E-14)) ;
#38143 = DIRECTION('',(4.54195640846217E-14,-1.66321791214601E-16,1.)) ;
#38144 = DIRECTION('center_axis',(-1.75658099177411E-13,-1.,-1.66321791206623E-16)) ;
#38145 = DIRECTION('ref_axis',(0.99999997726804,-1.75658059720776E-13,-0.000213222701069828)) ;
#38146 = DIRECTION('center_axis',(-1.75658099177411E-13,-1.,-1.66321791206623E-16)) ;
#38147 = DIRECTION('ref_axis',(4.54195640846217E-14,-1.66321791214601E-16,
1.)) ;
#38148 = DIRECTION('',(1.,-1.75658099177411E-13,-4.54195640846217E-14)) ;
#38149 = DIRECTION('',(4.54195640846217E-14,-1.66321791214601E-16,1.)) ;
#38150 = DIRECTION('center_axis',(-1.75658099177411E-13,-1.,-1.66321791206623E-16)) ;
#38151 = DIRECTION('ref_axis',(1.,-1.75658099177411E-13,-4.54195640846217E-14)) ;
#38152 = DIRECTION('',(-4.54195640846217E-14,1.66321791214601E-16,-1.)) ;
#38153 = DIRECTION('',(-1.,1.75658099177411E-13,4.54195640846217E-14)) ;
#38154 = DIRECTION('',(4.54195640846217E-14,-1.66321791214601E-16,1.)) ;
#38155 = DIRECTION('center_axis',(-1.75658099177411E-13,-1.,-1.66321791206623E-16)) ;
#38156 = DIRECTION('ref_axis',(1.,-1.75658099177411E-13,-4.54195640846217E-14)) ;
#38157 = DIRECTION('',(4.54195640846217E-14,-1.66321791214601E-16,1.)) ;
#38158 = DIRECTION('',(1.,-1.75658099177411E-13,-4.54195640846217E-14)) ;
#38159 = DIRECTION('',(4.54195640846217E-14,-1.66321791214601E-16,1.)) ;
#38160 = DIRECTION('center_axis',(-1.75658099177411E-13,-1.,-1.66321791206623E-16)) ;
#38161 = DIRECTION('ref_axis',(1.,-1.75658099177411E-13,-4.54195640846217E-14)) ;
#38162 = DIRECTION('',(-4.54195640846217E-14,1.66321791214601E-16,-1.)) ;
#38163 = DIRECTION('',(1.,-1.75658099177411E-13,-4.54195640846217E-14)) ;
#38164 = DIRECTION('',(4.54195640846217E-14,-1.66321791214601E-16,1.)) ;
#38165 = DIRECTION('center_axis',(-1.75658099177411E-13,-1.,-1.66321791206623E-16)) ;
#38166 = DIRECTION('ref_axis',(1.,-1.75658099177411E-13,-4.54195640846217E-14)) ;
#38167 = DIRECTION('',(-4.54195640846217E-14,1.66321791214601E-16,-1.)) ;
#38168 = DIRECTION('',(1.,-1.75658099177411E-13,-4.54195640846217E-14)) ;
#38169 = DIRECTION('',(2.71407300257853E-29,1.66321791206623E-16,-1.)) ;
#38170 = DIRECTION('',(1.,-1.75658099177411E-13,0.)) ;
#38171 = DIRECTION('',(-4.54195640846217E-14,1.66321791214601E-16,-1.)) ;
#38172 = DIRECTION('',(-1.,1.75658099177411E-13,4.54195640846217E-14)) ;
#38173 = DIRECTION('center_axis',(1.75658099177411E-13,1.,1.66321791206623E-16)) ;
#38174 = DIRECTION('ref_axis',(0.707106781186522,-1.24326640365103E-13,0.707106781186573)) ;
#38175 = DIRECTION('',(1.,-1.75658099177411E-13,-3.1720657846433E-16)) ;
#38176 = DIRECTION('center_axis',(1.75658099177411E-13,1.,1.66321791206623E-16)) ;
#38177 = DIRECTION('ref_axis',(-0.707106781186548,1.24091425832265E-13,0.707106781186548)) ;
#38178 = DIRECTION('',(-2.92157696951376E-29,-1.66321791206623E-16,1.)) ;
#38179 = DIRECTION('center_axis',(1.75658099177411E-13,1.,1.66321791206623E-16)) ;
#38180 = DIRECTION('ref_axis',(-0.707106781186548,1.24326640365108E-13,-0.707106781186548)) ;
#38181 = DIRECTION('',(-1.,1.75658099177411E-13,6.34413156928661E-16)) ;
#38182 = DIRECTION('center_axis',(1.75658099177411E-13,1.,1.66321791206623E-16)) ;
#38183 = DIRECTION('ref_axis',(0.707106781186522,-1.24091425832261E-13,-0.707106781186573)) ;
#38184 = DIRECTION('',(2.92157696951376E-29,1.66321791206623E-16,-1.)) ;
#38185 = DIRECTION('center_axis',(-1.75658099177411E-13,-1.,-1.66321791206623E-16)) ;
#38186 = DIRECTION('ref_axis',(-1.,1.75658099177411E-13,4.54195640846217E-14)) ;
#38187 = DIRECTION('',(-1.,1.75658099177411E-13,4.54195640846217E-14)) ;
#38188 = DIRECTION('center_axis',(-1.75658099177411E-13,-1.,-1.66321791206623E-16)) ;
#38189 = DIRECTION('ref_axis',(-4.54195640846217E-14,1.66321791214601E-16,
-1.)) ;
#38190 = DIRECTION('',(-4.54195640846217E-14,1.66321791214602E-16,-1.)) ;
#38191 = DIRECTION('',(1.,-1.75658099177411E-13,-4.54195640846217E-14)) ;
#38192 = DIRECTION('',(4.54195640846217E-14,-1.66321791214601E-16,1.)) ;
#38193 = DIRECTION('',(1.,-1.75658099177411E-13,-4.54195640846217E-14)) ;
#38194 = DIRECTION('',(4.54195640846217E-14,-1.66321791214601E-16,1.)) ;
#38195 = DIRECTION('',(-1.,1.75658099177411E-13,4.54195640846217E-14)) ;
#38196 = DIRECTION('',(-4.54195640846217E-14,1.66321791214601E-16,-1.)) ;
#38197 = DIRECTION('',(1.,-1.75658099177411E-13,-4.54195640846217E-14)) ;
#38198 = DIRECTION('',(4.54195640846217E-14,-1.66321791214601E-16,1.)) ;
#38199 = DIRECTION('',(-1.,1.75658099177411E-13,4.54195640846217E-14)) ;
#38200 = DIRECTION('',(-4.54195640846217E-14,1.66321791214601E-16,-1.)) ;
#38201 = DIRECTION('',(1.,-1.75658099177411E-13,-4.54195640846217E-14)) ;
#38202 = DIRECTION('',(4.54195640846217E-14,-1.66321791214601E-16,1.)) ;
#38203 = DIRECTION('',(-1.,1.75658099177411E-13,4.54195640846217E-14)) ;
#38204 = DIRECTION('',(-4.54195640846217E-14,1.66321791214601E-16,-1.)) ;
#38205 = DIRECTION('',(1.,-1.75658099177411E-13,-4.54195640846217E-14)) ;
#38206 = DIRECTION('',(4.54195640846217E-14,-1.66321791214601E-16,1.)) ;
#38207 = DIRECTION('',(-1.,1.75658099177411E-13,4.54195640846217E-14)) ;
#38208 = DIRECTION('',(-4.54195640846217E-14,1.66321791214601E-16,-1.)) ;
#38209 = DIRECTION('center_axis',(1.75658099177411E-13,1.,1.66321791206623E-16)) ;
#38210 = DIRECTION('ref_axis',(0.00363593456997526,-8.05002047109562E-16,
0.999993389968055)) ;
#38211 = DIRECTION('center_axis',(1.75658099177411E-13,1.,1.66321791206623E-16)) ;
#38212 = DIRECTION('ref_axis',(0.00363593456997526,-8.05002047109562E-16,
0.999993389968055)) ;
#38213 = DIRECTION('center_axis',(-1.,1.63182045051861E-13,0.)) ;
#38214 = DIRECTION('ref_axis',(-1.63182045051861E-13,-1.,0.)) ;
#38215 = DIRECTION('center_axis',(-1.,1.63182045051861E-13,0.)) ;
#38216 = DIRECTION('ref_axis',(2.71407300258777E-29,1.66321791207189E-16,
-1.)) ;
#38217 = DIRECTION('',(1.63182045051861E-13,1.,1.66321791207189E-16)) ;
#38218 = DIRECTION('',(0.,0.,-1.)) ;
#38219 = DIRECTION('',(1.63182045051861E-13,1.,1.66321791207189E-16)) ;
#38220 = DIRECTION('',(1.63182045051861E-13,1.,0.)) ;
#38221 = DIRECTION('center_axis',(-1.,1.63182045051861E-13,0.)) ;
#38222 = DIRECTION('ref_axis',(-1.63182045051861E-13,-1.,0.)) ;
#38223 = DIRECTION('',(0.,0.,-1.)) ;
#38224 = DIRECTION('',(0.,0.,1.)) ;
#38225 = DIRECTION('',(1.63182045051861E-13,1.,0.)) ;
#38226 = DIRECTION('',(1.63182045051861E-13,1.,1.66321791207189E-16)) ;
#38227 = DIRECTION('',(2.71407300257853E-29,1.66321791206623E-16,-1.)) ;
#38228 = DIRECTION('',(1.63182045051861E-13,1.,0.)) ;
#38229 = DIRECTION('center_axis',(1.,-1.75658099177411E-13,-4.54195640846217E-14)) ;
#38230 = DIRECTION('ref_axis',(-4.54195640846217E-14,1.66321791214601E-16,
-1.)) ;
#38231 = DIRECTION('center_axis',(1.,-1.75658099177411E-13,-4.54195640846217E-14)) ;
#38232 = DIRECTION('ref_axis',(-4.54195640846217E-14,1.66321791214601E-16,
-1.)) ;
#38233 = DIRECTION('',(1.,-1.75658099177411E-13,-4.54195640846217E-14)) ;
#38234 = DIRECTION('center_axis',(1.,-1.75658099177411E-13,-4.54195640846217E-14)) ;
#38235 = DIRECTION('ref_axis',(-4.54195640846217E-14,1.66321791214601E-16,
-1.)) ;
#38236 = DIRECTION('',(1.,-1.75658099177411E-13,-4.54195640846217E-14)) ;
#38237 = DIRECTION('center_axis',(-1.,1.75658099177411E-13,4.54195640846217E-14)) ;
#38238 = DIRECTION('ref_axis',(1.75658099177411E-13,1.,1.66321791206623E-16)) ;
#38239 = DIRECTION('center_axis',(1.,-1.75658099177411E-13,-4.54195640846217E-14)) ;
#38240 = DIRECTION('ref_axis',(-1.75658099177411E-13,-1.,-1.66321791206623E-16)) ;
#38241 = DIRECTION('center_axis',(-1.,1.75658099177411E-13,4.54195640846217E-14)) ;
#38242 = DIRECTION('ref_axis',(-4.54195640846217E-14,1.66321791214601E-16,
-1.)) ;
#38243 = DIRECTION('',(1.,-1.75658099177411E-13,-4.54195640846217E-14)) ;
#38244 = DIRECTION('center_axis',(1.,-1.75658099177411E-13,-4.54195640846217E-14)) ;
#38245 = DIRECTION('ref_axis',(-1.56325514861458E-13,-0.707106781186535,-0.70710678118656)) ;
#38246 = DIRECTION('center_axis',(1.,-1.75658099177411E-13,-4.54195640846217E-14)) ;
#38247 = DIRECTION('ref_axis',(-1.56325514861458E-13,-0.707106781186535,-0.70710678118656)) ;
#38248 = DIRECTION('',(1.,-1.75658099177411E-13,-4.54195640846217E-14)) ;
#38249 = DIRECTION('center_axis',(1.,-1.63182045051861E-13,0.)) ;
#38250 = DIRECTION('ref_axis',(-1.15387130624058E-13,-0.707106781186535,-0.70710678118656)) ;
#38251 = DIRECTION('center_axis',(1.,-1.75658099177411E-13,-4.54195640846217E-14)) ;
#38252 = DIRECTION('ref_axis',(-4.54195640846217E-14,1.66321791214601E-16,
-1.)) ;
#38253 = DIRECTION('',(-1.75658099177411E-13,-1.,0.)) ;
#38254 = DIRECTION('center_axis',(-4.54195640846217E-14,1.66321791214601E-16,
-1.)) ;
#38255 = DIRECTION('ref_axis',(-1.75658099177411E-13,-1.,-1.66321791206623E-16)) ;
#38256 = DIRECTION('',(-1.,-4.97379915027563E-13,5.10702591322944E-14)) ;
#38257 = DIRECTION('',(-1.75658099177411E-13,-1.,-1.66321791206623E-16)) ;
#38258 = DIRECTION('',(1.,-1.75658099177411E-13,-4.54195640846217E-14)) ;
#38259 = DIRECTION('center_axis',(1.75658099177411E-13,1.,1.66321791206623E-16)) ;
#38260 = DIRECTION('ref_axis',(-4.54195640846217E-14,1.66321791214601E-16,
-1.)) ;
#38261 = DIRECTION('',(1.,-1.75658099177411E-13,0.)) ;
#38262 = DIRECTION('',(4.54195640846217E-14,-1.66321791214601E-16,1.)) ;
#38263 = DIRECTION('',(-1.,0.,1.46549439249113E-13)) ;
#38264 = DIRECTION('center_axis',(0.,0.,-1.)) ;
#38265 = DIRECTION('ref_axis',(1.63182045051861E-13,1.,0.)) ;
#38266 = DIRECTION('',(-1.,1.63182045051861E-13,0.)) ;
#38267 = DIRECTION('',(-1.75658099177411E-13,-1.,0.)) ;
#38268 = DIRECTION('center_axis',(1.63182045051861E-13,1.,0.)) ;
#38269 = DIRECTION('ref_axis',(0.,0.,1.)) ;
#38270 = DIRECTION('',(-1.,1.63182045051861E-13,4.54195640846217E-14)) ;
#38271 = DIRECTION('',(0.,0.,1.)) ;
#38272 = DIRECTION('',(4.54195640846217E-14,-7.41165735269262E-27,1.)) ;
#38273 = DIRECTION('center_axis',(-1.,1.63182045051861E-13,0.)) ;
#38274 = DIRECTION('ref_axis',(-1.63182045051861E-13,-1.,0.)) ;
#38275 = DIRECTION('',(1.63182045051861E-13,1.,1.66321791207189E-16)) ;
#38276 = DIRECTION('',(1.63182045051861E-13,1.,1.66321791207189E-16)) ;
#38277 = DIRECTION('center_axis',(-1.,1.63182045051861E-13,0.)) ;
#38278 = DIRECTION('ref_axis',(-1.63182045051861E-13,-1.,-1.66321791206623E-16)) ;
#38279 = DIRECTION('',(1.63182045051861E-13,1.,0.)) ;
#38280 = DIRECTION('center_axis',(0.,0.,-1.)) ;
#38281 = DIRECTION('ref_axis',(1.63182045051861E-13,1.,0.)) ;
#38282 = DIRECTION('center_axis',(0.,0.,-1.)) ;
#38283 = DIRECTION('ref_axis',(1.63182045051861E-13,1.,0.)) ;
#38284 = DIRECTION('',(-1.75658099177411E-13,-1.,0.)) ;
#38285 = DIRECTION('center_axis',(1.63182045051861E-13,1.,0.)) ;
#38286 = DIRECTION('ref_axis',(0.,0.,1.)) ;
#38287 = DIRECTION('',(1.,-1.63182045051861E-13,-4.54195640846217E-14)) ;
#38288 = DIRECTION('',(-4.54195640846217E-14,7.41165735269262E-27,-1.)) ;
#38289 = DIRECTION('',(1.,-1.63182045051861E-13,0.)) ;
#38290 = DIRECTION('center_axis',(0.,0.,-1.)) ;
#38291 = DIRECTION('ref_axis',(1.63182045051861E-13,1.,0.)) ;
#38292 = DIRECTION('',(-1.75658099177411E-13,-1.,0.)) ;
#38293 = DIRECTION('center_axis',(4.54195640846217E-14,-1.66321791214601E-16,
1.)) ;
#38294 = DIRECTION('ref_axis',(-0.707106781186698,-0.707106781186397,3.19988744963529E-14)) ;
#38295 = DIRECTION('center_axis',(-4.54195640846217E-14,1.66321791214601E-16,
-1.)) ;
#38296 = DIRECTION('ref_axis',(-0.707106781186698,-0.707106781186397,3.19988744963529E-14)) ;
#38297 = DIRECTION('',(4.54195640846217E-14,-1.66321791214601E-16,1.)) ;
#38298 = DIRECTION('center_axis',(4.54195640846217E-14,-1.66321791214601E-16,
1.)) ;
#38299 = DIRECTION('ref_axis',(-0.707106781186698,-0.707106781186397,3.19988744963529E-14)) ;
#38300 = DIRECTION('center_axis',(1.,-1.75658099177411E-13,-4.54195640846217E-14)) ;
#38301 = DIRECTION('ref_axis',(4.54195640846217E-14,-1.66321791214601E-16,
1.)) ;
#38302 = DIRECTION('',(1.75658099177411E-13,1.,1.66321791206623E-16)) ;
#38303 = DIRECTION('',(-4.54195640846217E-14,1.66321791214601E-16,-1.)) ;
#38304 = DIRECTION('',(1.75658099177411E-13,1.,1.66321791206623E-16)) ;
#38305 = DIRECTION('center_axis',(-4.54195640846217E-14,1.66321791214601E-16,
-1.)) ;
#38306 = DIRECTION('ref_axis',(0.707106781186409,-0.707106781186686,-3.22340890291936E-14)) ;
#38307 = DIRECTION('center_axis',(-3.99680288865058E-14,7.09974814698903E-27,
-1.)) ;
#38308 = DIRECTION('ref_axis',(1.,-1.42108547152021E-13,-3.99680288865058E-14)) ;
#38309 = DIRECTION('center_axis',(4.54195640846217E-14,-1.66321791214601E-16,
1.)) ;
#38310 = DIRECTION('ref_axis',(0.707106781186409,-0.707106781186686,-3.22340890291936E-14)) ;
#38311 = DIRECTION('',(-4.54195640846217E-14,1.66321791214601E-16,-1.)) ;
#38312 = DIRECTION('center_axis',(-1.75658099177411E-13,-1.,-1.66321791206623E-16)) ;
#38313 = DIRECTION('ref_axis',(0.,0.,-1.)) ;
#38314 = DIRECTION('center_axis',(1.,-1.77635683940023E-13,-3.55271579388434E-14)) ;
#38315 = DIRECTION('ref_axis',(3.55271579388434E-14,0.,1.)) ;
#38316 = DIRECTION('center_axis',(-1.75658099177411E-13,-1.,-1.66321791206623E-16)) ;
#38317 = DIRECTION('ref_axis',(-0.707106781186586,1.24326640365114E-13,-0.707106781186509)) ;
#38318 = DIRECTION('center_axis',(1.,-1.75658099177411E-13,-4.54195640846217E-14)) ;
#38319 = DIRECTION('ref_axis',(-9.20925513359094E-14,-0.707106781186529,0.707106781186566)) ;
#38320 = DIRECTION('center_axis',(1.,-2.13162820728042E-13,-3.55271156371924E-14)) ;
#38321 = DIRECTION('ref_axis',(3.55271156371924E-14,0.,1.)) ;
#38322 = DIRECTION('',(1.,-1.75658099177411E-13,-4.54195640846217E-14)) ;
#38323 = DIRECTION('center_axis',(-1.75658099177411E-13,-1.,-1.66321791206623E-16)) ;
#38324 = DIRECTION('ref_axis',(0.,0.,-1.)) ;
#38325 = DIRECTION('center_axis',(3.99680288865051E-14,-7.0997481469889E-27,
1.)) ;
#38326 = DIRECTION('ref_axis',(-1.,1.42108547152018E-13,3.99680288865051E-14)) ;
#38327 = DIRECTION('center_axis',(-1.75658099177411E-13,-1.,-1.66321791206623E-16)) ;
#38328 = DIRECTION('ref_axis',(0.707106781186528,-1.24091425832262E-13,-0.707106781186567)) ;
#38329 = DIRECTION('center_axis',(4.54195640846217E-14,-1.66321791214601E-16,
1.)) ;
#38330 = DIRECTION('ref_axis',(-0.707106781186698,-0.707106781186397,3.19988744963529E-14)) ;
#38331 = DIRECTION('center_axis',(4.54195640846217E-14,-1.66321791214601E-16,
1.)) ;
#38332 = DIRECTION('ref_axis',(-0.707106781186698,-0.707106781186397,3.19988744963529E-14)) ;
#38333 = DIRECTION('',(4.54195640846217E-14,-1.66321791214601E-16,1.)) ;
#38334 = DIRECTION('center_axis',(1.,-1.75658099177411E-13,-4.54195640846217E-14)) ;
#38335 = DIRECTION('ref_axis',(4.54195640846217E-14,-1.66321791214601E-16,
1.)) ;
#38336 = DIRECTION('',(-1.75658099177411E-13,-1.,-1.66321791206623E-16)) ;
#38337 = DIRECTION('',(-4.54195640846217E-14,1.66321791214601E-16,-1.)) ;
#38338 = DIRECTION('',(-1.75658099177411E-13,-1.,-1.66321791206623E-16)) ;
#38339 = DIRECTION('center_axis',(1.75658099177411E-13,1.,1.66321791206623E-16)) ;
#38340 = DIRECTION('ref_axis',(1.,-1.75658099177411E-13,-4.54195640846217E-14)) ;
#38341 = DIRECTION('',(-2.79089251708989E-13,1.,1.66321791227277E-16)) ;
#38342 = DIRECTION('center_axis',(1.75658099177411E-13,1.,1.66321791206623E-16)) ;
#38343 = DIRECTION('ref_axis',(0.258819045102331,-4.53030069799869E-14,-0.965925826289119)) ;
#38344 = DIRECTION('center_axis',(4.54195640846217E-14,-1.66321791214601E-16,
1.)) ;
#38345 = DIRECTION('ref_axis',(1.75658099177411E-13,1.,1.66321791206623E-16)) ;
#38346 = DIRECTION('',(-1.75658099177411E-13,-1.,-1.66321791206623E-16)) ;
#38347 = DIRECTION('',(-1.,1.75658099177411E-13,4.54195640846217E-14)) ;
#38348 = DIRECTION('center_axis',(-1.75658099177411E-13,-1.,-1.66321791206623E-16)) ;
#38349 = DIRECTION('ref_axis',(-1.,1.75658099177411E-13,4.54195640846217E-14)) ;
#38350 = DIRECTION('',(1.87026782949573E-13,1.,4.56410568798561E-14)) ;
#38351 = DIRECTION('center_axis',(1.75658099177411E-13,1.,1.66321791206623E-16)) ;
#38352 = DIRECTION('ref_axis',(-0.258819045102564,4.56243160072301E-14,-0.965925826289057)) ;
#38353 = DIRECTION('center_axis',(-1.,1.75658099177411E-13,4.54195640846217E-14)) ;
#38354 = DIRECTION('ref_axis',(-4.54195640846217E-14,1.66321791214601E-16,
-1.)) ;
#38355 = DIRECTION('',(1.75658099177411E-13,1.,1.66321791206623E-16)) ;
#38356 = DIRECTION('',(4.54195640846217E-14,-1.66321791214601E-16,1.)) ;
#38357 = DIRECTION('center_axis',(-4.54195640846217E-14,1.66321791214601E-16,
-1.)) ;
#38358 = DIRECTION('ref_axis',(-0.707106781186397,0.707106781186698,3.22340890291931E-14)) ;
#38359 = DIRECTION('center_axis',(-4.44089209850056E-14,7.88860905220989E-27,
-1.)) ;
#38360 = DIRECTION('ref_axis',(-1.,1.42108547152018E-13,4.44089209850056E-14)) ;
#38361 = DIRECTION('center_axis',(4.54195640846217E-14,-1.66321791214601E-16,
1.)) ;
#38362 = DIRECTION('ref_axis',(-0.707106781186397,0.707106781186698,3.22340890291931E-14)) ;
#38363 = DIRECTION('',(-4.54195640846217E-14,1.66321791214601E-16,-1.)) ;
#38364 = DIRECTION('center_axis',(1.75658099177411E-13,1.,1.66321791206623E-16)) ;
#38365 = DIRECTION('ref_axis',(0.,0.,1.)) ;
#38366 = DIRECTION('center_axis',(-1.,1.77635683940022E-13,3.5527157938743E-14)) ;
#38367 = DIRECTION('ref_axis',(3.5527157938743E-14,0.,1.)) ;
#38368 = DIRECTION('center_axis',(1.75658099177411E-13,1.,1.66321791206623E-16)) ;
#38369 = DIRECTION('ref_axis',(0.70710678118651,-1.24091425832259E-13,-0.707106781186585)) ;
#38370 = DIRECTION('center_axis',(1.,-1.75658099177411E-13,-4.54195640846217E-14)) ;
#38371 = DIRECTION('ref_axis',(1.56325514861457E-13,0.707106781186529,0.707106781186566)) ;
#38372 = DIRECTION('center_axis',(-1.,1.77635683940023E-13,5.32906734559391E-14)) ;
#38373 = DIRECTION('ref_axis',(5.32906734559391E-14,0.,1.)) ;
#38374 = DIRECTION('',(-1.,1.75658099177411E-13,4.54195640846217E-14)) ;
#38375 = DIRECTION('center_axis',(1.75658099177411E-13,1.,1.66321791206623E-16)) ;
#38376 = DIRECTION('ref_axis',(0.,0.,1.)) ;
#38377 = DIRECTION('center_axis',(4.88498130835079E-14,-8.67746995743119E-27,
1.)) ;
#38378 = DIRECTION('ref_axis',(1.,-1.42108547152023E-13,-4.88498130835079E-14)) ;
#38379 = DIRECTION('center_axis',(1.75658099177411E-13,1.,1.66321791206623E-16)) ;
#38380 = DIRECTION('ref_axis',(-0.707106781186573,1.24326640365112E-13,-0.707106781186522)) ;
#38381 = DIRECTION('center_axis',(4.54195640846217E-14,-1.66321791214601E-16,
1.)) ;
#38382 = DIRECTION('ref_axis',(0.707106781186636,0.70710678118646,-3.199887449635E-14)) ;
#38383 = DIRECTION('center_axis',(4.54195640846217E-14,-1.66321791214601E-16,
1.)) ;
#38384 = DIRECTION('ref_axis',(0.707106781186636,0.70710678118646,-3.199887449635E-14)) ;
#38385 = DIRECTION('',(4.54195640846217E-14,-1.66321791214601E-16,1.)) ;
#38386 = DIRECTION('center_axis',(-1.,1.75658099177411E-13,4.54195640846217E-14)) ;
#38387 = DIRECTION('ref_axis',(4.54195640846217E-14,-1.66321791214601E-16,
1.)) ;
#38388 = DIRECTION('',(1.75658099177411E-13,1.,1.66321791206623E-16)) ;
#38389 = DIRECTION('',(-4.54195640846217E-14,1.66321791214601E-16,-1.)) ;
#38390 = DIRECTION('',(1.75658099177411E-13,1.,1.66321791206623E-16)) ;
#38391 = DIRECTION('center_axis',(-1.75658099177411E-13,-1.,-1.66321791206623E-16)) ;
#38392 = DIRECTION('ref_axis',(-1.,1.75658099177411E-13,4.54195640846217E-14)) ;
#38393 = DIRECTION('',(-1.75658099177411E-13,-1.,-1.66321791206623E-16)) ;
#38394 = DIRECTION('center_axis',(-1.75658099177411E-13,-1.,-1.66321791206623E-16)) ;
#38395 = DIRECTION('ref_axis',(-0.258819045102557,4.56243160072289E-14,-0.965925826289059)) ;
#38396 = DIRECTION('center_axis',(4.54195640846217E-14,-1.66321791214601E-16,
1.)) ;
#38397 = DIRECTION('ref_axis',(1.75658099177411E-13,1.,1.66321791206623E-16)) ;
#38398 = DIRECTION('',(1.75658099177411E-13,1.,1.66321791206623E-16)) ;
#38399 = DIRECTION('',(1.,-1.75658099177411E-13,-4.54195640846217E-14)) ;
#38400 = DIRECTION('center_axis',(1.75658099177411E-13,1.,1.66321791206623E-16)) ;
#38401 = DIRECTION('ref_axis',(1.,-1.75658099177411E-13,-4.54195640846217E-14)) ;
#38402 = DIRECTION('',(-1.75658099177411E-13,-1.,-1.66321791206623E-16)) ;
#38403 = DIRECTION('center_axis',(-1.75658099177411E-13,-1.,-1.66321791206623E-16)) ;
#38404 = DIRECTION('ref_axis',(0.258819045102475,-4.53030069800122E-14,-0.965925826289081)) ;
#38405 = DIRECTION('center_axis',(1.,-1.75658099177411E-13,-4.54195640846217E-14)) ;
#38406 = DIRECTION('ref_axis',(-4.54195640846217E-14,1.66321791214601E-16,
-1.)) ;
#38407 = DIRECTION('',(-1.75658099177411E-13,-1.,-1.66321791206623E-16)) ;
#38408 = DIRECTION('',(4.54195640846217E-14,-1.66321791214601E-16,1.)) ;
#38409 = DIRECTION('center_axis',(-0.5,0.866025403784438,7.35649810170484E-14)) ;
#38410 = DIRECTION('ref_axis',(-0.866025403784438,-0.5,-4.2407782439997E-14)) ;
#38411 = DIRECTION('',(-0.866025403784438,-0.5,3.92513354304904E-14)) ;
#38412 = DIRECTION('',(-5.62735973232286E-17,8.49130336096823E-14,-1.)) ;
#38413 = DIRECTION('',(0.866025403784438,0.5,-3.92513354304904E-14)) ;
#38414 = DIRECTION('',(-5.62735973232286E-17,8.49130336096823E-14,-1.)) ;
#38415 = DIRECTION('center_axis',(0.5,0.866025403784439,7.35087074197251E-14)) ;
#38416 = DIRECTION('ref_axis',(-0.866025403784439,0.5,4.25052511696854E-14)) ;
#38417 = DIRECTION('',(-0.866025403784438,0.5,3.9417657221705E-14)) ;
#38418 = DIRECTION('',(0.866025403784438,-0.5,-3.9417657221705E-14)) ;
#38419 = DIRECTION('',(-5.62735973232286E-17,8.49130336096823E-14,-1.)) ;
#38420 = DIRECTION('center_axis',(1.,8.10629031994436E-17,-5.62735973232217E-17)) ;
#38421 = DIRECTION('ref_axis',(-8.10629031994388E-17,1.,8.49130336096823E-14)) ;
#38422 = DIRECTION('',(-8.10629031994436E-17,1.,1.66321791214605E-16)) ;
#38423 = DIRECTION('',(8.10629031994341E-17,-1.,-1.66321791214605E-16)) ;
#38424 = DIRECTION('',(-5.62735973232286E-17,8.49130336096823E-14,-1.)) ;
#38425 = DIRECTION('center_axis',(0.5,-0.866025403784439,-7.35649810170484E-14)) ;
#38426 = DIRECTION('ref_axis',(0.866025403784439,0.5,4.24077824399969E-14)) ;
#38427 = DIRECTION('',(0.866025403784439,0.5,-3.92513354304904E-14)) ;
#38428 = DIRECTION('',(-0.866025403784439,-0.5,3.92513354304904E-14)) ;
#38429 = DIRECTION('',(-5.62735973232286E-17,8.49130336096823E-14,-1.)) ;
#38430 = DIRECTION('center_axis',(-1.,5.55111512312073E-17,5.62735973232333E-17)) ;
#38431 = DIRECTION('ref_axis',(-5.55111512312121E-17,-1.,-8.49130336096823E-14)) ;
#38432 = DIRECTION('',(-5.55111512312074E-17,-1.,-1.66321791214598E-16)) ;
#38433 = DIRECTION('',(-5.62735973232286E-17,8.49130336096823E-14,-1.)) ;
#38434 = DIRECTION('',(5.55111512312168E-17,1.,1.66321791214598E-16)) ;
#38435 = DIRECTION('center_axis',(-0.5,-0.866025403784439,-7.35087074197251E-14)) ;
#38436 = DIRECTION('ref_axis',(0.866025403784439,-0.5,-4.25052511696854E-14)) ;
#38437 = DIRECTION('',(0.866025403784439,-0.5,-3.9417657221705E-14)) ;
#38438 = DIRECTION('',(-0.866025403784439,0.5,3.9417657221705E-14)) ;
#38439 = DIRECTION('center_axis',(-0.5,0.866025403784438,7.35750690713851E-14)) ;
#38440 = DIRECTION('ref_axis',(-0.866025403784438,-0.5,-4.24144871777968E-14)) ;
#38441 = DIRECTION('',(-0.866025403784438,-0.5,3.92513354304904E-14)) ;
#38442 = DIRECTION('',(-5.55111512312515E-17,8.49251224899127E-14,-1.)) ;
#38443 = DIRECTION('',(0.866025403784438,0.5,-3.92513354304904E-14)) ;
#38444 = DIRECTION('',(-5.55111512312515E-17,8.49251224899126E-14,-1.)) ;
#38445 = DIRECTION('center_axis',(0.5,0.866025403784439,7.35195579201539E-14)) ;
#38446 = DIRECTION('ref_axis',(-0.866025403784439,0.5,4.25106353121159E-14)) ;
#38447 = DIRECTION('',(-0.866025403784438,0.5,3.9417657221705E-14)) ;
#38448 = DIRECTION('',(0.866025403784438,-0.5,-3.9417657221705E-14)) ;
#38449 = DIRECTION('',(-5.55111512312515E-17,8.49251224899127E-14,-1.)) ;
#38450 = DIRECTION('center_axis',(1.,1.36574054430676E-16,-5.55111512312399E-17)) ;
#38451 = DIRECTION('ref_axis',(-1.36574054430671E-16,1.,8.49251224899126E-14)) ;
#38452 = DIRECTION('',(-1.36574054430676E-16,1.,1.66321791214607E-16)) ;
#38453 = DIRECTION('',(1.36574054430667E-16,-1.,-1.66321791214607E-16)) ;
#38454 = DIRECTION('',(-5.55111512312515E-17,8.49251224899127E-14,-1.)) ;
#38455 = DIRECTION('center_axis',(0.5,-0.866025403784439,-7.35750690713851E-14)) ;
#38456 = DIRECTION('ref_axis',(0.866025403784439,0.5,4.24144871777967E-14)) ;
#38457 = DIRECTION('',(0.866025403784439,0.5,-3.92513354304904E-14)) ;
#38458 = DIRECTION('',(-0.866025403784439,-0.5,3.92513354304904E-14)) ;
#38459 = DIRECTION('',(-5.55111512312515E-17,8.49251224899126E-14,-1.)) ;
#38460 = DIRECTION('center_axis',(-1.,-2.52435489670719E-29,5.55111512312515E-17)) ;
#38461 = DIRECTION('ref_axis',(2.05292576492018E-29,-1.,-8.49251224899126E-14)) ;
#38462 = DIRECTION('',(2.52343162529668E-29,-1.,-1.66321791214601E-16)) ;
#38463 = DIRECTION('',(-5.55111512312515E-17,8.49251224899127E-14,-1.)) ;
#38464 = DIRECTION('',(-1.58057336172267E-29,1.,1.66321791214601E-16)) ;
#38465 = DIRECTION('center_axis',(-0.5,-0.866025403784439,-7.35195579201539E-14)) ;
#38466 = DIRECTION('ref_axis',(0.866025403784439,-0.5,-4.25106353121159E-14)) ;
#38467 = DIRECTION('',(0.866025403784439,-0.5,-3.9417657221705E-14)) ;
#38468 = DIRECTION('',(-0.866025403784439,0.5,3.9417657221705E-14)) ;
#38469 = DIRECTION('center_axis',(1.,-1.75658099177411E-13,-4.54195640846217E-14)) ;
#38470 = DIRECTION('ref_axis',(-4.54195640846217E-14,1.66321791214601E-16,
-1.)) ;
#38471 = DIRECTION('center_axis',(1.,-1.75658099177411E-13,-4.54195640846217E-14)) ;
#38472 = DIRECTION('ref_axis',(-4.54195640846217E-14,1.66321791214601E-16,
-1.)) ;
#38473 = DIRECTION('center_axis',(-1.,1.75658099177411E-13,4.54195640846217E-14)) ;
#38474 = DIRECTION('ref_axis',(9.20925513359107E-14,0.707106781186535,-0.70710678118656)) ;
#38475 = DIRECTION('center_axis',(1.,-1.75658099177411E-13,-4.54195640846217E-14)) ;
#38476 = DIRECTION('ref_axis',(9.20925513359107E-14,0.707106781186535,-0.70710678118656)) ;
#38477 = DIRECTION('center_axis',(-1.,1.75658099177411E-13,4.54195640846217E-14)) ;
#38478 = DIRECTION('ref_axis',(9.20925513359107E-14,0.707106781186535,-0.70710678118656)) ;
#38479 = DIRECTION('',(1.,-1.75658099177411E-13,-4.54195640846217E-14)) ;
#38480 = DIRECTION('center_axis',(1.,-1.75658099177411E-13,-4.54195640846217E-14)) ;
#38481 = DIRECTION('ref_axis',(-1.56325514861458E-13,-0.707106781186535,-0.70710678118656)) ;
#38482 = DIRECTION('center_axis',(-1.,1.75658099177411E-13,4.54195640846217E-14)) ;
#38483 = DIRECTION('ref_axis',(-1.56325514861458E-13,-0.707106781186535,-0.70710678118656)) ;
#38484 = DIRECTION('center_axis',(1.,-1.75658099177411E-13,-4.54195640846217E-14)) ;
#38485 = DIRECTION('ref_axis',(-1.56325514861458E-13,-0.707106781186535,-0.70710678118656)) ;
#38486 = DIRECTION('',(-1.,1.75658099177411E-13,4.54195640846217E-14)) ;
#38487 = DIRECTION('center_axis',(1.,-1.75658099177411E-13,-4.54195640846217E-14)) ;
#38488 = DIRECTION('ref_axis',(-1.56325514861458E-13,-0.707106781186535,-0.70710678118656)) ;
#38489 = DIRECTION('',(-1.,1.75658099177411E-13,4.54195640846217E-14)) ;
#38490 = DIRECTION('center_axis',(-1.,1.75658099177411E-13,4.54195640846217E-14)) ;
#38491 = DIRECTION('ref_axis',(-1.56325514861458E-13,-0.707106781186535,-0.70710678118656)) ;
#38492 = DIRECTION('center_axis',(-1.,1.75658099177411E-13,4.54195640846217E-14)) ;
#38493 = DIRECTION('ref_axis',(9.20925513359107E-14,0.707106781186535,-0.70710678118656)) ;
#38494 = DIRECTION('center_axis',(1.,-1.75658099177411E-13,-4.54195640846217E-14)) ;
#38495 = DIRECTION('ref_axis',(9.20925513359107E-14,0.707106781186535,-0.70710678118656)) ;
#38496 = DIRECTION('center_axis',(-1.,1.75658099177411E-13,4.54195640846217E-14)) ;
#38497 = DIRECTION('ref_axis',(9.20925513359107E-14,0.707106781186535,-0.70710678118656)) ;
#38498 = DIRECTION('',(1.,-1.75658099177411E-13,-4.54195640846217E-14)) ;
#38499 = DIRECTION('center_axis',(1.,-1.75658099177411E-13,-4.54195640846217E-14)) ;
#38500 = DIRECTION('ref_axis',(9.20925513359107E-14,0.707106781186535,-0.70710678118656)) ;
#38501 = DIRECTION('center_axis',(-1.,1.75658099177411E-13,4.54195640846217E-14)) ;
#38502 = DIRECTION('ref_axis',(9.20925513359107E-14,0.707106781186535,-0.70710678118656)) ;
#38503 = DIRECTION('',(1.,-1.75658099177411E-13,-4.54195640846217E-14)) ;
#38504 = DIRECTION('center_axis',(1.,-1.75658099177411E-13,-4.54195640846217E-14)) ;
#38505 = DIRECTION('ref_axis',(9.20925513359107E-14,0.707106781186535,-0.70710678118656)) ;
#38506 = DIRECTION('center_axis',(-1.,1.75658099177411E-13,4.54195640846217E-14)) ;
#38507 = DIRECTION('ref_axis',(4.54195640846217E-14,-1.66321791214601E-16,
1.)) ;
#38508 = DIRECTION('',(1.75658099177411E-13,1.,1.66321791206623E-16)) ;
#38509 = DIRECTION('',(4.54195640846217E-14,-1.66321791214601E-16,1.)) ;
#38510 = DIRECTION('',(-1.75658099177411E-13,-1.,-1.66321791206623E-16)) ;
#38511 = DIRECTION('',(1.75658099177411E-13,1.,1.66321791206623E-16)) ;
#38512 = DIRECTION('center_axis',(-1.61486985400024E-13,-1.,0.)) ;
#38513 = DIRECTION('ref_axis',(0.99999997726804,-1.61486981729108E-13,-0.000213222701069828)) ;
#38514 = DIRECTION('center_axis',(1.75658099177411E-13,1.,1.66321791206623E-16)) ;
#38515 = DIRECTION('ref_axis',(0.99999997726804,-1.75658059720776E-13,-0.000213222701069828)) ;
#38516 = DIRECTION('',(-0.707106765112755,-0.707106781186416,0.000150771217829304)) ;
#38517 = DIRECTION('center_axis',(-1.75658099177411E-13,-1.,-1.66321791206623E-16)) ;
#38518 = DIRECTION('ref_axis',(0.99999997726804,-1.75658059720776E-13,-0.000213222701069828)) ;
#38519 = DIRECTION('',(-1.75658099177411E-13,-1.,-1.66321791206623E-16)) ;
#38520 = DIRECTION('center_axis',(1.61486985400024E-13,1.,0.)) ;
#38521 = DIRECTION('ref_axis',(0.00363593456997526,-5.87156112817037E-16,
0.999993389968055)) ;
#38522 = DIRECTION('center_axis',(-1.75658099177411E-13,-1.,-1.66321791206623E-16)) ;
#38523 = DIRECTION('ref_axis',(0.00363593456997526,-8.05002047109562E-16,
0.999993389968055)) ;
#38524 = DIRECTION('',(-0.002570993990266,0.707106781186547,-0.707102107188137)) ;
#38525 = DIRECTION('center_axis',(-1.75658099177411E-13,-1.,-1.66321791206623E-16)) ;
#38526 = DIRECTION('ref_axis',(0.00363593456997526,-8.05002047109562E-16,
0.999993389968055)) ;
#38527 = DIRECTION('',(-1.75658099177411E-13,-1.,-1.66321791206623E-16)) ;
#38528 = DIRECTION('center_axis',(-1.75617096622526E-13,-1.,0.)) ;
#38529 = DIRECTION('ref_axis',(1.,-1.75617096622526E-13,-4.54195640846217E-14)) ;
#38530 = DIRECTION('center_axis',(1.75658099177411E-13,1.,1.66321791206623E-16)) ;
#38531 = DIRECTION('ref_axis',(1.,-1.75658099177411E-13,-4.54195640846217E-14)) ;
#38532 = DIRECTION('',(-0.707106781186674,-0.707106781186421,3.20298861571495E-14)) ;
#38533 = DIRECTION('center_axis',(-1.75658099177411E-13,-1.,-1.66321791206623E-16)) ;
#38534 = DIRECTION('ref_axis',(1.,-1.75658099177411E-13,-4.54195640846217E-14)) ;
#38535 = DIRECTION('',(-1.75658099177411E-13,-1.,-1.66321791206623E-16)) ;
#38536 = DIRECTION('center_axis',(-4.54195640846217E-14,1.66321791214601E-16,
-1.)) ;
#38537 = DIRECTION('ref_axis',(-1.,5.55236256206829E-46,4.54195640846217E-14)) ;
#38538 = DIRECTION('',(1.,-1.75658099177411E-13,-4.54195640846217E-14)) ;
#38539 = DIRECTION('center_axis',(-4.54195640846217E-14,1.66321791214601E-16,
-1.)) ;
#38540 = DIRECTION('ref_axis',(0.923076923076982,0.384615384615244,-4.18617815430325E-14)) ;
#38541 = DIRECTION('center_axis',(-4.54195640846217E-14,1.66321791214601E-16,
-1.)) ;
#38542 = DIRECTION('ref_axis',(-1.,5.55236256206829E-46,4.54195640846217E-14)) ;
#38543 = DIRECTION('',(1.,-1.75658099177411E-13,-4.54195640846217E-14)) ;
#38544 = DIRECTION('center_axis',(4.54195640846217E-14,-1.66321791214601E-16,
1.)) ;
#38545 = DIRECTION('ref_axis',(-0.923076923076847,0.384615384615568,4.19897213824222E-14)) ;
#38546 = DIRECTION('center_axis',(1.75658099177411E-13,1.,1.66321791206623E-16)) ;
#38547 = DIRECTION('ref_axis',(-1.,1.75658099177411E-13,4.54195640846217E-14)) ;
#38548 = DIRECTION('center_axis',(-1.75658099177411E-13,-1.,-1.66321791206623E-16)) ;
#38549 = DIRECTION('ref_axis',(-1.,1.75658099177411E-13,4.54195640846217E-14)) ;
#38550 = DIRECTION('',(1.75658099177411E-13,1.,1.66321791206623E-16)) ;
#38551 = DIRECTION('center_axis',(1.75658099177411E-13,1.,1.66321791206623E-16)) ;
#38552 = DIRECTION('ref_axis',(-1.,1.75658099173691E-13,2.23674678734541E-8)) ;
#38553 = DIRECTION('center_axis',(1.75658099177411E-13,1.,1.66321791206623E-16)) ;
#38554 = DIRECTION('ref_axis',(-1.,1.75658099173691E-13,2.23674678734541E-8)) ;
#38555 = DIRECTION('center_axis',(1.75658099177411E-13,1.,1.66321791206623E-16)) ;
#38556 = DIRECTION('ref_axis',(-4.54195640846217E-14,1.66321791214601E-16,
-1.)) ;
#38557 = DIRECTION('',(1.56412110467083E-13,0.707106781186548,0.707106781186547)) ;
#38558 = DIRECTION('center_axis',(1.75658099177411E-13,1.,1.66321791206623E-16)) ;
#38559 = DIRECTION('ref_axis',(1.,-1.75658099177411E-13,-4.54195640846217E-14)) ;
#38560 = DIRECTION('center_axis',(4.54195640846217E-14,-1.66321791214601E-16,
1.)) ;
#38561 = DIRECTION('ref_axis',(-1.,1.75658099177411E-13,4.54195640846217E-14)) ;
#38562 = DIRECTION('center_axis',(-4.54195640846217E-14,1.66321791214601E-16,
-1.)) ;
#38563 = DIRECTION('ref_axis',(1.,-1.75658099177411E-13,-4.54195640846217E-14)) ;
#38564 = DIRECTION('',(-4.54195640846217E-14,1.66321791214601E-16,-1.)) ;
#38565 = DIRECTION('center_axis',(4.54195640846217E-14,-1.66321791214601E-16,
1.)) ;
#38566 = DIRECTION('ref_axis',(-1.,1.75658099177411E-13,4.54195640846217E-14)) ;
#38567 = DIRECTION('',(4.54195640846217E-14,-1.66321791214601E-16,1.)) ;
#38568 = DIRECTION('center_axis',(4.54195640846217E-14,-1.66321791214601E-16,
1.)) ;
#38569 = DIRECTION('ref_axis',(-1.,1.75658099177411E-13,4.54195640846217E-14)) ;
#38570 = DIRECTION('center_axis',(-4.54195640846217E-14,1.66321791214601E-16,
-1.)) ;
#38571 = DIRECTION('ref_axis',(1.,-1.75658099177411E-13,-4.54195640846217E-14)) ;
#38572 = DIRECTION('',(-4.54195640846217E-14,1.66321791214601E-16,-1.)) ;
#38573 = DIRECTION('center_axis',(4.54195640846217E-14,-1.66321791214601E-16,
1.)) ;
#38574 = DIRECTION('ref_axis',(-1.,1.75658099177411E-13,4.54195640846217E-14)) ;
#38575 = DIRECTION('',(4.54195640846217E-14,-1.66321791214601E-16,1.)) ;
#38576 = DIRECTION('center_axis',(-4.54195640846217E-14,1.66321791214601E-16,
-1.)) ;
#38577 = DIRECTION('ref_axis',(-1.,1.75658099177411E-13,4.54195640846217E-14)) ;
#38578 = DIRECTION('center_axis',(4.54195640846217E-14,-1.66321791214601E-16,
1.)) ;
#38579 = DIRECTION('ref_axis',(1.,-1.75658099177411E-13,-4.54195640846217E-14)) ;
#38580 = DIRECTION('',(4.54195640846217E-14,-1.66321791214601E-16,1.)) ;
#38581 = DIRECTION('center_axis',(-4.54195640846217E-14,1.66321791214601E-16,
-1.)) ;
#38582 = DIRECTION('ref_axis',(-1.,1.75658099177411E-13,4.54195640846217E-14)) ;
#38583 = DIRECTION('',(-4.54195640846217E-14,1.66321791214601E-16,-1.)) ;
#38584 = DIRECTION('center_axis',(-4.54195640846217E-14,1.66321791214601E-16,
-1.)) ;
#38585 = DIRECTION('ref_axis',(-1.,1.75658099177411E-13,4.54195640846217E-14)) ;
#38586 = DIRECTION('center_axis',(4.54195640846217E-14,-1.66321791214601E-16,
1.)) ;
#38587 = DIRECTION('ref_axis',(1.,-1.75658099177411E-13,-4.54195640846217E-14)) ;
#38588 = DIRECTION('',(4.54195640846217E-14,-1.66321791214601E-16,1.)) ;
#38589 = DIRECTION('center_axis',(-4.54195640846217E-14,1.66321791214601E-16,
-1.)) ;
#38590 = DIRECTION('ref_axis',(-1.,1.75658099177411E-13,4.54195640846217E-14)) ;
#38591 = DIRECTION('',(-4.54195640846217E-14,1.66321791214601E-16,-1.)) ;
#38592 = DIRECTION('center_axis',(4.54195640846217E-14,-1.66321791214601E-16,
1.)) ;
#38593 = DIRECTION('ref_axis',(-1.75658099177411E-13,-1.,-1.66321791206623E-16)) ;
#38594 = DIRECTION('center_axis',(-4.54195640846217E-14,1.66321791214601E-16,
-1.)) ;
#38595 = DIRECTION('ref_axis',(1.,-1.75658099177411E-13,-4.54195640846217E-14)) ;
#38596 = DIRECTION('center_axis',(-4.54195640846217E-14,1.66321791214601E-16,
-1.)) ;
#38597 = DIRECTION('ref_axis',(1.,-1.75658099177411E-13,-4.54195640846217E-14)) ;
#38598 = DIRECTION('',(-4.54195640846217E-14,1.66321791214601E-16,-1.)) ;
#38599 = DIRECTION('center_axis',(4.54195640846217E-14,-1.66321791214601E-16,
1.)) ;
#38600 = DIRECTION('ref_axis',(-1.75658099177411E-13,-1.,-1.66321791206623E-16)) ;
#38601 = DIRECTION('center_axis',(-4.54195640846217E-14,1.66321791214601E-16,
-1.)) ;
#38602 = DIRECTION('ref_axis',(1.,-1.75658099177411E-13,-4.54195640846217E-14)) ;
#38603 = DIRECTION('',(4.54195640846217E-14,-1.66321791214601E-16,1.)) ;
#38604 = DIRECTION('center_axis',(-4.54195640846217E-14,1.66321791214601E-16,
-1.)) ;
#38605 = DIRECTION('ref_axis',(1.,-1.75658099177411E-13,-4.54195640846217E-14)) ;
#38606 = DIRECTION('',(-4.54195640846217E-14,1.66321791214601E-16,-1.)) ;
#38607 = DIRECTION('center_axis',(1.75658099177411E-13,1.,1.66321791206623E-16)) ;
#38608 = DIRECTION('ref_axis',(-0.268757454585954,4.0124766254688E-14,-0.963207885455927)) ;
#38609 = DIRECTION('center_axis',(-4.54195640846217E-14,1.66321791214601E-16,
-1.)) ;
#38610 = DIRECTION('ref_axis',(-1.,1.75658099177411E-13,4.54195640846217E-14)) ;
#38611 = DIRECTION('center_axis',(1.,-1.75658099177411E-13,-4.54195640846217E-14)) ;
#38612 = DIRECTION('ref_axis',(1.75658099177411E-13,1.,1.66321791206622E-16)) ;
#38613 = DIRECTION('center_axis',(1.75658099177411E-13,1.,1.66321791206623E-16)) ;
#38614 = DIRECTION('ref_axis',(1.,-1.75658099177198E-13,-1.28004463729308E-9)) ;
#38615 = DIRECTION('center_axis',(4.54195640846217E-14,-1.66321791214601E-16,
1.)) ;
#38616 = DIRECTION('ref_axis',(1.75658099177411E-13,1.,1.66321791206623E-16)) ;
#38617 = DIRECTION('center_axis',(4.54195640846217E-14,-1.66321791214601E-16,
1.)) ;
#38618 = DIRECTION('ref_axis',(1.75658099177411E-13,1.,1.66321791206623E-16)) ;
#38619 = DIRECTION('',(4.54195640846217E-14,-1.66321791214601E-16,1.)) ;
#38620 = DIRECTION('center_axis',(-1.75658099177411E-13,-1.,-1.66321791206623E-16)) ;
#38621 = DIRECTION('ref_axis',(1.,-1.75658099177411E-13,-4.54195640846217E-14)) ;
#38622 = DIRECTION('',(1.75658099177411E-13,1.,1.66321791206623E-16)) ;
#38623 = DIRECTION('',(-1.75658099177411E-13,-1.,-1.66321791206623E-16)) ;
#38624 = DIRECTION('center_axis',(1.75658099177411E-13,1.,1.66321791206623E-16)) ;
#38625 = DIRECTION('ref_axis',(-1.,1.75658099177411E-13,4.54195640846217E-14)) ;
#38626 = DIRECTION('',(-1.75658099177411E-13,-1.,-1.66321791206623E-16)) ;
#38627 = DIRECTION('',(1.75658099177411E-13,1.,1.66321791206623E-16)) ;
#38628 = DIRECTION('center_axis',(1.75658099177411E-13,1.,1.66321791206623E-16)) ;
#38629 = DIRECTION('ref_axis',(-1.,1.75658099177411E-13,4.54195640846217E-14)) ;
#38630 = DIRECTION('',(-1.75658099177411E-13,-1.,-1.66321791206623E-16)) ;
#38631 = DIRECTION('',(1.75658099177411E-13,1.,1.66321791206623E-16)) ;
#38632 = DIRECTION('center_axis',(-4.54195640846217E-14,1.66321791214601E-16,
-1.)) ;
#38633 = DIRECTION('ref_axis',(-1.75658099177411E-13,-1.,-1.66321791206623E-16)) ;
#38634 = DIRECTION('center_axis',(-1.75658099177411E-13,-1.,-1.66321791206623E-16)) ;
#38635 = DIRECTION('ref_axis',(1.,-1.75658099177411E-13,-4.54195640846217E-14)) ;
#38636 = DIRECTION('',(-1.75658099177411E-13,-1.,-1.66321791206623E-16)) ;
#38637 = DIRECTION('center_axis',(1.,-1.75658099177411E-13,-4.54195640846217E-14)) ;
#38638 = DIRECTION('ref_axis',(-4.54195640846217E-14,1.66321791214601E-16,
-1.)) ;
#38639 = DIRECTION('',(-1.75658099177411E-13,-1.,-1.66321791206623E-16)) ;
#38640 = DIRECTION('',(1.75658099177411E-13,1.,1.66321791206623E-16)) ;
#38641 = DIRECTION('center_axis',(-4.54195640846217E-14,1.66321791214601E-16,
-1.)) ;
#38642 = DIRECTION('ref_axis',(-1.,1.75658099177411E-13,4.54195640846217E-14)) ;
#38643 = DIRECTION('',(1.75658099177411E-13,1.,1.66321791206623E-16)) ;
#38644 = DIRECTION('center_axis',(-1.,1.75658099177411E-13,4.54195640846217E-14)) ;
#38645 = DIRECTION('ref_axis',(4.54195640846217E-14,-1.66321791214601E-16,
1.)) ;
#38646 = DIRECTION('',(1.75658099177411E-13,1.,1.66321791206623E-16)) ;
#38647 = DIRECTION('center_axis',(4.54195640846217E-14,-1.66321791214601E-16,
1.)) ;
#38648 = DIRECTION('ref_axis',(1.,-1.75658099177411E-13,-4.54195640846217E-14)) ;
#38649 = DIRECTION('center_axis',(1.,-1.75658099177411E-13,-4.54195640846217E-14)) ;
#38650 = DIRECTION('ref_axis',(-4.54195640846217E-14,1.66321791214601E-16,
-1.)) ;
#38651 = DIRECTION('',(-1.75658099177411E-13,-1.,-1.66321791206623E-16)) ;
#38652 = DIRECTION('',(1.75658099177411E-13,1.,1.66321791206623E-16)) ;
#38653 = DIRECTION('center_axis',(-4.54195640846217E-14,1.66321791214601E-16,
-1.)) ;
#38654 = DIRECTION('ref_axis',(-1.,1.75658099177411E-13,4.54195640846217E-14)) ;
#38655 = DIRECTION('',(1.75658099177411E-13,1.,1.66321791206623E-16)) ;
#38656 = DIRECTION('center_axis',(-1.,1.75658099177411E-13,4.54195640846217E-14)) ;
#38657 = DIRECTION('ref_axis',(4.54195640846217E-14,-1.66321791214601E-16,
1.)) ;
#38658 = DIRECTION('',(1.75658099177411E-13,1.,1.66321791206623E-16)) ;
#38659 = DIRECTION('center_axis',(4.54195640846217E-14,-1.66321791214601E-16,
1.)) ;
#38660 = DIRECTION('ref_axis',(1.,-1.75658099177411E-13,-4.54195640846217E-14)) ;
#38661 = DIRECTION('center_axis',(1.,-1.75658099177411E-13,-4.54195640846217E-14)) ;
#38662 = DIRECTION('ref_axis',(-4.54195640846217E-14,1.66321791214601E-16,
-1.)) ;
#38663 = DIRECTION('',(-1.75658099177411E-13,-1.,-1.66321791206623E-16)) ;
#38664 = DIRECTION('',(1.75658099177411E-13,1.,1.66321791206623E-16)) ;
#38665 = DIRECTION('center_axis',(-4.54195640846217E-14,1.66321791214601E-16,
-1.)) ;
#38666 = DIRECTION('ref_axis',(-1.,1.75658099177411E-13,4.54195640846217E-14)) ;
#38667 = DIRECTION('',(1.75658099177411E-13,1.,1.66321791206623E-16)) ;
#38668 = DIRECTION('center_axis',(-1.,1.75658099177411E-13,4.54195640846217E-14)) ;
#38669 = DIRECTION('ref_axis',(4.54195640846217E-14,-1.66321791214601E-16,
1.)) ;
#38670 = DIRECTION('',(1.75658099177411E-13,1.,1.66321791206623E-16)) ;
#38671 = DIRECTION('center_axis',(4.54195640846217E-14,-1.66321791214601E-16,
1.)) ;
#38672 = DIRECTION('ref_axis',(1.,-1.75658099177411E-13,-4.54195640846217E-14)) ;
#38673 = DIRECTION('center_axis',(4.54195640846217E-14,-1.66321791214601E-16,
1.)) ;
#38674 = DIRECTION('ref_axis',(1.,-1.75658099177411E-13,-4.54195640846217E-14)) ;
#38675 = DIRECTION('center_axis',(4.54195640846217E-14,-1.66321791214601E-16,
1.)) ;
#38676 = DIRECTION('ref_axis',(0.923076923076982,0.384615384615244,-4.18617815430325E-14)) ;
#38677 = DIRECTION('center_axis',(-1.,1.75658099177411E-13,4.54195640846217E-14)) ;
#38678 = DIRECTION('ref_axis',(4.54195640846217E-14,-1.66321791214601E-16,
1.)) ;
#38679 = DIRECTION('',(1.75658099177411E-13,1.,1.66321791206623E-16)) ;
#38680 = DIRECTION('',(1.75658099177411E-13,1.,1.66321791206623E-16)) ;
#38681 = DIRECTION('center_axis',(4.54195640846217E-14,-1.66321791214601E-16,
1.)) ;
#38682 = DIRECTION('ref_axis',(1.,-1.75658099177411E-13,-4.54195640846217E-14)) ;
#38683 = DIRECTION('',(-1.75658099177411E-13,-1.,-1.66321791206623E-16)) ;
#38684 = DIRECTION('center_axis',(1.,-1.75658099177411E-13,-4.54195640846217E-14)) ;
#38685 = DIRECTION('ref_axis',(-4.54195640846217E-14,1.66321791214601E-16,
-1.)) ;
#38686 = DIRECTION('',(1.75658099177411E-13,1.,1.66321791206623E-16)) ;
#38687 = DIRECTION('center_axis',(-4.54195640846217E-14,1.66321791214601E-16,
-1.)) ;
#38688 = DIRECTION('ref_axis',(-1.,1.75658099177411E-13,4.54195640846217E-14)) ;
#38689 = DIRECTION('center_axis',(-1.,1.75658099177411E-13,4.54195640846217E-14)) ;
#38690 = DIRECTION('ref_axis',(4.54195640846217E-14,-1.66321791214601E-16,
1.)) ;
#38691 = DIRECTION('',(1.75658099177411E-13,1.,1.66321791206623E-16)) ;
#38692 = DIRECTION('',(-1.75658099177411E-13,-1.,-1.66321791206623E-16)) ;
#38693 = DIRECTION('center_axis',(1.,-1.75658099177411E-13,-4.54195640846217E-14)) ;
#38694 = DIRECTION('ref_axis',(-4.54195640846217E-14,1.66321791214601E-16,
-1.)) ;
#38695 = DIRECTION('center_axis',(1.,-1.75658099177411E-13,-4.54195640846217E-14)) ;
#38696 = DIRECTION('ref_axis',(1.75658099177411E-13,1.,1.66321791206623E-16)) ;
#38697 = DIRECTION('',(-1.75658099177411E-13,-1.,-1.66321791206623E-16)) ;
#38698 = DIRECTION('',(-1.75658099177411E-13,-1.,-1.66321791206622E-16)) ;
#38699 = DIRECTION('center_axis',(1.,-1.75658099177411E-13,-4.54195640846217E-14)) ;
#38700 = DIRECTION('ref_axis',(-4.54195640846217E-14,1.66321791214601E-16,
-1.)) ;
#38701 = DIRECTION('center_axis',(-1.,1.75658099177411E-13,4.54195640846217E-14)) ;
#38702 = DIRECTION('ref_axis',(1.75658099177411E-13,1.,1.66321791206623E-16)) ;
#38703 = DIRECTION('center_axis',(-1.,1.75658099177411E-13,4.54195640846217E-14)) ;
#38704 = DIRECTION('ref_axis',(1.75658099177411E-13,1.,1.66321791206623E-16)) ;
#38705 = DIRECTION('',(-1.,1.75658099177411E-13,4.54195640846217E-14)) ;
#38706 = DIRECTION('center_axis',(1.,-1.75658099177411E-13,-4.54195640846217E-14)) ;
#38707 = DIRECTION('ref_axis',(-4.54195640846217E-14,1.66321791214601E-16,
-1.)) ;
#38708 = DIRECTION('',(1.,-1.75658099177411E-13,-4.54195640846217E-14)) ;
#38709 = DIRECTION('center_axis',(-1.,1.75658099177411E-13,4.54195640846217E-14)) ;
#38710 = DIRECTION('ref_axis',(1.75658099177411E-13,1.,1.66321791206623E-16)) ;
#38711 = DIRECTION('center_axis',(1.,-1.75658099177411E-13,-4.54195640846217E-14)) ;
#38712 = DIRECTION('ref_axis',(1.75658099177411E-13,1.,1.66321791206623E-16)) ;
#38713 = DIRECTION('',(1.75658099177411E-13,1.,1.66321791206623E-16)) ;
#38714 = DIRECTION('',(-1.75658099177411E-13,-1.,-1.66321791206622E-16)) ;
#38715 = DIRECTION('center_axis',(1.,-1.75658099177411E-13,-4.54195640846217E-14)) ;
#38716 = DIRECTION('ref_axis',(-4.54195640846217E-14,1.66321791214601E-16,
-1.)) ;
#38717 = DIRECTION('center_axis',(1.,-1.75658099177411E-13,-4.54195640846217E-14)) ;
#38718 = DIRECTION('ref_axis',(-4.54195640846217E-14,1.66321791214601E-16,
-1.)) ;
#38719 = DIRECTION('',(1.,-1.75658099177411E-13,-4.54195640846217E-14)) ;
#38720 = DIRECTION('center_axis',(-1.,1.75658099177411E-13,4.54195640846217E-14)) ;
#38721 = DIRECTION('ref_axis',(1.75658099177411E-13,1.,1.66321791206623E-16)) ;
#38722 = DIRECTION('center_axis',(1.,-1.75658099177411E-13,-4.54195640846217E-14)) ;
#38723 = DIRECTION('ref_axis',(1.75658099177411E-13,1.,1.66321791206622E-16)) ;
#38724 = DIRECTION('center_axis',(-1.,1.75658099177411E-13,4.54195640846217E-14)) ;
#38725 = DIRECTION('ref_axis',(4.54195640846217E-14,-1.66321791214601E-16,
1.)) ;
#38726 = DIRECTION('',(1.,-1.75658099177411E-13,-4.54195640846217E-14)) ;
#38727 = DIRECTION('center_axis',(1.75658099177411E-13,1.,1.66321791206623E-16)) ;
#38728 = DIRECTION('ref_axis',(-0.963207885455927,1.73873987103648E-13,0.268757454585955)) ;
#38729 = DIRECTION('center_axis',(-4.54195640846217E-14,1.66321791214601E-16,
-1.)) ;
#38730 = DIRECTION('ref_axis',(1.75658099177411E-13,1.,1.66321791206623E-16)) ;
#38731 = DIRECTION('center_axis',(1.75658099177411E-13,1.,1.66321791206623E-16)) ;
#38732 = DIRECTION('ref_axis',(-1.28008105260808E-9,1.66322016063228E-16,
-1.)) ;
#38733 = DIRECTION('center_axis',(-4.54195640846217E-14,1.66321791214601E-16,
-1.)) ;
#38734 = DIRECTION('ref_axis',(1.75658099177411E-13,1.,1.66321791206623E-16)) ;
#38735 = DIRECTION('',(-4.54195640846217E-14,1.66321791214601E-16,-1.)) ;
#38736 = DIRECTION('center_axis',(1.,-1.75658099177411E-13,-4.54195640846217E-14)) ;
#38737 = DIRECTION('ref_axis',(1.75658099177411E-13,1.,1.66321791206623E-16)) ;
#38738 = DIRECTION('',(1.75658099177411E-13,1.,1.66321791206623E-16)) ;
#38739 = DIRECTION('',(1.75658099177411E-13,1.,1.66321791206622E-16)) ;
#38740 = DIRECTION('center_axis',(1.,-1.75658099177411E-13,-4.54195640846217E-14)) ;
#38741 = DIRECTION('ref_axis',(1.75658099177411E-13,1.,1.66321791206623E-16)) ;
#38742 = DIRECTION('',(1.75658099177411E-13,1.,1.66321791206623E-16)) ;
#38743 = DIRECTION('',(1.75658099177411E-13,1.,1.66321791206622E-16)) ;
#38744 = DIRECTION('center_axis',(1.,-1.75658099177411E-13,-4.54195640846217E-14)) ;
#38745 = DIRECTION('ref_axis',(-4.54195640846217E-14,1.66321791214601E-16,
-1.)) ;
#38746 = DIRECTION('',(1.75658099177411E-13,1.,1.66321791206623E-16)) ;
#38747 = DIRECTION('',(-1.75658099177411E-13,-1.,-1.66321791206623E-16)) ;
#38748 = DIRECTION('center_axis',(1.,-1.75658099177411E-13,-4.54195640846217E-14)) ;
#38749 = DIRECTION('ref_axis',(-4.54195640846217E-14,1.66321791214601E-16,
-1.)) ;
#38750 = DIRECTION('',(1.75658099177411E-13,1.,1.66321791206623E-16)) ;
#38751 = DIRECTION('',(-1.75658099177411E-13,-1.,-1.66321791206623E-16)) ;
#38752 = DIRECTION('center_axis',(1.75658099177411E-13,1.,1.66321791206623E-16)) ;
#38753 = DIRECTION('ref_axis',(-1.,1.75658099177411E-13,4.54195640846217E-14)) ;
#38754 = DIRECTION('',(-4.54195640846217E-14,1.663217912146E-16,-1.)) ;
#38755 = DIRECTION('',(1.,-1.75658099177411E-13,-4.54195640846217E-14)) ;
#38756 = DIRECTION('',(-4.54195640846217E-14,1.66321791214601E-16,-1.)) ;
#38757 = DIRECTION('',(-1.,1.75658099177411E-13,4.54195640846217E-14)) ;
#38758 = DIRECTION('',(4.54195640846217E-14,-1.66321791214601E-16,1.)) ;
#38759 = DIRECTION('',(1.,-1.75658099177411E-13,-4.54195640846217E-14)) ;
#38760 = DIRECTION('',(4.54195640846217E-14,-1.66321791214601E-16,1.)) ;
#38761 = DIRECTION('center_axis',(-1.75658099177411E-13,-1.,-1.66321791206623E-16)) ;
#38762 = DIRECTION('ref_axis',(-1.,1.75658099177624E-13,-1.27995379816492E-9)) ;
#38763 = DIRECTION('',(-1.,1.75658099177411E-13,4.54195640846217E-14)) ;
#38764 = DIRECTION('center_axis',(-1.75658099177411E-13,-1.,-1.66321791206623E-16)) ;
#38765 = DIRECTION('ref_axis',(1.28005416232692E-9,1.66321566354742E-16,-1.)) ;
#38766 = DIRECTION('',(-4.54195640846195E-14,1.25021331759346E-14,-1.)) ;
#38767 = DIRECTION('',(4.54195640846217E-14,-1.66321791214601E-16,1.)) ;
#38768 = DIRECTION('center_axis',(-1.75658099177411E-13,-1.,-1.66321791206623E-16)) ;
#38769 = DIRECTION('ref_axis',(1.,-1.75658099177411E-13,-4.54195640846217E-14)) ;
#38770 = DIRECTION('center_axis',(-1.75658099177411E-13,-1.,-1.66321791206623E-16)) ;
#38771 = DIRECTION('ref_axis',(1.,-1.75658099177411E-13,-4.54195640846217E-14)) ;
#38772 = DIRECTION('center_axis',(-1.75658099177411E-13,-1.,-1.66321791206623E-16)) ;
#38773 = DIRECTION('ref_axis',(1.,-1.75658099177411E-13,-4.54195640846217E-14)) ;
#38774 = DIRECTION('center_axis',(-1.75658099177411E-13,-1.,-1.66321791206623E-16)) ;
#38775 = DIRECTION('ref_axis',(1.,-1.75658099177411E-13,-4.54195640846217E-14)) ;
#38776 = DIRECTION('center_axis',(4.54195640846217E-14,-1.66321791214601E-16,
1.)) ;
#38777 = DIRECTION('ref_axis',(-1.,1.75658099177411E-13,4.54195640846217E-14)) ;
#38778 = DIRECTION('center_axis',(-4.54195640846217E-14,1.66321791214601E-16,
-1.)) ;
#38779 = DIRECTION('ref_axis',(0.707106781186648,0.707106781186447,-3.19988744963506E-14)) ;
#38780 = DIRECTION('',(1.,-1.75658099177411E-13,-4.54195640846217E-14)) ;
#38781 = DIRECTION('center_axis',(-4.54195640846217E-14,1.66321791214601E-16,
-1.)) ;
#38782 = DIRECTION('ref_axis',(-0.707106781186397,0.707106781186698,3.22340890291931E-14)) ;
#38783 = DIRECTION('center_axis',(-1.75658099177411E-13,-1.,-1.66321791206623E-16)) ;
#38784 = DIRECTION('ref_axis',(1.,-1.75658099177411E-13,-4.54195640846217E-14)) ;
#38785 = DIRECTION('center_axis',(1.75658099177411E-13,1.,1.66321791206623E-16)) ;
#38786 = DIRECTION('ref_axis',(1.,-1.75658099177411E-13,-4.54195640846217E-14)) ;
#38787 = DIRECTION('',(-1.75658099177411E-13,-1.,-1.66321791206623E-16)) ;
#38788 = DIRECTION('center_axis',(1.75658099177411E-13,1.,1.66321791206623E-16)) ;
#38789 = DIRECTION('ref_axis',(-1.,1.75658099177411E-13,4.54195640846217E-14)) ;
#38790 = DIRECTION('center_axis',(1.75658099177411E-13,1.,1.66321791206623E-16)) ;
#38791 = DIRECTION('ref_axis',(-1.,1.75658099177411E-13,4.54195640846217E-14)) ;
#38792 = DIRECTION('center_axis',(-1.75658099177411E-13,-1.,-1.66321791206623E-16)) ;
#38793 = DIRECTION('ref_axis',(-4.54195640846217E-14,1.66321791214601E-16,
-1.)) ;
#38794 = DIRECTION('',(-9.21791469415371E-14,-0.707106781186548,0.707106781186547)) ;
#38795 = DIRECTION('center_axis',(-1.75658099177411E-13,-1.,-1.66321791206623E-16)) ;
#38796 = DIRECTION('ref_axis',(1.,-1.75658099177411E-13,-4.54195640846217E-14)) ;
#38797 = DIRECTION('center_axis',(1.75658099177411E-13,1.,1.66321791206623E-16)) ;
#38798 = DIRECTION('ref_axis',(1.,-1.75658099177411E-13,-4.54195640846217E-14)) ;
#38799 = DIRECTION('',(-1.75658099177411E-13,-1.,-1.66321791206623E-16)) ;
#38800 = DIRECTION('center_axis',(1.75658099177411E-13,1.,1.66321791206623E-16)) ;
#38801 = DIRECTION('ref_axis',(-1.,1.75658099177411E-13,4.54195640846217E-14)) ;
#38802 = DIRECTION('center_axis',(1.75658099177411E-13,1.,1.66321791206623E-16)) ;
#38803 = DIRECTION('ref_axis',(-1.,1.75658099177411E-13,4.54195640846217E-14)) ;
#38804 = DIRECTION('center_axis',(-1.75658099177411E-13,-1.,-1.66321791206623E-16)) ;
#38805 = DIRECTION('ref_axis',(-4.54195640846217E-14,1.66321791214601E-16,
-1.)) ;
#38806 = DIRECTION('',(-9.21791469415371E-14,-0.707106781186548,0.707106781186547)) ;
#38807 = DIRECTION('center_axis',(-1.75658099177411E-13,-1.,-1.66321791206623E-16)) ;
#38808 = DIRECTION('ref_axis',(1.,-1.75658099177411E-13,-4.54195640846217E-14)) ;
#38809 = DIRECTION('center_axis',(1.75658099177411E-13,1.,1.66321791206623E-16)) ;
#38810 = DIRECTION('ref_axis',(1.,-1.75658099177411E-13,-4.54195640846217E-14)) ;
#38811 = DIRECTION('',(-1.75658099177411E-13,-1.,-1.66321791206623E-16)) ;
#38812 = DIRECTION('center_axis',(1.75658099177411E-13,1.,1.66321791206623E-16)) ;
#38813 = DIRECTION('ref_axis',(-1.,1.75658099177411E-13,4.54195640846217E-14)) ;
#38814 = DIRECTION('center_axis',(1.75658099177411E-13,1.,1.66321791206623E-16)) ;
#38815 = DIRECTION('ref_axis',(-1.,1.75658099177411E-13,4.54195640846217E-14)) ;
#38816 = DIRECTION('center_axis',(-1.75658099177411E-13,-1.,-1.66321791206623E-16)) ;
#38817 = DIRECTION('ref_axis',(-4.54195640846217E-14,1.66321791214601E-16,
-1.)) ;
#38818 = DIRECTION('',(-9.21791469415371E-14,-0.707106781186548,0.707106781186547)) ;
#38819 = DIRECTION('center_axis',(-1.75658099177411E-13,-1.,-1.66321791206623E-16)) ;
#38820 = DIRECTION('ref_axis',(1.,-1.75658099177411E-13,-4.54195640846217E-14)) ;
#38821 = DIRECTION('center_axis',(1.75658099177411E-13,1.,1.66321791206623E-16)) ;
#38822 = DIRECTION('ref_axis',(1.,-1.75658099177411E-13,-4.54195640846217E-14)) ;
#38823 = DIRECTION('',(-1.75658099177411E-13,-1.,-1.66321791206623E-16)) ;
#38824 = DIRECTION('center_axis',(1.75658099177411E-13,1.,1.66321791206623E-16)) ;
#38825 = DIRECTION('ref_axis',(-1.,1.75658099177411E-13,4.54195640846217E-14)) ;
#38826 = DIRECTION('center_axis',(1.75658099177411E-13,1.,1.66321791206623E-16)) ;
#38827 = DIRECTION('ref_axis',(-1.,1.75658099177411E-13,4.54195640846217E-14)) ;
#38828 = DIRECTION('center_axis',(-1.75658099177411E-13,-1.,-1.66321791206623E-16)) ;
#38829 = DIRECTION('ref_axis',(-4.54195640846217E-14,1.66321791214601E-16,
-1.)) ;
#38830 = DIRECTION('',(-9.21791469415371E-14,-0.707106781186548,0.707106781186547)) ;
#38831 = DIRECTION('center_axis',(-1.,1.75658099177411E-13,4.54195640846217E-14)) ;
#38832 = DIRECTION('ref_axis',(4.54195640846217E-14,-1.66321791214601E-16,
1.)) ;
#38833 = DIRECTION('',(4.54195640846217E-14,-1.66321791214601E-16,1.)) ;
#38834 = DIRECTION('',(1.75658099177411E-13,1.,1.66321791206623E-16)) ;
#38835 = DIRECTION('',(-1.75658099177411E-13,-1.,-1.66321791206623E-16)) ;
#38836 = DIRECTION('center_axis',(-4.54195640846217E-14,1.66321791214601E-16,
-1.)) ;
#38837 = DIRECTION('ref_axis',(-1.,5.55236256206829E-46,4.54195640846217E-14)) ;
#38838 = DIRECTION('center_axis',(-4.54195640846217E-14,1.66321791214601E-16,
-1.)) ;
#38839 = DIRECTION('ref_axis',(-0.923076923076982,-0.384615384615244,4.18617815430325E-14)) ;
#38840 = DIRECTION('center_axis',(-4.54195640846217E-14,1.66321791214601E-16,
-1.)) ;
#38841 = DIRECTION('ref_axis',(-1.,5.55236256206829E-46,4.54195640846217E-14)) ;
#38842 = DIRECTION('center_axis',(4.54195640846217E-14,-1.66321791214601E-16,
1.)) ;
#38843 = DIRECTION('ref_axis',(0.923076923076847,-0.384615384615568,-4.19897213824222E-14)) ;
#38844 = DIRECTION('center_axis',(1.,-1.75658099177411E-13,-4.54195640846217E-14)) ;
#38845 = DIRECTION('ref_axis',(1.75658099177411E-13,1.,1.66321791206623E-16)) ;
#38846 = DIRECTION('',(1.75658099177411E-13,1.,1.66321791206623E-16)) ;
#38847 = DIRECTION('center_axis',(1.,-1.75658099177411E-13,-4.54195640846217E-14)) ;
#38848 = DIRECTION('ref_axis',(-1.75658099177411E-13,-1.,-1.66321791206623E-16)) ;
#38849 = DIRECTION('',(-1.75658099177411E-13,-1.,-1.66321791206622E-16)) ;
#38850 = DIRECTION('',(1.75658099177411E-13,1.,1.66321791206623E-16)) ;
#38851 = DIRECTION('center_axis',(1.,-1.75658099177411E-13,-4.54195640846217E-14)) ;
#38852 = DIRECTION('ref_axis',(1.75658099177411E-13,1.,1.66321791206623E-16)) ;
#38853 = DIRECTION('',(-1.75658099177411E-13,-1.,-1.66321791206623E-16)) ;
#38854 = DIRECTION('',(1.75658099177411E-13,1.,1.66321791206622E-16)) ;
#38855 = DIRECTION('',(-1.75658099177411E-13,-1.,-1.66321791206623E-16)) ;
#38856 = DIRECTION('center_axis',(4.54195640846217E-14,-1.66321791214601E-16,
1.)) ;
#38857 = DIRECTION('ref_axis',(1.,-1.75658099177411E-13,-4.54195640846217E-14)) ;
#38858 = DIRECTION('',(-1.75658099177411E-13,-1.,-1.66321791206623E-16)) ;
#38859 = DIRECTION('',(-1.75658099177411E-13,-1.,-1.66321791206623E-16)) ;
#38860 = DIRECTION('center_axis',(1.,-1.75658099177411E-13,-4.54195640846217E-14)) ;
#38861 = DIRECTION('ref_axis',(-4.54195640846217E-14,1.66321791214601E-16,
-1.)) ;
#38862 = DIRECTION('',(1.75658099177411E-13,1.,1.66321791206623E-16)) ;
#38863 = DIRECTION('center_axis',(-4.54195640846217E-14,1.66321791214601E-16,
-1.)) ;
#38864 = DIRECTION('ref_axis',(-1.,1.75658099177411E-13,4.54195640846217E-14)) ;
#38865 = DIRECTION('',(-1.75658099177411E-13,-1.,-1.66321791206623E-16)) ;
#38866 = DIRECTION('center_axis',(-1.,1.75658099177411E-13,4.54195640846217E-14)) ;
#38867 = DIRECTION('ref_axis',(4.54195640846217E-14,-1.66321791214601E-16,
1.)) ;
#38868 = DIRECTION('center_axis',(1.,-1.75658099177411E-13,-4.54195640846217E-14)) ;
#38869 = DIRECTION('ref_axis',(-4.54195640846217E-14,1.66321791214601E-16,
-1.)) ;
#38870 = DIRECTION('',(-1.75658099177411E-13,-1.,-1.66321791206622E-16)) ;
#38871 = DIRECTION('',(-4.54195640846217E-14,1.66321791214601E-16,-1.)) ;
#38872 = DIRECTION('',(-1.75658099177411E-13,-1.,-1.66321791206622E-16)) ;
#38873 = DIRECTION('center_axis',(1.75658099177411E-13,1.,1.66321791206623E-16)) ;
#38874 = DIRECTION('ref_axis',(-1.,1.75658099177411E-13,4.54195640846217E-14)) ;
#38875 = DIRECTION('',(-1.75658099177411E-13,-1.,-1.66321791206623E-16)) ;
#38876 = DIRECTION('',(1.75658099177411E-13,1.,1.66321791206623E-16)) ;
#38877 = DIRECTION('center_axis',(1.75658099177411E-13,1.,1.66321791206623E-16)) ;
#38878 = DIRECTION('ref_axis',(-1.,1.75658099177411E-13,4.54195640846217E-14)) ;
#38879 = DIRECTION('center_axis',(-4.54195640846217E-14,1.66321791214601E-16,
-1.)) ;
#38880 = DIRECTION('ref_axis',(-1.75658099177411E-13,-1.,-1.66321791206623E-16)) ;
#38881 = DIRECTION('center_axis',(4.54195640846217E-14,-1.66321791214601E-16,
1.)) ;
#38882 = DIRECTION('ref_axis',(-1.,1.75658099177411E-13,4.54195640846217E-14)) ;
#38883 = DIRECTION('center_axis',(4.54195640846217E-14,-1.66321791214601E-16,
1.)) ;
#38884 = DIRECTION('ref_axis',(-0.923076923076982,-0.384615384615244,4.18617815430325E-14)) ;
#38885 = DIRECTION('center_axis',(4.54195640846217E-14,-1.66321791214601E-16,
1.)) ;
#38886 = DIRECTION('ref_axis',(-1.75658099177411E-13,-1.,-1.66321791206623E-16)) ;
#38887 = DIRECTION('center_axis',(-4.54195640846217E-14,1.66321791214601E-16,
-1.)) ;
#38888 = DIRECTION('ref_axis',(-1.,1.75658099177411E-13,4.54195640846217E-14)) ;
#38889 = DIRECTION('',(-1.75658099177411E-13,-1.,-1.66321791206623E-16)) ;
#38890 = DIRECTION('',(1.75658099177411E-13,1.,1.66321791206623E-16)) ;
#38891 = DIRECTION('center_axis',(-1.,1.75658099177411E-13,4.54195640846217E-14)) ;
#38892 = DIRECTION('ref_axis',(4.54195640846217E-14,-1.66321791214601E-16,
1.)) ;
#38893 = DIRECTION('',(-1.75658099177411E-13,-1.,-1.66321791206623E-16)) ;
#38894 = DIRECTION('center_axis',(4.54195640846217E-14,-1.66321791214601E-16,
1.)) ;
#38895 = DIRECTION('ref_axis',(1.,-1.75658099177411E-13,-4.54195640846217E-14)) ;
#38896 = DIRECTION('',(-1.75658099177411E-13,-1.,-1.66321791206623E-16)) ;
#38897 = DIRECTION('center_axis',(1.,-1.75658099177411E-13,-4.54195640846217E-14)) ;
#38898 = DIRECTION('ref_axis',(-4.54195640846217E-14,1.66321791214601E-16,
-1.)) ;
#38899 = DIRECTION('center_axis',(-4.54195640846217E-14,1.66321791214601E-16,
-1.)) ;
#38900 = DIRECTION('ref_axis',(-1.,1.75658099177411E-13,4.54195640846217E-14)) ;
#38901 = DIRECTION('',(-1.75658099177411E-13,-1.,-1.66321791206623E-16)) ;
#38902 = DIRECTION('',(1.75658099177411E-13,1.,1.66321791206623E-16)) ;
#38903 = DIRECTION('center_axis',(-1.,1.75658099177411E-13,4.54195640846217E-14)) ;
#38904 = DIRECTION('ref_axis',(4.54195640846217E-14,-1.66321791214601E-16,
1.)) ;
#38905 = DIRECTION('',(-1.75658099177411E-13,-1.,-1.66321791206623E-16)) ;
#38906 = DIRECTION('center_axis',(4.54195640846217E-14,-1.66321791214601E-16,
1.)) ;
#38907 = DIRECTION('ref_axis',(1.,-1.75658099177411E-13,-4.54195640846217E-14)) ;
#38908 = DIRECTION('',(-1.75658099177411E-13,-1.,-1.66321791206623E-16)) ;
#38909 = DIRECTION('center_axis',(1.,-1.75658099177411E-13,-4.54195640846217E-14)) ;
#38910 = DIRECTION('ref_axis',(-4.54195640846217E-14,1.66321791214601E-16,
-1.)) ;
#38911 = DIRECTION('center_axis',(-1.75658099177411E-13,-1.,-1.66321791206623E-16)) ;
#38912 = DIRECTION('ref_axis',(0.963207885455952,-1.73873987103648E-13,0.268757454585867)) ;
#38913 = DIRECTION('center_axis',(1.,-1.75658099177411E-13,-4.54195640846217E-14)) ;
#38914 = DIRECTION('ref_axis',(4.54195640846217E-14,-1.66321791214601E-16,
1.)) ;
#38915 = DIRECTION('center_axis',(-4.54195640846217E-14,1.66321791214601E-16,
-1.)) ;
#38916 = DIRECTION('ref_axis',(-1.75658099177411E-13,-1.,-1.66321791206623E-16)) ;
#38917 = DIRECTION('center_axis',(-1.,1.75658099177411E-13,4.54195640846217E-14)) ;
#38918 = DIRECTION('ref_axis',(-1.75658099177411E-13,-1.,-1.66321791206622E-16)) ;
#38919 = DIRECTION('center_axis',(-1.,1.75658099177411E-13,4.54195640846217E-14)) ;
#38920 = DIRECTION('ref_axis',(-1.75658099177411E-13,-1.,-1.66321791206622E-16)) ;
#38921 = DIRECTION('center_axis',(-1.75658099177411E-13,-1.,-1.66321791206623E-16)) ;
#38922 = DIRECTION('ref_axis',(0.268757454585866,-4.6812227297136E-14,-0.963207885455952)) ;
#38923 = DIRECTION('center_axis',(-4.54195640846217E-14,1.66321791214601E-16,
-1.)) ;
#38924 = DIRECTION('ref_axis',(1.,-1.75658099177411E-13,-4.54195640846217E-14)) ;
#38925 = DIRECTION('center_axis',(1.,-1.75658099177411E-13,-4.54195640846217E-14)) ;
#38926 = DIRECTION('ref_axis',(-1.75658099177411E-13,-1.,-1.66321791206623E-16)) ;
#38927 = DIRECTION('',(1.,-1.75658099177411E-13,-4.54195640846217E-14)) ;
#38928 = DIRECTION('center_axis',(1.,-1.75658099177411E-13,-4.54195640846217E-14)) ;
#38929 = DIRECTION('ref_axis',(-1.75658099177411E-13,-1.,-1.66321791206623E-16)) ;
#38930 = DIRECTION('center_axis',(1.,-1.75658099177411E-13,-4.54195640846217E-14)) ;
#38931 = DIRECTION('ref_axis',(1.75658099177411E-13,1.,1.66321791206623E-16)) ;
#38932 = DIRECTION('',(-1.75658099177411E-13,-1.,-1.66321791206622E-16)) ;
#38933 = DIRECTION('',(1.75658099177411E-13,1.,1.66321791206623E-16)) ;
#38934 = DIRECTION('center_axis',(-1.,1.75658099177411E-13,4.54195640846217E-14)) ;
#38935 = DIRECTION('ref_axis',(-4.54195640846217E-14,1.66321791214601E-16,
-1.)) ;
#38936 = DIRECTION('center_axis',(-1.,1.75658099177411E-13,4.54195640846217E-14)) ;
#38937 = DIRECTION('ref_axis',(-4.54195640846217E-14,1.66321791214601E-16,
-1.)) ;
#38938 = DIRECTION('',(-1.,1.75658099177411E-13,4.54195640846217E-14)) ;
#38939 = DIRECTION('center_axis',(1.,-1.75658099177411E-13,-4.54195640846217E-14)) ;
#38940 = DIRECTION('ref_axis',(1.75658099177411E-13,1.,1.66321791206623E-16)) ;
#38941 = DIRECTION('',(-1.75658099177411E-13,-1.,-1.66321791206623E-16)) ;
#38942 = DIRECTION('',(1.75658099177411E-13,1.,1.66321791206622E-16)) ;
#38943 = DIRECTION('center_axis',(-4.54195640846217E-14,1.66321791214601E-16,
-1.)) ;
#38944 = DIRECTION('ref_axis',(-1.75658099177411E-13,-1.,-1.66321791206623E-16)) ;
#38945 = DIRECTION('center_axis',(-4.54195640846217E-14,1.66321791214601E-16,
-1.)) ;
#38946 = DIRECTION('ref_axis',(-0.384615384615568,-0.923076923076847,1.73155353022032E-14)) ;
#38947 = DIRECTION('center_axis',(4.54195640846217E-14,-1.66321791214601E-16,
1.)) ;
#38948 = DIRECTION('ref_axis',(-1.,1.75658099177411E-13,4.54195640846217E-14)) ;
#38949 = DIRECTION('center_axis',(4.54195640846217E-14,-1.66321791214601E-16,
1.)) ;
#38950 = DIRECTION('ref_axis',(-1.75658099177411E-13,-1.,-1.66321791206623E-16)) ;
#38951 = DIRECTION('center_axis',(-1.75658099177411E-13,-1.,-1.66321791206623E-16)) ;
#38952 = DIRECTION('ref_axis',(2.14929886997261E-46,1.66321791206623E-16,
-1.)) ;
#38953 = DIRECTION('',(1.,-1.75658099177411E-13,-4.54195640846217E-14)) ;
#38954 = DIRECTION('',(-4.54195640846217E-14,1.66321791214601E-16,-1.)) ;
#38955 = DIRECTION('',(-4.54195640846217E-14,1.66321791214601E-16,-1.)) ;
#38956 = DIRECTION('center_axis',(-1.75658099177411E-13,-1.,-1.66321791206623E-16)) ;
#38957 = DIRECTION('ref_axis',(1.,-1.75658099177411E-13,-4.54195640846217E-14)) ;
#38958 = DIRECTION('center_axis',(0.000159104274938584,-0.999999372085354,
-0.00110928568305424)) ;
#38959 = DIRECTION('ref_axis',(-0.00379983340424099,0.00110867311936705,-0.999992166024322)) ;
#38960 = DIRECTION('',(-1.75658099177411E-13,-1.,-1.66321791206623E-16)) ;
#38961 = DIRECTION('center_axis',(0.000159104274938584,-0.999999372085354,
-0.00110928568305424)) ;
#38962 = DIRECTION('ref_axis',(-0.00379983340424099,0.00110867311936705,-0.999992166024322)) ;
#38963 = DIRECTION('center_axis',(1.61486985400024E-13,1.,0.)) ;
#38964 = DIRECTION('ref_axis',(0.00363593456997526,-5.87156112817037E-16,
0.999993389968055)) ;
#38965 = DIRECTION('',(-0.002570993990266,0.707106781186547,-0.707102107188137)) ;
#38966 = DIRECTION('center_axis',(3.1720657846433E-16,-5.63472075157877E-29,
1.)) ;
#38967 = DIRECTION('ref_axis',(-1.,1.75658099177411E-13,3.1720657846433E-16)) ;
#38968 = DIRECTION('',(1.77635683940029E-13,1.,0.)) ;
#38969 = DIRECTION('',(-1.77635683940029E-13,-1.,0.)) ;
#38970 = DIRECTION('',(-1.,1.75658099177411E-13,3.1720657846433E-16)) ;
#38971 = DIRECTION('center_axis',(-1.,1.77635683940029E-13,3.28915439981538E-31)) ;
#38972 = DIRECTION('ref_axis',(2.92157696951376E-29,1.66321791206623E-16,
-1.)) ;
#38973 = DIRECTION('',(1.77635683940029E-13,1.,0.)) ;
#38974 = DIRECTION('',(-1.77635683940029E-13,-1.,0.)) ;
#38975 = DIRECTION('',(2.92157696951376E-29,1.66321791206623E-16,-1.)) ;
#38976 = DIRECTION('center_axis',(-6.34413156928661E-16,1.12694415031575E-28,
-1.)) ;
#38977 = DIRECTION('ref_axis',(1.,-1.75658099177411E-13,-6.34413156928661E-16)) ;
#38978 = DIRECTION('',(-1.77635683940029E-13,-1.,0.)) ;
#38979 = DIRECTION('',(1.,-1.75658099177411E-13,-6.34413156928661E-16)) ;
#38980 = DIRECTION('',(1.77635683940029E-13,1.,0.)) ;
#38981 = DIRECTION('center_axis',(1.,-1.77635683940029E-13,-3.28915439981538E-31)) ;
#38982 = DIRECTION('ref_axis',(-2.92157696951376E-29,-1.66321791206623E-16,
1.)) ;
#38983 = DIRECTION('',(-1.77635683940029E-13,-1.,0.)) ;
#38984 = DIRECTION('',(-2.92157696951376E-29,-1.66321791206623E-16,1.)) ;
#38985 = DIRECTION('',(1.77635683940029E-13,1.,0.)) ;
#38986 = DIRECTION('center_axis',(-1.77635683940029E-13,-1.,0.)) ;
#38987 = DIRECTION('ref_axis',(-0.707106781186573,1.25607396694709E-13,-0.707106781186523)) ;
#38988 = DIRECTION('center_axis',(0.,-1.,0.)) ;
#38989 = DIRECTION('ref_axis',(0.,0.,-1.)) ;
#38990 = DIRECTION('center_axis',(-1.77635683940029E-13,-1.,0.)) ;
#38991 = DIRECTION('ref_axis',(0.707106781186522,-1.256073966947E-13,-0.707106781186573)) ;
#38992 = DIRECTION('center_axis',(0.,-1.,-5.68434188608072E-13)) ;
#38993 = DIRECTION('ref_axis',(1.,0.,0.)) ;
#38994 = DIRECTION('center_axis',(1.,-1.75658099177411E-13,-6.34413156928661E-16)) ;
#38995 = DIRECTION('ref_axis',(1.24657630944033E-13,0.707106781186598,0.707106781186497)) ;
#38996 = DIRECTION('center_axis',(-1.,1.42108547151988E-13,0.)) ;
#38997 = DIRECTION('ref_axis',(0.,0.,1.)) ;
#38998 = DIRECTION('center_axis',(1.,-1.42108547151988E-13,0.)) ;
#38999 = DIRECTION('ref_axis',(1.42108547151988E-13,1.,0.)) ;
#39000 = DIRECTION('center_axis',(-1.77635683940029E-13,-1.,0.)) ;
#39001 = DIRECTION('ref_axis',(-0.707106781186573,1.25607396694709E-13,0.707106781186523)) ;
#39002 = DIRECTION('center_axis',(0.,-1.,0.)) ;
#39003 = DIRECTION('ref_axis',(-1.,0.,0.)) ;
#39004 = DIRECTION('center_axis',(-1.,1.75658099177411E-13,3.1720657846433E-16)) ;
#39005 = DIRECTION('ref_axis',(1.23984734176031E-13,0.707106781186623,-0.707106781186472)) ;
#39006 = DIRECTION('center_axis',(1.,-1.42108547152069E-13,0.)) ;
#39007 = DIRECTION('ref_axis',(0.,0.,-1.)) ;
#39008 = DIRECTION('center_axis',(-1.,1.42108547152069E-13,0.)) ;
#39009 = DIRECTION('ref_axis',(1.42108547152069E-13,1.,0.)) ;
#39010 = DIRECTION('center_axis',(-1.77635683940029E-13,-1.,0.)) ;
#39011 = DIRECTION('ref_axis',(0.707106781186522,-1.256073966947E-13,0.707106781186573)) ;
#39012 = DIRECTION('center_axis',(-5.68434188608112E-13,-1.,0.)) ;
#39013 = DIRECTION('ref_axis',(0.,0.,1.)) ;
#39014 = DIRECTION('center_axis',(-2.92157696951376E-29,-1.66321791206623E-16,
1.)) ;
#39015 = DIRECTION('ref_axis',(-0.707106781186347,0.707106781186749,1.17607266421309E-16)) ;
#39016 = DIRECTION('center_axis',(0.,0.,-1.)) ;
#39017 = DIRECTION('ref_axis',(-1.,0.,0.)) ;
#39018 = DIRECTION('center_axis',(0.,0.,1.)) ;
#39019 = DIRECTION('ref_axis',(1.42108547151988E-13,1.,0.)) ;
#39020 = DIRECTION('center_axis',(1.42108547152069E-13,1.,0.)) ;
#39021 = DIRECTION('ref_axis',(0.,0.,1.)) ;
#39022 = DIRECTION('center_axis',(2.92157696951376E-29,1.66321791206623E-16,
-1.)) ;
#39023 = DIRECTION('ref_axis',(0.707106781186548,0.707106781186548,1.17607266421317E-16)) ;
#39024 = DIRECTION('center_axis',(0.,0.,1.)) ;
#39025 = DIRECTION('ref_axis',(1.,0.,0.)) ;
#39026 = DIRECTION('center_axis',(0.,0.,-1.)) ;
#39027 = DIRECTION('ref_axis',(1.42108547151988E-13,1.,0.)) ;
#39028 = DIRECTION('center_axis',(-1.42108547152069E-13,-1.,0.)) ;
#39029 = DIRECTION('ref_axis',(0.,0.,-1.)) ;
#39030 = DIRECTION('center_axis',(-1.42108547151988E-13,-1.,0.)) ;
#39031 = DIRECTION('ref_axis',(0.,0.,-1.)) ;
#39032 = DIRECTION('center_axis',(-1.42108547151988E-13,-1.,0.)) ;
#39033 = DIRECTION('ref_axis',(0.,0.,-1.)) ;
#39034 = DIRECTION('center_axis',(4.54195640846217E-14,-1.66321791214601E-16,
1.)) ;
#39035 = DIRECTION('ref_axis',(1.,-1.75658099177411E-13,-4.54195640846217E-14)) ;
#39036 = DIRECTION('center_axis',(-4.54195640846217E-14,1.66321791214601E-16,
-1.)) ;
#39037 = DIRECTION('ref_axis',(-0.707106781186661,-0.707106781186434,3.19988744963512E-14)) ;
#39038 = DIRECTION('',(-1.,1.75658099177411E-13,4.54195640846217E-14)) ;
#39039 = DIRECTION('center_axis',(-4.54195640846217E-14,1.66321791214601E-16,
-1.)) ;
#39040 = DIRECTION('ref_axis',(0.707106781186403,-0.707106781186692,-3.22340890291934E-14)) ;
#39041 = DIRECTION('center_axis',(-4.54195640846217E-14,1.66321791214601E-16,
-1.)) ;
#39042 = DIRECTION('ref_axis',(-1.,1.75658099177411E-13,4.54195640846217E-14)) ;
#39043 = DIRECTION('center_axis',(-4.54195640846217E-14,1.66321791214601E-16,
-1.)) ;
#39044 = DIRECTION('ref_axis',(0.707106781186648,0.707106781186447,-3.19988744963506E-14)) ;
#39045 = DIRECTION('center_axis',(4.54195640846217E-14,-1.66321791214601E-16,
1.)) ;
#39046 = DIRECTION('ref_axis',(0.707106781186648,0.707106781186447,-3.19988744963506E-14)) ;
#39047 = DIRECTION('center_axis',(-3.10862446895045E-14,5.52202633654702E-27,
-1.)) ;
#39048 = DIRECTION('ref_axis',(1.77635683940023E-13,1.,-2.00890147845606E-41)) ;
#39049 = DIRECTION('',(4.54195640846217E-14,-1.66321791214601E-16,1.)) ;
#39050 = DIRECTION('center_axis',(4.54195640846217E-14,-1.66321791214601E-16,
1.)) ;
#39051 = DIRECTION('ref_axis',(1.,-1.75658099177411E-13,-4.54195640846217E-14)) ;
#39052 = DIRECTION('center_axis',(4.54195640846217E-14,-1.66321791214601E-16,
1.)) ;
#39053 = DIRECTION('ref_axis',(0.707106781186648,0.707106781186447,-3.19988744963506E-14)) ;
#39054 = DIRECTION('center_axis',(4.54195640846217E-14,-1.66321791214601E-16,
1.)) ;
#39055 = DIRECTION('ref_axis',(0.707106781186648,0.707106781186447,-3.19988744963506E-14)) ;
#39056 = DIRECTION('',(4.54195640846217E-14,-1.66321791214601E-16,1.)) ;
#39057 = DIRECTION('center_axis',(-4.54195640846217E-14,1.66321791214601E-16,
-1.)) ;
#39058 = DIRECTION('ref_axis',(0.707106781186403,-0.707106781186692,-3.22340890291934E-14)) ;
#39059 = DIRECTION('center_axis',(-3.77475828372543E-14,6.66133814775755E-15,
-1.)) ;
#39060 = DIRECTION('ref_axis',(1.,-1.77635683940026E-13,-3.77475828372555E-14)) ;
#39061 = DIRECTION('',(-4.54195640846217E-14,1.66321791214601E-16,-1.)) ;
#39062 = DIRECTION('center_axis',(4.54195640846217E-14,-1.66321791214601E-16,
1.)) ;
#39063 = DIRECTION('ref_axis',(-0.707106781186397,0.707106781186698,3.22340890291931E-14)) ;
#39064 = DIRECTION('center_axis',(-5.1070259132759E-14,-6.66133814774199E-15,
-1.)) ;
#39065 = DIRECTION('ref_axis',(-1.,1.77635683940027E-13,5.10702591327578E-14)) ;
#39066 = DIRECTION('',(-4.54195640846217E-14,1.66321791214601E-16,-1.)) ;
#39067 = DIRECTION('center_axis',(1.75658099177411E-13,1.,1.66321791206623E-16)) ;
#39068 = DIRECTION('ref_axis',(-1.,1.75658099177411E-13,4.54195640846217E-14)) ;
#39069 = DIRECTION('center_axis',(-1.75658099177411E-13,-1.,-1.66321791206623E-16)) ;
#39070 = DIRECTION('ref_axis',(0.258819045102331,-4.53030069799869E-14,-0.965925826289119)) ;
#39071 = DIRECTION('',(1.,-1.75658099177411E-13,-4.54195640846217E-14)) ;
#39072 = DIRECTION('center_axis',(-1.75658099177411E-13,-1.,-1.66321791206623E-16)) ;
#39073 = DIRECTION('ref_axis',(-0.258819045102564,4.56243160072301E-14,-0.965925826289057)) ;
#39074 = DIRECTION('center_axis',(1.,-1.77635683940023E-13,-4.44089209850062E-14)) ;
#39075 = DIRECTION('ref_axis',(-4.44089209850062E-14,0.,-1.)) ;
#39076 = DIRECTION('center_axis',(-1.,1.75658099177411E-13,4.54195640846217E-14)) ;
#39077 = DIRECTION('ref_axis',(9.20925513359143E-14,0.707106781186551,-0.707106781186544)) ;
#39078 = DIRECTION('center_axis',(1.,-1.77635683940023E-13,-1.42108547152023E-13)) ;
#39079 = DIRECTION('ref_axis',(-1.42108547152023E-13,0.,-1.)) ;
#39080 = DIRECTION('center_axis',(-1.75658099177411E-13,-1.,-1.66321791206623E-16)) ;
#39081 = DIRECTION('ref_axis',(1.,-1.75658099177411E-13,-4.54195640846217E-14)) ;
#39082 = DIRECTION('center_axis',(1.75658099177411E-13,1.,1.66321791206623E-16)) ;
#39083 = DIRECTION('ref_axis',(0.258819045102475,-4.53030069800122E-14,-0.965925826289081)) ;
#39084 = DIRECTION('',(4.54195640846217E-14,-1.66321791214601E-16,1.)) ;
#39085 = DIRECTION('center_axis',(1.75658099177411E-13,1.,1.66321791206623E-16)) ;
#39086 = DIRECTION('ref_axis',(-0.258819045102557,4.56243160072289E-14,-0.965925826289059)) ;
#39087 = DIRECTION('',(-1.,1.75658099177411E-13,4.54195640846217E-14)) ;
#39088 = DIRECTION('center_axis',(-4.54195640846217E-14,1.66321791214601E-16,
-1.)) ;
#39089 = DIRECTION('ref_axis',(-0.707106781186661,-0.707106781186434,3.19988744963512E-14)) ;
#39090 = DIRECTION('center_axis',(-5.77315972805084E-14,8.71691300269209E-27,
-1.)) ;
#39091 = DIRECTION('ref_axis',(-1.50990331349019E-13,-1.,-2.86985925493723E-42)) ;
#39092 = DIRECTION('center_axis',(-1.,1.77635683940029E-13,4.44089209850064E-14)) ;
#39093 = DIRECTION('ref_axis',(-4.44089209850064E-14,0.,-1.)) ;
#39094 = DIRECTION('center_axis',(1.,-1.75658099177411E-13,-4.54195640846217E-14)) ;
#39095 = DIRECTION('ref_axis',(-1.5632551486146E-13,-0.707106781186551,-0.707106781186544)) ;
#39096 = DIRECTION('center_axis',(-1.,1.77635683940023E-13,2.66453525910034E-14)) ;
#39097 = DIRECTION('ref_axis',(-2.66453525910034E-14,0.,-1.)) ;
#39098 = DIRECTION('center_axis',(4.54195640846217E-14,-1.66321791214601E-16,
1.)) ;
#39099 = DIRECTION('ref_axis',(1.75658099177411E-13,1.,1.66321791206623E-16)) ;
#39100 = DIRECTION('',(-0.866025403784439,-0.5,3.92513354304904E-14)) ;
#39101 = DIRECTION('',(1.36574054430667E-16,-1.,-1.66321791214607E-16)) ;
#39102 = DIRECTION('',(0.866025403784438,-0.5,-3.9417657221705E-14)) ;
#39103 = DIRECTION('',(0.866025403784438,0.5,-3.92513354304904E-14)) ;
#39104 = DIRECTION('',(-1.58057336172267E-29,1.,1.66321791214601E-16)) ;
#39105 = DIRECTION('',(-0.866025403784439,0.5,3.9417657221705E-14)) ;
#39106 = DIRECTION('',(-0.866025403784439,-0.5,3.92513354304904E-14)) ;
#39107 = DIRECTION('',(8.10629031994341E-17,-1.,-1.66321791214605E-16)) ;
#39108 = DIRECTION('',(0.866025403784438,-0.5,-3.9417657221705E-14)) ;
#39109 = DIRECTION('',(0.866025403784438,0.5,-3.92513354304904E-14)) ;
#39110 = DIRECTION('',(5.55111512312168E-17,1.,1.66321791214598E-16)) ;
#39111 = DIRECTION('',(-0.866025403784439,0.5,3.9417657221705E-14)) ;
#39112 = DIRECTION('',(-0.866025403784439,-0.5,3.92513354304904E-14)) ;
#39113 = DIRECTION('',(1.36574054430641E-16,-1.,-1.66321791214607E-16)) ;
#39114 = DIRECTION('',(0.866025403784438,-0.5,-3.9417657221705E-14)) ;
#39115 = DIRECTION('',(0.866025403784438,0.5,-3.92513354304904E-14)) ;
#39116 = DIRECTION('',(9.43781534984571E-30,1.,1.66321791214601E-16)) ;
#39117 = DIRECTION('',(-0.866025403784439,0.5,3.9417657221705E-14)) ;
#39118 = DIRECTION('center_axis',(-0.5,-0.866025403784439,-7.35195579201608E-14)) ;
#39119 = DIRECTION('ref_axis',(0.866025403784439,-0.5,-4.25106353121199E-14)) ;
#39120 = DIRECTION('',(0.866025403784439,-0.5,-3.9417657221705E-14)) ;
#39121 = DIRECTION('',(-5.55111512312578E-17,8.49251224899206E-14,-1.)) ;
#39122 = DIRECTION('',(-5.55111512312578E-17,8.49251224899206E-14,-1.)) ;
#39123 = DIRECTION('center_axis',(-1.,0.,5.55111512312578E-17)) ;
#39124 = DIRECTION('ref_axis',(-4.71429131787108E-30,-1.,-8.49251224899206E-14)) ;
#39125 = DIRECTION('',(-9.2327141051674E-33,-1.,-1.66321791214601E-16)) ;
#39126 = DIRECTION('',(-5.55111512312578E-17,8.49251224899206E-14,-1.)) ;
#39127 = DIRECTION('center_axis',(0.5,-0.866025403784439,-7.3575069071392E-14)) ;
#39128 = DIRECTION('ref_axis',(0.866025403784439,0.5,4.24144871778007E-14)) ;
#39129 = DIRECTION('',(0.866025403784439,0.5,-3.92513354304904E-14)) ;
#39130 = DIRECTION('',(-5.55111512312578E-17,8.49251224899206E-14,-1.)) ;
#39131 = DIRECTION('center_axis',(1.,1.36574054430651E-16,-5.55111512312462E-17)) ;
#39132 = DIRECTION('ref_axis',(-1.36574054430646E-16,1.,8.49251224899206E-14)) ;
#39133 = DIRECTION('',(-1.36574054430651E-16,1.,1.66321791214607E-16)) ;
#39134 = DIRECTION('',(-5.55111512312578E-17,8.49251224899206E-14,-1.)) ;
#39135 = DIRECTION('center_axis',(0.5,0.866025403784439,7.35195579201608E-14)) ;
#39136 = DIRECTION('ref_axis',(-0.866025403784439,0.5,4.25106353121199E-14)) ;
#39137 = DIRECTION('',(-0.866025403784438,0.5,3.9417657221705E-14)) ;
#39138 = DIRECTION('',(-5.55111512312578E-17,8.49251224899206E-14,-1.)) ;
#39139 = DIRECTION('center_axis',(-0.5,0.866025403784438,7.3575069071392E-14)) ;
#39140 = DIRECTION('ref_axis',(-0.866025403784438,-0.5,-4.24144871778007E-14)) ;
#39141 = DIRECTION('',(-0.866025403784438,-0.5,3.92513354304904E-14)) ;
#39142 = DIRECTION('center_axis',(-0.5,-0.866025403784439,-7.35195579201539E-14)) ;
#39143 = DIRECTION('ref_axis',(0.866025403784439,-0.5,-4.25106353121159E-14)) ;
#39144 = DIRECTION('',(0.866025403784439,-0.5,-3.9417657221705E-14)) ;
#39145 = DIRECTION('',(-5.55111512312187E-17,8.49251224899126E-14,-1.)) ;
#39146 = DIRECTION('',(-5.55111512312187E-17,8.49251224899127E-14,-1.)) ;
#39147 = DIRECTION('center_axis',(-1.,-2.52435489670719E-29,5.55111512312187E-17)) ;
#39148 = DIRECTION('ref_axis',(2.05292576492046E-29,-1.,-8.49251224899126E-14)) ;
#39149 = DIRECTION('',(2.52343162529668E-29,-1.,-1.66321791214601E-16)) ;
#39150 = DIRECTION('',(-5.55111512312187E-17,8.49251224899127E-14,-1.)) ;
#39151 = DIRECTION('center_axis',(0.5,-0.866025403784439,-7.35750690713851E-14)) ;
#39152 = DIRECTION('ref_axis',(0.866025403784439,0.5,4.24144871777968E-14)) ;
#39153 = DIRECTION('',(0.866025403784439,0.5,-3.92513354304904E-14)) ;
#39154 = DIRECTION('',(-5.55111512312187E-17,8.49251224899127E-14,-1.)) ;
#39155 = DIRECTION('center_axis',(1.,1.36574054430676E-16,-5.55111512312071E-17)) ;
#39156 = DIRECTION('ref_axis',(-1.36574054430671E-16,1.,8.49251224899126E-14)) ;
#39157 = DIRECTION('',(-1.36574054430676E-16,1.,1.66321791214607E-16)) ;
#39158 = DIRECTION('',(-5.55111512312187E-17,8.49251224899127E-14,-1.)) ;
#39159 = DIRECTION('center_axis',(0.5,0.866025403784439,7.35195579201539E-14)) ;
#39160 = DIRECTION('ref_axis',(-0.866025403784439,0.5,4.25106353121159E-14)) ;
#39161 = DIRECTION('',(-0.866025403784438,0.5,3.9417657221705E-14)) ;
#39162 = DIRECTION('',(-5.55111512312187E-17,8.49251224899126E-14,-1.)) ;
#39163 = DIRECTION('center_axis',(-0.5,0.866025403784438,7.35750690713851E-14)) ;
#39164 = DIRECTION('ref_axis',(-0.866025403784438,-0.5,-4.24144871777968E-14)) ;
#39165 = DIRECTION('',(-0.866025403784438,-0.5,3.92513354304904E-14)) ;
#39166 = DIRECTION('center_axis',(4.54195640846217E-14,-1.66321791214601E-16,
1.)) ;
#39167 = DIRECTION('ref_axis',(1.75658099177411E-13,1.,1.66321791206623E-16)) ;
#39168 = DIRECTION('',(0.866025403784439,0.5,-3.92513354304904E-14)) ;
#39169 = DIRECTION('',(0.866025403784439,-0.5,-3.9417657221705E-14)) ;
#39170 = DIRECTION('',(-5.55111512312074E-17,-1.,-1.66321791214598E-16)) ;
#39171 = DIRECTION('',(-0.866025403784438,-0.5,3.92513354304904E-14)) ;
#39172 = DIRECTION('',(-0.866025403784438,0.5,3.9417657221705E-14)) ;
#39173 = DIRECTION('',(-8.10629031994436E-17,1.,1.66321791214605E-16)) ;
#39174 = DIRECTION('center_axis',(-0.5,-0.866025403784439,-7.34978569193033E-14)) ;
#39175 = DIRECTION('ref_axis',(0.866025403784439,-0.5,-4.2499867027259E-14)) ;
#39176 = DIRECTION('',(-5.70360434152559E-17,8.490094472946E-14,-1.)) ;
#39177 = DIRECTION('',(-5.70360434152559E-17,8.490094472946E-14,-1.)) ;
#39178 = DIRECTION('center_axis',(-1.,5.55111512312073E-17,5.70360434152606E-17)) ;
#39179 = DIRECTION('ref_axis',(-5.55111512312121E-17,-1.,-8.490094472946E-14)) ;
#39180 = DIRECTION('',(-5.70360434152559E-17,8.490094472946E-14,-1.)) ;
#39181 = DIRECTION('center_axis',(0.5,-0.866025403784439,-7.35548929627185E-14)) ;
#39182 = DIRECTION('ref_axis',(0.866025403784439,0.5,4.2401077702201E-14)) ;
#39183 = DIRECTION('',(-5.70360434152559E-17,8.490094472946E-14,-1.)) ;
#39184 = DIRECTION('center_axis',(1.,8.10629031994436E-17,-5.7036043415249E-17)) ;
#39185 = DIRECTION('ref_axis',(-8.10629031994388E-17,1.,8.490094472946E-14)) ;
#39186 = DIRECTION('',(-5.70360434152559E-17,8.490094472946E-14,-1.)) ;
#39187 = DIRECTION('center_axis',(0.5,0.866025403784439,7.34978569193033E-14)) ;
#39188 = DIRECTION('ref_axis',(-0.866025403784439,0.5,4.2499867027259E-14)) ;
#39189 = DIRECTION('',(-5.70360434152559E-17,8.490094472946E-14,-1.)) ;
#39190 = DIRECTION('center_axis',(-0.5,0.866025403784438,7.35548929627185E-14)) ;
#39191 = DIRECTION('ref_axis',(-0.866025403784438,-0.5,-4.24010777022011E-14)) ;
#39192 = DIRECTION('',(0.,0.,1.)) ;
#39193 = DIRECTION('',(1.,0.,0.)) ;
#39194 = DIRECTION('',(0.,0.,1.)) ;
#39195 = DIRECTION('',(1.,0.,0.)) ;
#39196 = DIRECTION('',(0.,0.,1.)) ;
#39197 = DIRECTION('',(1.,0.,0.)) ;
#39198 = DIRECTION('',(0.,0.,1.)) ;
#39199 = DIRECTION('',(1.,0.,0.)) ;
#39200 = DIRECTION('axis',(0.,0.,1.)) ;
#39201 = DIRECTION('refdir',(1.,0.,0.)) ;
#39202 = DIRECTION('axis',(0.,0.,1.)) ;
#39203 = DIRECTION('refdir',(1.,0.,0.)) ;
#39204 = DIRECTION('axis',(0.,0.,1.)) ;
#39205 = DIRECTION('refdir',(1.,0.,0.)) ;
#39206 = DIRECTION('center_axis',(4.58892183511729E-14,-7.97041684978857E-27,
1.)) ;
#39207 = DIRECTION('ref_axis',(-1.73688224296914E-13,-1.,1.14794370197489E-41)) ;
#39208 = DIRECTION('',(-1.73688224296914E-13,-1.,0.)) ;
#39209 = DIRECTION('',(1.,-1.6579330501069E-13,-4.58892183511729E-14)) ;
#39210 = DIRECTION('',(-1.73688224296914E-13,-1.,3.58732406867123E-43)) ;
#39211 = DIRECTION('',(1.,-1.6579330501069E-13,-4.58892183511729E-14)) ;
#39212 = DIRECTION('center_axis',(1.6579330501069E-13,1.,3.5839606558192E-28)) ;
#39213 = DIRECTION('ref_axis',(4.53957858957841E-14,-7.88471344280163E-27,
1.)) ;
#39214 = DIRECTION('',(4.53957858957841E-14,-7.88471344280162E-27,1.)) ;
#39215 = DIRECTION('',(-1.,1.6579330501069E-13,4.54195640846217E-14)) ;
#39216 = DIRECTION('',(4.53957858957841E-14,-7.88471344280162E-27,1.)) ;
#39217 = DIRECTION('center_axis',(-1.6579330501069E-13,-1.,-3.43824445941423E-28)) ;
#39218 = DIRECTION('ref_axis',(-4.35500900612589E-14,7.56413781071074E-27,
-1.)) ;
#39219 = DIRECTION('',(-4.53957858957841E-14,7.87014182316113E-27,-1.)) ;
#39220 = DIRECTION('',(-4.35500900612589E-14,7.56413781071072E-27,-1.)) ;
#39221 = DIRECTION('',(1.,-1.6579330501069E-13,-4.54195640846217E-14)) ;
#39222 = DIRECTION('center_axis',(1.,-1.6579330501069E-13,-4.58892183511729E-14)) ;
#39223 = DIRECTION('ref_axis',(-4.58892183511729E-14,-2.00890147845606E-41,
-1.)) ;
#39224 = DIRECTION('',(1.6579330501069E-13,1.,1.66321791207071E-16)) ;
#39225 = DIRECTION('center_axis',(4.58892183511729E-14,-7.97041684978857E-27,
1.)) ;
#39226 = DIRECTION('ref_axis',(-1.73688224296914E-13,-1.,1.14794370197489E-41)) ;
#39227 = DIRECTION('',(-1.73688224296914E-13,-1.,0.)) ;
#39228 = DIRECTION('',(1.,-1.6579330501069E-13,-4.58892183511729E-14)) ;
#39229 = DIRECTION('',(-1.73688224296914E-13,-1.,3.58732406867123E-43)) ;
#39230 = DIRECTION('',(1.,-1.6579330501069E-13,-4.58892183511729E-14)) ;
#39231 = DIRECTION('center_axis',(1.6579330501069E-13,1.,3.5839606558192E-28)) ;
#39232 = DIRECTION('ref_axis',(4.53957858957841E-14,-7.88471344280163E-27,
1.)) ;
#39233 = DIRECTION('',(4.53957858957841E-14,-7.88471344280162E-27,1.)) ;
#39234 = DIRECTION('',(-1.,1.6579330501069E-13,4.54195640846217E-14)) ;
#39235 = DIRECTION('',(4.53957858957841E-14,-7.88471344280162E-27,1.)) ;
#39236 = DIRECTION('center_axis',(-1.6579330501069E-13,-1.,-3.43824445941423E-28)) ;
#39237 = DIRECTION('ref_axis',(-4.35500900612589E-14,7.56413781071074E-27,
-1.)) ;
#39238 = DIRECTION('',(-4.53957858957841E-14,7.87014182316113E-27,-1.)) ;
#39239 = DIRECTION('',(-4.35500900612589E-14,7.56413781071072E-27,-1.)) ;
#39240 = DIRECTION('',(1.,-1.6579330501069E-13,-4.54195640846217E-14)) ;
#39241 = DIRECTION('center_axis',(1.,-1.6579330501069E-13,-4.58892183511729E-14)) ;
#39242 = DIRECTION('ref_axis',(-4.58892183511729E-14,-2.00890147845606E-41,
-1.)) ;
#39243 = DIRECTION('',(1.6579330501069E-13,1.,1.66321791207071E-16)) ;
#39244 = DIRECTION('center_axis',(-1.6579330501069E-13,-1.,-3.43824445941423E-28)) ;
#39245 = DIRECTION('ref_axis',(-4.35500900612589E-14,7.56413781071074E-27,
-1.)) ;
#39246 = DIRECTION('',(-4.53957858957841E-14,7.87014182316113E-27,-1.)) ;
#39247 = DIRECTION('',(1.,-1.6579330501069E-13,-4.4408920985006E-14)) ;
#39248 = DIRECTION('',(-4.35500900612589E-14,7.56413781071072E-27,-1.)) ;
#39249 = DIRECTION('',(1.,-1.6579330501069E-13,-4.54195640846217E-14)) ;
#39250 = DIRECTION('center_axis',(4.4408920985006E-14,-7.71330662882764E-27,
1.)) ;
#39251 = DIRECTION('ref_axis',(-1.73688224296914E-13,-1.,1.29143666472175E-41)) ;
#39252 = DIRECTION('',(-1.73688224296914E-13,-1.,1.43492962746861E-42)) ;
#39253 = DIRECTION('',(1.,-1.6579330501069E-13,-4.4408920985006E-14)) ;
#39254 = DIRECTION('',(-1.73688224296914E-13,-1.,3.58732406867123E-43)) ;
#39255 = DIRECTION('center_axis',(1.6579330501069E-13,1.,3.5839606558192E-28)) ;
#39256 = DIRECTION('ref_axis',(4.53957858957841E-14,-7.88471344280163E-27,
1.)) ;
#39257 = DIRECTION('',(4.53957858957841E-14,-7.88471344280162E-27,1.)) ;
#39258 = DIRECTION('',(-1.,1.6579330501069E-13,4.54195640846217E-14)) ;
#39259 = DIRECTION('',(4.53957858957841E-14,-7.88471344280162E-27,1.)) ;
#39260 = DIRECTION('center_axis',(1.,-1.6579330501069E-13,-4.4408920985006E-14)) ;
#39261 = DIRECTION('ref_axis',(-4.4408920985006E-14,-2.00890147845606E-41,
-1.)) ;
#39262 = DIRECTION('',(1.6579330501069E-13,1.,1.66321791207071E-16)) ;
#39263 = DIRECTION('center_axis',(4.58892183511729E-14,-7.97041684978857E-27,
1.)) ;
#39264 = DIRECTION('ref_axis',(-1.73688224296914E-13,-1.,1.14794370197489E-41)) ;
#39265 = DIRECTION('',(-1.73688224296914E-13,-1.,0.)) ;
#39266 = DIRECTION('',(1.,-1.6579330501069E-13,-4.58892183511729E-14)) ;
#39267 = DIRECTION('',(-1.73688224296914E-13,-1.,3.58732406867123E-43)) ;
#39268 = DIRECTION('',(1.,-1.6579330501069E-13,-4.58892183511729E-14)) ;
#39269 = DIRECTION('center_axis',(1.6579330501069E-13,1.,3.5839606558192E-28)) ;
#39270 = DIRECTION('ref_axis',(4.53957858957841E-14,-7.88471344280163E-27,
1.)) ;
#39271 = DIRECTION('',(4.53957858957841E-14,-7.88471344280162E-27,1.)) ;
#39272 = DIRECTION('',(-1.,1.6579330501069E-13,4.54195640846217E-14)) ;
#39273 = DIRECTION('',(4.53957858957841E-14,-7.88471344280162E-27,1.)) ;
#39274 = DIRECTION('center_axis',(-1.6579330501069E-13,-1.,-3.43824445941423E-28)) ;
#39275 = DIRECTION('ref_axis',(-4.35500900612589E-14,7.56413781071074E-27,
-1.)) ;
#39276 = DIRECTION('',(-4.53957858957841E-14,7.87014182316113E-27,-1.)) ;
#39277 = DIRECTION('',(-4.35500900612589E-14,7.56413781071072E-27,-1.)) ;
#39278 = DIRECTION('',(1.,-1.6579330501069E-13,-4.54195640846217E-14)) ;
#39279 = DIRECTION('center_axis',(1.,-1.6579330501069E-13,-4.58892183511729E-14)) ;
#39280 = DIRECTION('ref_axis',(-4.58892183511729E-14,-2.00890147845606E-41,
-1.)) ;
#39281 = DIRECTION('',(1.6579330501069E-13,1.,1.66321791207071E-16)) ;
#39282 = DIRECTION('center_axis',(4.58892183511729E-14,-7.97041684978857E-27,
1.)) ;
#39283 = DIRECTION('ref_axis',(-1.73688224296914E-13,-1.,1.14794370197489E-41)) ;
#39284 = DIRECTION('',(-1.73688224296914E-13,-1.,0.)) ;
#39285 = DIRECTION('',(1.,-1.6579330501069E-13,-4.58892183511729E-14)) ;
#39286 = DIRECTION('',(-1.73688224296914E-13,-1.,3.58732406867123E-43)) ;
#39287 = DIRECTION('',(1.,-1.6579330501069E-13,-4.58892183511729E-14)) ;
#39288 = DIRECTION('center_axis',(1.6579330501069E-13,1.,3.5839606558192E-28)) ;
#39289 = DIRECTION('ref_axis',(4.53957858957841E-14,-7.88471344280163E-27,
1.)) ;
#39290 = DIRECTION('',(4.53957858957841E-14,-7.88471344280162E-27,1.)) ;
#39291 = DIRECTION('',(-1.,1.6579330501069E-13,4.54195640846217E-14)) ;
#39292 = DIRECTION('',(4.53957858957841E-14,-7.88471344280162E-27,1.)) ;
#39293 = DIRECTION('center_axis',(-1.6579330501069E-13,-1.,-3.43824445941423E-28)) ;
#39294 = DIRECTION('ref_axis',(-4.35500900612589E-14,7.56413781071074E-27,
-1.)) ;
#39295 = DIRECTION('',(-4.53957858957841E-14,7.87014182316113E-27,-1.)) ;
#39296 = DIRECTION('',(-4.35500900612589E-14,7.56413781071072E-27,-1.)) ;
#39297 = DIRECTION('',(1.,-1.6579330501069E-13,-4.54195640846217E-14)) ;
#39298 = DIRECTION('center_axis',(1.,-1.6579330501069E-13,-4.58892183511729E-14)) ;
#39299 = DIRECTION('ref_axis',(-4.58892183511729E-14,-2.00890147845606E-41,
-1.)) ;
#39300 = DIRECTION('',(1.6579330501069E-13,1.,1.66321791207071E-16)) ;
#39301 = DIRECTION('center_axis',(4.58892183511729E-14,-7.97041684978857E-27,
1.)) ;
#39302 = DIRECTION('ref_axis',(-1.73688224296914E-13,-1.,1.14794370197489E-41)) ;
#39303 = DIRECTION('',(-1.73688224296914E-13,-1.,0.)) ;
#39304 = DIRECTION('',(1.,-1.6579330501069E-13,-4.58892183511729E-14)) ;
#39305 = DIRECTION('',(-1.73688224296914E-13,-1.,3.58732406867123E-43)) ;
#39306 = DIRECTION('',(1.,-1.6579330501069E-13,-4.58892183511729E-14)) ;
#39307 = DIRECTION('center_axis',(1.6579330501069E-13,1.,3.5839606558192E-28)) ;
#39308 = DIRECTION('ref_axis',(4.53957858957841E-14,-7.88471344280163E-27,
1.)) ;
#39309 = DIRECTION('',(4.53957858957841E-14,-7.88471344280162E-27,1.)) ;
#39310 = DIRECTION('',(-1.,1.6579330501069E-13,4.54195640846217E-14)) ;
#39311 = DIRECTION('',(4.53957858957841E-14,-7.88471344280162E-27,1.)) ;
#39312 = DIRECTION('center_axis',(-1.6579330501069E-13,-1.,-3.43824445941423E-28)) ;
#39313 = DIRECTION('ref_axis',(-4.35500900612589E-14,7.56413781071074E-27,
-1.)) ;
#39314 = DIRECTION('',(-4.53957858957841E-14,7.87014182316113E-27,-1.)) ;
#39315 = DIRECTION('',(-4.35500900612589E-14,7.56413781071072E-27,-1.)) ;
#39316 = DIRECTION('',(1.,-1.6579330501069E-13,-4.54195640846217E-14)) ;
#39317 = DIRECTION('center_axis',(1.,-1.6579330501069E-13,-4.58892183511729E-14)) ;
#39318 = DIRECTION('ref_axis',(-4.58892183511729E-14,-2.00890147845606E-41,
-1.)) ;
#39319 = DIRECTION('',(1.6579330501069E-13,1.,1.66321791207071E-16)) ;
#39320 = DIRECTION('center_axis',(-1.6579330501069E-13,-1.,-3.43824445941423E-28)) ;
#39321 = DIRECTION('ref_axis',(-4.35500900612589E-14,7.56413781071074E-27,
-1.)) ;
#39322 = DIRECTION('',(-4.53957858957841E-14,7.87014182316113E-27,-1.)) ;
#39323 = DIRECTION('',(1.,-1.6579330501069E-13,-4.4408920985006E-14)) ;
#39324 = DIRECTION('',(-4.35500900612589E-14,7.56413781071072E-27,-1.)) ;
#39325 = DIRECTION('',(1.,-1.6579330501069E-13,-4.54195640846217E-14)) ;
#39326 = DIRECTION('center_axis',(4.4408920985006E-14,-7.71330662882764E-27,
1.)) ;
#39327 = DIRECTION('ref_axis',(-1.73688224296914E-13,-1.,1.29143666472175E-41)) ;
#39328 = DIRECTION('',(-1.73688224296914E-13,-1.,1.43492962746861E-42)) ;
#39329 = DIRECTION('',(1.,-1.6579330501069E-13,-4.4408920985006E-14)) ;
#39330 = DIRECTION('',(-1.73688224296914E-13,-1.,3.58732406867123E-43)) ;
#39331 = DIRECTION('center_axis',(1.6579330501069E-13,1.,3.5839606558192E-28)) ;
#39332 = DIRECTION('ref_axis',(4.53957858957841E-14,-7.88471344280163E-27,
1.)) ;
#39333 = DIRECTION('',(4.53957858957841E-14,-7.88471344280162E-27,1.)) ;
#39334 = DIRECTION('',(-1.,1.6579330501069E-13,4.54195640846217E-14)) ;
#39335 = DIRECTION('',(4.53957858957841E-14,-7.88471344280162E-27,1.)) ;
#39336 = DIRECTION('center_axis',(1.,-1.6579330501069E-13,-4.4408920985006E-14)) ;
#39337 = DIRECTION('ref_axis',(-4.4408920985006E-14,-2.00890147845606E-41,
-1.)) ;
#39338 = DIRECTION('',(1.6579330501069E-13,1.,1.66321791207071E-16)) ;
#39339 = DIRECTION('center_axis',(4.58892183511729E-14,-7.97041684978857E-27,
1.)) ;
#39340 = DIRECTION('ref_axis',(-1.73688224296914E-13,-1.,1.14794370197489E-41)) ;
#39341 = DIRECTION('',(-1.73688224296914E-13,-1.,0.)) ;
#39342 = DIRECTION('',(1.,-1.6579330501069E-13,-4.58892183511729E-14)) ;
#39343 = DIRECTION('',(-1.73688224296914E-13,-1.,3.58732406867123E-43)) ;
#39344 = DIRECTION('',(1.,-1.6579330501069E-13,-4.58892183511729E-14)) ;
#39345 = DIRECTION('center_axis',(1.6579330501069E-13,1.,3.5839606558192E-28)) ;
#39346 = DIRECTION('ref_axis',(4.53957858957841E-14,-7.88471344280163E-27,
1.)) ;
#39347 = DIRECTION('',(4.53957858957841E-14,-7.88471344280162E-27,1.)) ;
#39348 = DIRECTION('',(-1.,1.6579330501069E-13,4.54195640846217E-14)) ;
#39349 = DIRECTION('',(4.53957858957841E-14,-7.88471344280162E-27,1.)) ;
#39350 = DIRECTION('center_axis',(-1.6579330501069E-13,-1.,-3.43824445941423E-28)) ;
#39351 = DIRECTION('ref_axis',(-4.35500900612589E-14,7.56413781071074E-27,
-1.)) ;
#39352 = DIRECTION('',(-4.53957858957841E-14,7.87014182316113E-27,-1.)) ;
#39353 = DIRECTION('',(-4.35500900612589E-14,7.56413781071072E-27,-1.)) ;
#39354 = DIRECTION('',(1.,-1.6579330501069E-13,-4.54195640846217E-14)) ;
#39355 = DIRECTION('center_axis',(1.,-1.6579330501069E-13,-4.58892183511729E-14)) ;
#39356 = DIRECTION('ref_axis',(-4.58892183511729E-14,-2.00890147845606E-41,
-1.)) ;
#39357 = DIRECTION('',(1.6579330501069E-13,1.,1.66321791207071E-16)) ;
#39358 = DIRECTION('center_axis',(4.58892183511729E-14,-7.97041684978857E-27,
1.)) ;
#39359 = DIRECTION('ref_axis',(-1.73688224296914E-13,-1.,1.14794370197489E-41)) ;
#39360 = DIRECTION('',(-1.73688224296914E-13,-1.,0.)) ;
#39361 = DIRECTION('',(1.,-1.6579330501069E-13,-4.58892183511729E-14)) ;
#39362 = DIRECTION('',(-1.73688224296914E-13,-1.,3.58732406867123E-43)) ;
#39363 = DIRECTION('',(1.,-1.6579330501069E-13,-4.58892183511729E-14)) ;
#39364 = DIRECTION('center_axis',(1.6579330501069E-13,1.,3.5839606558192E-28)) ;
#39365 = DIRECTION('ref_axis',(4.53957858957841E-14,-7.88471344280163E-27,
1.)) ;
#39366 = DIRECTION('',(4.53957858957841E-14,-7.88471344280162E-27,1.)) ;
#39367 = DIRECTION('',(-1.,1.6579330501069E-13,4.54195640846217E-14)) ;
#39368 = DIRECTION('',(4.53957858957841E-14,-7.88471344280162E-27,1.)) ;
#39369 = DIRECTION('center_axis',(-1.6579330501069E-13,-1.,-3.43824445941423E-28)) ;
#39370 = DIRECTION('ref_axis',(-4.35500900612589E-14,7.56413781071074E-27,
-1.)) ;
#39371 = DIRECTION('',(-4.53957858957841E-14,7.87014182316113E-27,-1.)) ;
#39372 = DIRECTION('',(-4.35500900612589E-14,7.56413781071072E-27,-1.)) ;
#39373 = DIRECTION('',(1.,-1.6579330501069E-13,-4.54195640846217E-14)) ;
#39374 = DIRECTION('center_axis',(1.,-1.6579330501069E-13,-4.58892183511729E-14)) ;
#39375 = DIRECTION('ref_axis',(-4.58892183511729E-14,-2.00890147845606E-41,
-1.)) ;
#39376 = DIRECTION('',(1.6579330501069E-13,1.,1.66321791207071E-16)) ;
#39377 = DIRECTION('center_axis',(-4.54195640846217E-14,1.66321791214601E-16,
-1.)) ;
#39378 = DIRECTION('ref_axis',(-1.,1.75658099177411E-13,4.54195640846217E-14)) ;
#39379 = DIRECTION('',(-1.75658099177411E-13,-1.,-6.12002098060108E-16)) ;
#39380 = DIRECTION('',(-1.75658099177411E-13,-1.,-6.12002098060108E-16)) ;
#39381 = DIRECTION('',(-1.75658099177411E-13,-1.,-6.12002098060108E-16)) ;
#39382 = DIRECTION('',(-1.75658099177411E-13,-1.,-6.12002098060108E-16)) ;
#39383 = DIRECTION('',(-1.75658099177411E-13,-1.,-6.12002098060108E-16)) ;
#39384 = DIRECTION('',(-1.75658099177411E-13,-1.,-6.12002098060108E-16)) ;
#39385 = DIRECTION('',(-1.75658099177411E-13,-1.,-6.12002098060108E-16)) ;
#39386 = DIRECTION('',(-1.,1.75658099177411E-13,4.54195640846217E-14)) ;
#39387 = DIRECTION('',(-1.75658099177411E-13,-1.,-1.66321791206623E-16)) ;
#39388 = DIRECTION('',(-1.,1.75658099177411E-13,4.54195640846217E-14)) ;
#39389 = DIRECTION('',(-1.75658099177411E-13,-1.,-6.12002098060108E-16)) ;
#39390 = DIRECTION('',(1.,-1.75658099177411E-13,-4.54195640846217E-14)) ;
#39391 = DIRECTION('',(-1.75658099177411E-13,-1.,-1.66321791206623E-16)) ;
#39392 = DIRECTION('',(-1.,1.75658099177411E-13,4.54195640846217E-14)) ;
#39393 = DIRECTION('',(-1.75658099177411E-13,-1.,-6.12002098060108E-16)) ;
#39394 = DIRECTION('',(1.,-1.75658099177411E-13,-4.54195640846217E-14)) ;
#39395 = DIRECTION('',(-1.75658099177411E-13,-1.,-1.66321791206623E-16)) ;
#39396 = DIRECTION('',(-1.,1.75658099177411E-13,4.54195640846217E-14)) ;
#39397 = DIRECTION('',(-1.75658099177411E-13,-1.,-6.12002098060108E-16)) ;
#39398 = DIRECTION('',(1.,-1.75658099177411E-13,-4.54195640846217E-14)) ;
#39399 = DIRECTION('',(-1.75658099177411E-13,-1.,-1.66321791206623E-16)) ;
#39400 = DIRECTION('',(-1.,1.75658099177411E-13,4.54195640846217E-14)) ;
#39401 = DIRECTION('',(-1.75658099177411E-13,-1.,-6.12002098060108E-16)) ;
#39402 = DIRECTION('',(1.,-1.75658099177411E-13,-4.54195640846217E-14)) ;
#39403 = DIRECTION('',(-1.75658099177411E-13,-1.,-1.66321791206623E-16)) ;
#39404 = DIRECTION('',(-1.,1.75658099177411E-13,4.54195640846217E-14)) ;
#39405 = DIRECTION('',(-1.75658099177411E-13,-1.,-6.12002098060108E-16)) ;
#39406 = DIRECTION('',(1.,-1.75658099177411E-13,-4.54195640846217E-14)) ;
#39407 = DIRECTION('',(-1.75658099177411E-13,-1.,-1.66321791206623E-16)) ;
#39408 = DIRECTION('',(-1.,1.75658099177411E-13,4.54195640846217E-14)) ;
#39409 = DIRECTION('',(-1.75658099177411E-13,-1.,-6.12002098060108E-16)) ;
#39410 = DIRECTION('',(1.,-1.75658099177411E-13,-4.54195640846217E-14)) ;
#39411 = DIRECTION('',(-1.75658099177411E-13,-1.,-1.66321791206623E-16)) ;
#39412 = DIRECTION('',(-1.,1.75658099177411E-13,4.54195640846217E-14)) ;
#39413 = DIRECTION('',(-1.75658099177411E-13,-1.,-6.12002098060108E-16)) ;
#39414 = DIRECTION('',(1.,-1.75658099177411E-13,-4.54195640846217E-14)) ;
#39415 = DIRECTION('',(-1.75658099177411E-13,-1.,-1.66321791206623E-16)) ;
#39416 = DIRECTION('',(-1.,1.75658099177411E-13,4.54195640846217E-14)) ;
#39417 = DIRECTION('',(-1.75658099177411E-13,-1.,-6.12002098060108E-16)) ;
#39418 = DIRECTION('',(1.,-1.75658099177411E-13,-4.54195640846217E-14)) ;
#39419 = DIRECTION('',(-1.75658099177411E-13,-1.,-1.66321791206623E-16)) ;
#39420 = DIRECTION('',(-1.,1.75658099177411E-13,4.54195640846217E-14)) ;
#39421 = DIRECTION('',(-1.75658099177411E-13,-1.,-6.12002098060108E-16)) ;
#39422 = DIRECTION('',(1.,-1.75658099177411E-13,-4.54195640846217E-14)) ;
#39423 = DIRECTION('',(-1.75658099177411E-13,-1.,-1.66321791206623E-16)) ;
#39424 = DIRECTION('',(-1.,1.73688224296914E-13,4.53957858957841E-14)) ;
#39425 = DIRECTION('',(-1.75658099177411E-13,-1.,-6.12002098060108E-16)) ;
#39426 = DIRECTION('',(-1.75658099177411E-13,-1.,-6.12002098060108E-16)) ;
#39427 = DIRECTION('',(-1.75658099177411E-13,-1.,-6.12002098060108E-16)) ;
#39428 = DIRECTION('center_axis',(-4.54195640846217E-14,1.66321791214601E-16,
-1.)) ;
#39429 = DIRECTION('ref_axis',(-1.,0.,4.46626862477777E-14)) ;
#39430 = DIRECTION('center_axis',(4.54195640846217E-14,-1.66321791214601E-16,
1.)) ;
#39431 = DIRECTION('ref_axis',(-1.,1.8946420272009E-13,4.54195640846217E-14)) ;
#39432 = DIRECTION('center_axis',(-7.59720474939486E-30,-1.,-1.66321791214601E-16)) ;
#39433 = DIRECTION('ref_axis',(1.,0.,-4.56777472988634E-14)) ;
#39434 = DIRECTION('center_axis',(-4.54195640846217E-14,1.66321791214601E-16,
-1.)) ;
#39435 = DIRECTION('ref_axis',(-1.,1.8946420272009E-13,4.54195640846217E-14)) ;
#39436 = DIRECTION('center_axis',(-4.54195640846217E-14,1.66321791214601E-16,
-1.)) ;
#39437 = DIRECTION('ref_axis',(-1.,1.75658099177411E-13,4.54195640846217E-14)) ;
#39438 = DIRECTION('center_axis',(-2.1716102378779E-15,3.83815143260386E-28,
1.)) ;
#39439 = DIRECTION('ref_axis',(-1.,1.75658099177411E-13,-2.1716102378779E-15)) ;
#39440 = DIRECTION('',(-4.54195640846217E-14,1.66321791214601E-16,-1.)) ;
#39441 = DIRECTION('center_axis',(-4.54195640846217E-14,1.66321791214601E-16,
-1.)) ;
#39442 = DIRECTION('ref_axis',(-1.,5.55236256206829E-46,4.54195640846217E-14)) ;
#39443 = DIRECTION('',(1.75658099177411E-13,1.,1.66321791206623E-16)) ;
#39444 = DIRECTION('',(1.,-1.75658099177411E-13,-4.54195640846217E-14)) ;
#39445 = DIRECTION('',(-1.75658099177411E-13,-1.,-1.66321791206623E-16)) ;
#39446 = DIRECTION('',(-1.,1.75658099177411E-13,4.54195640846217E-14)) ;
#39447 = DIRECTION('',(-1.,3.33066907386739E-16,4.54195640846217E-14)) ;
#39448 = DIRECTION('center_axis',(-4.54195640846217E-14,1.66321791214601E-16,
-1.)) ;
#39449 = DIRECTION('ref_axis',(1.,-5.55236256206829E-46,-4.54195640846217E-14)) ;
#39450 = DIRECTION('',(-8.32667268460786E-17,-1.,-1.66321791214597E-16)) ;
#39451 = DIRECTION('center_axis',(-4.54195640846217E-14,1.66321791214601E-16,
-1.)) ;
#39452 = DIRECTION('ref_axis',(1.,-5.55236256206829E-46,-4.54195640846217E-14)) ;
#39453 = DIRECTION('',(1.,-3.33066907386739E-16,-4.54195640846217E-14)) ;
#39454 = DIRECTION('center_axis',(-4.54195640846217E-14,1.66321791214601E-16,
-1.)) ;
#39455 = DIRECTION('ref_axis',(1.,-5.55236256206829E-46,-4.54195640846217E-14)) ;
#39456 = DIRECTION('',(1.66533453692965E-16,1.,1.66321791214593E-16)) ;
#39457 = DIRECTION('center_axis',(-4.54195640846217E-14,1.66321791214601E-16,
-1.)) ;
#39458 = DIRECTION('ref_axis',(1.,-5.55236256206829E-46,-4.54195640846217E-14)) ;
#39459 = DIRECTION('center_axis',(-4.54195640846217E-14,1.66321791214601E-16,
-1.)) ;
#39460 = DIRECTION('ref_axis',(-1.,0.,4.46626862477777E-14)) ;
#39461 = DIRECTION('center_axis',(4.54195640846217E-14,-1.66321791214601E-16,
1.)) ;
#39462 = DIRECTION('ref_axis',(-1.,1.8946420272009E-13,4.54195640846217E-14)) ;
#39463 = DIRECTION('center_axis',(-7.59720474939486E-30,-1.,-1.66321791214601E-16)) ;
#39464 = DIRECTION('ref_axis',(1.,0.,-4.56777472988634E-14)) ;
#39465 = DIRECTION('center_axis',(-4.54195640846217E-14,1.66321791214601E-16,
-1.)) ;
#39466 = DIRECTION('ref_axis',(-1.,1.8946420272009E-13,4.54195640846217E-14)) ;
#39467 = DIRECTION('center_axis',(-4.54195640846217E-14,1.66321791214601E-16,
-1.)) ;
#39468 = DIRECTION('ref_axis',(-1.,1.75658099177411E-13,4.54195640846217E-14)) ;
#39469 = DIRECTION('center_axis',(-2.1716102378779E-15,3.83815143260386E-28,
1.)) ;
#39470 = DIRECTION('ref_axis',(-1.,1.75658099177411E-13,-2.1716102378779E-15)) ;
#39471 = DIRECTION('',(-4.54195640846217E-14,1.66321791214601E-16,-1.)) ;
#39472 = DIRECTION('center_axis',(-4.54195640846217E-14,1.66321791214601E-16,
-1.)) ;
#39473 = DIRECTION('ref_axis',(-1.,5.55236256206829E-46,4.54195640846217E-14)) ;
#39474 = DIRECTION('',(1.75658099177411E-13,1.,1.66321791206623E-16)) ;
#39475 = DIRECTION('',(1.,-1.75658099177411E-13,-4.54195640846217E-14)) ;
#39476 = DIRECTION('',(-1.75658099177411E-13,-1.,-1.66321791206623E-16)) ;
#39477 = DIRECTION('',(-1.,1.75658099177411E-13,4.54195640846217E-14)) ;
#39478 = DIRECTION('',(-1.,3.33066907386739E-16,4.54195640846217E-14)) ;
#39479 = DIRECTION('center_axis',(-4.54195640846217E-14,1.66321791214601E-16,
-1.)) ;
#39480 = DIRECTION('ref_axis',(1.,-5.55236256206829E-46,-4.54195640846217E-14)) ;
#39481 = DIRECTION('',(-8.32667268460786E-17,-1.,-1.66321791214597E-16)) ;
#39482 = DIRECTION('center_axis',(-4.54195640846217E-14,1.66321791214601E-16,
-1.)) ;
#39483 = DIRECTION('ref_axis',(1.,-5.55236256206829E-46,-4.54195640846217E-14)) ;
#39484 = DIRECTION('',(1.,-3.33066907386739E-16,-4.54195640846217E-14)) ;
#39485 = DIRECTION('center_axis',(-4.54195640846217E-14,1.66321791214601E-16,
-1.)) ;
#39486 = DIRECTION('ref_axis',(1.,-5.55236256206829E-46,-4.54195640846217E-14)) ;
#39487 = DIRECTION('',(1.66533453692965E-16,1.,1.66321791214593E-16)) ;
#39488 = DIRECTION('center_axis',(-4.54195640846217E-14,1.66321791214601E-16,
-1.)) ;
#39489 = DIRECTION('ref_axis',(1.,-5.55236256206829E-46,-4.54195640846217E-14)) ;
#39490 = DIRECTION('center_axis',(-4.54195640846217E-14,1.66321791214601E-16,
-1.)) ;
#39491 = DIRECTION('ref_axis',(-1.,0.,4.46626862477777E-14)) ;
#39492 = DIRECTION('center_axis',(4.54195640846217E-14,-1.66321791214601E-16,
1.)) ;
#39493 = DIRECTION('ref_axis',(-1.,1.8946420272009E-13,4.54195640846217E-14)) ;
#39494 = DIRECTION('center_axis',(-7.59720474939486E-30,-1.,-1.66321791214601E-16)) ;
#39495 = DIRECTION('ref_axis',(1.,0.,-4.56777472988634E-14)) ;
#39496 = DIRECTION('center_axis',(-4.54195640846217E-14,1.66321791214601E-16,
-1.)) ;
#39497 = DIRECTION('ref_axis',(-1.,1.8946420272009E-13,4.54195640846217E-14)) ;
#39498 = DIRECTION('center_axis',(-4.54195640846217E-14,1.66321791214601E-16,
-1.)) ;
#39499 = DIRECTION('ref_axis',(-1.,1.75658099177411E-13,4.54195640846217E-14)) ;
#39500 = DIRECTION('center_axis',(-2.1716102378779E-15,3.83815143260386E-28,
1.)) ;
#39501 = DIRECTION('ref_axis',(-1.,1.75658099177411E-13,-2.1716102378779E-15)) ;
#39502 = DIRECTION('',(-4.54195640846217E-14,1.66321791214601E-16,-1.)) ;
#39503 = DIRECTION('center_axis',(-4.54195640846217E-14,1.66321791214601E-16,
-1.)) ;
#39504 = DIRECTION('ref_axis',(-1.,5.55236256206829E-46,4.54195640846217E-14)) ;
#39505 = DIRECTION('',(1.75658099177411E-13,1.,1.66321791206623E-16)) ;
#39506 = DIRECTION('',(1.,-1.75658099177411E-13,-4.54195640846217E-14)) ;
#39507 = DIRECTION('',(-1.75658099177411E-13,-1.,-1.66321791206623E-16)) ;
#39508 = DIRECTION('',(-1.,1.75658099177411E-13,4.54195640846217E-14)) ;
#39509 = DIRECTION('',(-1.,3.33066907386739E-16,4.54195640846217E-14)) ;
#39510 = DIRECTION('center_axis',(-4.54195640846217E-14,1.66321791214601E-16,
-1.)) ;
#39511 = DIRECTION('ref_axis',(1.,-5.55236256206829E-46,-4.54195640846217E-14)) ;
#39512 = DIRECTION('',(-8.32667268460786E-17,-1.,-1.66321791214597E-16)) ;
#39513 = DIRECTION('center_axis',(-4.54195640846217E-14,1.66321791214601E-16,
-1.)) ;
#39514 = DIRECTION('ref_axis',(1.,-5.55236256206829E-46,-4.54195640846217E-14)) ;
#39515 = DIRECTION('',(1.,-3.33066907386739E-16,-4.54195640846217E-14)) ;
#39516 = DIRECTION('center_axis',(-4.54195640846217E-14,1.66321791214601E-16,
-1.)) ;
#39517 = DIRECTION('ref_axis',(1.,-5.55236256206829E-46,-4.54195640846217E-14)) ;
#39518 = DIRECTION('',(1.66533453692965E-16,1.,1.66321791214593E-16)) ;
#39519 = DIRECTION('center_axis',(-4.54195640846217E-14,1.66321791214601E-16,
-1.)) ;
#39520 = DIRECTION('ref_axis',(1.,-5.55236256206829E-46,-4.54195640846217E-14)) ;
#39521 = DIRECTION('center_axis',(-4.54195640846217E-14,1.66321791214601E-16,
-1.)) ;
#39522 = DIRECTION('ref_axis',(-1.,0.,4.46626862477777E-14)) ;
#39523 = DIRECTION('center_axis',(4.54195640846217E-14,-1.66321791214601E-16,
1.)) ;
#39524 = DIRECTION('ref_axis',(-1.,1.8946420272009E-13,4.54195640846217E-14)) ;
#39525 = DIRECTION('center_axis',(-7.59720474939486E-30,-1.,-1.66321791214601E-16)) ;
#39526 = DIRECTION('ref_axis',(1.,0.,-4.56777472988634E-14)) ;
#39527 = DIRECTION('center_axis',(-4.54195640846217E-14,1.66321791214601E-16,
-1.)) ;
#39528 = DIRECTION('ref_axis',(-1.,1.8946420272009E-13,4.54195640846217E-14)) ;
#39529 = DIRECTION('center_axis',(-4.54195640846217E-14,1.66321791214601E-16,
-1.)) ;
#39530 = DIRECTION('ref_axis',(-1.,1.75658099177411E-13,4.54195640846217E-14)) ;
#39531 = DIRECTION('center_axis',(-2.1716102378779E-15,3.83815143260386E-28,
1.)) ;
#39532 = DIRECTION('ref_axis',(-1.,1.75658099177411E-13,-2.1716102378779E-15)) ;
#39533 = DIRECTION('',(-4.54195640846217E-14,1.66321791214601E-16,-1.)) ;
#39534 = DIRECTION('center_axis',(-4.54195640846217E-14,1.66321791214601E-16,
-1.)) ;
#39535 = DIRECTION('ref_axis',(-1.,5.55236256206829E-46,4.54195640846217E-14)) ;
#39536 = DIRECTION('',(1.75658099177411E-13,1.,1.66321791206623E-16)) ;
#39537 = DIRECTION('',(1.,-1.75658099177411E-13,-4.54195640846217E-14)) ;
#39538 = DIRECTION('',(-1.75658099177411E-13,-1.,-1.66321791206623E-16)) ;
#39539 = DIRECTION('',(-1.,1.75658099177411E-13,4.54195640846217E-14)) ;
#39540 = DIRECTION('',(-1.,3.33066907386739E-16,4.54195640846217E-14)) ;
#39541 = DIRECTION('center_axis',(-4.54195640846217E-14,1.66321791214601E-16,
-1.)) ;
#39542 = DIRECTION('ref_axis',(1.,-5.55236256206829E-46,-4.54195640846217E-14)) ;
#39543 = DIRECTION('',(-8.32667268460786E-17,-1.,-1.66321791214597E-16)) ;
#39544 = DIRECTION('center_axis',(-4.54195640846217E-14,1.66321791214601E-16,
-1.)) ;
#39545 = DIRECTION('ref_axis',(1.,-5.55236256206829E-46,-4.54195640846217E-14)) ;
#39546 = DIRECTION('',(1.,-3.33066907386739E-16,-4.54195640846217E-14)) ;
#39547 = DIRECTION('center_axis',(-4.54195640846217E-14,1.66321791214601E-16,
-1.)) ;
#39548 = DIRECTION('ref_axis',(1.,-5.55236256206829E-46,-4.54195640846217E-14)) ;
#39549 = DIRECTION('',(1.66533453692965E-16,1.,1.66321791214593E-16)) ;
#39550 = DIRECTION('center_axis',(-4.54195640846217E-14,1.66321791214601E-16,
-1.)) ;
#39551 = DIRECTION('ref_axis',(1.,-5.55236256206829E-46,-4.54195640846217E-14)) ;
#39552 = DIRECTION('center_axis',(-4.54195640846217E-14,1.66321791214601E-16,
-1.)) ;
#39553 = DIRECTION('ref_axis',(-1.,0.,4.46626862477777E-14)) ;
#39554 = DIRECTION('center_axis',(4.54195640846217E-14,-1.66321791214601E-16,
1.)) ;
#39555 = DIRECTION('ref_axis',(-1.,1.8946420272009E-13,4.54195640846217E-14)) ;
#39556 = DIRECTION('center_axis',(-7.59720474939486E-30,-1.,-1.66321791214601E-16)) ;
#39557 = DIRECTION('ref_axis',(1.,0.,-4.56777472988634E-14)) ;
#39558 = DIRECTION('center_axis',(-4.54195640846217E-14,1.66321791214601E-16,
-1.)) ;
#39559 = DIRECTION('ref_axis',(-1.,1.8946420272009E-13,4.54195640846217E-14)) ;
#39560 = DIRECTION('center_axis',(-4.54195640846217E-14,1.66321791214601E-16,
-1.)) ;
#39561 = DIRECTION('ref_axis',(-1.,1.75658099177411E-13,4.54195640846217E-14)) ;
#39562 = DIRECTION('center_axis',(-2.1716102378779E-15,3.83815143260386E-28,
1.)) ;
#39563 = DIRECTION('ref_axis',(-1.,1.75658099177411E-13,-2.1716102378779E-15)) ;
#39564 = DIRECTION('',(-4.54195640846217E-14,1.66321791214601E-16,-1.)) ;
#39565 = DIRECTION('center_axis',(-4.54195640846217E-14,1.66321791214601E-16,
-1.)) ;
#39566 = DIRECTION('ref_axis',(-1.,5.55236256206829E-46,4.54195640846217E-14)) ;
#39567 = DIRECTION('',(-1.75658099177411E-13,-1.,-1.66321791206623E-16)) ;
#39568 = DIRECTION('',(-1.,1.75658099177411E-13,4.54195640846217E-14)) ;
#39569 = DIRECTION('',(1.75658099177411E-13,1.,1.66321791206623E-16)) ;
#39570 = DIRECTION('',(1.,-1.75658099177411E-13,-4.54195640846217E-14)) ;
#39571 = DIRECTION('',(-1.,3.33066907386739E-16,4.54195640846217E-14)) ;
#39572 = DIRECTION('center_axis',(-4.54195640846217E-14,1.66321791214601E-16,
-1.)) ;
#39573 = DIRECTION('ref_axis',(1.,-5.55236256206829E-46,-4.54195640846217E-14)) ;
#39574 = DIRECTION('',(-8.32667268460786E-17,-1.,-1.66321791214597E-16)) ;
#39575 = DIRECTION('center_axis',(-4.54195640846217E-14,1.66321791214601E-16,
-1.)) ;
#39576 = DIRECTION('ref_axis',(1.,-5.55236256206829E-46,-4.54195640846217E-14)) ;
#39577 = DIRECTION('',(1.,-3.33066907386739E-16,-4.54195640846217E-14)) ;
#39578 = DIRECTION('center_axis',(-4.54195640846217E-14,1.66321791214601E-16,
-1.)) ;
#39579 = DIRECTION('ref_axis',(1.,-5.55236256206829E-46,-4.54195640846217E-14)) ;
#39580 = DIRECTION('',(1.66533453692965E-16,1.,1.66321791214593E-16)) ;
#39581 = DIRECTION('center_axis',(-4.54195640846217E-14,1.66321791214601E-16,
-1.)) ;
#39582 = DIRECTION('ref_axis',(1.,-5.55236256206829E-46,-4.54195640846217E-14)) ;
#39583 = DIRECTION('center_axis',(-4.54195640846217E-14,1.66321791214601E-16,
-1.)) ;
#39584 = DIRECTION('ref_axis',(-1.,0.,4.46626862477777E-14)) ;
#39585 = DIRECTION('center_axis',(4.54195640846217E-14,-1.66321791214601E-16,
1.)) ;
#39586 = DIRECTION('ref_axis',(-1.,1.8946420272009E-13,4.54195640846217E-14)) ;
#39587 = DIRECTION('center_axis',(-7.59720474939486E-30,-1.,-1.66321791214601E-16)) ;
#39588 = DIRECTION('ref_axis',(1.,0.,-4.56777472988634E-14)) ;
#39589 = DIRECTION('center_axis',(-4.54195640846217E-14,1.66321791214601E-16,
-1.)) ;
#39590 = DIRECTION('ref_axis',(-1.,1.8946420272009E-13,4.54195640846217E-14)) ;
#39591 = DIRECTION('center_axis',(-4.54195640846217E-14,1.66321791214601E-16,
-1.)) ;
#39592 = DIRECTION('ref_axis',(-1.,1.75658099177411E-13,4.54195640846217E-14)) ;
#39593 = DIRECTION('center_axis',(-2.1716102378779E-15,3.83815143260386E-28,
1.)) ;
#39594 = DIRECTION('ref_axis',(-1.,1.75658099177411E-13,-2.1716102378779E-15)) ;
#39595 = DIRECTION('',(-4.54195640846217E-14,1.66321791214601E-16,-1.)) ;
#39596 = DIRECTION('center_axis',(-4.54195640846217E-14,1.66321791214601E-16,
-1.)) ;
#39597 = DIRECTION('ref_axis',(-1.,5.55236256206829E-46,4.54195640846217E-14)) ;
#39598 = DIRECTION('',(-1.75658099177411E-13,-1.,-1.66321791206623E-16)) ;
#39599 = DIRECTION('',(-1.,1.75658099177411E-13,4.54195640846217E-14)) ;
#39600 = DIRECTION('',(1.75658099177411E-13,1.,1.66321791206623E-16)) ;
#39601 = DIRECTION('',(1.,-1.75658099177411E-13,-4.54195640846217E-14)) ;
#39602 = DIRECTION('',(-1.,3.33066907386739E-16,4.54195640846217E-14)) ;
#39603 = DIRECTION('center_axis',(-4.54195640846217E-14,1.66321791214601E-16,
-1.)) ;
#39604 = DIRECTION('ref_axis',(1.,-5.55236256206829E-46,-4.54195640846217E-14)) ;
#39605 = DIRECTION('',(-8.32667268460786E-17,-1.,-1.66321791214597E-16)) ;
#39606 = DIRECTION('center_axis',(-4.54195640846217E-14,1.66321791214601E-16,
-1.)) ;
#39607 = DIRECTION('ref_axis',(1.,-5.55236256206829E-46,-4.54195640846217E-14)) ;
#39608 = DIRECTION('',(1.,-3.33066907386739E-16,-4.54195640846217E-14)) ;
#39609 = DIRECTION('center_axis',(-4.54195640846217E-14,1.66321791214601E-16,
-1.)) ;
#39610 = DIRECTION('ref_axis',(1.,-5.55236256206829E-46,-4.54195640846217E-14)) ;
#39611 = DIRECTION('',(1.66533453692965E-16,1.,1.66321791214593E-16)) ;
#39612 = DIRECTION('center_axis',(-4.54195640846217E-14,1.66321791214601E-16,
-1.)) ;
#39613 = DIRECTION('ref_axis',(1.,-5.55236256206829E-46,-4.54195640846217E-14)) ;
#39614 = DIRECTION('center_axis',(-4.54195640846217E-14,1.66321791214601E-16,
-1.)) ;
#39615 = DIRECTION('ref_axis',(-1.,0.,4.46626862477777E-14)) ;
#39616 = DIRECTION('center_axis',(4.54195640846217E-14,-1.66321791214601E-16,
1.)) ;
#39617 = DIRECTION('ref_axis',(-1.,1.8946420272009E-13,4.54195640846217E-14)) ;
#39618 = DIRECTION('center_axis',(-7.59720474939486E-30,-1.,-1.66321791214601E-16)) ;
#39619 = DIRECTION('ref_axis',(1.,0.,-4.56777472988634E-14)) ;
#39620 = DIRECTION('center_axis',(-4.54195640846217E-14,1.66321791214601E-16,
-1.)) ;
#39621 = DIRECTION('ref_axis',(-1.,1.8946420272009E-13,4.54195640846217E-14)) ;
#39622 = DIRECTION('center_axis',(-4.54195640846217E-14,1.66321791214601E-16,
-1.)) ;
#39623 = DIRECTION('ref_axis',(-1.,1.75658099177411E-13,4.54195640846217E-14)) ;
#39624 = DIRECTION('center_axis',(-2.1716102378779E-15,3.83815143260386E-28,
1.)) ;
#39625 = DIRECTION('ref_axis',(-1.,1.75658099177411E-13,-2.1716102378779E-15)) ;
#39626 = DIRECTION('',(-4.54195640846217E-14,1.66321791214601E-16,-1.)) ;
#39627 = DIRECTION('center_axis',(-4.54195640846217E-14,1.66321791214601E-16,
-1.)) ;
#39628 = DIRECTION('ref_axis',(-1.,5.55236256206829E-46,4.54195640846217E-14)) ;
#39629 = DIRECTION('',(-1.75658099177411E-13,-1.,-1.66321791206623E-16)) ;
#39630 = DIRECTION('',(-1.,1.75658099177411E-13,4.54195640846217E-14)) ;
#39631 = DIRECTION('',(1.75658099177411E-13,1.,1.66321791206623E-16)) ;
#39632 = DIRECTION('',(1.,-1.75658099177411E-13,-4.54195640846217E-14)) ;
#39633 = DIRECTION('',(-1.,3.33066907386739E-16,4.54195640846217E-14)) ;
#39634 = DIRECTION('center_axis',(-4.54195640846217E-14,1.66321791214601E-16,
-1.)) ;
#39635 = DIRECTION('ref_axis',(1.,-5.55236256206829E-46,-4.54195640846217E-14)) ;
#39636 = DIRECTION('',(-8.32667268460786E-17,-1.,-1.66321791214597E-16)) ;
#39637 = DIRECTION('center_axis',(-4.54195640846217E-14,1.66321791214601E-16,
-1.)) ;
#39638 = DIRECTION('ref_axis',(1.,-5.55236256206829E-46,-4.54195640846217E-14)) ;
#39639 = DIRECTION('',(1.,-3.33066907386739E-16,-4.54195640846217E-14)) ;
#39640 = DIRECTION('center_axis',(-4.54195640846217E-14,1.66321791214601E-16,
-1.)) ;
#39641 = DIRECTION('ref_axis',(1.,-5.55236256206829E-46,-4.54195640846217E-14)) ;
#39642 = DIRECTION('',(1.66533453692965E-16,1.,1.66321791214593E-16)) ;
#39643 = DIRECTION('center_axis',(-4.54195640846217E-14,1.66321791214601E-16,
-1.)) ;
#39644 = DIRECTION('ref_axis',(1.,-5.55236256206829E-46,-4.54195640846217E-14)) ;
#39645 = DIRECTION('center_axis',(-4.54195640846217E-14,1.66321791214601E-16,
-1.)) ;
#39646 = DIRECTION('ref_axis',(-1.,0.,4.46626862477777E-14)) ;
#39647 = DIRECTION('center_axis',(4.54195640846217E-14,-1.66321791214601E-16,
1.)) ;
#39648 = DIRECTION('ref_axis',(-1.,1.8946420272009E-13,4.54195640846217E-14)) ;
#39649 = DIRECTION('center_axis',(-7.59720474939486E-30,-1.,-1.66321791214601E-16)) ;
#39650 = DIRECTION('ref_axis',(1.,0.,-4.56777472988634E-14)) ;
#39651 = DIRECTION('center_axis',(-4.54195640846217E-14,1.66321791214601E-16,
-1.)) ;
#39652 = DIRECTION('ref_axis',(-1.,1.8946420272009E-13,4.54195640846217E-14)) ;
#39653 = DIRECTION('center_axis',(-4.54195640846217E-14,1.66321791214601E-16,
-1.)) ;
#39654 = DIRECTION('ref_axis',(-1.,1.75658099177411E-13,4.54195640846217E-14)) ;
#39655 = DIRECTION('center_axis',(-2.1716102378779E-15,3.83815143260386E-28,
1.)) ;
#39656 = DIRECTION('ref_axis',(-1.,1.75658099177411E-13,-2.1716102378779E-15)) ;
#39657 = DIRECTION('',(-4.54195640846217E-14,1.66321791214601E-16,-1.)) ;
#39658 = DIRECTION('center_axis',(-4.54195640846217E-14,1.66321791214601E-16,
-1.)) ;
#39659 = DIRECTION('ref_axis',(-1.,5.55236256206829E-46,4.54195640846217E-14)) ;
#39660 = DIRECTION('',(-1.75658099177411E-13,-1.,-1.66321791206623E-16)) ;
#39661 = DIRECTION('',(-1.,1.75658099177411E-13,4.54195640846217E-14)) ;
#39662 = DIRECTION('',(1.75658099177411E-13,1.,1.66321791206623E-16)) ;
#39663 = DIRECTION('',(1.,-1.75658099177411E-13,-4.54195640846217E-14)) ;
#39664 = DIRECTION('',(-1.,3.33066907386739E-16,4.54195640846217E-14)) ;
#39665 = DIRECTION('center_axis',(-4.54195640846217E-14,1.66321791214601E-16,
-1.)) ;
#39666 = DIRECTION('ref_axis',(1.,-5.55236256206829E-46,-4.54195640846217E-14)) ;
#39667 = DIRECTION('',(-8.32667268460786E-17,-1.,-1.66321791214597E-16)) ;
#39668 = DIRECTION('center_axis',(-4.54195640846217E-14,1.66321791214601E-16,
-1.)) ;
#39669 = DIRECTION('ref_axis',(1.,-5.55236256206829E-46,-4.54195640846217E-14)) ;
#39670 = DIRECTION('',(1.,-3.33066907386739E-16,-4.54195640846217E-14)) ;
#39671 = DIRECTION('center_axis',(-4.54195640846217E-14,1.66321791214601E-16,
-1.)) ;
#39672 = DIRECTION('ref_axis',(1.,-5.55236256206829E-46,-4.54195640846217E-14)) ;
#39673 = DIRECTION('',(1.66533453692965E-16,1.,1.66321791214593E-16)) ;
#39674 = DIRECTION('center_axis',(-4.54195640846217E-14,1.66321791214601E-16,
-1.)) ;
#39675 = DIRECTION('ref_axis',(1.,-5.55236256206829E-46,-4.54195640846217E-14)) ;
#39676 = DIRECTION('center_axis',(-4.54195640846217E-14,1.66321791214601E-16,
-1.)) ;
#39677 = DIRECTION('ref_axis',(-1.,0.,4.46626862477777E-14)) ;
#39678 = DIRECTION('center_axis',(4.54195640846217E-14,-1.66321791214601E-16,
1.)) ;
#39679 = DIRECTION('ref_axis',(-1.,1.8946420272009E-13,4.54195640846217E-14)) ;
#39680 = DIRECTION('center_axis',(-7.59720474939486E-30,-1.,-1.66321791214601E-16)) ;
#39681 = DIRECTION('ref_axis',(1.,0.,-4.56777472988634E-14)) ;
#39682 = DIRECTION('center_axis',(-4.54195640846217E-14,1.66321791214601E-16,
-1.)) ;
#39683 = DIRECTION('ref_axis',(-1.,1.8946420272009E-13,4.54195640846217E-14)) ;
#39684 = DIRECTION('center_axis',(-4.54195640846217E-14,1.66321791214601E-16,
-1.)) ;
#39685 = DIRECTION('ref_axis',(-1.,5.55236256206829E-46,4.54195640846217E-14)) ;
#39686 = DIRECTION('',(-1.75658099177411E-13,-1.,-1.66321791206623E-16)) ;
#39687 = DIRECTION('',(-1.,1.75658099177411E-13,4.54195640846217E-14)) ;
#39688 = DIRECTION('',(1.75658099177411E-13,1.,1.66321791206623E-16)) ;
#39689 = DIRECTION('',(1.,-1.75658099177411E-13,-4.54195640846217E-14)) ;
#39690 = DIRECTION('',(1.,-3.33066907386739E-16,-4.54195640846217E-14)) ;
#39691 = DIRECTION('center_axis',(-4.54195640846217E-14,1.66321791214601E-16,
-1.)) ;
#39692 = DIRECTION('ref_axis',(-0.707106781186502,0.707106781186593,3.22340890291979E-14)) ;
#39693 = DIRECTION('',(8.32667268460786E-17,1.,1.66321791214597E-16)) ;
#39694 = DIRECTION('center_axis',(-4.54195640846217E-14,1.66321791214601E-16,
-1.)) ;
#39695 = DIRECTION('ref_axis',(-0.707106781186502,-0.707106781186593,3.1998874496344E-14)) ;
#39696 = DIRECTION('',(-1.,3.33066907386739E-16,4.54195640846217E-14)) ;
#39697 = DIRECTION('center_axis',(-4.54195640846217E-14,1.66321791214601E-16,
-1.)) ;
#39698 = DIRECTION('ref_axis',(0.707106781186593,-0.707106781186502,-3.2234089029202E-14)) ;
#39699 = DIRECTION('',(-1.66533453692965E-16,-1.,-1.66321791214593E-16)) ;
#39700 = DIRECTION('center_axis',(-4.54195640846217E-14,1.66321791214601E-16,
-1.)) ;
#39701 = DIRECTION('ref_axis',(0.707106781186593,0.707106781186502,-3.19988744963481E-14)) ;
#39702 = DIRECTION('center_axis',(-4.54195640846217E-14,1.66321791214601E-16,
-1.)) ;
#39703 = DIRECTION('ref_axis',(-1.,1.75658099177411E-13,4.54195640846217E-14)) ;
#39704 = DIRECTION('center_axis',(-2.1716102378779E-15,3.83815143260386E-28,
1.)) ;
#39705 = DIRECTION('ref_axis',(-1.,1.75658099177411E-13,-2.1716102378779E-15)) ;
#39706 = DIRECTION('',(-4.54195640846217E-14,1.66321791214601E-16,-1.)) ;
#39707 = DIRECTION('center_axis',(2.1716102378779E-15,-3.83815143260386E-28,
-1.)) ;
#39708 = DIRECTION('ref_axis',(1.,-1.66533453692941E-16,2.1716102378779E-15)) ;
#39709 = DIRECTION('center_axis',(-2.1716102378779E-15,3.83815143260386E-28,
1.)) ;
#39710 = DIRECTION('ref_axis',(-1.,-7.33033736753389E-16,-2.1716102378779E-15)) ;
#39711 = DIRECTION('center_axis',(2.1716102378779E-15,-3.83815143260386E-28,
-1.)) ;
#39712 = DIRECTION('ref_axis',(1.,-1.66533453692941E-16,2.1716102378779E-15)) ;
#39713 = DIRECTION('center_axis',(-2.1716102378779E-15,3.83815143260386E-28,
1.)) ;
#39714 = DIRECTION('ref_axis',(-1.,-7.33033736753389E-16,-2.1716102378779E-15)) ;
#39715 = DIRECTION('center_axis',(2.1716102378779E-15,-3.83815143260386E-28,
-1.)) ;
#39716 = DIRECTION('ref_axis',(1.,-1.66533453692941E-16,2.1716102378779E-15)) ;
#39717 = DIRECTION('center_axis',(-2.1716102378779E-15,3.83815143260386E-28,
1.)) ;
#39718 = DIRECTION('ref_axis',(-1.,-7.33033736753389E-16,-2.1716102378779E-15)) ;
#39719 = DIRECTION('center_axis',(2.1716102378779E-15,-3.83815143260386E-28,
-1.)) ;
#39720 = DIRECTION('ref_axis',(1.,-1.66533453692941E-16,2.1716102378779E-15)) ;
#39721 = DIRECTION('center_axis',(-2.1716102378779E-15,3.83815143260386E-28,
1.)) ;
#39722 = DIRECTION('ref_axis',(-1.,-7.33033736753389E-16,-2.1716102378779E-15)) ;
#39723 = DIRECTION('center_axis',(2.1716102378779E-15,-3.83815143260386E-28,
-1.)) ;
#39724 = DIRECTION('ref_axis',(1.,-1.66533453692941E-16,2.1716102378779E-15)) ;
#39725 = DIRECTION('center_axis',(-2.1716102378779E-15,3.83815143260386E-28,
1.)) ;
#39726 = DIRECTION('ref_axis',(-1.,-7.33033736753389E-16,-2.1716102378779E-15)) ;
#39727 = DIRECTION('center_axis',(2.1716102378779E-15,-3.83815143260386E-28,
-1.)) ;
#39728 = DIRECTION('ref_axis',(1.,-1.66533453692941E-16,2.1716102378779E-15)) ;
#39729 = DIRECTION('center_axis',(-2.1716102378779E-15,3.83815143260386E-28,
1.)) ;
#39730 = DIRECTION('ref_axis',(-1.,-7.33033736753389E-16,-2.1716102378779E-15)) ;
#39731 = DIRECTION('center_axis',(2.1716102378779E-15,-3.83815143260386E-28,
-1.)) ;
#39732 = DIRECTION('ref_axis',(1.,-1.66533453692941E-16,2.1716102378779E-15)) ;
#39733 = DIRECTION('center_axis',(-2.1716102378779E-15,3.83815143260386E-28,
1.)) ;
#39734 = DIRECTION('ref_axis',(-1.,-7.33033736753389E-16,-2.1716102378779E-15)) ;
#39735 = DIRECTION('center_axis',(2.1716102378779E-15,-3.83815143260386E-28,
-1.)) ;
#39736 = DIRECTION('ref_axis',(1.,-1.66533453692941E-16,2.1716102378779E-15)) ;
#39737 = DIRECTION('center_axis',(-2.1716102378779E-15,3.83815143260386E-28,
1.)) ;
#39738 = DIRECTION('ref_axis',(-1.,-7.33033736753389E-16,-2.1716102378779E-15)) ;
#39739 = DIRECTION('center_axis',(-1.,3.33066907386739E-16,4.54195640846217E-14)) ;
#39740 = DIRECTION('ref_axis',(-3.23519956315716E-14,-0.707106781186623,-0.707106781186472)) ;
#39741 = DIRECTION('center_axis',(-1.,0.,0.)) ;
#39742 = DIRECTION('ref_axis',(0.,0.,-1.)) ;
#39743 = DIRECTION('',(-1.,3.33066907386739E-16,4.54195640846217E-14)) ;
#39744 = DIRECTION('center_axis',(1.,0.,0.)) ;
#39745 = DIRECTION('ref_axis',(0.,-1.,0.)) ;
#39746 = DIRECTION('center_axis',(4.54195640846217E-14,-1.66321791214601E-16,
1.)) ;
#39747 = DIRECTION('ref_axis',(1.,0.,-4.54747350886464E-14)) ;
#39748 = DIRECTION('center_axis',(0.,1.,0.)) ;
#39749 = DIRECTION('ref_axis',(1.,0.,-3.5527136788002E-14)) ;
#39750 = DIRECTION('center_axis',(2.17161023787787E-15,-3.6685463379813E-28,
-1.)) ;
#39751 = DIRECTION('ref_axis',(-0.707106781186543,0.707106781186552,-1.53556032529782E-15)) ;
#39752 = DIRECTION('center_axis',(-8.32667268460786E-17,-1.,-1.66321791214597E-16)) ;
#39753 = DIRECTION('ref_axis',(0.707106781186522,5.87287992268709E-17,-0.707106781186573)) ;
#39754 = DIRECTION('center_axis',(0.,1.,0.)) ;
#39755 = DIRECTION('ref_axis',(1.,0.,0.)) ;
#39756 = DIRECTION('',(-8.32667268460786E-17,-1.,-1.66321791214597E-16)) ;
#39757 = DIRECTION('center_axis',(4.54195640846217E-14,-1.66321791214601E-16,
1.)) ;
#39758 = DIRECTION('ref_axis',(1.,0.,-4.54747350886464E-14)) ;
#39759 = DIRECTION('center_axis',(-1.,-2.84217094303975E-13,0.)) ;
#39760 = DIRECTION('ref_axis',(-2.84217094303975E-13,1.,0.)) ;
#39761 = DIRECTION('center_axis',(-2.17161023787787E-15,3.6685463379813E-28,
1.)) ;
#39762 = DIRECTION('ref_axis',(-0.707106781186552,-0.707106781186543,-1.53556032529732E-15)) ;
#39763 = DIRECTION('center_axis',(1.,-3.33066907386739E-16,-4.54195640846217E-14)) ;
#39764 = DIRECTION('ref_axis',(-3.18809678939767E-14,0.707106781186422,-0.707106781186673)) ;
#39765 = DIRECTION('center_axis',(-1.,0.,0.)) ;
#39766 = DIRECTION('ref_axis',(0.,1.,0.)) ;
#39767 = DIRECTION('',(1.,-3.33066907386739E-16,-4.54195640846217E-14)) ;
#39768 = DIRECTION('center_axis',(4.54195640846217E-14,-1.66321791214601E-16,
1.)) ;
#39769 = DIRECTION('ref_axis',(1.,0.,-4.54747350886464E-14)) ;
#39770 = DIRECTION('center_axis',(0.,-1.,0.)) ;
#39771 = DIRECTION('ref_axis',(-1.,0.,3.5527136788007E-14)) ;
#39772 = DIRECTION('center_axis',(2.1716102378779E-15,-3.66854633798134E-28,
-1.)) ;
#39773 = DIRECTION('ref_axis',(0.707106781186543,-0.707106781186552,1.53556032529784E-15)) ;
#39774 = DIRECTION('center_axis',(1.66533453692965E-16,1.,1.66321791214593E-16)) ;
#39775 = DIRECTION('ref_axis',(-0.707106781186522,2.35364200827643E-16,-0.707106781186573)) ;
#39776 = DIRECTION('center_axis',(0.,-1.,0.)) ;
#39777 = DIRECTION('ref_axis',(-1.,0.,0.)) ;
#39778 = DIRECTION('',(1.66533453692965E-16,1.,1.66321791214593E-16)) ;
#39779 = DIRECTION('center_axis',(4.54195640846217E-14,-1.66321791214601E-16,
1.)) ;
#39780 = DIRECTION('ref_axis',(1.,0.,-4.54747350886464E-14)) ;
#39781 = DIRECTION('center_axis',(-2.1716102378779E-15,3.66854633798134E-28,
1.)) ;
#39782 = DIRECTION('ref_axis',(0.707106781186452,0.707106781186643,1.53556032529713E-15)) ;
#39783 = DIRECTION('center_axis',(-2.17161023787787E-15,3.6685463379813E-28,
1.)) ;
#39784 = DIRECTION('ref_axis',(-0.707106781186552,-0.707106781186543,-1.53556032529732E-15)) ;
#39785 = DIRECTION('',(2.17161023787787E-15,-3.6685463379813E-28,-1.)) ;
#39786 = DIRECTION('center_axis',(1.88526971141291E-28,-2.90739654573716E-15,
-1.)) ;
#39787 = DIRECTION('ref_axis',(1.35627620245787E-13,-1.,2.90739654573716E-15)) ;
#39788 = DIRECTION('',(-2.17161023787787E-15,3.6685463379813E-28,1.)) ;
#39789 = DIRECTION('center_axis',(-1.,8.32667268460789E-17,-2.17161023787787E-15)) ;
#39790 = DIRECTION('ref_axis',(8.32667268460789E-17,1.,-3.92101138914083E-28)) ;
#39791 = DIRECTION('',(-2.17161023787787E-15,3.6685463379813E-28,1.)) ;
#39792 = DIRECTION('center_axis',(-1.,8.32667268460789E-17,-2.17161023787787E-15)) ;
#39793 = DIRECTION('ref_axis',(-1.59443879249779E-15,-0.707106781186479,0.707106781186616)) ;
#39794 = DIRECTION('',(8.32667268460789E-17,1.,-3.83780830390118E-28)) ;
#39795 = DIRECTION('',(-2.17161023787787E-15,3.83815143260382E-28,1.)) ;
#39796 = DIRECTION('',(8.32667268460786E-17,1.,1.66321791214597E-16)) ;
#39797 = DIRECTION('',(2.17161023787787E-15,-3.83420712807771E-28,-1.)) ;
#39798 = DIRECTION('',(8.32667268460789E-17,1.,-3.83780830390118E-28)) ;
#39799 = DIRECTION('center_axis',(-1.,8.32667268460789E-17,-2.17161023787787E-15)) ;
#39800 = DIRECTION('ref_axis',(-1.47668185809765E-15,0.707106781186483,0.707106781186612)) ;
#39801 = DIRECTION('center_axis',(2.17161023787787E-15,-3.6685463379813E-28,
-1.)) ;
#39802 = DIRECTION('ref_axis',(-0.707106781186543,0.707106781186552,-1.53556032529782E-15)) ;
#39803 = DIRECTION('',(2.17161023787787E-15,-3.6685463379813E-28,-1.)) ;
#39804 = DIRECTION('center_axis',(1.88526971141291E-28,-2.90739654573716E-15,
-1.)) ;
#39805 = DIRECTION('ref_axis',(-1.,6.48092690620067E-15,-2.07369595641554E-28)) ;
#39806 = DIRECTION('center_axis',(3.33066907386739E-16,1.,-3.66031460022645E-28)) ;
#39807 = DIRECTION('ref_axis',(2.17161023787795E-15,-3.66754751528624E-28,
-1.)) ;
#39808 = DIRECTION('',(-2.1716102378779E-15,3.66854633798134E-28,1.)) ;
#39809 = DIRECTION('',(-1.,3.33066907386739E-16,-2.1716102378779E-15)) ;
#39810 = DIRECTION('center_axis',(-1.,3.33066907386739E-16,4.54195640846217E-14)) ;
#39811 = DIRECTION('ref_axis',(-3.23519956315716E-14,-0.707106781186623,-0.707106781186472)) ;
#39812 = DIRECTION('center_axis',(-1.,0.,0.)) ;
#39813 = DIRECTION('ref_axis',(0.,0.,-1.)) ;
#39814 = DIRECTION('',(-1.,3.33066907386739E-16,4.54195640846217E-14)) ;
#39815 = DIRECTION('center_axis',(1.,0.,0.)) ;
#39816 = DIRECTION('ref_axis',(0.,-1.,0.)) ;
#39817 = DIRECTION('center_axis',(4.54195640846217E-14,-1.66321791214601E-16,
1.)) ;
#39818 = DIRECTION('ref_axis',(1.,0.,-4.54747350886464E-14)) ;
#39819 = DIRECTION('center_axis',(0.,1.,0.)) ;
#39820 = DIRECTION('ref_axis',(1.,0.,-3.5527136788002E-14)) ;
#39821 = DIRECTION('center_axis',(2.17161023787787E-15,-3.6685463379813E-28,
-1.)) ;
#39822 = DIRECTION('ref_axis',(-0.707106781186543,0.707106781186552,-1.53556032529782E-15)) ;
#39823 = DIRECTION('center_axis',(-8.32667268460786E-17,-1.,-1.66321791214597E-16)) ;
#39824 = DIRECTION('ref_axis',(0.707106781186522,5.87287992268709E-17,-0.707106781186573)) ;
#39825 = DIRECTION('center_axis',(0.,1.,0.)) ;
#39826 = DIRECTION('ref_axis',(1.,0.,0.)) ;
#39827 = DIRECTION('',(-8.32667268460786E-17,-1.,-1.66321791214597E-16)) ;
#39828 = DIRECTION('center_axis',(4.54195640846217E-14,-1.66321791214601E-16,
1.)) ;
#39829 = DIRECTION('ref_axis',(1.,0.,-4.54747350886464E-14)) ;
#39830 = DIRECTION('center_axis',(-1.,-2.84217094303975E-13,0.)) ;
#39831 = DIRECTION('ref_axis',(-2.84217094303975E-13,1.,0.)) ;
#39832 = DIRECTION('center_axis',(-2.17161023787787E-15,3.6685463379813E-28,
1.)) ;
#39833 = DIRECTION('ref_axis',(-0.707106781186552,-0.707106781186543,-1.53556032529732E-15)) ;
#39834 = DIRECTION('center_axis',(1.,-3.33066907386739E-16,-4.54195640846217E-14)) ;
#39835 = DIRECTION('ref_axis',(-3.18809678939767E-14,0.707106781186422,-0.707106781186673)) ;
#39836 = DIRECTION('center_axis',(-1.,0.,0.)) ;
#39837 = DIRECTION('ref_axis',(0.,1.,0.)) ;
#39838 = DIRECTION('',(1.,-3.33066907386739E-16,-4.54195640846217E-14)) ;
#39839 = DIRECTION('center_axis',(4.54195640846217E-14,-1.66321791214601E-16,
1.)) ;
#39840 = DIRECTION('ref_axis',(1.,0.,-4.54747350886464E-14)) ;
#39841 = DIRECTION('center_axis',(0.,-1.,0.)) ;
#39842 = DIRECTION('ref_axis',(-1.,0.,3.5527136788007E-14)) ;
#39843 = DIRECTION('center_axis',(2.1716102378779E-15,-3.66854633798134E-28,
-1.)) ;
#39844 = DIRECTION('ref_axis',(0.707106781186543,-0.707106781186552,1.53556032529784E-15)) ;
#39845 = DIRECTION('center_axis',(1.66533453692965E-16,1.,1.66321791214593E-16)) ;
#39846 = DIRECTION('ref_axis',(-0.707106781186522,2.35364200827643E-16,-0.707106781186573)) ;
#39847 = DIRECTION('center_axis',(0.,-1.,0.)) ;
#39848 = DIRECTION('ref_axis',(-1.,0.,0.)) ;
#39849 = DIRECTION('',(1.66533453692965E-16,1.,1.66321791214593E-16)) ;
#39850 = DIRECTION('center_axis',(4.54195640846217E-14,-1.66321791214601E-16,
1.)) ;
#39851 = DIRECTION('ref_axis',(1.,0.,-4.54747350886464E-14)) ;
#39852 = DIRECTION('center_axis',(-2.1716102378779E-15,3.66854633798134E-28,
1.)) ;
#39853 = DIRECTION('ref_axis',(0.707106781186452,0.707106781186643,1.53556032529713E-15)) ;
#39854 = DIRECTION('center_axis',(-2.17161023787787E-15,3.6685463379813E-28,
1.)) ;
#39855 = DIRECTION('ref_axis',(-0.707106781186552,-0.707106781186543,-1.53556032529732E-15)) ;
#39856 = DIRECTION('',(2.17161023787787E-15,-3.6685463379813E-28,-1.)) ;
#39857 = DIRECTION('center_axis',(1.88526971141291E-28,-2.90739654573716E-15,
-1.)) ;
#39858 = DIRECTION('ref_axis',(1.35627620245787E-13,-1.,2.90739654573716E-15)) ;
#39859 = DIRECTION('',(-2.17161023787787E-15,3.6685463379813E-28,1.)) ;
#39860 = DIRECTION('center_axis',(-1.,8.32667268460789E-17,-2.17161023787787E-15)) ;
#39861 = DIRECTION('ref_axis',(8.32667268460789E-17,1.,-3.92101138914083E-28)) ;
#39862 = DIRECTION('',(-2.17161023787787E-15,3.6685463379813E-28,1.)) ;
#39863 = DIRECTION('center_axis',(-1.,8.32667268460789E-17,-2.17161023787787E-15)) ;
#39864 = DIRECTION('ref_axis',(-1.59443879249779E-15,-0.707106781186479,0.707106781186616)) ;
#39865 = DIRECTION('',(8.32667268460789E-17,1.,-3.83780830390118E-28)) ;
#39866 = DIRECTION('',(-2.17161023787787E-15,3.83815143260382E-28,1.)) ;
#39867 = DIRECTION('',(8.32667268460786E-17,1.,1.66321791214597E-16)) ;
#39868 = DIRECTION('',(2.17161023787787E-15,-3.83420712807771E-28,-1.)) ;
#39869 = DIRECTION('',(8.32667268460789E-17,1.,-3.83780830390118E-28)) ;
#39870 = DIRECTION('center_axis',(-1.,8.32667268460789E-17,-2.17161023787787E-15)) ;
#39871 = DIRECTION('ref_axis',(-1.47668185809765E-15,0.707106781186483,0.707106781186612)) ;
#39872 = DIRECTION('center_axis',(2.17161023787787E-15,-3.6685463379813E-28,
-1.)) ;
#39873 = DIRECTION('ref_axis',(-0.707106781186543,0.707106781186552,-1.53556032529782E-15)) ;
#39874 = DIRECTION('',(2.17161023787787E-15,-3.6685463379813E-28,-1.)) ;
#39875 = DIRECTION('center_axis',(1.88526971141291E-28,-2.90739654573716E-15,
-1.)) ;
#39876 = DIRECTION('ref_axis',(-1.,6.48092690620067E-15,-2.07369595641554E-28)) ;
#39877 = DIRECTION('center_axis',(3.33066907386739E-16,1.,-3.66031460022645E-28)) ;
#39878 = DIRECTION('ref_axis',(2.17161023787795E-15,-3.66754751528624E-28,
-1.)) ;
#39879 = DIRECTION('',(-2.1716102378779E-15,3.66854633798134E-28,1.)) ;
#39880 = DIRECTION('',(-1.,3.33066907386739E-16,-2.1716102378779E-15)) ;
#39881 = DIRECTION('center_axis',(-1.,3.33066907386739E-16,4.54195640846217E-14)) ;
#39882 = DIRECTION('ref_axis',(-3.23519956315716E-14,-0.707106781186623,-0.707106781186472)) ;
#39883 = DIRECTION('center_axis',(-1.,0.,0.)) ;
#39884 = DIRECTION('ref_axis',(0.,0.,-1.)) ;
#39885 = DIRECTION('',(-1.,3.33066907386739E-16,4.54195640846217E-14)) ;
#39886 = DIRECTION('center_axis',(1.,0.,0.)) ;
#39887 = DIRECTION('ref_axis',(0.,-1.,0.)) ;
#39888 = DIRECTION('center_axis',(4.54195640846217E-14,-1.66321791214601E-16,
1.)) ;
#39889 = DIRECTION('ref_axis',(1.,0.,-4.54747350886464E-14)) ;
#39890 = DIRECTION('center_axis',(0.,1.,0.)) ;
#39891 = DIRECTION('ref_axis',(1.,0.,-3.5527136788002E-14)) ;
#39892 = DIRECTION('center_axis',(2.17161023787787E-15,-3.6685463379813E-28,
-1.)) ;
#39893 = DIRECTION('ref_axis',(-0.707106781186543,0.707106781186552,-1.53556032529782E-15)) ;
#39894 = DIRECTION('center_axis',(-8.32667268460786E-17,-1.,-1.66321791214597E-16)) ;
#39895 = DIRECTION('ref_axis',(0.707106781186522,5.87287992268709E-17,-0.707106781186573)) ;
#39896 = DIRECTION('center_axis',(0.,1.,0.)) ;
#39897 = DIRECTION('ref_axis',(1.,0.,0.)) ;
#39898 = DIRECTION('',(-8.32667268460786E-17,-1.,-1.66321791214597E-16)) ;
#39899 = DIRECTION('center_axis',(4.54195640846217E-14,-1.66321791214601E-16,
1.)) ;
#39900 = DIRECTION('ref_axis',(1.,0.,-4.54747350886464E-14)) ;
#39901 = DIRECTION('center_axis',(-1.,-2.84217094303975E-13,0.)) ;
#39902 = DIRECTION('ref_axis',(-2.84217094303975E-13,1.,0.)) ;
#39903 = DIRECTION('center_axis',(-2.17161023787787E-15,3.6685463379813E-28,
1.)) ;
#39904 = DIRECTION('ref_axis',(-0.707106781186552,-0.707106781186543,-1.53556032529732E-15)) ;
#39905 = DIRECTION('center_axis',(1.,-3.33066907386739E-16,-4.54195640846217E-14)) ;
#39906 = DIRECTION('ref_axis',(-3.18809678939767E-14,0.707106781186422,-0.707106781186673)) ;
#39907 = DIRECTION('center_axis',(-1.,0.,0.)) ;
#39908 = DIRECTION('ref_axis',(0.,1.,0.)) ;
#39909 = DIRECTION('',(1.,-3.33066907386739E-16,-4.54195640846217E-14)) ;
#39910 = DIRECTION('center_axis',(4.54195640846217E-14,-1.66321791214601E-16,
1.)) ;
#39911 = DIRECTION('ref_axis',(1.,0.,-4.54747350886464E-14)) ;
#39912 = DIRECTION('center_axis',(0.,-1.,0.)) ;
#39913 = DIRECTION('ref_axis',(-1.,0.,3.5527136788007E-14)) ;
#39914 = DIRECTION('center_axis',(2.1716102378779E-15,-3.66854633798134E-28,
-1.)) ;
#39915 = DIRECTION('ref_axis',(0.707106781186543,-0.707106781186552,1.53556032529784E-15)) ;
#39916 = DIRECTION('center_axis',(1.66533453692965E-16,1.,1.66321791214593E-16)) ;
#39917 = DIRECTION('ref_axis',(-0.707106781186522,2.35364200827643E-16,-0.707106781186573)) ;
#39918 = DIRECTION('center_axis',(0.,-1.,0.)) ;
#39919 = DIRECTION('ref_axis',(-1.,0.,0.)) ;
#39920 = DIRECTION('',(1.66533453692965E-16,1.,1.66321791214593E-16)) ;
#39921 = DIRECTION('center_axis',(4.54195640846217E-14,-1.66321791214601E-16,
1.)) ;
#39922 = DIRECTION('ref_axis',(1.,0.,-4.54747350886464E-14)) ;
#39923 = DIRECTION('center_axis',(-2.1716102378779E-15,3.66854633798134E-28,
1.)) ;
#39924 = DIRECTION('ref_axis',(0.707106781186452,0.707106781186643,1.53556032529713E-15)) ;
#39925 = DIRECTION('center_axis',(-2.17161023787787E-15,3.6685463379813E-28,
1.)) ;
#39926 = DIRECTION('ref_axis',(-0.707106781186552,-0.707106781186543,-1.53556032529732E-15)) ;
#39927 = DIRECTION('',(2.17161023787787E-15,-3.6685463379813E-28,-1.)) ;
#39928 = DIRECTION('center_axis',(1.88526971141291E-28,-2.90739654573716E-15,
-1.)) ;
#39929 = DIRECTION('ref_axis',(1.35627620245787E-13,-1.,2.90739654573716E-15)) ;
#39930 = DIRECTION('',(-2.17161023787787E-15,3.6685463379813E-28,1.)) ;
#39931 = DIRECTION('center_axis',(-1.,8.32667268460789E-17,-2.17161023787787E-15)) ;
#39932 = DIRECTION('ref_axis',(8.32667268460789E-17,1.,-3.92101138914083E-28)) ;
#39933 = DIRECTION('',(-2.17161023787787E-15,3.6685463379813E-28,1.)) ;
#39934 = DIRECTION('center_axis',(-1.,8.32667268460789E-17,-2.17161023787787E-15)) ;
#39935 = DIRECTION('ref_axis',(-1.59443879249779E-15,-0.707106781186479,0.707106781186616)) ;
#39936 = DIRECTION('',(8.32667268460789E-17,1.,-3.83780830390118E-28)) ;
#39937 = DIRECTION('',(-2.17161023787787E-15,3.83815143260382E-28,1.)) ;
#39938 = DIRECTION('',(8.32667268460786E-17,1.,1.66321791214597E-16)) ;
#39939 = DIRECTION('',(2.17161023787787E-15,-3.83420712807771E-28,-1.)) ;
#39940 = DIRECTION('',(8.32667268460789E-17,1.,-3.83780830390118E-28)) ;
#39941 = DIRECTION('center_axis',(-1.,8.32667268460789E-17,-2.17161023787787E-15)) ;
#39942 = DIRECTION('ref_axis',(-1.47668185809765E-15,0.707106781186483,0.707106781186612)) ;
#39943 = DIRECTION('center_axis',(2.17161023787787E-15,-3.6685463379813E-28,
-1.)) ;
#39944 = DIRECTION('ref_axis',(-0.707106781186543,0.707106781186552,-1.53556032529782E-15)) ;
#39945 = DIRECTION('',(2.17161023787787E-15,-3.6685463379813E-28,-1.)) ;
#39946 = DIRECTION('center_axis',(1.88526971141291E-28,-2.90739654573716E-15,
-1.)) ;
#39947 = DIRECTION('ref_axis',(-1.,6.48092690620067E-15,-2.07369595641554E-28)) ;
#39948 = DIRECTION('center_axis',(3.33066907386739E-16,1.,-3.66031460022645E-28)) ;
#39949 = DIRECTION('ref_axis',(2.17161023787795E-15,-3.66754751528624E-28,
-1.)) ;
#39950 = DIRECTION('',(-2.1716102378779E-15,3.66854633798134E-28,1.)) ;
#39951 = DIRECTION('',(-1.,3.33066907386739E-16,-2.1716102378779E-15)) ;
#39952 = DIRECTION('center_axis',(-1.,3.33066907386739E-16,4.54195640846217E-14)) ;
#39953 = DIRECTION('ref_axis',(-3.23519956315716E-14,-0.707106781186623,-0.707106781186472)) ;
#39954 = DIRECTION('center_axis',(-1.,0.,0.)) ;
#39955 = DIRECTION('ref_axis',(0.,0.,-1.)) ;
#39956 = DIRECTION('',(-1.,3.33066907386739E-16,4.54195640846217E-14)) ;
#39957 = DIRECTION('center_axis',(1.,0.,0.)) ;
#39958 = DIRECTION('ref_axis',(0.,-1.,0.)) ;
#39959 = DIRECTION('center_axis',(4.54195640846217E-14,-1.66321791214601E-16,
1.)) ;
#39960 = DIRECTION('ref_axis',(1.,0.,-4.54747350886464E-14)) ;
#39961 = DIRECTION('center_axis',(0.,1.,0.)) ;
#39962 = DIRECTION('ref_axis',(1.,0.,-3.5527136788002E-14)) ;
#39963 = DIRECTION('center_axis',(2.17161023787787E-15,-3.6685463379813E-28,
-1.)) ;
#39964 = DIRECTION('ref_axis',(-0.707106781186543,0.707106781186552,-1.53556032529782E-15)) ;
#39965 = DIRECTION('center_axis',(-8.32667268460786E-17,-1.,-1.66321791214597E-16)) ;
#39966 = DIRECTION('ref_axis',(0.707106781186522,5.87287992268709E-17,-0.707106781186573)) ;
#39967 = DIRECTION('center_axis',(0.,1.,0.)) ;
#39968 = DIRECTION('ref_axis',(1.,0.,0.)) ;
#39969 = DIRECTION('',(-8.32667268460786E-17,-1.,-1.66321791214597E-16)) ;
#39970 = DIRECTION('center_axis',(4.54195640846217E-14,-1.66321791214601E-16,
1.)) ;
#39971 = DIRECTION('ref_axis',(1.,0.,-4.54747350886464E-14)) ;
#39972 = DIRECTION('center_axis',(-1.,-2.84217094303975E-13,0.)) ;
#39973 = DIRECTION('ref_axis',(-2.84217094303975E-13,1.,0.)) ;
#39974 = DIRECTION('center_axis',(-2.17161023787787E-15,3.6685463379813E-28,
1.)) ;
#39975 = DIRECTION('ref_axis',(-0.707106781186552,-0.707106781186543,-1.53556032529732E-15)) ;
#39976 = DIRECTION('center_axis',(1.,-3.33066907386739E-16,-4.54195640846217E-14)) ;
#39977 = DIRECTION('ref_axis',(-3.18809678939767E-14,0.707106781186422,-0.707106781186673)) ;
#39978 = DIRECTION('center_axis',(-1.,0.,0.)) ;
#39979 = DIRECTION('ref_axis',(0.,1.,0.)) ;
#39980 = DIRECTION('',(1.,-3.33066907386739E-16,-4.54195640846217E-14)) ;
#39981 = DIRECTION('center_axis',(4.54195640846217E-14,-1.66321791214601E-16,
1.)) ;
#39982 = DIRECTION('ref_axis',(1.,0.,-4.54747350886464E-14)) ;
#39983 = DIRECTION('center_axis',(0.,-1.,0.)) ;
#39984 = DIRECTION('ref_axis',(-1.,0.,3.5527136788007E-14)) ;
#39985 = DIRECTION('center_axis',(2.1716102378779E-15,-3.66854633798134E-28,
-1.)) ;
#39986 = DIRECTION('ref_axis',(0.707106781186543,-0.707106781186552,1.53556032529784E-15)) ;
#39987 = DIRECTION('center_axis',(1.66533453692965E-16,1.,1.66321791214593E-16)) ;
#39988 = DIRECTION('ref_axis',(-0.707106781186522,2.35364200827643E-16,-0.707106781186573)) ;
#39989 = DIRECTION('center_axis',(0.,-1.,0.)) ;
#39990 = DIRECTION('ref_axis',(-1.,0.,0.)) ;
#39991 = DIRECTION('',(1.66533453692965E-16,1.,1.66321791214593E-16)) ;
#39992 = DIRECTION('center_axis',(4.54195640846217E-14,-1.66321791214601E-16,
1.)) ;
#39993 = DIRECTION('ref_axis',(1.,0.,-4.54747350886464E-14)) ;
#39994 = DIRECTION('center_axis',(-2.1716102378779E-15,3.66854633798134E-28,
1.)) ;
#39995 = DIRECTION('ref_axis',(0.707106781186452,0.707106781186643,1.53556032529713E-15)) ;
#39996 = DIRECTION('center_axis',(-2.17161023787787E-15,3.6685463379813E-28,
1.)) ;
#39997 = DIRECTION('ref_axis',(-0.707106781186552,-0.707106781186543,-1.53556032529732E-15)) ;
#39998 = DIRECTION('',(2.17161023787787E-15,-3.6685463379813E-28,-1.)) ;
#39999 = DIRECTION('center_axis',(1.88526971141291E-28,-2.90739654573716E-15,
-1.)) ;
#40000 = DIRECTION('ref_axis',(1.35627620245787E-13,-1.,2.90739654573716E-15)) ;
#40001 = DIRECTION('',(-2.17161023787787E-15,3.6685463379813E-28,1.)) ;
#40002 = DIRECTION('center_axis',(-1.,8.32667268460789E-17,-2.17161023787787E-15)) ;
#40003 = DIRECTION('ref_axis',(8.32667268460789E-17,1.,-3.92101138914083E-28)) ;
#40004 = DIRECTION('',(-2.17161023787787E-15,3.6685463379813E-28,1.)) ;
#40005 = DIRECTION('center_axis',(-1.,8.32667268460789E-17,-2.17161023787787E-15)) ;
#40006 = DIRECTION('ref_axis',(-1.59443879249779E-15,-0.707106781186479,0.707106781186616)) ;
#40007 = DIRECTION('',(8.32667268460789E-17,1.,-3.83780830390118E-28)) ;
#40008 = DIRECTION('',(-2.17161023787787E-15,3.83815143260382E-28,1.)) ;
#40009 = DIRECTION('',(8.32667268460786E-17,1.,1.66321791214597E-16)) ;
#40010 = DIRECTION('',(2.17161023787787E-15,-3.83420712807771E-28,-1.)) ;
#40011 = DIRECTION('',(8.32667268460789E-17,1.,-3.83780830390118E-28)) ;
#40012 = DIRECTION('center_axis',(-1.,8.32667268460789E-17,-2.17161023787787E-15)) ;
#40013 = DIRECTION('ref_axis',(-1.47668185809765E-15,0.707106781186483,0.707106781186612)) ;
#40014 = DIRECTION('center_axis',(2.17161023787787E-15,-3.6685463379813E-28,
-1.)) ;
#40015 = DIRECTION('ref_axis',(-0.707106781186543,0.707106781186552,-1.53556032529782E-15)) ;
#40016 = DIRECTION('',(2.17161023787787E-15,-3.6685463379813E-28,-1.)) ;
#40017 = DIRECTION('center_axis',(1.88526971141291E-28,-2.90739654573716E-15,
-1.)) ;
#40018 = DIRECTION('ref_axis',(-1.,6.48092690620067E-15,-2.07369595641554E-28)) ;
#40019 = DIRECTION('center_axis',(3.33066907386739E-16,1.,-3.66031460022645E-28)) ;
#40020 = DIRECTION('ref_axis',(2.17161023787795E-15,-3.66754751528624E-28,
-1.)) ;
#40021 = DIRECTION('',(-2.1716102378779E-15,3.66854633798134E-28,1.)) ;
#40022 = DIRECTION('',(-1.,3.33066907386739E-16,-2.1716102378779E-15)) ;
#40023 = DIRECTION('center_axis',(-1.,3.33066907386739E-16,4.54195640846217E-14)) ;
#40024 = DIRECTION('ref_axis',(-3.23519956315716E-14,-0.707106781186623,-0.707106781186472)) ;
#40025 = DIRECTION('center_axis',(-1.,0.,0.)) ;
#40026 = DIRECTION('ref_axis',(0.,0.,-1.)) ;
#40027 = DIRECTION('',(-1.,3.33066907386739E-16,4.54195640846217E-14)) ;
#40028 = DIRECTION('center_axis',(1.,0.,0.)) ;
#40029 = DIRECTION('ref_axis',(0.,-1.,0.)) ;
#40030 = DIRECTION('center_axis',(4.54195640846217E-14,-1.66321791214601E-16,
1.)) ;
#40031 = DIRECTION('ref_axis',(1.,0.,-4.54747350886464E-14)) ;
#40032 = DIRECTION('center_axis',(0.,1.,0.)) ;
#40033 = DIRECTION('ref_axis',(1.,0.,-3.5527136788002E-14)) ;
#40034 = DIRECTION('center_axis',(2.17161023787787E-15,-3.6685463379813E-28,
-1.)) ;
#40035 = DIRECTION('ref_axis',(-0.707106781186543,0.707106781186552,-1.53556032529782E-15)) ;
#40036 = DIRECTION('center_axis',(-8.32667268460786E-17,-1.,-1.66321791214597E-16)) ;
#40037 = DIRECTION('ref_axis',(0.707106781186522,5.87287992268709E-17,-0.707106781186573)) ;
#40038 = DIRECTION('center_axis',(0.,1.,0.)) ;
#40039 = DIRECTION('ref_axis',(1.,0.,0.)) ;
#40040 = DIRECTION('',(-8.32667268460786E-17,-1.,-1.66321791214597E-16)) ;
#40041 = DIRECTION('center_axis',(4.54195640846217E-14,-1.66321791214601E-16,
1.)) ;
#40042 = DIRECTION('ref_axis',(1.,0.,-4.54747350886464E-14)) ;
#40043 = DIRECTION('center_axis',(-1.,-2.84217094303975E-13,0.)) ;
#40044 = DIRECTION('ref_axis',(-2.84217094303975E-13,1.,0.)) ;
#40045 = DIRECTION('center_axis',(-2.17161023787787E-15,3.6685463379813E-28,
1.)) ;
#40046 = DIRECTION('ref_axis',(-0.707106781186552,-0.707106781186543,-1.53556032529732E-15)) ;
#40047 = DIRECTION('center_axis',(1.,-3.33066907386739E-16,-4.54195640846217E-14)) ;
#40048 = DIRECTION('ref_axis',(-3.18809678939767E-14,0.707106781186422,-0.707106781186673)) ;
#40049 = DIRECTION('center_axis',(-1.,0.,0.)) ;
#40050 = DIRECTION('ref_axis',(0.,1.,0.)) ;
#40051 = DIRECTION('',(1.,-3.33066907386739E-16,-4.54195640846217E-14)) ;
#40052 = DIRECTION('center_axis',(4.54195640846217E-14,-1.66321791214601E-16,
1.)) ;
#40053 = DIRECTION('ref_axis',(1.,0.,-4.54747350886464E-14)) ;
#40054 = DIRECTION('center_axis',(0.,-1.,0.)) ;
#40055 = DIRECTION('ref_axis',(-1.,0.,3.5527136788007E-14)) ;
#40056 = DIRECTION('center_axis',(2.1716102378779E-15,-3.66854633798134E-28,
-1.)) ;
#40057 = DIRECTION('ref_axis',(0.707106781186543,-0.707106781186552,1.53556032529784E-15)) ;
#40058 = DIRECTION('center_axis',(1.66533453692965E-16,1.,1.66321791214593E-16)) ;
#40059 = DIRECTION('ref_axis',(-0.707106781186522,2.35364200827643E-16,-0.707106781186573)) ;
#40060 = DIRECTION('center_axis',(0.,-1.,0.)) ;
#40061 = DIRECTION('ref_axis',(-1.,0.,0.)) ;
#40062 = DIRECTION('',(1.66533453692965E-16,1.,1.66321791214593E-16)) ;
#40063 = DIRECTION('center_axis',(4.54195640846217E-14,-1.66321791214601E-16,
1.)) ;
#40064 = DIRECTION('ref_axis',(1.,0.,-4.54747350886464E-14)) ;
#40065 = DIRECTION('center_axis',(-2.1716102378779E-15,3.66854633798134E-28,
1.)) ;
#40066 = DIRECTION('ref_axis',(0.707106781186452,0.707106781186643,1.53556032529713E-15)) ;
#40067 = DIRECTION('center_axis',(-2.17161023787787E-15,3.6685463379813E-28,
1.)) ;
#40068 = DIRECTION('ref_axis',(-0.707106781186552,-0.707106781186543,-1.53556032529732E-15)) ;
#40069 = DIRECTION('',(2.17161023787787E-15,-3.6685463379813E-28,-1.)) ;
#40070 = DIRECTION('center_axis',(1.88526971141291E-28,-2.90739654573716E-15,
-1.)) ;
#40071 = DIRECTION('ref_axis',(1.35627620245787E-13,-1.,2.90739654573716E-15)) ;
#40072 = DIRECTION('',(-2.17161023787787E-15,3.6685463379813E-28,1.)) ;
#40073 = DIRECTION('center_axis',(-1.,8.32667268460789E-17,-2.17161023787787E-15)) ;
#40074 = DIRECTION('ref_axis',(8.32667268460789E-17,1.,-3.92101138914083E-28)) ;
#40075 = DIRECTION('',(-2.17161023787787E-15,3.6685463379813E-28,1.)) ;
#40076 = DIRECTION('center_axis',(-1.,8.32667268460789E-17,-2.17161023787787E-15)) ;
#40077 = DIRECTION('ref_axis',(-1.59443879249779E-15,-0.707106781186479,0.707106781186616)) ;
#40078 = DIRECTION('',(8.32667268460789E-17,1.,-3.83780830390118E-28)) ;
#40079 = DIRECTION('',(-2.17161023787787E-15,3.83815143260382E-28,1.)) ;
#40080 = DIRECTION('',(8.32667268460786E-17,1.,1.66321791214597E-16)) ;
#40081 = DIRECTION('',(2.17161023787787E-15,-3.83420712807771E-28,-1.)) ;
#40082 = DIRECTION('',(8.32667268460789E-17,1.,-3.83780830390118E-28)) ;
#40083 = DIRECTION('center_axis',(-1.,8.32667268460789E-17,-2.17161023787787E-15)) ;
#40084 = DIRECTION('ref_axis',(-1.47668185809765E-15,0.707106781186483,0.707106781186612)) ;
#40085 = DIRECTION('center_axis',(2.17161023787787E-15,-3.6685463379813E-28,
-1.)) ;
#40086 = DIRECTION('ref_axis',(-0.707106781186543,0.707106781186552,-1.53556032529782E-15)) ;
#40087 = DIRECTION('',(2.17161023787787E-15,-3.6685463379813E-28,-1.)) ;
#40088 = DIRECTION('center_axis',(1.88526971141291E-28,-2.90739654573716E-15,
-1.)) ;
#40089 = DIRECTION('ref_axis',(-1.,6.48092690620067E-15,-2.07369595641554E-28)) ;
#40090 = DIRECTION('center_axis',(3.33066907386739E-16,1.,-3.66031460022645E-28)) ;
#40091 = DIRECTION('ref_axis',(2.17161023787795E-15,-3.66754751528624E-28,
-1.)) ;
#40092 = DIRECTION('',(-2.1716102378779E-15,3.66854633798134E-28,1.)) ;
#40093 = DIRECTION('',(-1.,3.33066907386739E-16,-2.1716102378779E-15)) ;
#40094 = DIRECTION('center_axis',(-1.,3.33066907386739E-16,4.54195640846217E-14)) ;
#40095 = DIRECTION('ref_axis',(-3.23519956315716E-14,-0.707106781186623,-0.707106781186472)) ;
#40096 = DIRECTION('center_axis',(-1.,0.,0.)) ;
#40097 = DIRECTION('ref_axis',(0.,0.,-1.)) ;
#40098 = DIRECTION('',(-1.,3.33066907386739E-16,4.54195640846217E-14)) ;
#40099 = DIRECTION('center_axis',(1.,0.,0.)) ;
#40100 = DIRECTION('ref_axis',(0.,-1.,0.)) ;
#40101 = DIRECTION('center_axis',(4.54195640846217E-14,-1.66321791214601E-16,
1.)) ;
#40102 = DIRECTION('ref_axis',(1.,0.,-4.54747350886464E-14)) ;
#40103 = DIRECTION('center_axis',(0.,1.,0.)) ;
#40104 = DIRECTION('ref_axis',(1.,0.,-3.5527136788002E-14)) ;
#40105 = DIRECTION('center_axis',(2.17161023787787E-15,-3.6685463379813E-28,
-1.)) ;
#40106 = DIRECTION('ref_axis',(-0.707106781186543,0.707106781186552,-1.53556032529782E-15)) ;
#40107 = DIRECTION('center_axis',(-8.32667268460786E-17,-1.,-1.66321791214597E-16)) ;
#40108 = DIRECTION('ref_axis',(0.707106781186522,5.87287992268709E-17,-0.707106781186573)) ;
#40109 = DIRECTION('center_axis',(0.,1.,0.)) ;
#40110 = DIRECTION('ref_axis',(1.,0.,0.)) ;
#40111 = DIRECTION('',(-8.32667268460786E-17,-1.,-1.66321791214597E-16)) ;
#40112 = DIRECTION('center_axis',(4.54195640846217E-14,-1.66321791214601E-16,
1.)) ;
#40113 = DIRECTION('ref_axis',(1.,0.,-4.54747350886464E-14)) ;
#40114 = DIRECTION('center_axis',(-1.,-2.84217094303975E-13,0.)) ;
#40115 = DIRECTION('ref_axis',(-2.84217094303975E-13,1.,0.)) ;
#40116 = DIRECTION('center_axis',(-2.17161023787787E-15,3.6685463379813E-28,
1.)) ;
#40117 = DIRECTION('ref_axis',(-0.707106781186552,-0.707106781186543,-1.53556032529732E-15)) ;
#40118 = DIRECTION('center_axis',(1.,-3.33066907386739E-16,-4.54195640846217E-14)) ;
#40119 = DIRECTION('ref_axis',(-3.18809678939767E-14,0.707106781186422,-0.707106781186673)) ;
#40120 = DIRECTION('center_axis',(-1.,0.,0.)) ;
#40121 = DIRECTION('ref_axis',(0.,1.,0.)) ;
#40122 = DIRECTION('',(1.,-3.33066907386739E-16,-4.54195640846217E-14)) ;
#40123 = DIRECTION('center_axis',(4.54195640846217E-14,-1.66321791214601E-16,
1.)) ;
#40124 = DIRECTION('ref_axis',(1.,0.,-4.54747350886464E-14)) ;
#40125 = DIRECTION('center_axis',(0.,-1.,0.)) ;
#40126 = DIRECTION('ref_axis',(-1.,0.,3.5527136788007E-14)) ;
#40127 = DIRECTION('center_axis',(2.1716102378779E-15,-3.66854633798134E-28,
-1.)) ;
#40128 = DIRECTION('ref_axis',(0.707106781186543,-0.707106781186552,1.53556032529784E-15)) ;
#40129 = DIRECTION('center_axis',(1.66533453692965E-16,1.,1.66321791214593E-16)) ;
#40130 = DIRECTION('ref_axis',(-0.707106781186522,2.35364200827643E-16,-0.707106781186573)) ;
#40131 = DIRECTION('center_axis',(0.,-1.,0.)) ;
#40132 = DIRECTION('ref_axis',(-1.,0.,0.)) ;
#40133 = DIRECTION('',(1.66533453692965E-16,1.,1.66321791214593E-16)) ;
#40134 = DIRECTION('center_axis',(4.54195640846217E-14,-1.66321791214601E-16,
1.)) ;
#40135 = DIRECTION('ref_axis',(1.,0.,-4.54747350886464E-14)) ;
#40136 = DIRECTION('center_axis',(-2.1716102378779E-15,3.66854633798134E-28,
1.)) ;
#40137 = DIRECTION('ref_axis',(0.707106781186452,0.707106781186643,1.53556032529713E-15)) ;
#40138 = DIRECTION('center_axis',(-2.17161023787787E-15,3.6685463379813E-28,
1.)) ;
#40139 = DIRECTION('ref_axis',(-0.707106781186552,-0.707106781186543,-1.53556032529732E-15)) ;
#40140 = DIRECTION('',(2.17161023787787E-15,-3.6685463379813E-28,-1.)) ;
#40141 = DIRECTION('center_axis',(1.88526971141291E-28,-2.90739654573716E-15,
-1.)) ;
#40142 = DIRECTION('ref_axis',(1.35627620245787E-13,-1.,2.90739654573716E-15)) ;
#40143 = DIRECTION('',(-2.17161023787787E-15,3.6685463379813E-28,1.)) ;
#40144 = DIRECTION('center_axis',(-1.,8.32667268460789E-17,-2.17161023787787E-15)) ;
#40145 = DIRECTION('ref_axis',(8.32667268460789E-17,1.,-3.92101138914083E-28)) ;
#40146 = DIRECTION('',(-2.17161023787787E-15,3.6685463379813E-28,1.)) ;
#40147 = DIRECTION('center_axis',(-1.,8.32667268460789E-17,-2.17161023787787E-15)) ;
#40148 = DIRECTION('ref_axis',(-1.59443879249779E-15,-0.707106781186479,0.707106781186616)) ;
#40149 = DIRECTION('',(8.32667268460789E-17,1.,-3.83780830390118E-28)) ;
#40150 = DIRECTION('',(-2.17161023787787E-15,3.83815143260382E-28,1.)) ;
#40151 = DIRECTION('',(8.32667268460786E-17,1.,1.66321791214597E-16)) ;
#40152 = DIRECTION('',(2.17161023787787E-15,-3.83420712807771E-28,-1.)) ;
#40153 = DIRECTION('',(8.32667268460789E-17,1.,-3.83780830390118E-28)) ;
#40154 = DIRECTION('center_axis',(-1.,8.32667268460789E-17,-2.17161023787787E-15)) ;
#40155 = DIRECTION('ref_axis',(-1.47668185809765E-15,0.707106781186483,0.707106781186612)) ;
#40156 = DIRECTION('center_axis',(2.17161023787787E-15,-3.6685463379813E-28,
-1.)) ;
#40157 = DIRECTION('ref_axis',(-0.707106781186543,0.707106781186552,-1.53556032529782E-15)) ;
#40158 = DIRECTION('',(2.17161023787787E-15,-3.6685463379813E-28,-1.)) ;
#40159 = DIRECTION('center_axis',(1.88526971141291E-28,-2.90739654573716E-15,
-1.)) ;
#40160 = DIRECTION('ref_axis',(-1.,6.48092690620067E-15,-2.07369595641554E-28)) ;
#40161 = DIRECTION('center_axis',(3.33066907386739E-16,1.,-3.66031460022645E-28)) ;
#40162 = DIRECTION('ref_axis',(2.17161023787795E-15,-3.66754751528624E-28,
-1.)) ;
#40163 = DIRECTION('',(-2.1716102378779E-15,3.66854633798134E-28,1.)) ;
#40164 = DIRECTION('',(-1.,3.33066907386739E-16,-2.1716102378779E-15)) ;
#40165 = DIRECTION('center_axis',(-1.,3.33066907386739E-16,4.54195640846217E-14)) ;
#40166 = DIRECTION('ref_axis',(-3.23519956315716E-14,-0.707106781186623,-0.707106781186472)) ;
#40167 = DIRECTION('center_axis',(-1.,0.,0.)) ;
#40168 = DIRECTION('ref_axis',(0.,0.,-1.)) ;
#40169 = DIRECTION('',(-1.,3.33066907386739E-16,4.54195640846217E-14)) ;
#40170 = DIRECTION('center_axis',(1.,0.,0.)) ;
#40171 = DIRECTION('ref_axis',(0.,-1.,0.)) ;
#40172 = DIRECTION('center_axis',(4.54195640846217E-14,-1.66321791214601E-16,
1.)) ;
#40173 = DIRECTION('ref_axis',(1.,0.,-4.54747350886464E-14)) ;
#40174 = DIRECTION('center_axis',(0.,1.,0.)) ;
#40175 = DIRECTION('ref_axis',(1.,0.,-3.5527136788002E-14)) ;
#40176 = DIRECTION('center_axis',(2.17161023787787E-15,-3.6685463379813E-28,
-1.)) ;
#40177 = DIRECTION('ref_axis',(-0.707106781186543,0.707106781186552,-1.53556032529782E-15)) ;
#40178 = DIRECTION('center_axis',(-8.32667268460786E-17,-1.,-1.66321791214597E-16)) ;
#40179 = DIRECTION('ref_axis',(0.707106781186522,5.87287992268709E-17,-0.707106781186573)) ;
#40180 = DIRECTION('center_axis',(0.,1.,0.)) ;
#40181 = DIRECTION('ref_axis',(1.,0.,0.)) ;
#40182 = DIRECTION('',(-8.32667268460786E-17,-1.,-1.66321791214597E-16)) ;
#40183 = DIRECTION('center_axis',(4.54195640846217E-14,-1.66321791214601E-16,
1.)) ;
#40184 = DIRECTION('ref_axis',(1.,0.,-4.54747350886464E-14)) ;
#40185 = DIRECTION('center_axis',(-1.,-2.84217094303975E-13,0.)) ;
#40186 = DIRECTION('ref_axis',(-2.84217094303975E-13,1.,0.)) ;
#40187 = DIRECTION('center_axis',(-2.17161023787787E-15,3.6685463379813E-28,
1.)) ;
#40188 = DIRECTION('ref_axis',(-0.707106781186552,-0.707106781186543,-1.53556032529732E-15)) ;
#40189 = DIRECTION('center_axis',(1.,-3.33066907386739E-16,-4.54195640846217E-14)) ;
#40190 = DIRECTION('ref_axis',(-3.18809678939767E-14,0.707106781186422,-0.707106781186673)) ;
#40191 = DIRECTION('center_axis',(-1.,0.,0.)) ;
#40192 = DIRECTION('ref_axis',(0.,1.,0.)) ;
#40193 = DIRECTION('',(1.,-3.33066907386739E-16,-4.54195640846217E-14)) ;
#40194 = DIRECTION('center_axis',(4.54195640846217E-14,-1.66321791214601E-16,
1.)) ;
#40195 = DIRECTION('ref_axis',(1.,0.,-4.54747350886464E-14)) ;
#40196 = DIRECTION('center_axis',(0.,-1.,0.)) ;
#40197 = DIRECTION('ref_axis',(-1.,0.,3.5527136788007E-14)) ;
#40198 = DIRECTION('center_axis',(2.1716102378779E-15,-3.66854633798134E-28,
-1.)) ;
#40199 = DIRECTION('ref_axis',(0.707106781186543,-0.707106781186552,1.53556032529784E-15)) ;
#40200 = DIRECTION('center_axis',(1.66533453692965E-16,1.,1.66321791214593E-16)) ;
#40201 = DIRECTION('ref_axis',(-0.707106781186522,2.35364200827643E-16,-0.707106781186573)) ;
#40202 = DIRECTION('center_axis',(0.,-1.,0.)) ;
#40203 = DIRECTION('ref_axis',(-1.,0.,0.)) ;
#40204 = DIRECTION('',(1.66533453692965E-16,1.,1.66321791214593E-16)) ;
#40205 = DIRECTION('center_axis',(4.54195640846217E-14,-1.66321791214601E-16,
1.)) ;
#40206 = DIRECTION('ref_axis',(1.,0.,-4.54747350886464E-14)) ;
#40207 = DIRECTION('center_axis',(-2.1716102378779E-15,3.66854633798134E-28,
1.)) ;
#40208 = DIRECTION('ref_axis',(0.707106781186452,0.707106781186643,1.53556032529713E-15)) ;
#40209 = DIRECTION('center_axis',(-2.17161023787787E-15,3.6685463379813E-28,
1.)) ;
#40210 = DIRECTION('ref_axis',(-0.707106781186552,-0.707106781186543,-1.53556032529732E-15)) ;
#40211 = DIRECTION('',(2.17161023787787E-15,-3.6685463379813E-28,-1.)) ;
#40212 = DIRECTION('center_axis',(1.88526971141291E-28,-2.90739654573716E-15,
-1.)) ;
#40213 = DIRECTION('ref_axis',(1.35627620245787E-13,-1.,2.90739654573716E-15)) ;
#40214 = DIRECTION('',(-2.17161023787787E-15,3.6685463379813E-28,1.)) ;
#40215 = DIRECTION('center_axis',(-1.,8.32667268460789E-17,-2.17161023787787E-15)) ;
#40216 = DIRECTION('ref_axis',(8.32667268460789E-17,1.,-3.92101138914083E-28)) ;
#40217 = DIRECTION('',(-2.17161023787787E-15,3.6685463379813E-28,1.)) ;
#40218 = DIRECTION('center_axis',(-1.,8.32667268460789E-17,-2.17161023787787E-15)) ;
#40219 = DIRECTION('ref_axis',(-1.59443879249779E-15,-0.707106781186479,0.707106781186616)) ;
#40220 = DIRECTION('',(8.32667268460789E-17,1.,-3.83780830390118E-28)) ;
#40221 = DIRECTION('',(-2.17161023787787E-15,3.83815143260382E-28,1.)) ;
#40222 = DIRECTION('',(8.32667268460786E-17,1.,1.66321791214597E-16)) ;
#40223 = DIRECTION('',(2.17161023787787E-15,-3.83420712807771E-28,-1.)) ;
#40224 = DIRECTION('',(8.32667268460789E-17,1.,-3.83780830390118E-28)) ;
#40225 = DIRECTION('center_axis',(-1.,8.32667268460789E-17,-2.17161023787787E-15)) ;
#40226 = DIRECTION('ref_axis',(-1.47668185809765E-15,0.707106781186483,0.707106781186612)) ;
#40227 = DIRECTION('center_axis',(2.17161023787787E-15,-3.6685463379813E-28,
-1.)) ;
#40228 = DIRECTION('ref_axis',(-0.707106781186543,0.707106781186552,-1.53556032529782E-15)) ;
#40229 = DIRECTION('',(2.17161023787787E-15,-3.6685463379813E-28,-1.)) ;
#40230 = DIRECTION('center_axis',(1.88526971141291E-28,-2.90739654573716E-15,
-1.)) ;
#40231 = DIRECTION('ref_axis',(-1.,6.48092690620067E-15,-2.07369595641554E-28)) ;
#40232 = DIRECTION('center_axis',(3.33066907386739E-16,1.,-3.66031460022645E-28)) ;
#40233 = DIRECTION('ref_axis',(2.17161023787795E-15,-3.66754751528624E-28,
-1.)) ;
#40234 = DIRECTION('',(-2.1716102378779E-15,3.66854633798134E-28,1.)) ;
#40235 = DIRECTION('',(-1.,3.33066907386739E-16,-2.1716102378779E-15)) ;
#40236 = DIRECTION('center_axis',(-1.,3.33066907386739E-16,4.54195640846217E-14)) ;
#40237 = DIRECTION('ref_axis',(-3.23519956315716E-14,-0.707106781186623,-0.707106781186472)) ;
#40238 = DIRECTION('center_axis',(-1.,0.,0.)) ;
#40239 = DIRECTION('ref_axis',(0.,0.,-1.)) ;
#40240 = DIRECTION('',(-1.,3.33066907386739E-16,4.54195640846217E-14)) ;
#40241 = DIRECTION('center_axis',(1.,0.,0.)) ;
#40242 = DIRECTION('ref_axis',(0.,-1.,0.)) ;
#40243 = DIRECTION('center_axis',(4.54195640846217E-14,-1.66321791214601E-16,
1.)) ;
#40244 = DIRECTION('ref_axis',(1.,0.,-4.54747350886464E-14)) ;
#40245 = DIRECTION('center_axis',(0.,1.,0.)) ;
#40246 = DIRECTION('ref_axis',(1.,0.,-3.5527136788002E-14)) ;
#40247 = DIRECTION('center_axis',(2.17161023787787E-15,-3.6685463379813E-28,
-1.)) ;
#40248 = DIRECTION('ref_axis',(-0.707106781186543,0.707106781186552,-1.53556032529782E-15)) ;
#40249 = DIRECTION('center_axis',(-8.32667268460786E-17,-1.,-1.66321791214597E-16)) ;
#40250 = DIRECTION('ref_axis',(0.707106781186522,5.87287992268709E-17,-0.707106781186573)) ;
#40251 = DIRECTION('center_axis',(0.,1.,0.)) ;
#40252 = DIRECTION('ref_axis',(1.,0.,0.)) ;
#40253 = DIRECTION('',(-8.32667268460786E-17,-1.,-1.66321791214597E-16)) ;
#40254 = DIRECTION('center_axis',(4.54195640846217E-14,-1.66321791214601E-16,
1.)) ;
#40255 = DIRECTION('ref_axis',(1.,0.,-4.54747350886464E-14)) ;
#40256 = DIRECTION('center_axis',(-1.,-2.84217094303975E-13,0.)) ;
#40257 = DIRECTION('ref_axis',(-2.84217094303975E-13,1.,0.)) ;
#40258 = DIRECTION('center_axis',(-2.17161023787787E-15,3.6685463379813E-28,
1.)) ;
#40259 = DIRECTION('ref_axis',(-0.707106781186552,-0.707106781186543,-1.53556032529732E-15)) ;
#40260 = DIRECTION('center_axis',(1.,-3.33066907386739E-16,-4.54195640846217E-14)) ;
#40261 = DIRECTION('ref_axis',(-3.18809678939767E-14,0.707106781186422,-0.707106781186673)) ;
#40262 = DIRECTION('center_axis',(-1.,0.,0.)) ;
#40263 = DIRECTION('ref_axis',(0.,1.,0.)) ;
#40264 = DIRECTION('',(1.,-3.33066907386739E-16,-4.54195640846217E-14)) ;
#40265 = DIRECTION('center_axis',(4.54195640846217E-14,-1.66321791214601E-16,
1.)) ;
#40266 = DIRECTION('ref_axis',(1.,0.,-4.54747350886464E-14)) ;
#40267 = DIRECTION('center_axis',(0.,-1.,0.)) ;
#40268 = DIRECTION('ref_axis',(-1.,0.,3.5527136788007E-14)) ;
#40269 = DIRECTION('center_axis',(2.1716102378779E-15,-3.66854633798134E-28,
-1.)) ;
#40270 = DIRECTION('ref_axis',(0.707106781186543,-0.707106781186552,1.53556032529784E-15)) ;
#40271 = DIRECTION('center_axis',(1.66533453692965E-16,1.,1.66321791214593E-16)) ;
#40272 = DIRECTION('ref_axis',(-0.707106781186522,2.35364200827643E-16,-0.707106781186573)) ;
#40273 = DIRECTION('center_axis',(0.,-1.,0.)) ;
#40274 = DIRECTION('ref_axis',(-1.,0.,0.)) ;
#40275 = DIRECTION('',(1.66533453692965E-16,1.,1.66321791214593E-16)) ;
#40276 = DIRECTION('center_axis',(4.54195640846217E-14,-1.66321791214601E-16,
1.)) ;
#40277 = DIRECTION('ref_axis',(1.,0.,-4.54747350886464E-14)) ;
#40278 = DIRECTION('center_axis',(-2.1716102378779E-15,3.66854633798134E-28,
1.)) ;
#40279 = DIRECTION('ref_axis',(0.707106781186452,0.707106781186643,1.53556032529713E-15)) ;
#40280 = DIRECTION('center_axis',(-2.17161023787787E-15,3.6685463379813E-28,
1.)) ;
#40281 = DIRECTION('ref_axis',(-0.707106781186552,-0.707106781186543,-1.53556032529732E-15)) ;
#40282 = DIRECTION('',(2.17161023787787E-15,-3.6685463379813E-28,-1.)) ;
#40283 = DIRECTION('center_axis',(1.88526971141291E-28,-2.90739654573716E-15,
-1.)) ;
#40284 = DIRECTION('ref_axis',(1.35627620245787E-13,-1.,2.90739654573716E-15)) ;
#40285 = DIRECTION('',(-2.17161023787787E-15,3.6685463379813E-28,1.)) ;
#40286 = DIRECTION('center_axis',(-1.,8.32667268460789E-17,-2.17161023787787E-15)) ;
#40287 = DIRECTION('ref_axis',(8.32667268460789E-17,1.,-3.92101138914083E-28)) ;
#40288 = DIRECTION('',(-2.17161023787787E-15,3.6685463379813E-28,1.)) ;
#40289 = DIRECTION('center_axis',(-1.,8.32667268460789E-17,-2.17161023787787E-15)) ;
#40290 = DIRECTION('ref_axis',(-1.59443879249779E-15,-0.707106781186479,0.707106781186616)) ;
#40291 = DIRECTION('',(8.32667268460789E-17,1.,-3.83780830390118E-28)) ;
#40292 = DIRECTION('',(-2.17161023787787E-15,3.83815143260382E-28,1.)) ;
#40293 = DIRECTION('',(8.32667268460786E-17,1.,1.66321791214597E-16)) ;
#40294 = DIRECTION('',(2.17161023787787E-15,-3.83420712807771E-28,-1.)) ;
#40295 = DIRECTION('',(8.32667268460789E-17,1.,-3.83780830390118E-28)) ;
#40296 = DIRECTION('center_axis',(-1.,8.32667268460789E-17,-2.17161023787787E-15)) ;
#40297 = DIRECTION('ref_axis',(-1.47668185809765E-15,0.707106781186483,0.707106781186612)) ;
#40298 = DIRECTION('center_axis',(2.17161023787787E-15,-3.6685463379813E-28,
-1.)) ;
#40299 = DIRECTION('ref_axis',(-0.707106781186543,0.707106781186552,-1.53556032529782E-15)) ;
#40300 = DIRECTION('',(2.17161023787787E-15,-3.6685463379813E-28,-1.)) ;
#40301 = DIRECTION('center_axis',(1.88526971141291E-28,-2.90739654573716E-15,
-1.)) ;
#40302 = DIRECTION('ref_axis',(-1.,6.48092690620067E-15,-2.07369595641554E-28)) ;
#40303 = DIRECTION('center_axis',(3.33066907386739E-16,1.,-3.66031460022645E-28)) ;
#40304 = DIRECTION('ref_axis',(2.17161023787795E-15,-3.66754751528624E-28,
-1.)) ;
#40305 = DIRECTION('',(-2.1716102378779E-15,3.66854633798134E-28,1.)) ;
#40306 = DIRECTION('',(-1.,3.33066907386739E-16,-2.1716102378779E-15)) ;
#40307 = DIRECTION('center_axis',(-1.,3.33066907386739E-16,4.54195640846217E-14)) ;
#40308 = DIRECTION('ref_axis',(-3.23519956315716E-14,-0.707106781186623,-0.707106781186472)) ;
#40309 = DIRECTION('center_axis',(-1.,0.,0.)) ;
#40310 = DIRECTION('ref_axis',(0.,0.,-1.)) ;
#40311 = DIRECTION('',(-1.,3.33066907386739E-16,4.54195640846217E-14)) ;
#40312 = DIRECTION('center_axis',(1.,0.,0.)) ;
#40313 = DIRECTION('ref_axis',(0.,-1.,0.)) ;
#40314 = DIRECTION('center_axis',(4.54195640846217E-14,-1.66321791214601E-16,
1.)) ;
#40315 = DIRECTION('ref_axis',(1.,0.,-4.54747350886464E-14)) ;
#40316 = DIRECTION('center_axis',(0.,1.,0.)) ;
#40317 = DIRECTION('ref_axis',(1.,0.,-3.5527136788002E-14)) ;
#40318 = DIRECTION('center_axis',(4.54195640846217E-14,-1.66321791214601E-16,
1.)) ;
#40319 = DIRECTION('ref_axis',(-0.707106781186502,0.707106781186593,3.22340890291979E-14)) ;
#40320 = DIRECTION('center_axis',(-8.32667268460786E-17,-1.,-1.66321791214597E-16)) ;
#40321 = DIRECTION('ref_axis',(0.707106781186522,5.87287992268709E-17,-0.707106781186573)) ;
#40322 = DIRECTION('center_axis',(0.,1.,0.)) ;
#40323 = DIRECTION('ref_axis',(1.,0.,0.)) ;
#40324 = DIRECTION('',(-8.32667268460786E-17,-1.,-1.66321791214597E-16)) ;
#40325 = DIRECTION('center_axis',(4.54195640846217E-14,-1.66321791214601E-16,
1.)) ;
#40326 = DIRECTION('ref_axis',(1.,0.,-4.54747350886464E-14)) ;
#40327 = DIRECTION('center_axis',(-1.,-2.84217094303975E-13,0.)) ;
#40328 = DIRECTION('ref_axis',(-2.84217094303975E-13,1.,0.)) ;
#40329 = DIRECTION('center_axis',(4.54195640846217E-14,-1.66321791214601E-16,
1.)) ;
#40330 = DIRECTION('ref_axis',(-0.707106781186502,-0.707106781186593,3.1998874496344E-14)) ;
#40331 = DIRECTION('center_axis',(1.,-3.33066907386739E-16,-4.54195640846217E-14)) ;
#40332 = DIRECTION('ref_axis',(-3.18809678939767E-14,0.707106781186422,-0.707106781186673)) ;
#40333 = DIRECTION('center_axis',(-1.,0.,0.)) ;
#40334 = DIRECTION('ref_axis',(0.,1.,0.)) ;
#40335 = DIRECTION('',(1.,-3.33066907386739E-16,-4.54195640846217E-14)) ;
#40336 = DIRECTION('center_axis',(4.54195640846217E-14,-1.66321791214601E-16,
1.)) ;
#40337 = DIRECTION('ref_axis',(1.,0.,-4.54747350886464E-14)) ;
#40338 = DIRECTION('center_axis',(0.,-1.,0.)) ;
#40339 = DIRECTION('ref_axis',(-1.,0.,3.5527136788007E-14)) ;
#40340 = DIRECTION('center_axis',(4.54195640846217E-14,-1.66321791214601E-16,
1.)) ;
#40341 = DIRECTION('ref_axis',(0.707106781186593,-0.707106781186502,-3.2234089029202E-14)) ;
#40342 = DIRECTION('center_axis',(1.66533453692965E-16,1.,1.66321791214593E-16)) ;
#40343 = DIRECTION('ref_axis',(-0.707106781186522,2.35364200827643E-16,-0.707106781186573)) ;
#40344 = DIRECTION('center_axis',(0.,-1.,0.)) ;
#40345 = DIRECTION('ref_axis',(-1.,0.,0.)) ;
#40346 = DIRECTION('',(1.66533453692965E-16,1.,1.66321791214593E-16)) ;
#40347 = DIRECTION('center_axis',(4.54195640846217E-14,-1.66321791214601E-16,
1.)) ;
#40348 = DIRECTION('ref_axis',(1.,0.,-4.54747350886464E-14)) ;
#40349 = DIRECTION('center_axis',(4.54195640846217E-14,-1.66321791214601E-16,
1.)) ;
#40350 = DIRECTION('ref_axis',(0.707106781186593,0.707106781186502,-3.19988744963481E-14)) ;
#40351 = DIRECTION('center_axis',(-2.17161023787787E-15,3.6685463379813E-28,
1.)) ;
#40352 = DIRECTION('ref_axis',(-0.707106781186552,-0.707106781186543,-1.53556032529732E-15)) ;
#40353 = DIRECTION('',(2.17161023787787E-15,-3.6685463379813E-28,-1.)) ;
#40354 = DIRECTION('center_axis',(1.88526971141291E-28,-2.90739654573716E-15,
-1.)) ;
#40355 = DIRECTION('ref_axis',(1.35627620245787E-13,-1.,2.90739654573716E-15)) ;
#40356 = DIRECTION('',(-2.17161023787787E-15,3.6685463379813E-28,1.)) ;
#40357 = DIRECTION('center_axis',(-1.,8.32667268460789E-17,-2.17161023787787E-15)) ;
#40358 = DIRECTION('ref_axis',(8.32667268460789E-17,1.,-3.92101138914083E-28)) ;
#40359 = DIRECTION('',(8.32667268460786E-17,1.,1.66321791214597E-16)) ;
#40360 = DIRECTION('',(2.17161023787787E-15,-3.83420712807771E-28,-1.)) ;
#40361 = DIRECTION('',(8.32667268460789E-17,1.,-3.83780830390118E-28)) ;
#40362 = DIRECTION('center_axis',(-1.,8.32667268460789E-17,-2.17161023787787E-15)) ;
#40363 = DIRECTION('ref_axis',(-1.47668185809765E-15,0.707106781186483,0.707106781186612)) ;
#40364 = DIRECTION('',(-2.17161023787787E-15,3.6685463379813E-28,1.)) ;
#40365 = DIRECTION('center_axis',(-1.,8.32667268460789E-17,-2.17161023787787E-15)) ;
#40366 = DIRECTION('ref_axis',(-1.59443879249779E-15,-0.707106781186479,0.707106781186616)) ;
#40367 = DIRECTION('',(8.32667268460789E-17,1.,-3.83780830390118E-28)) ;
#40368 = DIRECTION('',(-2.17161023787787E-15,3.83815143260382E-28,1.)) ;
#40369 = DIRECTION('center_axis',(2.17161023787787E-15,-3.6685463379813E-28,
-1.)) ;
#40370 = DIRECTION('ref_axis',(-0.707106781186543,0.707106781186552,-1.53556032529782E-15)) ;
#40371 = DIRECTION('',(2.17161023787787E-15,-3.6685463379813E-28,-1.)) ;
#40372 = DIRECTION('center_axis',(1.88526971141291E-28,-2.90739654573716E-15,
-1.)) ;
#40373 = DIRECTION('ref_axis',(-1.,6.48092690620067E-15,-2.07369595641554E-28)) ;
#40374 = DIRECTION('center_axis',(3.33066907386739E-16,1.,-3.66031460022645E-28)) ;
#40375 = DIRECTION('ref_axis',(2.17161023787795E-15,-3.66754751528624E-28,
-1.)) ;
#40376 = DIRECTION('',(-2.1716102378779E-15,3.66854633798134E-28,1.)) ;
#40377 = DIRECTION('',(-1.,3.33066907386739E-16,-2.1716102378779E-15)) ;
#40378 = DIRECTION('center_axis',(1.,-1.66533453692966E-16,-4.54195640846217E-14)) ;
#40379 = DIRECTION('ref_axis',(3.19987248283774E-14,-0.707106781186434,0.707106781186661)) ;
#40380 = DIRECTION('center_axis',(1.,0.,0.)) ;
#40381 = DIRECTION('ref_axis',(0.,0.,1.)) ;
#40382 = DIRECTION('',(1.,-1.66533453692966E-16,-4.54195640846217E-14)) ;
#40383 = DIRECTION('center_axis',(-1.,0.,0.)) ;
#40384 = DIRECTION('ref_axis',(0.,-1.,0.)) ;
#40385 = DIRECTION('',(1.,-1.66533453692966E-16,-4.54195640846217E-14)) ;
#40386 = DIRECTION('center_axis',(-4.54195640846217E-14,1.66321791214601E-16,
-1.)) ;
#40387 = DIRECTION('ref_axis',(-1.,0.,4.54747350886464E-14)) ;
#40388 = DIRECTION('center_axis',(0.,1.,0.)) ;
#40389 = DIRECTION('ref_axis',(-1.,0.,5.32907051820105E-14)) ;
#40390 = DIRECTION('center_axis',(4.54195640846217E-14,-1.66321791214601E-16,
1.)) ;
#40391 = DIRECTION('ref_axis',(-1.,5.55236256206829E-46,4.54195640846217E-14)) ;
#40392 = DIRECTION('center_axis',(2.17161023787787E-15,-3.83815143260382E-28,
-1.)) ;
#40393 = DIRECTION('ref_axis',(0.707106781186452,0.707106781186643,1.53556032529709E-15)) ;
#40394 = DIRECTION('center_axis',(-8.32667268460786E-17,-1.,-1.66321791214597E-16)) ;
#40395 = DIRECTION('ref_axis',(-0.707106781186535,-5.87287992268677E-17,0.70710678118656)) ;
#40396 = DIRECTION('center_axis',(0.,1.,0.)) ;
#40397 = DIRECTION('ref_axis',(-1.,0.,0.)) ;
#40398 = DIRECTION('',(-8.32667268460786E-17,-1.,-1.66321791214597E-16)) ;
#40399 = DIRECTION('',(-8.32667268460786E-17,-1.,-1.66321791214597E-16)) ;
#40400 = DIRECTION('center_axis',(-4.54195640846217E-14,1.66321791214601E-16,
-1.)) ;
#40401 = DIRECTION('ref_axis',(-1.,0.,4.54747350886464E-14)) ;
#40402 = DIRECTION('center_axis',(1.,2.84217094304056E-13,0.)) ;
#40403 = DIRECTION('ref_axis',(-2.84217094304056E-13,1.,0.)) ;
#40404 = DIRECTION('center_axis',(4.54195640846217E-14,-1.66321791214601E-16,
1.)) ;
#40405 = DIRECTION('ref_axis',(-1.,5.55236256206829E-46,4.54195640846217E-14)) ;
#40406 = DIRECTION('center_axis',(-2.17161023787787E-15,3.83420712807771E-28,
1.)) ;
#40407 = DIRECTION('ref_axis',(0.707106781186543,-0.707106781186552,1.53556032529783E-15)) ;
#40408 = DIRECTION('center_axis',(-1.,1.66533453692587E-16,4.54195640846217E-14)) ;
#40409 = DIRECTION('ref_axis',(3.22342386971791E-14,0.707106781186422,0.707106781186673)) ;
#40410 = DIRECTION('center_axis',(1.,0.,0.)) ;
#40411 = DIRECTION('ref_axis',(0.,1.,0.)) ;
#40412 = DIRECTION('',(-1.,1.66533453692587E-16,4.54195640846217E-14)) ;
#40413 = DIRECTION('',(-1.,1.66533453692587E-16,4.54195640846217E-14)) ;
#40414 = DIRECTION('center_axis',(-4.54195640846217E-14,1.66321791214601E-16,
-1.)) ;
#40415 = DIRECTION('ref_axis',(-1.,0.,4.54747350886464E-14)) ;
#40416 = DIRECTION('center_axis',(0.,-1.,0.)) ;
#40417 = DIRECTION('ref_axis',(1.,0.,-5.32907051820105E-14)) ;
#40418 = DIRECTION('center_axis',(4.54195640846217E-14,-1.66321791214601E-16,
1.)) ;
#40419 = DIRECTION('ref_axis',(-1.,5.55236256206829E-46,4.54195640846217E-14)) ;
#40420 = DIRECTION('center_axis',(2.1716102378779E-15,-3.83420712807775E-28,
-1.)) ;
#40421 = DIRECTION('ref_axis',(-0.707106781186452,-0.707106781186643,-1.53556032529712E-15)) ;
#40422 = DIRECTION('center_axis',(1.66533453692965E-16,1.,1.66321791214593E-16)) ;
#40423 = DIRECTION('ref_axis',(0.707106781186535,-2.35364200827643E-16,0.70710678118656)) ;
#40424 = DIRECTION('center_axis',(0.,-1.,0.)) ;
#40425 = DIRECTION('ref_axis',(1.,0.,0.)) ;
#40426 = DIRECTION('',(1.66533453692965E-16,1.,1.66321791214593E-16)) ;
#40427 = DIRECTION('',(1.66533453692965E-16,1.,1.66321791214593E-16)) ;
#40428 = DIRECTION('center_axis',(-4.54195640846217E-14,1.66321791214601E-16,
-1.)) ;
#40429 = DIRECTION('ref_axis',(-1.,0.,4.54747350886464E-14)) ;
#40430 = DIRECTION('center_axis',(4.54195640846217E-14,-1.66321791214601E-16,
1.)) ;
#40431 = DIRECTION('ref_axis',(-1.,5.55236256206829E-46,4.54195640846217E-14)) ;
#40432 = DIRECTION('center_axis',(-2.1716102378779E-15,3.83815143260386E-28,
1.)) ;
#40433 = DIRECTION('ref_axis',(-0.707106781186643,0.707106781186452,-1.53556032529807E-15)) ;
#40434 = DIRECTION('center_axis',(-2.17161023787787E-15,3.83420712807771E-28,
1.)) ;
#40435 = DIRECTION('ref_axis',(0.707106781186543,-0.707106781186552,1.53556032529783E-15)) ;
#40436 = DIRECTION('',(-2.17161023787787E-15,3.83420712807771E-28,1.)) ;
#40437 = DIRECTION('center_axis',(2.17161023787792E-15,-2.90739654573749E-15,
-1.)) ;
#40438 = DIRECTION('ref_axis',(1.35627620245787E-13,-1.,2.90739654573778E-15)) ;
#40439 = DIRECTION('',(2.17161023787787E-15,-3.83420712807771E-28,-1.)) ;
#40440 = DIRECTION('center_axis',(1.,-8.32667268460789E-17,2.17161023787787E-15)) ;
#40441 = DIRECTION('ref_axis',(-8.32667268460789E-17,-1.,3.92101138914083E-28)) ;
#40442 = DIRECTION('',(2.17161023787787E-15,-3.83815143260382E-28,-1.)) ;
#40443 = DIRECTION('',(-8.32667268460789E-17,-1.,3.83780830390118E-28)) ;
#40444 = DIRECTION('center_axis',(2.17161023787787E-15,-3.83815143260382E-28,
-1.)) ;
#40445 = DIRECTION('ref_axis',(0.707106781186452,0.707106781186643,1.53556032529709E-15)) ;
#40446 = DIRECTION('',(-2.17161023787787E-15,3.83815143260382E-28,1.)) ;
#40447 = DIRECTION('center_axis',(2.17161023787746E-15,-7.39616701217516E-14,
-1.)) ;
#40448 = DIRECTION('ref_axis',(1.,-6.48092690624108E-15,2.17161023787794E-15)) ;
#40449 = DIRECTION('center_axis',(1.66533453692966E-16,1.,-3.83386399937507E-28)) ;
#40450 = DIRECTION('ref_axis',(2.1716102378779E-15,-3.83748045690496E-28,
-1.)) ;
#40451 = DIRECTION('',(2.1716102378779E-15,-3.83815143260386E-28,-1.)) ;
#40452 = DIRECTION('',(1.,-1.66533453692966E-16,2.1716102378779E-15)) ;
#40453 = DIRECTION('center_axis',(1.,-1.66533453692966E-16,-4.54195640846217E-14)) ;
#40454 = DIRECTION('ref_axis',(3.19987248283774E-14,-0.707106781186434,0.707106781186661)) ;
#40455 = DIRECTION('center_axis',(1.,0.,0.)) ;
#40456 = DIRECTION('ref_axis',(0.,0.,1.)) ;
#40457 = DIRECTION('',(1.,-1.66533453692966E-16,-4.54195640846217E-14)) ;
#40458 = DIRECTION('center_axis',(-1.,0.,0.)) ;
#40459 = DIRECTION('ref_axis',(0.,-1.,0.)) ;
#40460 = DIRECTION('',(1.,-1.66533453692966E-16,-4.54195640846217E-14)) ;
#40461 = DIRECTION('center_axis',(-4.54195640846217E-14,1.66321791214601E-16,
-1.)) ;
#40462 = DIRECTION('ref_axis',(-1.,0.,4.54747350886464E-14)) ;
#40463 = DIRECTION('center_axis',(0.,1.,0.)) ;
#40464 = DIRECTION('ref_axis',(-1.,0.,5.32907051820105E-14)) ;
#40465 = DIRECTION('center_axis',(4.54195640846217E-14,-1.66321791214601E-16,
1.)) ;
#40466 = DIRECTION('ref_axis',(-1.,5.55236256206829E-46,4.54195640846217E-14)) ;
#40467 = DIRECTION('center_axis',(2.17161023787787E-15,-3.83815143260382E-28,
-1.)) ;
#40468 = DIRECTION('ref_axis',(0.707106781186452,0.707106781186643,1.53556032529709E-15)) ;
#40469 = DIRECTION('center_axis',(-8.32667268460786E-17,-1.,-1.66321791214597E-16)) ;
#40470 = DIRECTION('ref_axis',(-0.707106781186535,-5.87287992268677E-17,0.70710678118656)) ;
#40471 = DIRECTION('center_axis',(0.,1.,0.)) ;
#40472 = DIRECTION('ref_axis',(-1.,0.,0.)) ;
#40473 = DIRECTION('',(-8.32667268460786E-17,-1.,-1.66321791214597E-16)) ;
#40474 = DIRECTION('',(-8.32667268460786E-17,-1.,-1.66321791214597E-16)) ;
#40475 = DIRECTION('center_axis',(-4.54195640846217E-14,1.66321791214601E-16,
-1.)) ;
#40476 = DIRECTION('ref_axis',(-1.,0.,4.54747350886464E-14)) ;
#40477 = DIRECTION('center_axis',(1.,2.84217094304056E-13,0.)) ;
#40478 = DIRECTION('ref_axis',(-2.84217094304056E-13,1.,0.)) ;
#40479 = DIRECTION('center_axis',(4.54195640846217E-14,-1.66321791214601E-16,
1.)) ;
#40480 = DIRECTION('ref_axis',(-1.,5.55236256206829E-46,4.54195640846217E-14)) ;
#40481 = DIRECTION('center_axis',(-2.17161023787787E-15,3.83420712807771E-28,
1.)) ;
#40482 = DIRECTION('ref_axis',(0.707106781186543,-0.707106781186552,1.53556032529783E-15)) ;
#40483 = DIRECTION('center_axis',(-1.,1.66533453692587E-16,4.54195640846217E-14)) ;
#40484 = DIRECTION('ref_axis',(3.22342386971791E-14,0.707106781186422,0.707106781186673)) ;
#40485 = DIRECTION('center_axis',(1.,0.,0.)) ;
#40486 = DIRECTION('ref_axis',(0.,1.,0.)) ;
#40487 = DIRECTION('',(-1.,1.66533453692587E-16,4.54195640846217E-14)) ;
#40488 = DIRECTION('',(-1.,1.66533453692587E-16,4.54195640846217E-14)) ;
#40489 = DIRECTION('center_axis',(-4.54195640846217E-14,1.66321791214601E-16,
-1.)) ;
#40490 = DIRECTION('ref_axis',(-1.,0.,4.54747350886464E-14)) ;
#40491 = DIRECTION('center_axis',(0.,-1.,0.)) ;
#40492 = DIRECTION('ref_axis',(1.,0.,-5.32907051820105E-14)) ;
#40493 = DIRECTION('center_axis',(4.54195640846217E-14,-1.66321791214601E-16,
1.)) ;
#40494 = DIRECTION('ref_axis',(-1.,5.55236256206829E-46,4.54195640846217E-14)) ;
#40495 = DIRECTION('center_axis',(2.1716102378779E-15,-3.83420712807775E-28,
-1.)) ;
#40496 = DIRECTION('ref_axis',(-0.707106781186452,-0.707106781186643,-1.53556032529712E-15)) ;
#40497 = DIRECTION('center_axis',(1.66533453692965E-16,1.,1.66321791214593E-16)) ;
#40498 = DIRECTION('ref_axis',(0.707106781186535,-2.35364200827643E-16,0.70710678118656)) ;
#40499 = DIRECTION('center_axis',(0.,-1.,0.)) ;
#40500 = DIRECTION('ref_axis',(1.,0.,0.)) ;
#40501 = DIRECTION('',(1.66533453692965E-16,1.,1.66321791214593E-16)) ;
#40502 = DIRECTION('',(1.66533453692965E-16,1.,1.66321791214593E-16)) ;
#40503 = DIRECTION('center_axis',(-4.54195640846217E-14,1.66321791214601E-16,
-1.)) ;
#40504 = DIRECTION('ref_axis',(-1.,0.,4.54747350886464E-14)) ;
#40505 = DIRECTION('center_axis',(4.54195640846217E-14,-1.66321791214601E-16,
1.)) ;
#40506 = DIRECTION('ref_axis',(-1.,5.55236256206829E-46,4.54195640846217E-14)) ;
#40507 = DIRECTION('center_axis',(-2.1716102378779E-15,3.83815143260386E-28,
1.)) ;
#40508 = DIRECTION('ref_axis',(-0.707106781186643,0.707106781186452,-1.53556032529807E-15)) ;
#40509 = DIRECTION('center_axis',(-2.17161023787787E-15,3.83420712807771E-28,
1.)) ;
#40510 = DIRECTION('ref_axis',(0.707106781186543,-0.707106781186552,1.53556032529783E-15)) ;
#40511 = DIRECTION('',(-2.17161023787787E-15,3.83420712807771E-28,1.)) ;
#40512 = DIRECTION('center_axis',(2.17161023787792E-15,-2.90739654573749E-15,
-1.)) ;
#40513 = DIRECTION('ref_axis',(1.35627620245787E-13,-1.,2.90739654573778E-15)) ;
#40514 = DIRECTION('',(2.17161023787787E-15,-3.83420712807771E-28,-1.)) ;
#40515 = DIRECTION('center_axis',(1.,-8.32667268460789E-17,2.17161023787787E-15)) ;
#40516 = DIRECTION('ref_axis',(-8.32667268460789E-17,-1.,3.92101138914083E-28)) ;
#40517 = DIRECTION('',(2.17161023787787E-15,-3.83815143260382E-28,-1.)) ;
#40518 = DIRECTION('',(-8.32667268460789E-17,-1.,3.83780830390118E-28)) ;
#40519 = DIRECTION('center_axis',(2.17161023787787E-15,-3.83815143260382E-28,
-1.)) ;
#40520 = DIRECTION('ref_axis',(0.707106781186452,0.707106781186643,1.53556032529709E-15)) ;
#40521 = DIRECTION('',(-2.17161023787787E-15,3.83815143260382E-28,1.)) ;
#40522 = DIRECTION('center_axis',(2.17161023787746E-15,-7.39616701217516E-14,
-1.)) ;
#40523 = DIRECTION('ref_axis',(1.,-6.48092690624108E-15,2.17161023787794E-15)) ;
#40524 = DIRECTION('center_axis',(1.66533453692966E-16,1.,-3.83386399937507E-28)) ;
#40525 = DIRECTION('ref_axis',(2.1716102378779E-15,-3.83748045690496E-28,
-1.)) ;
#40526 = DIRECTION('',(2.1716102378779E-15,-3.83815143260386E-28,-1.)) ;
#40527 = DIRECTION('',(1.,-1.66533453692966E-16,2.1716102378779E-15)) ;
#40528 = DIRECTION('center_axis',(1.,-1.66533453692966E-16,-4.54195640846217E-14)) ;
#40529 = DIRECTION('ref_axis',(3.19987248283774E-14,-0.707106781186434,0.707106781186661)) ;
#40530 = DIRECTION('center_axis',(1.,0.,0.)) ;
#40531 = DIRECTION('ref_axis',(0.,0.,1.)) ;
#40532 = DIRECTION('',(1.,-1.66533453692966E-16,-4.54195640846217E-14)) ;
#40533 = DIRECTION('center_axis',(-1.,0.,0.)) ;
#40534 = DIRECTION('ref_axis',(0.,-1.,0.)) ;
#40535 = DIRECTION('',(1.,-1.66533453692966E-16,-4.54195640846217E-14)) ;
#40536 = DIRECTION('center_axis',(-4.54195640846217E-14,1.66321791214601E-16,
-1.)) ;
#40537 = DIRECTION('ref_axis',(-1.,0.,4.54747350886464E-14)) ;
#40538 = DIRECTION('center_axis',(0.,1.,0.)) ;
#40539 = DIRECTION('ref_axis',(-1.,0.,5.32907051820105E-14)) ;
#40540 = DIRECTION('center_axis',(4.54195640846217E-14,-1.66321791214601E-16,
1.)) ;
#40541 = DIRECTION('ref_axis',(-1.,5.55236256206829E-46,4.54195640846217E-14)) ;
#40542 = DIRECTION('center_axis',(2.17161023787787E-15,-3.83815143260382E-28,
-1.)) ;
#40543 = DIRECTION('ref_axis',(0.707106781186452,0.707106781186643,1.53556032529709E-15)) ;
#40544 = DIRECTION('center_axis',(-8.32667268460786E-17,-1.,-1.66321791214597E-16)) ;
#40545 = DIRECTION('ref_axis',(-0.707106781186535,-5.87287992268677E-17,0.70710678118656)) ;
#40546 = DIRECTION('center_axis',(0.,1.,0.)) ;
#40547 = DIRECTION('ref_axis',(-1.,0.,0.)) ;
#40548 = DIRECTION('',(-8.32667268460786E-17,-1.,-1.66321791214597E-16)) ;
#40549 = DIRECTION('',(-8.32667268460786E-17,-1.,-1.66321791214597E-16)) ;
#40550 = DIRECTION('center_axis',(-4.54195640846217E-14,1.66321791214601E-16,
-1.)) ;
#40551 = DIRECTION('ref_axis',(-1.,0.,4.54747350886464E-14)) ;
#40552 = DIRECTION('center_axis',(1.,2.84217094304056E-13,0.)) ;
#40553 = DIRECTION('ref_axis',(-2.84217094304056E-13,1.,0.)) ;
#40554 = DIRECTION('center_axis',(4.54195640846217E-14,-1.66321791214601E-16,
1.)) ;
#40555 = DIRECTION('ref_axis',(-1.,5.55236256206829E-46,4.54195640846217E-14)) ;
#40556 = DIRECTION('center_axis',(-2.17161023787787E-15,3.83420712807771E-28,
1.)) ;
#40557 = DIRECTION('ref_axis',(0.707106781186543,-0.707106781186552,1.53556032529783E-15)) ;
#40558 = DIRECTION('center_axis',(-1.,1.66533453692587E-16,4.54195640846217E-14)) ;
#40559 = DIRECTION('ref_axis',(3.22342386971791E-14,0.707106781186422,0.707106781186673)) ;
#40560 = DIRECTION('center_axis',(1.,0.,0.)) ;
#40561 = DIRECTION('ref_axis',(0.,1.,0.)) ;
#40562 = DIRECTION('',(-1.,1.66533453692587E-16,4.54195640846217E-14)) ;
#40563 = DIRECTION('',(-1.,1.66533453692587E-16,4.54195640846217E-14)) ;
#40564 = DIRECTION('center_axis',(-4.54195640846217E-14,1.66321791214601E-16,
-1.)) ;
#40565 = DIRECTION('ref_axis',(-1.,0.,4.54747350886464E-14)) ;
#40566 = DIRECTION('center_axis',(0.,-1.,0.)) ;
#40567 = DIRECTION('ref_axis',(1.,0.,-5.32907051820105E-14)) ;
#40568 = DIRECTION('center_axis',(4.54195640846217E-14,-1.66321791214601E-16,
1.)) ;
#40569 = DIRECTION('ref_axis',(-1.,5.55236256206829E-46,4.54195640846217E-14)) ;
#40570 = DIRECTION('center_axis',(2.1716102378779E-15,-3.83420712807775E-28,
-1.)) ;
#40571 = DIRECTION('ref_axis',(-0.707106781186452,-0.707106781186643,-1.53556032529712E-15)) ;
#40572 = DIRECTION('center_axis',(1.66533453692965E-16,1.,1.66321791214593E-16)) ;
#40573 = DIRECTION('ref_axis',(0.707106781186535,-2.35364200827643E-16,0.70710678118656)) ;
#40574 = DIRECTION('center_axis',(0.,-1.,0.)) ;
#40575 = DIRECTION('ref_axis',(1.,0.,0.)) ;
#40576 = DIRECTION('',(1.66533453692965E-16,1.,1.66321791214593E-16)) ;
#40577 = DIRECTION('',(1.66533453692965E-16,1.,1.66321791214593E-16)) ;
#40578 = DIRECTION('center_axis',(-4.54195640846217E-14,1.66321791214601E-16,
-1.)) ;
#40579 = DIRECTION('ref_axis',(-1.,0.,4.54747350886464E-14)) ;
#40580 = DIRECTION('center_axis',(4.54195640846217E-14,-1.66321791214601E-16,
1.)) ;
#40581 = DIRECTION('ref_axis',(-1.,5.55236256206829E-46,4.54195640846217E-14)) ;
#40582 = DIRECTION('center_axis',(-2.1716102378779E-15,3.83815143260386E-28,
1.)) ;
#40583 = DIRECTION('ref_axis',(-0.707106781186643,0.707106781186452,-1.53556032529807E-15)) ;
#40584 = DIRECTION('center_axis',(-2.17161023787787E-15,3.83420712807771E-28,
1.)) ;
#40585 = DIRECTION('ref_axis',(0.707106781186543,-0.707106781186552,1.53556032529783E-15)) ;
#40586 = DIRECTION('',(-2.17161023787787E-15,3.83420712807771E-28,1.)) ;
#40587 = DIRECTION('center_axis',(2.17161023787792E-15,-2.90739654573749E-15,
-1.)) ;
#40588 = DIRECTION('ref_axis',(1.35627620245787E-13,-1.,2.90739654573778E-15)) ;
#40589 = DIRECTION('',(2.17161023787787E-15,-3.83420712807771E-28,-1.)) ;
#40590 = DIRECTION('center_axis',(1.,-8.32667268460789E-17,2.17161023787787E-15)) ;
#40591 = DIRECTION('ref_axis',(-8.32667268460789E-17,-1.,3.92101138914083E-28)) ;
#40592 = DIRECTION('',(2.17161023787787E-15,-3.83815143260382E-28,-1.)) ;
#40593 = DIRECTION('',(-8.32667268460789E-17,-1.,3.83780830390118E-28)) ;
#40594 = DIRECTION('center_axis',(2.17161023787787E-15,-3.83815143260382E-28,
-1.)) ;
#40595 = DIRECTION('ref_axis',(0.707106781186452,0.707106781186643,1.53556032529709E-15)) ;
#40596 = DIRECTION('',(-2.17161023787787E-15,3.83815143260382E-28,1.)) ;
#40597 = DIRECTION('center_axis',(2.17161023787746E-15,-7.39616701217516E-14,
-1.)) ;
#40598 = DIRECTION('ref_axis',(1.,-6.48092690624108E-15,2.17161023787794E-15)) ;
#40599 = DIRECTION('center_axis',(1.66533453692966E-16,1.,-3.83386399937507E-28)) ;
#40600 = DIRECTION('ref_axis',(2.1716102378779E-15,-3.83748045690496E-28,
-1.)) ;
#40601 = DIRECTION('',(2.1716102378779E-15,-3.83815143260386E-28,-1.)) ;
#40602 = DIRECTION('',(1.,-1.66533453692966E-16,2.1716102378779E-15)) ;
#40603 = DIRECTION('center_axis',(1.,-1.66533453692966E-16,-4.54195640846217E-14)) ;
#40604 = DIRECTION('ref_axis',(3.19987248283774E-14,-0.707106781186434,0.707106781186661)) ;
#40605 = DIRECTION('center_axis',(1.,0.,0.)) ;
#40606 = DIRECTION('ref_axis',(0.,0.,1.)) ;
#40607 = DIRECTION('',(1.,-1.66533453692966E-16,-4.54195640846217E-14)) ;
#40608 = DIRECTION('center_axis',(-1.,0.,0.)) ;
#40609 = DIRECTION('ref_axis',(0.,-1.,0.)) ;
#40610 = DIRECTION('',(1.,-1.66533453692966E-16,-4.54195640846217E-14)) ;
#40611 = DIRECTION('center_axis',(-4.54195640846217E-14,1.66321791214601E-16,
-1.)) ;
#40612 = DIRECTION('ref_axis',(-1.,0.,4.54747350886464E-14)) ;
#40613 = DIRECTION('center_axis',(0.,1.,0.)) ;
#40614 = DIRECTION('ref_axis',(-1.,0.,5.32907051820105E-14)) ;
#40615 = DIRECTION('center_axis',(4.54195640846217E-14,-1.66321791214601E-16,
1.)) ;
#40616 = DIRECTION('ref_axis',(-1.,5.55236256206829E-46,4.54195640846217E-14)) ;
#40617 = DIRECTION('center_axis',(2.17161023787787E-15,-3.83815143260382E-28,
-1.)) ;
#40618 = DIRECTION('ref_axis',(0.707106781186452,0.707106781186643,1.53556032529709E-15)) ;
#40619 = DIRECTION('center_axis',(-8.32667268460786E-17,-1.,-1.66321791214597E-16)) ;
#40620 = DIRECTION('ref_axis',(-0.707106781186535,-5.87287992268677E-17,0.70710678118656)) ;
#40621 = DIRECTION('center_axis',(0.,1.,0.)) ;
#40622 = DIRECTION('ref_axis',(-1.,0.,0.)) ;
#40623 = DIRECTION('',(-8.32667268460786E-17,-1.,-1.66321791214597E-16)) ;
#40624 = DIRECTION('',(-8.32667268460786E-17,-1.,-1.66321791214597E-16)) ;
#40625 = DIRECTION('center_axis',(-4.54195640846217E-14,1.66321791214601E-16,
-1.)) ;
#40626 = DIRECTION('ref_axis',(-1.,0.,4.54747350886464E-14)) ;
#40627 = DIRECTION('center_axis',(1.,2.84217094304056E-13,0.)) ;
#40628 = DIRECTION('ref_axis',(-2.84217094304056E-13,1.,0.)) ;
#40629 = DIRECTION('center_axis',(4.54195640846217E-14,-1.66321791214601E-16,
1.)) ;
#40630 = DIRECTION('ref_axis',(-1.,5.55236256206829E-46,4.54195640846217E-14)) ;
#40631 = DIRECTION('center_axis',(-2.17161023787787E-15,3.83420712807771E-28,
1.)) ;
#40632 = DIRECTION('ref_axis',(0.707106781186543,-0.707106781186552,1.53556032529783E-15)) ;
#40633 = DIRECTION('center_axis',(-1.,1.66533453692587E-16,4.54195640846217E-14)) ;
#40634 = DIRECTION('ref_axis',(3.22342386971791E-14,0.707106781186422,0.707106781186673)) ;
#40635 = DIRECTION('center_axis',(1.,0.,0.)) ;
#40636 = DIRECTION('ref_axis',(0.,1.,0.)) ;
#40637 = DIRECTION('',(-1.,1.66533453692587E-16,4.54195640846217E-14)) ;
#40638 = DIRECTION('',(-1.,1.66533453692587E-16,4.54195640846217E-14)) ;
#40639 = DIRECTION('center_axis',(-4.54195640846217E-14,1.66321791214601E-16,
-1.)) ;
#40640 = DIRECTION('ref_axis',(-1.,0.,4.54747350886464E-14)) ;
#40641 = DIRECTION('center_axis',(0.,-1.,0.)) ;
#40642 = DIRECTION('ref_axis',(1.,0.,-5.32907051820105E-14)) ;
#40643 = DIRECTION('center_axis',(4.54195640846217E-14,-1.66321791214601E-16,
1.)) ;
#40644 = DIRECTION('ref_axis',(-1.,5.55236256206829E-46,4.54195640846217E-14)) ;
#40645 = DIRECTION('center_axis',(2.1716102378779E-15,-3.83420712807775E-28,
-1.)) ;
#40646 = DIRECTION('ref_axis',(-0.707106781186452,-0.707106781186643,-1.53556032529712E-15)) ;
#40647 = DIRECTION('center_axis',(1.66533453692965E-16,1.,1.66321791214593E-16)) ;
#40648 = DIRECTION('ref_axis',(0.707106781186535,-2.35364200827643E-16,0.70710678118656)) ;
#40649 = DIRECTION('center_axis',(0.,-1.,0.)) ;
#40650 = DIRECTION('ref_axis',(1.,0.,0.)) ;
#40651 = DIRECTION('',(1.66533453692965E-16,1.,1.66321791214593E-16)) ;
#40652 = DIRECTION('',(1.66533453692965E-16,1.,1.66321791214593E-16)) ;
#40653 = DIRECTION('center_axis',(-4.54195640846217E-14,1.66321791214601E-16,
-1.)) ;
#40654 = DIRECTION('ref_axis',(-1.,0.,4.54747350886464E-14)) ;
#40655 = DIRECTION('center_axis',(4.54195640846217E-14,-1.66321791214601E-16,
1.)) ;
#40656 = DIRECTION('ref_axis',(-1.,5.55236256206829E-46,4.54195640846217E-14)) ;
#40657 = DIRECTION('center_axis',(-2.1716102378779E-15,3.83815143260386E-28,
1.)) ;
#40658 = DIRECTION('ref_axis',(-0.707106781186643,0.707106781186452,-1.53556032529807E-15)) ;
#40659 = DIRECTION('center_axis',(-2.17161023787787E-15,3.83420712807771E-28,
1.)) ;
#40660 = DIRECTION('ref_axis',(0.707106781186543,-0.707106781186552,1.53556032529783E-15)) ;
#40661 = DIRECTION('',(-2.17161023787787E-15,3.83420712807771E-28,1.)) ;
#40662 = DIRECTION('center_axis',(2.17161023787792E-15,-2.90739654573749E-15,
-1.)) ;
#40663 = DIRECTION('ref_axis',(1.35627620245787E-13,-1.,2.90739654573778E-15)) ;
#40664 = DIRECTION('',(2.17161023787787E-15,-3.83420712807771E-28,-1.)) ;
#40665 = DIRECTION('center_axis',(1.,-8.32667268460789E-17,2.17161023787787E-15)) ;
#40666 = DIRECTION('ref_axis',(-8.32667268460789E-17,-1.,3.92101138914083E-28)) ;
#40667 = DIRECTION('',(2.17161023787787E-15,-3.83815143260382E-28,-1.)) ;
#40668 = DIRECTION('',(-8.32667268460789E-17,-1.,3.83780830390118E-28)) ;
#40669 = DIRECTION('center_axis',(2.17161023787787E-15,-3.83815143260382E-28,
-1.)) ;
#40670 = DIRECTION('ref_axis',(0.707106781186452,0.707106781186643,1.53556032529709E-15)) ;
#40671 = DIRECTION('',(-2.17161023787787E-15,3.83815143260382E-28,1.)) ;
#40672 = DIRECTION('center_axis',(2.17161023787746E-15,-7.39616701217516E-14,
-1.)) ;
#40673 = DIRECTION('ref_axis',(1.,-6.48092690624108E-15,2.17161023787794E-15)) ;
#40674 = DIRECTION('center_axis',(1.66533453692966E-16,1.,-3.83386399937507E-28)) ;
#40675 = DIRECTION('ref_axis',(2.1716102378779E-15,-3.83748045690496E-28,
-1.)) ;
#40676 = DIRECTION('',(2.1716102378779E-15,-3.83815143260386E-28,-1.)) ;
#40677 = DIRECTION('',(1.,-1.66533453692966E-16,2.1716102378779E-15)) ;
#40678 = DIRECTION('center_axis',(1.,-1.66533453692966E-16,-4.54195640846217E-14)) ;
#40679 = DIRECTION('ref_axis',(3.19987248283774E-14,-0.707106781186434,0.707106781186661)) ;
#40680 = DIRECTION('center_axis',(1.,0.,0.)) ;
#40681 = DIRECTION('ref_axis',(0.,0.,1.)) ;
#40682 = DIRECTION('',(1.,-1.66533453692966E-16,-4.54195640846217E-14)) ;
#40683 = DIRECTION('center_axis',(-1.,0.,0.)) ;
#40684 = DIRECTION('ref_axis',(0.,-1.,0.)) ;
#40685 = DIRECTION('',(1.,-1.66533453692966E-16,-4.54195640846217E-14)) ;
#40686 = DIRECTION('center_axis',(-4.54195640846217E-14,1.66321791214601E-16,
-1.)) ;
#40687 = DIRECTION('ref_axis',(-1.,0.,4.54747350886464E-14)) ;
#40688 = DIRECTION('center_axis',(0.,1.,0.)) ;
#40689 = DIRECTION('ref_axis',(-1.,0.,5.32907051820105E-14)) ;
#40690 = DIRECTION('center_axis',(4.54195640846217E-14,-1.66321791214601E-16,
1.)) ;
#40691 = DIRECTION('ref_axis',(-1.,5.55236256206829E-46,4.54195640846217E-14)) ;
#40692 = DIRECTION('center_axis',(2.17161023787787E-15,-3.83815143260382E-28,
-1.)) ;
#40693 = DIRECTION('ref_axis',(0.707106781186452,0.707106781186643,1.53556032529709E-15)) ;
#40694 = DIRECTION('center_axis',(-8.32667268460786E-17,-1.,-1.66321791214597E-16)) ;
#40695 = DIRECTION('ref_axis',(-0.707106781186535,-5.87287992268677E-17,0.70710678118656)) ;
#40696 = DIRECTION('center_axis',(0.,1.,0.)) ;
#40697 = DIRECTION('ref_axis',(-1.,0.,0.)) ;
#40698 = DIRECTION('',(-8.32667268460786E-17,-1.,-1.66321791214597E-16)) ;
#40699 = DIRECTION('',(-8.32667268460786E-17,-1.,-1.66321791214597E-16)) ;
#40700 = DIRECTION('center_axis',(-4.54195640846217E-14,1.66321791214601E-16,
-1.)) ;
#40701 = DIRECTION('ref_axis',(-1.,0.,4.54747350886464E-14)) ;
#40702 = DIRECTION('center_axis',(1.,2.84217094304056E-13,0.)) ;
#40703 = DIRECTION('ref_axis',(-2.84217094304056E-13,1.,0.)) ;
#40704 = DIRECTION('center_axis',(4.54195640846217E-14,-1.66321791214601E-16,
1.)) ;
#40705 = DIRECTION('ref_axis',(-1.,5.55236256206829E-46,4.54195640846217E-14)) ;
#40706 = DIRECTION('center_axis',(-2.17161023787787E-15,3.83420712807771E-28,
1.)) ;
#40707 = DIRECTION('ref_axis',(0.707106781186543,-0.707106781186552,1.53556032529783E-15)) ;
#40708 = DIRECTION('center_axis',(-1.,1.66533453692587E-16,4.54195640846217E-14)) ;
#40709 = DIRECTION('ref_axis',(3.22342386971791E-14,0.707106781186422,0.707106781186673)) ;
#40710 = DIRECTION('center_axis',(1.,0.,0.)) ;
#40711 = DIRECTION('ref_axis',(0.,1.,0.)) ;
#40712 = DIRECTION('',(-1.,1.66533453692587E-16,4.54195640846217E-14)) ;
#40713 = DIRECTION('',(-1.,1.66533453692587E-16,4.54195640846217E-14)) ;
#40714 = DIRECTION('center_axis',(-4.54195640846217E-14,1.66321791214601E-16,
-1.)) ;
#40715 = DIRECTION('ref_axis',(-1.,0.,4.54747350886464E-14)) ;
#40716 = DIRECTION('center_axis',(0.,-1.,0.)) ;
#40717 = DIRECTION('ref_axis',(1.,0.,-5.32907051820105E-14)) ;
#40718 = DIRECTION('center_axis',(4.54195640846217E-14,-1.66321791214601E-16,
1.)) ;
#40719 = DIRECTION('ref_axis',(-1.,5.55236256206829E-46,4.54195640846217E-14)) ;
#40720 = DIRECTION('center_axis',(2.1716102378779E-15,-3.83420712807775E-28,
-1.)) ;
#40721 = DIRECTION('ref_axis',(-0.707106781186452,-0.707106781186643,-1.53556032529712E-15)) ;
#40722 = DIRECTION('center_axis',(1.66533453692965E-16,1.,1.66321791214593E-16)) ;
#40723 = DIRECTION('ref_axis',(0.707106781186535,-2.35364200827643E-16,0.70710678118656)) ;
#40724 = DIRECTION('center_axis',(0.,-1.,0.)) ;
#40725 = DIRECTION('ref_axis',(1.,0.,0.)) ;
#40726 = DIRECTION('',(1.66533453692965E-16,1.,1.66321791214593E-16)) ;
#40727 = DIRECTION('',(1.66533453692965E-16,1.,1.66321791214593E-16)) ;
#40728 = DIRECTION('center_axis',(-4.54195640846217E-14,1.66321791214601E-16,
-1.)) ;
#40729 = DIRECTION('ref_axis',(-1.,0.,4.54747350886464E-14)) ;
#40730 = DIRECTION('center_axis',(4.54195640846217E-14,-1.66321791214601E-16,
1.)) ;
#40731 = DIRECTION('ref_axis',(-1.,5.55236256206829E-46,4.54195640846217E-14)) ;
#40732 = DIRECTION('center_axis',(-2.1716102378779E-15,3.83815143260386E-28,
1.)) ;
#40733 = DIRECTION('ref_axis',(-0.707106781186643,0.707106781186452,-1.53556032529807E-15)) ;
#40734 = DIRECTION('center_axis',(-2.17161023787787E-15,3.83420712807771E-28,
1.)) ;
#40735 = DIRECTION('ref_axis',(0.707106781186543,-0.707106781186552,1.53556032529783E-15)) ;
#40736 = DIRECTION('',(-2.17161023787787E-15,3.83420712807771E-28,1.)) ;
#40737 = DIRECTION('center_axis',(2.17161023787792E-15,-2.90739654573749E-15,
-1.)) ;
#40738 = DIRECTION('ref_axis',(1.35627620245787E-13,-1.,2.90739654573778E-15)) ;
#40739 = DIRECTION('',(2.17161023787787E-15,-3.83420712807771E-28,-1.)) ;
#40740 = DIRECTION('center_axis',(1.,-8.32667268460789E-17,2.17161023787787E-15)) ;
#40741 = DIRECTION('ref_axis',(-8.32667268460789E-17,-1.,3.92101138914083E-28)) ;
#40742 = DIRECTION('',(2.17161023787787E-15,-3.83815143260382E-28,-1.)) ;
#40743 = DIRECTION('',(-8.32667268460789E-17,-1.,3.83780830390118E-28)) ;
#40744 = DIRECTION('center_axis',(2.17161023787787E-15,-3.83815143260382E-28,
-1.)) ;
#40745 = DIRECTION('ref_axis',(0.707106781186452,0.707106781186643,1.53556032529709E-15)) ;
#40746 = DIRECTION('',(-2.17161023787787E-15,3.83815143260382E-28,1.)) ;
#40747 = DIRECTION('center_axis',(2.17161023787746E-15,-7.39616701217516E-14,
-1.)) ;
#40748 = DIRECTION('ref_axis',(1.,-6.48092690624108E-15,2.17161023787794E-15)) ;
#40749 = DIRECTION('center_axis',(1.66533453692966E-16,1.,-3.83386399937507E-28)) ;
#40750 = DIRECTION('ref_axis',(2.1716102378779E-15,-3.83748045690496E-28,
-1.)) ;
#40751 = DIRECTION('',(2.1716102378779E-15,-3.83815143260386E-28,-1.)) ;
#40752 = DIRECTION('',(1.,-1.66533453692966E-16,2.1716102378779E-15)) ;
#40753 = DIRECTION('center_axis',(1.,-1.66533453692966E-16,-4.54195640846217E-14)) ;
#40754 = DIRECTION('ref_axis',(3.19987248283774E-14,-0.707106781186434,0.707106781186661)) ;
#40755 = DIRECTION('center_axis',(1.,0.,0.)) ;
#40756 = DIRECTION('ref_axis',(0.,0.,1.)) ;
#40757 = DIRECTION('',(1.,-1.66533453692966E-16,-4.54195640846217E-14)) ;
#40758 = DIRECTION('center_axis',(-1.,0.,0.)) ;
#40759 = DIRECTION('ref_axis',(0.,-1.,0.)) ;
#40760 = DIRECTION('',(1.,-1.66533453692966E-16,-4.54195640846217E-14)) ;
#40761 = DIRECTION('center_axis',(-4.54195640846217E-14,1.66321791214601E-16,
-1.)) ;
#40762 = DIRECTION('ref_axis',(-1.,0.,4.54747350886464E-14)) ;
#40763 = DIRECTION('center_axis',(0.,1.,0.)) ;
#40764 = DIRECTION('ref_axis',(-1.,0.,5.32907051820105E-14)) ;
#40765 = DIRECTION('center_axis',(4.54195640846217E-14,-1.66321791214601E-16,
1.)) ;
#40766 = DIRECTION('ref_axis',(-1.,5.55236256206829E-46,4.54195640846217E-14)) ;
#40767 = DIRECTION('center_axis',(2.17161023787787E-15,-3.83815143260382E-28,
-1.)) ;
#40768 = DIRECTION('ref_axis',(0.707106781186452,0.707106781186643,1.53556032529709E-15)) ;
#40769 = DIRECTION('center_axis',(-8.32667268460786E-17,-1.,-1.66321791214597E-16)) ;
#40770 = DIRECTION('ref_axis',(-0.707106781186535,-5.87287992268677E-17,0.70710678118656)) ;
#40771 = DIRECTION('center_axis',(0.,1.,0.)) ;
#40772 = DIRECTION('ref_axis',(-1.,0.,0.)) ;
#40773 = DIRECTION('',(-8.32667268460786E-17,-1.,-1.66321791214597E-16)) ;
#40774 = DIRECTION('',(-8.32667268460786E-17,-1.,-1.66321791214597E-16)) ;
#40775 = DIRECTION('center_axis',(-4.54195640846217E-14,1.66321791214601E-16,
-1.)) ;
#40776 = DIRECTION('ref_axis',(-1.,0.,4.54747350886464E-14)) ;
#40777 = DIRECTION('center_axis',(1.,2.84217094304056E-13,0.)) ;
#40778 = DIRECTION('ref_axis',(-2.84217094304056E-13,1.,0.)) ;
#40779 = DIRECTION('center_axis',(4.54195640846217E-14,-1.66321791214601E-16,
1.)) ;
#40780 = DIRECTION('ref_axis',(-1.,5.55236256206829E-46,4.54195640846217E-14)) ;
#40781 = DIRECTION('center_axis',(-2.17161023787787E-15,3.83420712807771E-28,
1.)) ;
#40782 = DIRECTION('ref_axis',(0.707106781186543,-0.707106781186552,1.53556032529783E-15)) ;
#40783 = DIRECTION('center_axis',(-1.,1.66533453692587E-16,4.54195640846217E-14)) ;
#40784 = DIRECTION('ref_axis',(3.22342386971791E-14,0.707106781186422,0.707106781186673)) ;
#40785 = DIRECTION('center_axis',(1.,0.,0.)) ;
#40786 = DIRECTION('ref_axis',(0.,1.,0.)) ;
#40787 = DIRECTION('',(-1.,1.66533453692587E-16,4.54195640846217E-14)) ;
#40788 = DIRECTION('',(-1.,1.66533453692587E-16,4.54195640846217E-14)) ;
#40789 = DIRECTION('center_axis',(-4.54195640846217E-14,1.66321791214601E-16,
-1.)) ;
#40790 = DIRECTION('ref_axis',(-1.,0.,4.54747350886464E-14)) ;
#40791 = DIRECTION('center_axis',(0.,-1.,0.)) ;
#40792 = DIRECTION('ref_axis',(1.,0.,-5.32907051820105E-14)) ;
#40793 = DIRECTION('center_axis',(4.54195640846217E-14,-1.66321791214601E-16,
1.)) ;
#40794 = DIRECTION('ref_axis',(-1.,5.55236256206829E-46,4.54195640846217E-14)) ;
#40795 = DIRECTION('center_axis',(2.1716102378779E-15,-3.83420712807775E-28,
-1.)) ;
#40796 = DIRECTION('ref_axis',(-0.707106781186452,-0.707106781186643,-1.53556032529712E-15)) ;
#40797 = DIRECTION('center_axis',(1.66533453692965E-16,1.,1.66321791214593E-16)) ;
#40798 = DIRECTION('ref_axis',(0.707106781186535,-2.35364200827643E-16,0.70710678118656)) ;
#40799 = DIRECTION('center_axis',(0.,-1.,0.)) ;
#40800 = DIRECTION('ref_axis',(1.,0.,0.)) ;
#40801 = DIRECTION('',(1.66533453692965E-16,1.,1.66321791214593E-16)) ;
#40802 = DIRECTION('',(1.66533453692965E-16,1.,1.66321791214593E-16)) ;
#40803 = DIRECTION('center_axis',(-4.54195640846217E-14,1.66321791214601E-16,
-1.)) ;
#40804 = DIRECTION('ref_axis',(-1.,0.,4.54747350886464E-14)) ;
#40805 = DIRECTION('center_axis',(4.54195640846217E-14,-1.66321791214601E-16,
1.)) ;
#40806 = DIRECTION('ref_axis',(-1.,5.55236256206829E-46,4.54195640846217E-14)) ;
#40807 = DIRECTION('center_axis',(-2.1716102378779E-15,3.83815143260386E-28,
1.)) ;
#40808 = DIRECTION('ref_axis',(-0.707106781186643,0.707106781186452,-1.53556032529807E-15)) ;
#40809 = DIRECTION('center_axis',(-2.17161023787787E-15,3.83420712807771E-28,
1.)) ;
#40810 = DIRECTION('ref_axis',(0.707106781186543,-0.707106781186552,1.53556032529783E-15)) ;
#40811 = DIRECTION('',(-2.17161023787787E-15,3.83420712807771E-28,1.)) ;
#40812 = DIRECTION('center_axis',(2.17161023787792E-15,-2.90739654573749E-15,
-1.)) ;
#40813 = DIRECTION('ref_axis',(1.35627620245787E-13,-1.,2.90739654573778E-15)) ;
#40814 = DIRECTION('',(2.17161023787787E-15,-3.83420712807771E-28,-1.)) ;
#40815 = DIRECTION('center_axis',(1.,-8.32667268460789E-17,2.17161023787787E-15)) ;
#40816 = DIRECTION('ref_axis',(-8.32667268460789E-17,-1.,3.92101138914083E-28)) ;
#40817 = DIRECTION('',(2.17161023787787E-15,-3.83815143260382E-28,-1.)) ;
#40818 = DIRECTION('',(-8.32667268460789E-17,-1.,3.83780830390118E-28)) ;
#40819 = DIRECTION('center_axis',(2.17161023787787E-15,-3.83815143260382E-28,
-1.)) ;
#40820 = DIRECTION('ref_axis',(0.707106781186452,0.707106781186643,1.53556032529709E-15)) ;
#40821 = DIRECTION('',(-2.17161023787787E-15,3.83815143260382E-28,1.)) ;
#40822 = DIRECTION('center_axis',(2.17161023787746E-15,-7.39616701217516E-14,
-1.)) ;
#40823 = DIRECTION('ref_axis',(1.,-6.48092690624108E-15,2.17161023787794E-15)) ;
#40824 = DIRECTION('center_axis',(1.66533453692966E-16,1.,-3.83386399937507E-28)) ;
#40825 = DIRECTION('ref_axis',(2.1716102378779E-15,-3.83748045690496E-28,
-1.)) ;
#40826 = DIRECTION('',(2.1716102378779E-15,-3.83815143260386E-28,-1.)) ;
#40827 = DIRECTION('',(1.,-1.66533453692966E-16,2.1716102378779E-15)) ;
#40828 = DIRECTION('center_axis',(1.,-1.66533453692966E-16,-4.54195640846217E-14)) ;
#40829 = DIRECTION('ref_axis',(3.19987248283774E-14,-0.707106781186434,0.707106781186661)) ;
#40830 = DIRECTION('center_axis',(1.,0.,0.)) ;
#40831 = DIRECTION('ref_axis',(0.,0.,1.)) ;
#40832 = DIRECTION('',(1.,-1.66533453692966E-16,-4.54195640846217E-14)) ;
#40833 = DIRECTION('center_axis',(-1.,0.,0.)) ;
#40834 = DIRECTION('ref_axis',(0.,-1.,0.)) ;
#40835 = DIRECTION('',(1.,-1.66533453692966E-16,-4.54195640846217E-14)) ;
#40836 = DIRECTION('center_axis',(-4.54195640846217E-14,1.66321791214601E-16,
-1.)) ;
#40837 = DIRECTION('ref_axis',(-1.,0.,4.54747350886464E-14)) ;
#40838 = DIRECTION('center_axis',(0.,1.,0.)) ;
#40839 = DIRECTION('ref_axis',(-1.,0.,5.32907051820105E-14)) ;
#40840 = DIRECTION('center_axis',(4.54195640846217E-14,-1.66321791214601E-16,
1.)) ;
#40841 = DIRECTION('ref_axis',(-1.,5.55236256206829E-46,4.54195640846217E-14)) ;
#40842 = DIRECTION('center_axis',(2.17161023787787E-15,-3.83815143260382E-28,
-1.)) ;
#40843 = DIRECTION('ref_axis',(0.707106781186452,0.707106781186643,1.53556032529709E-15)) ;
#40844 = DIRECTION('center_axis',(-8.32667268460786E-17,-1.,-1.66321791214597E-16)) ;
#40845 = DIRECTION('ref_axis',(-0.707106781186535,-5.87287992268677E-17,0.70710678118656)) ;
#40846 = DIRECTION('center_axis',(0.,1.,0.)) ;
#40847 = DIRECTION('ref_axis',(-1.,0.,0.)) ;
#40848 = DIRECTION('',(-8.32667268460786E-17,-1.,-1.66321791214597E-16)) ;
#40849 = DIRECTION('',(-8.32667268460786E-17,-1.,-1.66321791214597E-16)) ;
#40850 = DIRECTION('center_axis',(-4.54195640846217E-14,1.66321791214601E-16,
-1.)) ;
#40851 = DIRECTION('ref_axis',(-1.,0.,4.54747350886464E-14)) ;
#40852 = DIRECTION('center_axis',(1.,2.84217094304056E-13,0.)) ;
#40853 = DIRECTION('ref_axis',(-2.84217094304056E-13,1.,0.)) ;
#40854 = DIRECTION('center_axis',(4.54195640846217E-14,-1.66321791214601E-16,
1.)) ;
#40855 = DIRECTION('ref_axis',(-1.,5.55236256206829E-46,4.54195640846217E-14)) ;
#40856 = DIRECTION('center_axis',(-2.17161023787787E-15,3.83420712807771E-28,
1.)) ;
#40857 = DIRECTION('ref_axis',(0.707106781186543,-0.707106781186552,1.53556032529783E-15)) ;
#40858 = DIRECTION('center_axis',(-1.,1.66533453692587E-16,4.54195640846217E-14)) ;
#40859 = DIRECTION('ref_axis',(3.22342386971791E-14,0.707106781186422,0.707106781186673)) ;
#40860 = DIRECTION('center_axis',(1.,0.,0.)) ;
#40861 = DIRECTION('ref_axis',(0.,1.,0.)) ;
#40862 = DIRECTION('',(-1.,1.66533453692587E-16,4.54195640846217E-14)) ;
#40863 = DIRECTION('',(-1.,1.66533453692587E-16,4.54195640846217E-14)) ;
#40864 = DIRECTION('center_axis',(-4.54195640846217E-14,1.66321791214601E-16,
-1.)) ;
#40865 = DIRECTION('ref_axis',(-1.,0.,4.54747350886464E-14)) ;
#40866 = DIRECTION('center_axis',(0.,-1.,0.)) ;
#40867 = DIRECTION('ref_axis',(1.,0.,-5.32907051820105E-14)) ;
#40868 = DIRECTION('center_axis',(4.54195640846217E-14,-1.66321791214601E-16,
1.)) ;
#40869 = DIRECTION('ref_axis',(-1.,5.55236256206829E-46,4.54195640846217E-14)) ;
#40870 = DIRECTION('center_axis',(2.1716102378779E-15,-3.83420712807775E-28,
-1.)) ;
#40871 = DIRECTION('ref_axis',(-0.707106781186452,-0.707106781186643,-1.53556032529712E-15)) ;
#40872 = DIRECTION('center_axis',(1.66533453692965E-16,1.,1.66321791214593E-16)) ;
#40873 = DIRECTION('ref_axis',(0.707106781186535,-2.35364200827643E-16,0.70710678118656)) ;
#40874 = DIRECTION('center_axis',(0.,-1.,0.)) ;
#40875 = DIRECTION('ref_axis',(1.,0.,0.)) ;
#40876 = DIRECTION('',(1.66533453692965E-16,1.,1.66321791214593E-16)) ;
#40877 = DIRECTION('',(1.66533453692965E-16,1.,1.66321791214593E-16)) ;
#40878 = DIRECTION('center_axis',(-4.54195640846217E-14,1.66321791214601E-16,
-1.)) ;
#40879 = DIRECTION('ref_axis',(-1.,0.,4.54747350886464E-14)) ;
#40880 = DIRECTION('center_axis',(4.54195640846217E-14,-1.66321791214601E-16,
1.)) ;
#40881 = DIRECTION('ref_axis',(-1.,5.55236256206829E-46,4.54195640846217E-14)) ;
#40882 = DIRECTION('center_axis',(-2.1716102378779E-15,3.83815143260386E-28,
1.)) ;
#40883 = DIRECTION('ref_axis',(-0.707106781186643,0.707106781186452,-1.53556032529807E-15)) ;
#40884 = DIRECTION('center_axis',(-2.17161023787787E-15,3.83420712807771E-28,
1.)) ;
#40885 = DIRECTION('ref_axis',(0.707106781186543,-0.707106781186552,1.53556032529783E-15)) ;
#40886 = DIRECTION('',(-2.17161023787787E-15,3.83420712807771E-28,1.)) ;
#40887 = DIRECTION('center_axis',(2.17161023787792E-15,-2.90739654573749E-15,
-1.)) ;
#40888 = DIRECTION('ref_axis',(1.35627620245787E-13,-1.,2.90739654573778E-15)) ;
#40889 = DIRECTION('',(2.17161023787787E-15,-3.83420712807771E-28,-1.)) ;
#40890 = DIRECTION('center_axis',(1.,-8.32667268460789E-17,2.17161023787787E-15)) ;
#40891 = DIRECTION('ref_axis',(-8.32667268460789E-17,-1.,3.92101138914083E-28)) ;
#40892 = DIRECTION('',(2.17161023787787E-15,-3.83815143260382E-28,-1.)) ;
#40893 = DIRECTION('',(-8.32667268460789E-17,-1.,3.83780830390118E-28)) ;
#40894 = DIRECTION('center_axis',(2.17161023787787E-15,-3.83815143260382E-28,
-1.)) ;
#40895 = DIRECTION('ref_axis',(0.707106781186452,0.707106781186643,1.53556032529709E-15)) ;
#40896 = DIRECTION('',(-2.17161023787787E-15,3.83815143260382E-28,1.)) ;
#40897 = DIRECTION('center_axis',(2.17161023787746E-15,-7.39616701217516E-14,
-1.)) ;
#40898 = DIRECTION('ref_axis',(1.,-6.48092690624108E-15,2.17161023787794E-15)) ;
#40899 = DIRECTION('center_axis',(1.66533453692966E-16,1.,-3.83386399937507E-28)) ;
#40900 = DIRECTION('ref_axis',(2.1716102378779E-15,-3.83748045690496E-28,
-1.)) ;
#40901 = DIRECTION('',(2.1716102378779E-15,-3.83815143260386E-28,-1.)) ;
#40902 = DIRECTION('',(1.,-1.66533453692966E-16,2.1716102378779E-15)) ;
#40903 = DIRECTION('center_axis',(1.,-1.66533453692966E-16,-4.54195640846217E-14)) ;
#40904 = DIRECTION('ref_axis',(3.19987248283774E-14,-0.707106781186434,0.707106781186661)) ;
#40905 = DIRECTION('center_axis',(1.,0.,0.)) ;
#40906 = DIRECTION('ref_axis',(0.,0.,1.)) ;
#40907 = DIRECTION('',(1.,-1.66533453692966E-16,-4.54195640846217E-14)) ;
#40908 = DIRECTION('center_axis',(-1.,0.,0.)) ;
#40909 = DIRECTION('ref_axis',(0.,-1.,0.)) ;
#40910 = DIRECTION('',(1.,-1.66533453692966E-16,-4.54195640846217E-14)) ;
#40911 = DIRECTION('center_axis',(-4.54195640846217E-14,1.66321791214601E-16,
-1.)) ;
#40912 = DIRECTION('ref_axis',(-1.,0.,4.54747350886464E-14)) ;
#40913 = DIRECTION('center_axis',(0.,1.,0.)) ;
#40914 = DIRECTION('ref_axis',(-1.,0.,5.32907051820105E-14)) ;
#40915 = DIRECTION('center_axis',(4.54195640846217E-14,-1.66321791214601E-16,
1.)) ;
#40916 = DIRECTION('ref_axis',(-1.,5.55236256206829E-46,4.54195640846217E-14)) ;
#40917 = DIRECTION('center_axis',(2.17161023787787E-15,-3.83815143260382E-28,
-1.)) ;
#40918 = DIRECTION('ref_axis',(0.707106781186452,0.707106781186643,1.53556032529709E-15)) ;
#40919 = DIRECTION('center_axis',(-8.32667268460786E-17,-1.,-1.66321791214597E-16)) ;
#40920 = DIRECTION('ref_axis',(-0.707106781186535,-5.87287992268677E-17,0.70710678118656)) ;
#40921 = DIRECTION('center_axis',(0.,1.,0.)) ;
#40922 = DIRECTION('ref_axis',(-1.,0.,0.)) ;
#40923 = DIRECTION('',(-8.32667268460786E-17,-1.,-1.66321791214597E-16)) ;
#40924 = DIRECTION('',(-8.32667268460786E-17,-1.,-1.66321791214597E-16)) ;
#40925 = DIRECTION('center_axis',(-4.54195640846217E-14,1.66321791214601E-16,
-1.)) ;
#40926 = DIRECTION('ref_axis',(-1.,0.,4.54747350886464E-14)) ;
#40927 = DIRECTION('center_axis',(1.,2.84217094304056E-13,0.)) ;
#40928 = DIRECTION('ref_axis',(-2.84217094304056E-13,1.,0.)) ;
#40929 = DIRECTION('center_axis',(4.54195640846217E-14,-1.66321791214601E-16,
1.)) ;
#40930 = DIRECTION('ref_axis',(-1.,5.55236256206829E-46,4.54195640846217E-14)) ;
#40931 = DIRECTION('center_axis',(-2.17161023787787E-15,3.83420712807771E-28,
1.)) ;
#40932 = DIRECTION('ref_axis',(0.707106781186543,-0.707106781186552,1.53556032529783E-15)) ;
#40933 = DIRECTION('center_axis',(-1.,1.66533453692587E-16,4.54195640846217E-14)) ;
#40934 = DIRECTION('ref_axis',(3.22342386971791E-14,0.707106781186422,0.707106781186673)) ;
#40935 = DIRECTION('center_axis',(1.,0.,0.)) ;
#40936 = DIRECTION('ref_axis',(0.,1.,0.)) ;
#40937 = DIRECTION('',(-1.,1.66533453692587E-16,4.54195640846217E-14)) ;
#40938 = DIRECTION('',(-1.,1.66533453692587E-16,4.54195640846217E-14)) ;
#40939 = DIRECTION('center_axis',(-4.54195640846217E-14,1.66321791214601E-16,
-1.)) ;
#40940 = DIRECTION('ref_axis',(-1.,0.,4.54747350886464E-14)) ;
#40941 = DIRECTION('center_axis',(0.,-1.,0.)) ;
#40942 = DIRECTION('ref_axis',(1.,0.,-5.32907051820105E-14)) ;
#40943 = DIRECTION('center_axis',(4.54195640846217E-14,-1.66321791214601E-16,
1.)) ;
#40944 = DIRECTION('ref_axis',(-1.,5.55236256206829E-46,4.54195640846217E-14)) ;
#40945 = DIRECTION('center_axis',(2.1716102378779E-15,-3.83420712807775E-28,
-1.)) ;
#40946 = DIRECTION('ref_axis',(-0.707106781186452,-0.707106781186643,-1.53556032529712E-15)) ;
#40947 = DIRECTION('center_axis',(1.66533453692965E-16,1.,1.66321791214593E-16)) ;
#40948 = DIRECTION('ref_axis',(0.707106781186535,-2.35364200827643E-16,0.70710678118656)) ;
#40949 = DIRECTION('center_axis',(0.,-1.,0.)) ;
#40950 = DIRECTION('ref_axis',(1.,0.,0.)) ;
#40951 = DIRECTION('',(1.66533453692965E-16,1.,1.66321791214593E-16)) ;
#40952 = DIRECTION('',(1.66533453692965E-16,1.,1.66321791214593E-16)) ;
#40953 = DIRECTION('center_axis',(-4.54195640846217E-14,1.66321791214601E-16,
-1.)) ;
#40954 = DIRECTION('ref_axis',(-1.,0.,4.54747350886464E-14)) ;
#40955 = DIRECTION('center_axis',(4.54195640846217E-14,-1.66321791214601E-16,
1.)) ;
#40956 = DIRECTION('ref_axis',(-1.,5.55236256206829E-46,4.54195640846217E-14)) ;
#40957 = DIRECTION('center_axis',(-2.1716102378779E-15,3.83815143260386E-28,
1.)) ;
#40958 = DIRECTION('ref_axis',(-0.707106781186643,0.707106781186452,-1.53556032529807E-15)) ;
#40959 = DIRECTION('center_axis',(-2.17161023787787E-15,3.83420712807771E-28,
1.)) ;
#40960 = DIRECTION('ref_axis',(0.707106781186543,-0.707106781186552,1.53556032529783E-15)) ;
#40961 = DIRECTION('',(-2.17161023787787E-15,3.83420712807771E-28,1.)) ;
#40962 = DIRECTION('center_axis',(2.17161023787792E-15,-2.90739654573749E-15,
-1.)) ;
#40963 = DIRECTION('ref_axis',(1.35627620245787E-13,-1.,2.90739654573778E-15)) ;
#40964 = DIRECTION('',(2.17161023787787E-15,-3.83420712807771E-28,-1.)) ;
#40965 = DIRECTION('center_axis',(1.,-8.32667268460789E-17,2.17161023787787E-15)) ;
#40966 = DIRECTION('ref_axis',(-8.32667268460789E-17,-1.,3.92101138914083E-28)) ;
#40967 = DIRECTION('',(2.17161023787787E-15,-3.83815143260382E-28,-1.)) ;
#40968 = DIRECTION('',(-8.32667268460789E-17,-1.,3.83780830390118E-28)) ;
#40969 = DIRECTION('center_axis',(2.17161023787787E-15,-3.83815143260382E-28,
-1.)) ;
#40970 = DIRECTION('ref_axis',(0.707106781186452,0.707106781186643,1.53556032529709E-15)) ;
#40971 = DIRECTION('',(-2.17161023787787E-15,3.83815143260382E-28,1.)) ;
#40972 = DIRECTION('center_axis',(2.17161023787746E-15,-7.39616701217516E-14,
-1.)) ;
#40973 = DIRECTION('ref_axis',(1.,-6.48092690624108E-15,2.17161023787794E-15)) ;
#40974 = DIRECTION('center_axis',(1.66533453692966E-16,1.,-3.83386399937507E-28)) ;
#40975 = DIRECTION('ref_axis',(2.1716102378779E-15,-3.83748045690496E-28,
-1.)) ;
#40976 = DIRECTION('',(2.1716102378779E-15,-3.83815143260386E-28,-1.)) ;
#40977 = DIRECTION('',(1.,-1.66533453692966E-16,2.1716102378779E-15)) ;
#40978 = DIRECTION('center_axis',(1.,-1.66533453692966E-16,-4.54195640846217E-14)) ;
#40979 = DIRECTION('ref_axis',(3.19987248283774E-14,-0.707106781186434,0.707106781186661)) ;
#40980 = DIRECTION('center_axis',(1.,0.,0.)) ;
#40981 = DIRECTION('ref_axis',(0.,0.,1.)) ;
#40982 = DIRECTION('',(1.,-1.66533453692966E-16,-4.54195640846217E-14)) ;
#40983 = DIRECTION('center_axis',(-1.,0.,0.)) ;
#40984 = DIRECTION('ref_axis',(0.,-1.,0.)) ;
#40985 = DIRECTION('',(1.,-1.66533453692966E-16,-4.54195640846217E-14)) ;
#40986 = DIRECTION('center_axis',(-4.54195640846217E-14,1.66321791214601E-16,
-1.)) ;
#40987 = DIRECTION('ref_axis',(-1.,0.,4.54747350886464E-14)) ;
#40988 = DIRECTION('center_axis',(0.,1.,0.)) ;
#40989 = DIRECTION('ref_axis',(-1.,0.,5.32907051820105E-14)) ;
#40990 = DIRECTION('center_axis',(4.54195640846217E-14,-1.66321791214601E-16,
1.)) ;
#40991 = DIRECTION('ref_axis',(-1.,5.55236256206829E-46,4.54195640846217E-14)) ;
#40992 = DIRECTION('center_axis',(2.1716102378779E-15,-3.83815143260386E-28,
-1.)) ;
#40993 = DIRECTION('ref_axis',(0.707106781186552,0.707106781186543,1.53556032529733E-15)) ;
#40994 = DIRECTION('center_axis',(-1.66533453692965E-16,-1.,-1.66321791214593E-16)) ;
#40995 = DIRECTION('ref_axis',(-0.707106781186535,1.4966797377543E-19,0.70710678118656)) ;
#40996 = DIRECTION('center_axis',(0.,1.,0.)) ;
#40997 = DIRECTION('ref_axis',(-1.,0.,0.)) ;
#40998 = DIRECTION('',(-1.66533453692965E-16,-1.,-1.66321791214593E-16)) ;
#40999 = DIRECTION('',(-1.66533453692965E-16,-1.,-1.66321791214593E-16)) ;
#41000 = DIRECTION('center_axis',(-4.54195640846217E-14,1.66321791214601E-16,
-1.)) ;
#41001 = DIRECTION('ref_axis',(-1.,0.,4.54747350886464E-14)) ;
#41002 = DIRECTION('center_axis',(1.,2.84217094304056E-13,0.)) ;
#41003 = DIRECTION('ref_axis',(-2.84217094304056E-13,1.,0.)) ;
#41004 = DIRECTION('center_axis',(4.54195640846217E-14,-1.66321791214601E-16,
1.)) ;
#41005 = DIRECTION('ref_axis',(-1.,5.55236256206829E-46,4.54195640846217E-14)) ;
#41006 = DIRECTION('center_axis',(-2.1716102378779E-15,3.83420712807775E-28,
1.)) ;
#41007 = DIRECTION('ref_axis',(0.707106781186643,-0.707106781186452,1.53556032529807E-15)) ;
#41008 = DIRECTION('center_axis',(-1.,1.66533453692587E-16,4.54195640846217E-14)) ;
#41009 = DIRECTION('ref_axis',(3.22342386971791E-14,0.707106781186422,0.707106781186673)) ;
#41010 = DIRECTION('center_axis',(1.,0.,0.)) ;
#41011 = DIRECTION('ref_axis',(0.,1.,0.)) ;
#41012 = DIRECTION('',(-1.,1.66533453692587E-16,4.54195640846217E-14)) ;
#41013 = DIRECTION('',(-1.,1.66533453692587E-16,4.54195640846217E-14)) ;
#41014 = DIRECTION('center_axis',(-4.54195640846217E-14,1.66321791214601E-16,
-1.)) ;
#41015 = DIRECTION('ref_axis',(-1.,0.,4.54747350886464E-14)) ;
#41016 = DIRECTION('center_axis',(0.,-1.,0.)) ;
#41017 = DIRECTION('ref_axis',(1.,0.,-5.32907051820105E-14)) ;
#41018 = DIRECTION('center_axis',(4.54195640846217E-14,-1.66321791214601E-16,
1.)) ;
#41019 = DIRECTION('ref_axis',(-1.,5.55236256206829E-46,4.54195640846217E-14)) ;
#41020 = DIRECTION('center_axis',(2.17161023787787E-15,-3.83420712807771E-28,
-1.)) ;
#41021 = DIRECTION('ref_axis',(-0.707106781186552,-0.707106781186543,-1.53556032529731E-15)) ;
#41022 = DIRECTION('center_axis',(8.32667268460786E-17,1.,1.66321791214597E-16)) ;
#41023 = DIRECTION('ref_axis',(0.707106781186522,-1.76485733627007E-16,0.707106781186573)) ;
#41024 = DIRECTION('center_axis',(0.,-1.,0.)) ;
#41025 = DIRECTION('ref_axis',(1.,0.,1.77635683940035E-14)) ;
#41026 = DIRECTION('',(8.32667268460786E-17,1.,1.66321791214597E-16)) ;
#41027 = DIRECTION('center_axis',(-4.54195640846217E-14,1.66321791214601E-16,
-1.)) ;
#41028 = DIRECTION('ref_axis',(-1.,0.,4.54747350886464E-14)) ;
#41029 = DIRECTION('center_axis',(4.54195640846217E-14,-1.66321791214601E-16,
1.)) ;
#41030 = DIRECTION('ref_axis',(-1.,5.55236256206829E-46,4.54195640846217E-14)) ;
#41031 = DIRECTION('center_axis',(-2.17161023787787E-15,3.83815143260382E-28,
1.)) ;
#41032 = DIRECTION('ref_axis',(-0.707106781186643,0.707106781186452,-1.53556032529805E-15)) ;
#41033 = DIRECTION('center_axis',(-2.1716102378779E-15,3.83420712807775E-28,
1.)) ;
#41034 = DIRECTION('ref_axis',(0.707106781186643,-0.707106781186452,1.53556032529807E-15)) ;
#41035 = DIRECTION('',(-2.1716102378779E-15,3.83420712807775E-28,1.)) ;
#41036 = DIRECTION('center_axis',(2.1716102378779E-15,-3.83420712807775E-28,
-1.)) ;
#41037 = DIRECTION('ref_axis',(0.707106781186656,-0.707106781186439,1.5355603252981E-15)) ;
#41038 = DIRECTION('',(-2.1716102378779E-15,3.83322105194623E-28,1.)) ;
#41039 = DIRECTION('center_axis',(1.,-1.66533453692966E-16,2.1716102378779E-15)) ;
#41040 = DIRECTION('ref_axis',(-1.66533453692966E-16,-1.,3.82783884128008E-28)) ;
#41041 = DIRECTION('',(-2.1716102378779E-15,3.66854633798134E-28,1.)) ;
#41042 = DIRECTION('center_axis',(1.,-1.66533453692966E-16,2.1716102378779E-15)) ;
#41043 = DIRECTION('ref_axis',(-1.41780339089703E-15,0.707106781186483,0.707106781186612)) ;
#41044 = DIRECTION('',(-1.66533453692966E-16,-1.,3.83386399937507E-28)) ;
#41045 = DIRECTION('',(2.1716102378779E-15,-3.83815143260386E-28,-1.)) ;
#41046 = DIRECTION('',(-1.66533453692966E-16,-1.,3.83386399937507E-28)) ;
#41047 = DIRECTION('center_axis',(1.,-1.66533453692966E-16,2.1716102378779E-15)) ;
#41048 = DIRECTION('ref_axis',(-1.65331725969844E-15,-0.707106781186479,0.707106781186616)) ;
#41049 = DIRECTION('',(2.1716102378779E-15,-3.66854633798134E-28,-1.)) ;
#41050 = DIRECTION('center_axis',(2.1716102378779E-15,-3.83815143260386E-28,
-1.)) ;
#41051 = DIRECTION('ref_axis',(0.707106781186552,0.707106781186543,1.53556032529733E-15)) ;
#41052 = DIRECTION('',(-2.1716102378779E-15,3.83815143260386E-28,1.)) ;
#41053 = DIRECTION('center_axis',(2.1716102378779E-15,-3.83815143260386E-28,
-1.)) ;
#41054 = DIRECTION('ref_axis',(0.707106781186582,0.707106781186513,1.5355603252974E-15)) ;
#41055 = DIRECTION('center_axis',(1.66533453692966E-16,1.,-3.83386399937507E-28)) ;
#41056 = DIRECTION('ref_axis',(2.1716102378779E-15,-3.83748045690496E-28,
-1.)) ;
#41057 = DIRECTION('',(2.17161023787787E-15,-3.83815143260382E-28,-1.)) ;
#41058 = DIRECTION('',(1.,-1.66533453692966E-16,2.1716102378779E-15)) ;
#41059 = DIRECTION('center_axis',(1.,-1.66533453692966E-16,-4.54195640846217E-14)) ;
#41060 = DIRECTION('ref_axis',(3.19987248283774E-14,-0.707106781186434,0.707106781186661)) ;
#41061 = DIRECTION('center_axis',(1.,0.,0.)) ;
#41062 = DIRECTION('ref_axis',(0.,0.,1.)) ;
#41063 = DIRECTION('',(1.,-1.66533453692966E-16,-4.54195640846217E-14)) ;
#41064 = DIRECTION('center_axis',(-1.,0.,0.)) ;
#41065 = DIRECTION('ref_axis',(0.,-1.,0.)) ;
#41066 = DIRECTION('',(1.,-1.66533453692966E-16,-4.54195640846217E-14)) ;
#41067 = DIRECTION('center_axis',(-4.54195640846217E-14,1.66321791214601E-16,
-1.)) ;
#41068 = DIRECTION('ref_axis',(-1.,0.,4.54747350886464E-14)) ;
#41069 = DIRECTION('center_axis',(0.,1.,0.)) ;
#41070 = DIRECTION('ref_axis',(-1.,0.,5.32907051820105E-14)) ;
#41071 = DIRECTION('center_axis',(4.54195640846217E-14,-1.66321791214601E-16,
1.)) ;
#41072 = DIRECTION('ref_axis',(-1.,5.55236256206829E-46,4.54195640846217E-14)) ;
#41073 = DIRECTION('center_axis',(2.1716102378779E-15,-3.83815143260386E-28,
-1.)) ;
#41074 = DIRECTION('ref_axis',(0.707106781186552,0.707106781186543,1.53556032529733E-15)) ;
#41075 = DIRECTION('center_axis',(-1.66533453692965E-16,-1.,-1.66321791214593E-16)) ;
#41076 = DIRECTION('ref_axis',(-0.707106781186535,1.4966797377543E-19,0.70710678118656)) ;
#41077 = DIRECTION('center_axis',(0.,1.,0.)) ;
#41078 = DIRECTION('ref_axis',(-1.,0.,0.)) ;
#41079 = DIRECTION('',(-1.66533453692965E-16,-1.,-1.66321791214593E-16)) ;
#41080 = DIRECTION('',(-1.66533453692965E-16,-1.,-1.66321791214593E-16)) ;
#41081 = DIRECTION('center_axis',(-4.54195640846217E-14,1.66321791214601E-16,
-1.)) ;
#41082 = DIRECTION('ref_axis',(-1.,0.,4.54747350886464E-14)) ;
#41083 = DIRECTION('center_axis',(1.,2.84217094304056E-13,0.)) ;
#41084 = DIRECTION('ref_axis',(-2.84217094304056E-13,1.,0.)) ;
#41085 = DIRECTION('center_axis',(4.54195640846217E-14,-1.66321791214601E-16,
1.)) ;
#41086 = DIRECTION('ref_axis',(-1.,5.55236256206829E-46,4.54195640846217E-14)) ;
#41087 = DIRECTION('center_axis',(-2.1716102378779E-15,3.83420712807775E-28,
1.)) ;
#41088 = DIRECTION('ref_axis',(0.707106781186643,-0.707106781186452,1.53556032529807E-15)) ;
#41089 = DIRECTION('center_axis',(-1.,1.66533453692587E-16,4.54195640846217E-14)) ;
#41090 = DIRECTION('ref_axis',(3.22342386971791E-14,0.707106781186422,0.707106781186673)) ;
#41091 = DIRECTION('center_axis',(1.,0.,0.)) ;
#41092 = DIRECTION('ref_axis',(0.,1.,0.)) ;
#41093 = DIRECTION('',(-1.,1.66533453692587E-16,4.54195640846217E-14)) ;
#41094 = DIRECTION('',(-1.,1.66533453692587E-16,4.54195640846217E-14)) ;
#41095 = DIRECTION('center_axis',(-4.54195640846217E-14,1.66321791214601E-16,
-1.)) ;
#41096 = DIRECTION('ref_axis',(-1.,0.,4.54747350886464E-14)) ;
#41097 = DIRECTION('center_axis',(0.,-1.,0.)) ;
#41098 = DIRECTION('ref_axis',(1.,0.,-5.32907051820105E-14)) ;
#41099 = DIRECTION('center_axis',(4.54195640846217E-14,-1.66321791214601E-16,
1.)) ;
#41100 = DIRECTION('ref_axis',(-1.,5.55236256206829E-46,4.54195640846217E-14)) ;
#41101 = DIRECTION('center_axis',(2.17161023787787E-15,-3.83420712807771E-28,
-1.)) ;
#41102 = DIRECTION('ref_axis',(-0.707106781186552,-0.707106781186543,-1.53556032529731E-15)) ;
#41103 = DIRECTION('center_axis',(8.32667268460786E-17,1.,1.66321791214597E-16)) ;
#41104 = DIRECTION('ref_axis',(0.707106781186522,-1.76485733627007E-16,0.707106781186573)) ;
#41105 = DIRECTION('center_axis',(0.,-1.,0.)) ;
#41106 = DIRECTION('ref_axis',(1.,0.,1.77635683940035E-14)) ;
#41107 = DIRECTION('',(8.32667268460786E-17,1.,1.66321791214597E-16)) ;
#41108 = DIRECTION('center_axis',(-4.54195640846217E-14,1.66321791214601E-16,
-1.)) ;
#41109 = DIRECTION('ref_axis',(-1.,0.,4.54747350886464E-14)) ;
#41110 = DIRECTION('center_axis',(4.54195640846217E-14,-1.66321791214601E-16,
1.)) ;
#41111 = DIRECTION('ref_axis',(-1.,5.55236256206829E-46,4.54195640846217E-14)) ;
#41112 = DIRECTION('center_axis',(-2.17161023787787E-15,3.83815143260382E-28,
1.)) ;
#41113 = DIRECTION('ref_axis',(-0.707106781186643,0.707106781186452,-1.53556032529805E-15)) ;
#41114 = DIRECTION('center_axis',(-2.1716102378779E-15,3.83420712807775E-28,
1.)) ;
#41115 = DIRECTION('ref_axis',(0.707106781186643,-0.707106781186452,1.53556032529807E-15)) ;
#41116 = DIRECTION('',(-2.1716102378779E-15,3.83420712807775E-28,1.)) ;
#41117 = DIRECTION('center_axis',(2.1716102378779E-15,-3.83420712807775E-28,
-1.)) ;
#41118 = DIRECTION('ref_axis',(0.707106781186656,-0.707106781186439,1.5355603252981E-15)) ;
#41119 = DIRECTION('',(-2.1716102378779E-15,3.83322105194623E-28,1.)) ;
#41120 = DIRECTION('center_axis',(1.,-1.66533453692966E-16,2.1716102378779E-15)) ;
#41121 = DIRECTION('ref_axis',(-1.66533453692966E-16,-1.,3.82783884128008E-28)) ;
#41122 = DIRECTION('',(-2.1716102378779E-15,3.66854633798134E-28,1.)) ;
#41123 = DIRECTION('center_axis',(1.,-1.66533453692966E-16,2.1716102378779E-15)) ;
#41124 = DIRECTION('ref_axis',(-1.41780339089703E-15,0.707106781186483,0.707106781186612)) ;
#41125 = DIRECTION('',(-1.66533453692966E-16,-1.,3.83386399937507E-28)) ;
#41126 = DIRECTION('',(2.1716102378779E-15,-3.83815143260386E-28,-1.)) ;
#41127 = DIRECTION('',(-1.66533453692966E-16,-1.,3.83386399937507E-28)) ;
#41128 = DIRECTION('center_axis',(1.,-1.66533453692966E-16,2.1716102378779E-15)) ;
#41129 = DIRECTION('ref_axis',(-1.65331725969844E-15,-0.707106781186479,0.707106781186616)) ;
#41130 = DIRECTION('',(2.1716102378779E-15,-3.66854633798134E-28,-1.)) ;
#41131 = DIRECTION('center_axis',(2.1716102378779E-15,-3.83815143260386E-28,
-1.)) ;
#41132 = DIRECTION('ref_axis',(0.707106781186552,0.707106781186543,1.53556032529733E-15)) ;
#41133 = DIRECTION('',(-2.1716102378779E-15,3.83815143260386E-28,1.)) ;
#41134 = DIRECTION('center_axis',(2.1716102378779E-15,-3.83815143260386E-28,
-1.)) ;
#41135 = DIRECTION('ref_axis',(0.707106781186582,0.707106781186513,1.5355603252974E-15)) ;
#41136 = DIRECTION('center_axis',(1.66533453692966E-16,1.,-3.83386399937507E-28)) ;
#41137 = DIRECTION('ref_axis',(2.1716102378779E-15,-3.83748045690496E-28,
-1.)) ;
#41138 = DIRECTION('',(2.17161023787787E-15,-3.83815143260382E-28,-1.)) ;
#41139 = DIRECTION('',(1.,-1.66533453692966E-16,2.1716102378779E-15)) ;
#41140 = DIRECTION('center_axis',(1.,-1.66533453692966E-16,-4.54195640846217E-14)) ;
#41141 = DIRECTION('ref_axis',(3.19987248283774E-14,-0.707106781186434,0.707106781186661)) ;
#41142 = DIRECTION('center_axis',(1.,0.,0.)) ;
#41143 = DIRECTION('ref_axis',(0.,0.,1.)) ;
#41144 = DIRECTION('',(1.,-1.66533453692966E-16,-4.54195640846217E-14)) ;
#41145 = DIRECTION('center_axis',(-1.,0.,0.)) ;
#41146 = DIRECTION('ref_axis',(0.,-1.,0.)) ;
#41147 = DIRECTION('',(1.,-1.66533453692966E-16,-4.54195640846217E-14)) ;
#41148 = DIRECTION('center_axis',(-4.54195640846217E-14,1.66321791214601E-16,
-1.)) ;
#41149 = DIRECTION('ref_axis',(-1.,0.,4.54747350886464E-14)) ;
#41150 = DIRECTION('center_axis',(0.,1.,0.)) ;
#41151 = DIRECTION('ref_axis',(-1.,0.,5.32907051820105E-14)) ;
#41152 = DIRECTION('center_axis',(4.54195640846217E-14,-1.66321791214601E-16,
1.)) ;
#41153 = DIRECTION('ref_axis',(-1.,5.55236256206829E-46,4.54195640846217E-14)) ;
#41154 = DIRECTION('center_axis',(2.1716102378779E-15,-3.83815143260386E-28,
-1.)) ;
#41155 = DIRECTION('ref_axis',(0.707106781186552,0.707106781186543,1.53556032529733E-15)) ;
#41156 = DIRECTION('center_axis',(-1.66533453692965E-16,-1.,-1.66321791214593E-16)) ;
#41157 = DIRECTION('ref_axis',(-0.707106781186535,1.4966797377543E-19,0.70710678118656)) ;
#41158 = DIRECTION('center_axis',(0.,1.,0.)) ;
#41159 = DIRECTION('ref_axis',(-1.,0.,0.)) ;
#41160 = DIRECTION('',(-1.66533453692965E-16,-1.,-1.66321791214593E-16)) ;
#41161 = DIRECTION('',(-1.66533453692965E-16,-1.,-1.66321791214593E-16)) ;
#41162 = DIRECTION('center_axis',(-4.54195640846217E-14,1.66321791214601E-16,
-1.)) ;
#41163 = DIRECTION('ref_axis',(-1.,0.,4.54747350886464E-14)) ;
#41164 = DIRECTION('center_axis',(1.,2.84217094304056E-13,0.)) ;
#41165 = DIRECTION('ref_axis',(-2.84217094304056E-13,1.,0.)) ;
#41166 = DIRECTION('center_axis',(4.54195640846217E-14,-1.66321791214601E-16,
1.)) ;
#41167 = DIRECTION('ref_axis',(-1.,5.55236256206829E-46,4.54195640846217E-14)) ;
#41168 = DIRECTION('center_axis',(-2.1716102378779E-15,3.83420712807775E-28,
1.)) ;
#41169 = DIRECTION('ref_axis',(0.707106781186643,-0.707106781186452,1.53556032529807E-15)) ;
#41170 = DIRECTION('center_axis',(-1.,1.66533453692587E-16,4.54195640846217E-14)) ;
#41171 = DIRECTION('ref_axis',(3.22342386971791E-14,0.707106781186422,0.707106781186673)) ;
#41172 = DIRECTION('center_axis',(1.,0.,0.)) ;
#41173 = DIRECTION('ref_axis',(0.,1.,0.)) ;
#41174 = DIRECTION('',(-1.,1.66533453692587E-16,4.54195640846217E-14)) ;
#41175 = DIRECTION('',(-1.,1.66533453692587E-16,4.54195640846217E-14)) ;
#41176 = DIRECTION('center_axis',(-4.54195640846217E-14,1.66321791214601E-16,
-1.)) ;
#41177 = DIRECTION('ref_axis',(-1.,0.,4.54747350886464E-14)) ;
#41178 = DIRECTION('center_axis',(0.,-1.,0.)) ;
#41179 = DIRECTION('ref_axis',(1.,0.,-5.32907051820105E-14)) ;
#41180 = DIRECTION('center_axis',(4.54195640846217E-14,-1.66321791214601E-16,
1.)) ;
#41181 = DIRECTION('ref_axis',(-1.,5.55236256206829E-46,4.54195640846217E-14)) ;
#41182 = DIRECTION('center_axis',(2.17161023787787E-15,-3.83420712807771E-28,
-1.)) ;
#41183 = DIRECTION('ref_axis',(-0.707106781186552,-0.707106781186543,-1.53556032529731E-15)) ;
#41184 = DIRECTION('center_axis',(8.32667268460786E-17,1.,1.66321791214597E-16)) ;
#41185 = DIRECTION('ref_axis',(0.707106781186522,-1.76485733627007E-16,0.707106781186573)) ;
#41186 = DIRECTION('center_axis',(0.,-1.,0.)) ;
#41187 = DIRECTION('ref_axis',(1.,0.,1.77635683940035E-14)) ;
#41188 = DIRECTION('',(8.32667268460786E-17,1.,1.66321791214597E-16)) ;
#41189 = DIRECTION('center_axis',(-4.54195640846217E-14,1.66321791214601E-16,
-1.)) ;
#41190 = DIRECTION('ref_axis',(-1.,0.,4.54747350886464E-14)) ;
#41191 = DIRECTION('center_axis',(4.54195640846217E-14,-1.66321791214601E-16,
1.)) ;
#41192 = DIRECTION('ref_axis',(-1.,5.55236256206829E-46,4.54195640846217E-14)) ;
#41193 = DIRECTION('center_axis',(-2.17161023787787E-15,3.83815143260382E-28,
1.)) ;
#41194 = DIRECTION('ref_axis',(-0.707106781186643,0.707106781186452,-1.53556032529805E-15)) ;
#41195 = DIRECTION('center_axis',(-2.1716102378779E-15,3.83420712807775E-28,
1.)) ;
#41196 = DIRECTION('ref_axis',(0.707106781186643,-0.707106781186452,1.53556032529807E-15)) ;
#41197 = DIRECTION('',(-2.1716102378779E-15,3.83420712807775E-28,1.)) ;
#41198 = DIRECTION('center_axis',(2.1716102378779E-15,-3.83420712807775E-28,
-1.)) ;
#41199 = DIRECTION('ref_axis',(0.707106781186656,-0.707106781186439,1.5355603252981E-15)) ;
#41200 = DIRECTION('',(-2.1716102378779E-15,3.83322105194623E-28,1.)) ;
#41201 = DIRECTION('center_axis',(1.,-1.66533453692966E-16,2.1716102378779E-15)) ;
#41202 = DIRECTION('ref_axis',(-1.66533453692966E-16,-1.,3.82783884128008E-28)) ;
#41203 = DIRECTION('',(-2.1716102378779E-15,3.66854633798134E-28,1.)) ;
#41204 = DIRECTION('center_axis',(1.,-1.66533453692966E-16,2.1716102378779E-15)) ;
#41205 = DIRECTION('ref_axis',(-1.41780339089703E-15,0.707106781186483,0.707106781186612)) ;
#41206 = DIRECTION('',(-1.66533453692966E-16,-1.,3.83386399937507E-28)) ;
#41207 = DIRECTION('',(2.1716102378779E-15,-3.83815143260386E-28,-1.)) ;
#41208 = DIRECTION('',(-1.66533453692966E-16,-1.,3.83386399937507E-28)) ;
#41209 = DIRECTION('center_axis',(1.,-1.66533453692966E-16,2.1716102378779E-15)) ;
#41210 = DIRECTION('ref_axis',(-1.65331725969844E-15,-0.707106781186479,0.707106781186616)) ;
#41211 = DIRECTION('',(2.1716102378779E-15,-3.66854633798134E-28,-1.)) ;
#41212 = DIRECTION('center_axis',(2.1716102378779E-15,-3.83815143260386E-28,
-1.)) ;
#41213 = DIRECTION('ref_axis',(0.707106781186552,0.707106781186543,1.53556032529733E-15)) ;
#41214 = DIRECTION('',(-2.1716102378779E-15,3.83815143260386E-28,1.)) ;
#41215 = DIRECTION('center_axis',(2.1716102378779E-15,-3.83815143260386E-28,
-1.)) ;
#41216 = DIRECTION('ref_axis',(0.707106781186582,0.707106781186513,1.5355603252974E-15)) ;
#41217 = DIRECTION('center_axis',(1.66533453692966E-16,1.,-3.83386399937507E-28)) ;
#41218 = DIRECTION('ref_axis',(2.1716102378779E-15,-3.83748045690496E-28,
-1.)) ;
#41219 = DIRECTION('',(2.17161023787787E-15,-3.83815143260382E-28,-1.)) ;
#41220 = DIRECTION('',(1.,-1.66533453692966E-16,2.1716102378779E-15)) ;
#41221 = DIRECTION('center_axis',(1.,-1.66533453692966E-16,-4.54195640846217E-14)) ;
#41222 = DIRECTION('ref_axis',(3.19987248283774E-14,-0.707106781186434,0.707106781186661)) ;
#41223 = DIRECTION('center_axis',(1.,0.,0.)) ;
#41224 = DIRECTION('ref_axis',(0.,0.,1.)) ;
#41225 = DIRECTION('',(1.,-1.66533453692966E-16,-4.54195640846217E-14)) ;
#41226 = DIRECTION('center_axis',(-1.,0.,0.)) ;
#41227 = DIRECTION('ref_axis',(0.,-1.,0.)) ;
#41228 = DIRECTION('',(1.,-1.66533453692966E-16,-4.54195640846217E-14)) ;
#41229 = DIRECTION('center_axis',(-4.54195640846217E-14,1.66321791214601E-16,
-1.)) ;
#41230 = DIRECTION('ref_axis',(-1.,0.,4.54747350886464E-14)) ;
#41231 = DIRECTION('center_axis',(0.,1.,0.)) ;
#41232 = DIRECTION('ref_axis',(-1.,0.,5.32907051820105E-14)) ;
#41233 = DIRECTION('center_axis',(4.54195640846217E-14,-1.66321791214601E-16,
1.)) ;
#41234 = DIRECTION('ref_axis',(-1.,5.55236256206829E-46,4.54195640846217E-14)) ;
#41235 = DIRECTION('center_axis',(2.1716102378779E-15,-3.83815143260386E-28,
-1.)) ;
#41236 = DIRECTION('ref_axis',(0.707106781186552,0.707106781186543,1.53556032529733E-15)) ;
#41237 = DIRECTION('center_axis',(-1.66533453692965E-16,-1.,-1.66321791214593E-16)) ;
#41238 = DIRECTION('ref_axis',(-0.707106781186535,1.4966797377543E-19,0.70710678118656)) ;
#41239 = DIRECTION('center_axis',(0.,1.,0.)) ;
#41240 = DIRECTION('ref_axis',(-1.,0.,0.)) ;
#41241 = DIRECTION('',(-1.66533453692965E-16,-1.,-1.66321791214593E-16)) ;
#41242 = DIRECTION('',(-1.66533453692965E-16,-1.,-1.66321791214593E-16)) ;
#41243 = DIRECTION('center_axis',(-4.54195640846217E-14,1.66321791214601E-16,
-1.)) ;
#41244 = DIRECTION('ref_axis',(-1.,0.,4.54747350886464E-14)) ;
#41245 = DIRECTION('center_axis',(1.,2.84217094304056E-13,0.)) ;
#41246 = DIRECTION('ref_axis',(-2.84217094304056E-13,1.,0.)) ;
#41247 = DIRECTION('center_axis',(4.54195640846217E-14,-1.66321791214601E-16,
1.)) ;
#41248 = DIRECTION('ref_axis',(-1.,5.55236256206829E-46,4.54195640846217E-14)) ;
#41249 = DIRECTION('center_axis',(-2.1716102378779E-15,3.83420712807775E-28,
1.)) ;
#41250 = DIRECTION('ref_axis',(0.707106781186643,-0.707106781186452,1.53556032529807E-15)) ;
#41251 = DIRECTION('center_axis',(-1.,1.66533453692587E-16,4.54195640846217E-14)) ;
#41252 = DIRECTION('ref_axis',(3.22342386971791E-14,0.707106781186422,0.707106781186673)) ;
#41253 = DIRECTION('center_axis',(1.,0.,0.)) ;
#41254 = DIRECTION('ref_axis',(0.,1.,0.)) ;
#41255 = DIRECTION('',(-1.,1.66533453692587E-16,4.54195640846217E-14)) ;
#41256 = DIRECTION('',(-1.,1.66533453692587E-16,4.54195640846217E-14)) ;
#41257 = DIRECTION('center_axis',(-4.54195640846217E-14,1.66321791214601E-16,
-1.)) ;
#41258 = DIRECTION('ref_axis',(-1.,0.,4.54747350886464E-14)) ;
#41259 = DIRECTION('center_axis',(0.,-1.,0.)) ;
#41260 = DIRECTION('ref_axis',(1.,0.,-5.32907051820105E-14)) ;
#41261 = DIRECTION('center_axis',(4.54195640846217E-14,-1.66321791214601E-16,
1.)) ;
#41262 = DIRECTION('ref_axis',(-1.,5.55236256206829E-46,4.54195640846217E-14)) ;
#41263 = DIRECTION('center_axis',(2.17161023787787E-15,-3.83420712807771E-28,
-1.)) ;
#41264 = DIRECTION('ref_axis',(-0.707106781186552,-0.707106781186543,-1.53556032529731E-15)) ;
#41265 = DIRECTION('center_axis',(8.32667268460786E-17,1.,1.66321791214597E-16)) ;
#41266 = DIRECTION('ref_axis',(0.707106781186522,-1.76485733627007E-16,0.707106781186573)) ;
#41267 = DIRECTION('center_axis',(0.,-1.,0.)) ;
#41268 = DIRECTION('ref_axis',(1.,0.,1.77635683940035E-14)) ;
#41269 = DIRECTION('',(8.32667268460786E-17,1.,1.66321791214597E-16)) ;
#41270 = DIRECTION('center_axis',(-4.54195640846217E-14,1.66321791214601E-16,
-1.)) ;
#41271 = DIRECTION('ref_axis',(-1.,0.,4.54747350886464E-14)) ;
#41272 = DIRECTION('center_axis',(4.54195640846217E-14,-1.66321791214601E-16,
1.)) ;
#41273 = DIRECTION('ref_axis',(-1.,5.55236256206829E-46,4.54195640846217E-14)) ;
#41274 = DIRECTION('center_axis',(-2.17161023787787E-15,3.83815143260382E-28,
1.)) ;
#41275 = DIRECTION('ref_axis',(-0.707106781186643,0.707106781186452,-1.53556032529805E-15)) ;
#41276 = DIRECTION('center_axis',(-2.1716102378779E-15,3.83420712807775E-28,
1.)) ;
#41277 = DIRECTION('ref_axis',(0.707106781186643,-0.707106781186452,1.53556032529807E-15)) ;
#41278 = DIRECTION('',(-2.1716102378779E-15,3.83420712807775E-28,1.)) ;
#41279 = DIRECTION('center_axis',(2.1716102378779E-15,-3.83420712807775E-28,
-1.)) ;
#41280 = DIRECTION('ref_axis',(0.707106781186656,-0.707106781186439,1.5355603252981E-15)) ;
#41281 = DIRECTION('',(-2.1716102378779E-15,3.83322105194623E-28,1.)) ;
#41282 = DIRECTION('center_axis',(1.,-1.66533453692966E-16,2.1716102378779E-15)) ;
#41283 = DIRECTION('ref_axis',(-1.66533453692966E-16,-1.,3.82783884128008E-28)) ;
#41284 = DIRECTION('',(-2.1716102378779E-15,3.66854633798134E-28,1.)) ;
#41285 = DIRECTION('center_axis',(1.,-1.66533453692966E-16,2.1716102378779E-15)) ;
#41286 = DIRECTION('ref_axis',(-1.41780339089703E-15,0.707106781186483,0.707106781186612)) ;
#41287 = DIRECTION('',(-1.66533453692966E-16,-1.,3.83386399937507E-28)) ;
#41288 = DIRECTION('',(2.1716102378779E-15,-3.83815143260386E-28,-1.)) ;
#41289 = DIRECTION('',(-1.66533453692966E-16,-1.,3.83386399937507E-28)) ;
#41290 = DIRECTION('center_axis',(1.,-1.66533453692966E-16,2.1716102378779E-15)) ;
#41291 = DIRECTION('ref_axis',(-1.65331725969844E-15,-0.707106781186479,0.707106781186616)) ;
#41292 = DIRECTION('',(2.1716102378779E-15,-3.66854633798134E-28,-1.)) ;
#41293 = DIRECTION('center_axis',(2.1716102378779E-15,-3.83815143260386E-28,
-1.)) ;
#41294 = DIRECTION('ref_axis',(0.707106781186552,0.707106781186543,1.53556032529733E-15)) ;
#41295 = DIRECTION('',(-2.1716102378779E-15,3.83815143260386E-28,1.)) ;
#41296 = DIRECTION('center_axis',(2.1716102378779E-15,-3.83815143260386E-28,
-1.)) ;
#41297 = DIRECTION('ref_axis',(0.707106781186582,0.707106781186513,1.5355603252974E-15)) ;
#41298 = DIRECTION('center_axis',(1.66533453692966E-16,1.,-3.83386399937507E-28)) ;
#41299 = DIRECTION('ref_axis',(2.1716102378779E-15,-3.83748045690496E-28,
-1.)) ;
#41300 = DIRECTION('',(2.17161023787787E-15,-3.83815143260382E-28,-1.)) ;
#41301 = DIRECTION('',(1.,-1.66533453692966E-16,2.1716102378779E-15)) ;
#41302 = DIRECTION('center_axis',(1.,-1.66533453692966E-16,-4.54195640846217E-14)) ;
#41303 = DIRECTION('ref_axis',(3.19987248283774E-14,-0.707106781186434,0.707106781186661)) ;
#41304 = DIRECTION('center_axis',(1.,0.,0.)) ;
#41305 = DIRECTION('ref_axis',(0.,0.,1.)) ;
#41306 = DIRECTION('',(1.,-1.66533453692966E-16,-4.54195640846217E-14)) ;
#41307 = DIRECTION('center_axis',(-1.,0.,0.)) ;
#41308 = DIRECTION('ref_axis',(0.,-1.,0.)) ;
#41309 = DIRECTION('',(1.,-1.66533453692966E-16,-4.54195640846217E-14)) ;
#41310 = DIRECTION('center_axis',(-4.54195640846217E-14,1.66321791214601E-16,
-1.)) ;
#41311 = DIRECTION('ref_axis',(-1.,0.,4.54747350886464E-14)) ;
#41312 = DIRECTION('center_axis',(0.,1.,0.)) ;
#41313 = DIRECTION('ref_axis',(-1.,0.,5.32907051820105E-14)) ;
#41314 = DIRECTION('center_axis',(4.54195640846217E-14,-1.66321791214601E-16,
1.)) ;
#41315 = DIRECTION('ref_axis',(-1.,5.55236256206829E-46,4.54195640846217E-14)) ;
#41316 = DIRECTION('center_axis',(2.1716102378779E-15,-3.83815143260386E-28,
-1.)) ;
#41317 = DIRECTION('ref_axis',(0.707106781186552,0.707106781186543,1.53556032529733E-15)) ;
#41318 = DIRECTION('center_axis',(-1.66533453692965E-16,-1.,-1.66321791214593E-16)) ;
#41319 = DIRECTION('ref_axis',(-0.707106781186535,1.4966797377543E-19,0.70710678118656)) ;
#41320 = DIRECTION('center_axis',(0.,1.,0.)) ;
#41321 = DIRECTION('ref_axis',(-1.,0.,0.)) ;
#41322 = DIRECTION('',(-1.66533453692965E-16,-1.,-1.66321791214593E-16)) ;
#41323 = DIRECTION('',(-1.66533453692965E-16,-1.,-1.66321791214593E-16)) ;
#41324 = DIRECTION('center_axis',(-4.54195640846217E-14,1.66321791214601E-16,
-1.)) ;
#41325 = DIRECTION('ref_axis',(-1.,0.,4.54747350886464E-14)) ;
#41326 = DIRECTION('center_axis',(1.,2.84217094304056E-13,0.)) ;
#41327 = DIRECTION('ref_axis',(-2.84217094304056E-13,1.,0.)) ;
#41328 = DIRECTION('center_axis',(4.54195640846217E-14,-1.66321791214601E-16,
1.)) ;
#41329 = DIRECTION('ref_axis',(-1.,5.55236256206829E-46,4.54195640846217E-14)) ;
#41330 = DIRECTION('center_axis',(-2.1716102378779E-15,3.83420712807775E-28,
1.)) ;
#41331 = DIRECTION('ref_axis',(0.707106781186643,-0.707106781186452,1.53556032529807E-15)) ;
#41332 = DIRECTION('center_axis',(-1.,1.66533453692587E-16,4.54195640846217E-14)) ;
#41333 = DIRECTION('ref_axis',(3.22342386971791E-14,0.707106781186422,0.707106781186673)) ;
#41334 = DIRECTION('center_axis',(1.,0.,0.)) ;
#41335 = DIRECTION('ref_axis',(0.,1.,0.)) ;
#41336 = DIRECTION('',(-1.,1.66533453692587E-16,4.54195640846217E-14)) ;
#41337 = DIRECTION('',(-1.,1.66533453692587E-16,4.54195640846217E-14)) ;
#41338 = DIRECTION('center_axis',(-4.54195640846217E-14,1.66321791214601E-16,
-1.)) ;
#41339 = DIRECTION('ref_axis',(-1.,0.,4.54747350886464E-14)) ;
#41340 = DIRECTION('center_axis',(0.,-1.,0.)) ;
#41341 = DIRECTION('ref_axis',(1.,0.,-5.32907051820105E-14)) ;
#41342 = DIRECTION('center_axis',(4.54195640846217E-14,-1.66321791214601E-16,
1.)) ;
#41343 = DIRECTION('ref_axis',(-1.,5.55236256206829E-46,4.54195640846217E-14)) ;
#41344 = DIRECTION('center_axis',(2.17161023787787E-15,-3.83420712807771E-28,
-1.)) ;
#41345 = DIRECTION('ref_axis',(-0.707106781186552,-0.707106781186543,-1.53556032529731E-15)) ;
#41346 = DIRECTION('center_axis',(8.32667268460786E-17,1.,1.66321791214597E-16)) ;
#41347 = DIRECTION('ref_axis',(0.707106781186522,-1.76485733627007E-16,0.707106781186573)) ;
#41348 = DIRECTION('center_axis',(0.,-1.,0.)) ;
#41349 = DIRECTION('ref_axis',(1.,0.,1.77635683940035E-14)) ;
#41350 = DIRECTION('',(8.32667268460786E-17,1.,1.66321791214597E-16)) ;
#41351 = DIRECTION('center_axis',(-4.54195640846217E-14,1.66321791214601E-16,
-1.)) ;
#41352 = DIRECTION('ref_axis',(-1.,0.,4.54747350886464E-14)) ;
#41353 = DIRECTION('center_axis',(4.54195640846217E-14,-1.66321791214601E-16,
1.)) ;
#41354 = DIRECTION('ref_axis',(-1.,5.55236256206829E-46,4.54195640846217E-14)) ;
#41355 = DIRECTION('center_axis',(-2.17161023787787E-15,3.83815143260382E-28,
1.)) ;
#41356 = DIRECTION('ref_axis',(-0.707106781186643,0.707106781186452,-1.53556032529805E-15)) ;
#41357 = DIRECTION('center_axis',(-2.1716102378779E-15,3.83420712807775E-28,
1.)) ;
#41358 = DIRECTION('ref_axis',(0.707106781186643,-0.707106781186452,1.53556032529807E-15)) ;
#41359 = DIRECTION('',(-2.1716102378779E-15,3.83420712807775E-28,1.)) ;
#41360 = DIRECTION('center_axis',(2.1716102378779E-15,-3.83420712807775E-28,
-1.)) ;
#41361 = DIRECTION('ref_axis',(0.707106781186656,-0.707106781186439,1.5355603252981E-15)) ;
#41362 = DIRECTION('',(-2.1716102378779E-15,3.83322105194623E-28,1.)) ;
#41363 = DIRECTION('center_axis',(1.,-1.66533453692966E-16,2.1716102378779E-15)) ;
#41364 = DIRECTION('ref_axis',(-1.66533453692966E-16,-1.,3.82783884128008E-28)) ;
#41365 = DIRECTION('',(-2.1716102378779E-15,3.66854633798134E-28,1.)) ;
#41366 = DIRECTION('center_axis',(1.,-1.66533453692966E-16,2.1716102378779E-15)) ;
#41367 = DIRECTION('ref_axis',(-1.41780339089703E-15,0.707106781186483,0.707106781186612)) ;
#41368 = DIRECTION('',(-1.66533453692966E-16,-1.,3.83386399937507E-28)) ;
#41369 = DIRECTION('',(2.1716102378779E-15,-3.83815143260386E-28,-1.)) ;
#41370 = DIRECTION('',(-1.66533453692966E-16,-1.,3.83386399937507E-28)) ;
#41371 = DIRECTION('center_axis',(1.,-1.66533453692966E-16,2.1716102378779E-15)) ;
#41372 = DIRECTION('ref_axis',(-1.65331725969844E-15,-0.707106781186479,0.707106781186616)) ;
#41373 = DIRECTION('',(2.1716102378779E-15,-3.66854633798134E-28,-1.)) ;
#41374 = DIRECTION('center_axis',(2.1716102378779E-15,-3.83815143260386E-28,
-1.)) ;
#41375 = DIRECTION('ref_axis',(0.707106781186552,0.707106781186543,1.53556032529733E-15)) ;
#41376 = DIRECTION('',(-2.1716102378779E-15,3.83815143260386E-28,1.)) ;
#41377 = DIRECTION('center_axis',(2.1716102378779E-15,-3.83815143260386E-28,
-1.)) ;
#41378 = DIRECTION('ref_axis',(0.707106781186582,0.707106781186513,1.5355603252974E-15)) ;
#41379 = DIRECTION('center_axis',(1.66533453692966E-16,1.,-3.83386399937507E-28)) ;
#41380 = DIRECTION('ref_axis',(2.1716102378779E-15,-3.83748045690496E-28,
-1.)) ;
#41381 = DIRECTION('',(2.17161023787787E-15,-3.83815143260382E-28,-1.)) ;
#41382 = DIRECTION('',(1.,-1.66533453692966E-16,2.1716102378779E-15)) ;
#41383 = DIRECTION('center_axis',(1.,-1.66533453692966E-16,-4.54195640846217E-14)) ;
#41384 = DIRECTION('ref_axis',(3.19987248283774E-14,-0.707106781186434,0.707106781186661)) ;
#41385 = DIRECTION('center_axis',(1.,0.,0.)) ;
#41386 = DIRECTION('ref_axis',(0.,0.,1.)) ;
#41387 = DIRECTION('',(1.,-1.66533453692966E-16,-4.54195640846217E-14)) ;
#41388 = DIRECTION('center_axis',(-1.,0.,0.)) ;
#41389 = DIRECTION('ref_axis',(0.,-1.,0.)) ;
#41390 = DIRECTION('',(1.,-1.66533453692966E-16,-4.54195640846217E-14)) ;
#41391 = DIRECTION('center_axis',(-4.54195640846217E-14,1.66321791214601E-16,
-1.)) ;
#41392 = DIRECTION('ref_axis',(-1.,0.,4.54747350886464E-14)) ;
#41393 = DIRECTION('center_axis',(0.,1.,0.)) ;
#41394 = DIRECTION('ref_axis',(-1.,0.,5.32907051820105E-14)) ;
#41395 = DIRECTION('center_axis',(4.54195640846217E-14,-1.66321791214601E-16,
1.)) ;
#41396 = DIRECTION('ref_axis',(-1.,5.55236256206829E-46,4.54195640846217E-14)) ;
#41397 = DIRECTION('center_axis',(2.1716102378779E-15,-3.83815143260386E-28,
-1.)) ;
#41398 = DIRECTION('ref_axis',(0.707106781186552,0.707106781186543,1.53556032529733E-15)) ;
#41399 = DIRECTION('center_axis',(-1.66533453692965E-16,-1.,-1.66321791214593E-16)) ;
#41400 = DIRECTION('ref_axis',(-0.707106781186535,1.4966797377543E-19,0.70710678118656)) ;
#41401 = DIRECTION('center_axis',(0.,1.,0.)) ;
#41402 = DIRECTION('ref_axis',(-1.,0.,0.)) ;
#41403 = DIRECTION('',(-1.66533453692965E-16,-1.,-1.66321791214593E-16)) ;
#41404 = DIRECTION('',(-1.66533453692965E-16,-1.,-1.66321791214593E-16)) ;
#41405 = DIRECTION('center_axis',(-4.54195640846217E-14,1.66321791214601E-16,
-1.)) ;
#41406 = DIRECTION('ref_axis',(-1.,0.,4.54747350886464E-14)) ;
#41407 = DIRECTION('center_axis',(1.,2.84217094304056E-13,0.)) ;
#41408 = DIRECTION('ref_axis',(-2.84217094304056E-13,1.,0.)) ;
#41409 = DIRECTION('center_axis',(4.54195640846217E-14,-1.66321791214601E-16,
1.)) ;
#41410 = DIRECTION('ref_axis',(-1.,5.55236256206829E-46,4.54195640846217E-14)) ;
#41411 = DIRECTION('center_axis',(-2.1716102378779E-15,3.83420712807775E-28,
1.)) ;
#41412 = DIRECTION('ref_axis',(0.707106781186643,-0.707106781186452,1.53556032529807E-15)) ;
#41413 = DIRECTION('center_axis',(-1.,1.66533453692587E-16,4.54195640846217E-14)) ;
#41414 = DIRECTION('ref_axis',(3.22342386971791E-14,0.707106781186422,0.707106781186673)) ;
#41415 = DIRECTION('center_axis',(1.,0.,0.)) ;
#41416 = DIRECTION('ref_axis',(0.,1.,0.)) ;
#41417 = DIRECTION('',(-1.,1.66533453692587E-16,4.54195640846217E-14)) ;
#41418 = DIRECTION('',(-1.,1.66533453692587E-16,4.54195640846217E-14)) ;
#41419 = DIRECTION('center_axis',(-4.54195640846217E-14,1.66321791214601E-16,
-1.)) ;
#41420 = DIRECTION('ref_axis',(-1.,0.,4.54747350886464E-14)) ;
#41421 = DIRECTION('center_axis',(0.,-1.,0.)) ;
#41422 = DIRECTION('ref_axis',(1.,0.,-5.32907051820105E-14)) ;
#41423 = DIRECTION('center_axis',(4.54195640846217E-14,-1.66321791214601E-16,
1.)) ;
#41424 = DIRECTION('ref_axis',(-1.,5.55236256206829E-46,4.54195640846217E-14)) ;
#41425 = DIRECTION('center_axis',(2.17161023787787E-15,-3.83420712807771E-28,
-1.)) ;
#41426 = DIRECTION('ref_axis',(-0.707106781186552,-0.707106781186543,-1.53556032529731E-15)) ;
#41427 = DIRECTION('center_axis',(8.32667268460786E-17,1.,1.66321791214597E-16)) ;
#41428 = DIRECTION('ref_axis',(0.707106781186522,-1.76485733627007E-16,0.707106781186573)) ;
#41429 = DIRECTION('center_axis',(0.,-1.,0.)) ;
#41430 = DIRECTION('ref_axis',(1.,0.,1.77635683940035E-14)) ;
#41431 = DIRECTION('',(8.32667268460786E-17,1.,1.66321791214597E-16)) ;
#41432 = DIRECTION('center_axis',(-4.54195640846217E-14,1.66321791214601E-16,
-1.)) ;
#41433 = DIRECTION('ref_axis',(-1.,0.,4.54747350886464E-14)) ;
#41434 = DIRECTION('center_axis',(4.54195640846217E-14,-1.66321791214601E-16,
1.)) ;
#41435 = DIRECTION('ref_axis',(-1.,5.55236256206829E-46,4.54195640846217E-14)) ;
#41436 = DIRECTION('center_axis',(-2.17161023787787E-15,3.83815143260382E-28,
1.)) ;
#41437 = DIRECTION('ref_axis',(-0.707106781186643,0.707106781186452,-1.53556032529805E-15)) ;
#41438 = DIRECTION('center_axis',(-2.1716102378779E-15,3.83420712807775E-28,
1.)) ;
#41439 = DIRECTION('ref_axis',(0.707106781186643,-0.707106781186452,1.53556032529807E-15)) ;
#41440 = DIRECTION('',(-2.1716102378779E-15,3.83420712807775E-28,1.)) ;
#41441 = DIRECTION('center_axis',(2.1716102378779E-15,-3.83420712807775E-28,
-1.)) ;
#41442 = DIRECTION('ref_axis',(0.707106781186656,-0.707106781186439,1.5355603252981E-15)) ;
#41443 = DIRECTION('',(-2.1716102378779E-15,3.83322105194623E-28,1.)) ;
#41444 = DIRECTION('center_axis',(1.,-1.66533453692966E-16,2.1716102378779E-15)) ;
#41445 = DIRECTION('ref_axis',(-1.66533453692966E-16,-1.,3.82783884128008E-28)) ;
#41446 = DIRECTION('',(-2.1716102378779E-15,3.66854633798134E-28,1.)) ;
#41447 = DIRECTION('center_axis',(1.,-1.66533453692966E-16,2.1716102378779E-15)) ;
#41448 = DIRECTION('ref_axis',(-1.41780339089703E-15,0.707106781186483,0.707106781186612)) ;
#41449 = DIRECTION('',(-1.66533453692966E-16,-1.,3.83386399937507E-28)) ;
#41450 = DIRECTION('',(2.1716102378779E-15,-3.83815143260386E-28,-1.)) ;
#41451 = DIRECTION('',(-1.66533453692966E-16,-1.,3.83386399937507E-28)) ;
#41452 = DIRECTION('center_axis',(1.,-1.66533453692966E-16,2.1716102378779E-15)) ;
#41453 = DIRECTION('ref_axis',(-1.65331725969844E-15,-0.707106781186479,0.707106781186616)) ;
#41454 = DIRECTION('',(2.1716102378779E-15,-3.66854633798134E-28,-1.)) ;
#41455 = DIRECTION('center_axis',(2.1716102378779E-15,-3.83815143260386E-28,
-1.)) ;
#41456 = DIRECTION('ref_axis',(0.707106781186552,0.707106781186543,1.53556032529733E-15)) ;
#41457 = DIRECTION('',(-2.1716102378779E-15,3.83815143260386E-28,1.)) ;
#41458 = DIRECTION('center_axis',(2.1716102378779E-15,-3.83815143260386E-28,
-1.)) ;
#41459 = DIRECTION('ref_axis',(0.707106781186582,0.707106781186513,1.5355603252974E-15)) ;
#41460 = DIRECTION('center_axis',(1.66533453692966E-16,1.,-3.83386399937507E-28)) ;
#41461 = DIRECTION('ref_axis',(2.1716102378779E-15,-3.83748045690496E-28,
-1.)) ;
#41462 = DIRECTION('',(2.17161023787787E-15,-3.83815143260382E-28,-1.)) ;
#41463 = DIRECTION('',(1.,-1.66533453692966E-16,2.1716102378779E-15)) ;
#41464 = DIRECTION('center_axis',(1.,-1.66533453692966E-16,-4.54195640846217E-14)) ;
#41465 = DIRECTION('ref_axis',(3.19987248283774E-14,-0.707106781186434,0.707106781186661)) ;
#41466 = DIRECTION('center_axis',(1.,0.,0.)) ;
#41467 = DIRECTION('ref_axis',(0.,0.,1.)) ;
#41468 = DIRECTION('',(1.,-1.66533453692966E-16,-4.54195640846217E-14)) ;
#41469 = DIRECTION('center_axis',(-1.,0.,0.)) ;
#41470 = DIRECTION('ref_axis',(0.,-1.,0.)) ;
#41471 = DIRECTION('',(1.,-1.66533453692966E-16,-4.54195640846217E-14)) ;
#41472 = DIRECTION('center_axis',(-4.54195640846217E-14,1.66321791214601E-16,
-1.)) ;
#41473 = DIRECTION('ref_axis',(-1.,0.,4.54747350886464E-14)) ;
#41474 = DIRECTION('center_axis',(0.,1.,0.)) ;
#41475 = DIRECTION('ref_axis',(-1.,0.,5.32907051820105E-14)) ;
#41476 = DIRECTION('center_axis',(4.54195640846217E-14,-1.66321791214601E-16,
1.)) ;
#41477 = DIRECTION('ref_axis',(-1.,5.55236256206829E-46,4.54195640846217E-14)) ;
#41478 = DIRECTION('center_axis',(2.1716102378779E-15,-3.83815143260386E-28,
-1.)) ;
#41479 = DIRECTION('ref_axis',(0.707106781186552,0.707106781186543,1.53556032529733E-15)) ;
#41480 = DIRECTION('center_axis',(-1.66533453692965E-16,-1.,-1.66321791214593E-16)) ;
#41481 = DIRECTION('ref_axis',(-0.707106781186535,1.4966797377543E-19,0.70710678118656)) ;
#41482 = DIRECTION('center_axis',(0.,1.,0.)) ;
#41483 = DIRECTION('ref_axis',(-1.,0.,0.)) ;
#41484 = DIRECTION('',(-1.66533453692965E-16,-1.,-1.66321791214593E-16)) ;
#41485 = DIRECTION('',(-1.66533453692965E-16,-1.,-1.66321791214593E-16)) ;
#41486 = DIRECTION('center_axis',(-4.54195640846217E-14,1.66321791214601E-16,
-1.)) ;
#41487 = DIRECTION('ref_axis',(-1.,0.,4.54747350886464E-14)) ;
#41488 = DIRECTION('center_axis',(1.,2.84217094304056E-13,0.)) ;
#41489 = DIRECTION('ref_axis',(-2.84217094304056E-13,1.,0.)) ;
#41490 = DIRECTION('center_axis',(4.54195640846217E-14,-1.66321791214601E-16,
1.)) ;
#41491 = DIRECTION('ref_axis',(-1.,5.55236256206829E-46,4.54195640846217E-14)) ;
#41492 = DIRECTION('center_axis',(-2.1716102378779E-15,3.83420712807775E-28,
1.)) ;
#41493 = DIRECTION('ref_axis',(0.707106781186643,-0.707106781186452,1.53556032529807E-15)) ;
#41494 = DIRECTION('center_axis',(-1.,1.66533453692587E-16,4.54195640846217E-14)) ;
#41495 = DIRECTION('ref_axis',(3.22342386971791E-14,0.707106781186422,0.707106781186673)) ;
#41496 = DIRECTION('center_axis',(1.,0.,0.)) ;
#41497 = DIRECTION('ref_axis',(0.,1.,0.)) ;
#41498 = DIRECTION('',(-1.,1.66533453692587E-16,4.54195640846217E-14)) ;
#41499 = DIRECTION('',(-1.,1.66533453692587E-16,4.54195640846217E-14)) ;
#41500 = DIRECTION('center_axis',(-4.54195640846217E-14,1.66321791214601E-16,
-1.)) ;
#41501 = DIRECTION('ref_axis',(-1.,0.,4.54747350886464E-14)) ;
#41502 = DIRECTION('center_axis',(0.,-1.,0.)) ;
#41503 = DIRECTION('ref_axis',(1.,0.,-5.32907051820105E-14)) ;
#41504 = DIRECTION('center_axis',(4.54195640846217E-14,-1.66321791214601E-16,
1.)) ;
#41505 = DIRECTION('ref_axis',(-1.,5.55236256206829E-46,4.54195640846217E-14)) ;
#41506 = DIRECTION('center_axis',(2.17161023787787E-15,-3.83420712807771E-28,
-1.)) ;
#41507 = DIRECTION('ref_axis',(-0.707106781186552,-0.707106781186543,-1.53556032529731E-15)) ;
#41508 = DIRECTION('center_axis',(8.32667268460786E-17,1.,1.66321791214597E-16)) ;
#41509 = DIRECTION('ref_axis',(0.707106781186522,-1.76485733627007E-16,0.707106781186573)) ;
#41510 = DIRECTION('center_axis',(0.,-1.,0.)) ;
#41511 = DIRECTION('ref_axis',(1.,0.,1.77635683940035E-14)) ;
#41512 = DIRECTION('',(8.32667268460786E-17,1.,1.66321791214597E-16)) ;
#41513 = DIRECTION('center_axis',(-4.54195640846217E-14,1.66321791214601E-16,
-1.)) ;
#41514 = DIRECTION('ref_axis',(-1.,0.,4.54747350886464E-14)) ;
#41515 = DIRECTION('center_axis',(4.54195640846217E-14,-1.66321791214601E-16,
1.)) ;
#41516 = DIRECTION('ref_axis',(-1.,5.55236256206829E-46,4.54195640846217E-14)) ;
#41517 = DIRECTION('center_axis',(-2.17161023787787E-15,3.83815143260382E-28,
1.)) ;
#41518 = DIRECTION('ref_axis',(-0.707106781186643,0.707106781186452,-1.53556032529805E-15)) ;
#41519 = DIRECTION('center_axis',(-2.1716102378779E-15,3.83420712807775E-28,
1.)) ;
#41520 = DIRECTION('ref_axis',(0.707106781186643,-0.707106781186452,1.53556032529807E-15)) ;
#41521 = DIRECTION('',(-2.1716102378779E-15,3.83420712807775E-28,1.)) ;
#41522 = DIRECTION('center_axis',(2.1716102378779E-15,-3.83420712807775E-28,
-1.)) ;
#41523 = DIRECTION('ref_axis',(0.707106781186656,-0.707106781186439,1.5355603252981E-15)) ;
#41524 = DIRECTION('',(-2.1716102378779E-15,3.83322105194623E-28,1.)) ;
#41525 = DIRECTION('center_axis',(1.,-1.66533453692966E-16,2.1716102378779E-15)) ;
#41526 = DIRECTION('ref_axis',(-1.66533453692966E-16,-1.,3.82783884128008E-28)) ;
#41527 = DIRECTION('',(-2.1716102378779E-15,3.66854633798134E-28,1.)) ;
#41528 = DIRECTION('center_axis',(1.,-1.66533453692966E-16,2.1716102378779E-15)) ;
#41529 = DIRECTION('ref_axis',(-1.41780339089703E-15,0.707106781186483,0.707106781186612)) ;
#41530 = DIRECTION('',(-1.66533453692966E-16,-1.,3.83386399937507E-28)) ;
#41531 = DIRECTION('',(2.1716102378779E-15,-3.83815143260386E-28,-1.)) ;
#41532 = DIRECTION('',(-1.66533453692966E-16,-1.,3.83386399937507E-28)) ;
#41533 = DIRECTION('center_axis',(1.,-1.66533453692966E-16,2.1716102378779E-15)) ;
#41534 = DIRECTION('ref_axis',(-1.65331725969844E-15,-0.707106781186479,0.707106781186616)) ;
#41535 = DIRECTION('',(2.1716102378779E-15,-3.66854633798134E-28,-1.)) ;
#41536 = DIRECTION('center_axis',(2.1716102378779E-15,-3.83815143260386E-28,
-1.)) ;
#41537 = DIRECTION('ref_axis',(0.707106781186552,0.707106781186543,1.53556032529733E-15)) ;
#41538 = DIRECTION('',(-2.1716102378779E-15,3.83815143260386E-28,1.)) ;
#41539 = DIRECTION('center_axis',(2.1716102378779E-15,-3.83815143260386E-28,
-1.)) ;
#41540 = DIRECTION('ref_axis',(0.707106781186582,0.707106781186513,1.5355603252974E-15)) ;
#41541 = DIRECTION('center_axis',(1.66533453692966E-16,1.,-3.83386399937507E-28)) ;
#41542 = DIRECTION('ref_axis',(2.1716102378779E-15,-3.83748045690496E-28,
-1.)) ;
#41543 = DIRECTION('',(2.17161023787787E-15,-3.83815143260382E-28,-1.)) ;
#41544 = DIRECTION('',(1.,-1.66533453692966E-16,2.1716102378779E-15)) ;
#41545 = DIRECTION('center_axis',(1.,-1.66533453692966E-16,-4.54195640846217E-14)) ;
#41546 = DIRECTION('ref_axis',(3.19987248283774E-14,-0.707106781186434,0.707106781186661)) ;
#41547 = DIRECTION('center_axis',(1.,0.,0.)) ;
#41548 = DIRECTION('ref_axis',(0.,0.,1.)) ;
#41549 = DIRECTION('',(1.,-1.66533453692966E-16,-4.54195640846217E-14)) ;
#41550 = DIRECTION('center_axis',(-1.,0.,0.)) ;
#41551 = DIRECTION('ref_axis',(0.,-1.,0.)) ;
#41552 = DIRECTION('',(1.,-1.66533453692966E-16,-4.54195640846217E-14)) ;
#41553 = DIRECTION('center_axis',(-4.54195640846217E-14,1.66321791214601E-16,
-1.)) ;
#41554 = DIRECTION('ref_axis',(-1.,0.,4.54747350886464E-14)) ;
#41555 = DIRECTION('center_axis',(0.,1.,0.)) ;
#41556 = DIRECTION('ref_axis',(-1.,0.,5.32907051820105E-14)) ;
#41557 = DIRECTION('center_axis',(4.54195640846217E-14,-1.66321791214601E-16,
1.)) ;
#41558 = DIRECTION('ref_axis',(-1.,5.55236256206829E-46,4.54195640846217E-14)) ;
#41559 = DIRECTION('center_axis',(2.1716102378779E-15,-3.83815143260386E-28,
-1.)) ;
#41560 = DIRECTION('ref_axis',(0.707106781186552,0.707106781186543,1.53556032529733E-15)) ;
#41561 = DIRECTION('center_axis',(-1.66533453692965E-16,-1.,-1.66321791214593E-16)) ;
#41562 = DIRECTION('ref_axis',(-0.707106781186535,1.4966797377543E-19,0.70710678118656)) ;
#41563 = DIRECTION('center_axis',(0.,1.,0.)) ;
#41564 = DIRECTION('ref_axis',(-1.,0.,0.)) ;
#41565 = DIRECTION('',(-1.66533453692965E-16,-1.,-1.66321791214593E-16)) ;
#41566 = DIRECTION('',(-1.66533453692965E-16,-1.,-1.66321791214593E-16)) ;
#41567 = DIRECTION('center_axis',(-4.54195640846217E-14,1.66321791214601E-16,
-1.)) ;
#41568 = DIRECTION('ref_axis',(-1.,0.,4.54747350886464E-14)) ;
#41569 = DIRECTION('center_axis',(1.,2.84217094304056E-13,0.)) ;
#41570 = DIRECTION('ref_axis',(-2.84217094304056E-13,1.,0.)) ;
#41571 = DIRECTION('center_axis',(4.54195640846217E-14,-1.66321791214601E-16,
1.)) ;
#41572 = DIRECTION('ref_axis',(-1.,5.55236256206829E-46,4.54195640846217E-14)) ;
#41573 = DIRECTION('center_axis',(-2.1716102378779E-15,3.83420712807775E-28,
1.)) ;
#41574 = DIRECTION('ref_axis',(0.707106781186643,-0.707106781186452,1.53556032529807E-15)) ;
#41575 = DIRECTION('center_axis',(-1.,1.66533453692587E-16,4.54195640846217E-14)) ;
#41576 = DIRECTION('ref_axis',(3.22342386971791E-14,0.707106781186422,0.707106781186673)) ;
#41577 = DIRECTION('center_axis',(1.,0.,0.)) ;
#41578 = DIRECTION('ref_axis',(0.,1.,0.)) ;
#41579 = DIRECTION('',(-1.,1.66533453692587E-16,4.54195640846217E-14)) ;
#41580 = DIRECTION('',(-1.,1.66533453692587E-16,4.54195640846217E-14)) ;
#41581 = DIRECTION('center_axis',(-4.54195640846217E-14,1.66321791214601E-16,
-1.)) ;
#41582 = DIRECTION('ref_axis',(-1.,0.,4.54747350886464E-14)) ;
#41583 = DIRECTION('center_axis',(0.,-1.,0.)) ;
#41584 = DIRECTION('ref_axis',(1.,0.,-5.32907051820105E-14)) ;
#41585 = DIRECTION('center_axis',(4.54195640846217E-14,-1.66321791214601E-16,
1.)) ;
#41586 = DIRECTION('ref_axis',(-1.,5.55236256206829E-46,4.54195640846217E-14)) ;
#41587 = DIRECTION('center_axis',(2.17161023787787E-15,-3.83420712807771E-28,
-1.)) ;
#41588 = DIRECTION('ref_axis',(-0.707106781186552,-0.707106781186543,-1.53556032529731E-15)) ;
#41589 = DIRECTION('center_axis',(8.32667268460786E-17,1.,1.66321791214597E-16)) ;
#41590 = DIRECTION('ref_axis',(0.707106781186522,-1.76485733627007E-16,0.707106781186573)) ;
#41591 = DIRECTION('center_axis',(0.,-1.,0.)) ;
#41592 = DIRECTION('ref_axis',(1.,0.,1.77635683940035E-14)) ;
#41593 = DIRECTION('',(8.32667268460786E-17,1.,1.66321791214597E-16)) ;
#41594 = DIRECTION('center_axis',(-4.54195640846217E-14,1.66321791214601E-16,
-1.)) ;
#41595 = DIRECTION('ref_axis',(-1.,0.,4.54747350886464E-14)) ;
#41596 = DIRECTION('center_axis',(4.54195640846217E-14,-1.66321791214601E-16,
1.)) ;
#41597 = DIRECTION('ref_axis',(-1.,5.55236256206829E-46,4.54195640846217E-14)) ;
#41598 = DIRECTION('center_axis',(-2.17161023787787E-15,3.83815143260382E-28,
1.)) ;
#41599 = DIRECTION('ref_axis',(-0.707106781186643,0.707106781186452,-1.53556032529805E-15)) ;
#41600 = DIRECTION('center_axis',(-2.1716102378779E-15,3.83420712807775E-28,
1.)) ;
#41601 = DIRECTION('ref_axis',(0.707106781186643,-0.707106781186452,1.53556032529807E-15)) ;
#41602 = DIRECTION('',(-2.1716102378779E-15,3.83420712807775E-28,1.)) ;
#41603 = DIRECTION('center_axis',(2.1716102378779E-15,-3.83420712807775E-28,
-1.)) ;
#41604 = DIRECTION('ref_axis',(0.707106781186656,-0.707106781186439,1.5355603252981E-15)) ;
#41605 = DIRECTION('',(-2.1716102378779E-15,3.83322105194623E-28,1.)) ;
#41606 = DIRECTION('center_axis',(1.,-1.66533453692966E-16,2.1716102378779E-15)) ;
#41607 = DIRECTION('ref_axis',(-1.66533453692966E-16,-1.,3.82783884128008E-28)) ;
#41608 = DIRECTION('',(-2.1716102378779E-15,3.66854633798134E-28,1.)) ;
#41609 = DIRECTION('center_axis',(1.,-1.66533453692966E-16,2.1716102378779E-15)) ;
#41610 = DIRECTION('ref_axis',(-1.41780339089703E-15,0.707106781186483,0.707106781186612)) ;
#41611 = DIRECTION('',(-1.66533453692966E-16,-1.,3.83386399937507E-28)) ;
#41612 = DIRECTION('',(2.1716102378779E-15,-3.83815143260386E-28,-1.)) ;
#41613 = DIRECTION('',(-1.66533453692966E-16,-1.,3.83386399937507E-28)) ;
#41614 = DIRECTION('center_axis',(1.,-1.66533453692966E-16,2.1716102378779E-15)) ;
#41615 = DIRECTION('ref_axis',(-1.65331725969844E-15,-0.707106781186479,0.707106781186616)) ;
#41616 = DIRECTION('',(2.1716102378779E-15,-3.66854633798134E-28,-1.)) ;
#41617 = DIRECTION('center_axis',(2.1716102378779E-15,-3.83815143260386E-28,
-1.)) ;
#41618 = DIRECTION('ref_axis',(0.707106781186552,0.707106781186543,1.53556032529733E-15)) ;
#41619 = DIRECTION('',(-2.1716102378779E-15,3.83815143260386E-28,1.)) ;
#41620 = DIRECTION('center_axis',(2.1716102378779E-15,-3.83815143260386E-28,
-1.)) ;
#41621 = DIRECTION('ref_axis',(0.707106781186582,0.707106781186513,1.5355603252974E-15)) ;
#41622 = DIRECTION('center_axis',(1.66533453692966E-16,1.,-3.83386399937507E-28)) ;
#41623 = DIRECTION('ref_axis',(2.1716102378779E-15,-3.83748045690496E-28,
-1.)) ;
#41624 = DIRECTION('',(2.17161023787787E-15,-3.83815143260382E-28,-1.)) ;
#41625 = DIRECTION('',(1.,-1.66533453692966E-16,2.1716102378779E-15)) ;
#41626 = DIRECTION('center_axis',(1.,-1.66533453692966E-16,-4.54195640846217E-14)) ;
#41627 = DIRECTION('ref_axis',(3.19987248283774E-14,-0.707106781186434,0.707106781186661)) ;
#41628 = DIRECTION('center_axis',(1.,0.,0.)) ;
#41629 = DIRECTION('ref_axis',(0.,0.,1.)) ;
#41630 = DIRECTION('',(1.,-1.66533453692966E-16,-4.54195640846217E-14)) ;
#41631 = DIRECTION('center_axis',(-1.,0.,0.)) ;
#41632 = DIRECTION('ref_axis',(0.,-1.,0.)) ;
#41633 = DIRECTION('',(-1.,1.66533453692966E-16,4.54195640846217E-14)) ;
#41634 = DIRECTION('center_axis',(-4.54195640846217E-14,1.66321791214601E-16,
-1.)) ;
#41635 = DIRECTION('ref_axis',(-1.,0.,4.54747350886464E-14)) ;
#41636 = DIRECTION('center_axis',(0.,1.,0.)) ;
#41637 = DIRECTION('ref_axis',(-1.,0.,5.32907051820105E-14)) ;
#41638 = DIRECTION('center_axis',(4.54195640846217E-14,-1.66321791214601E-16,
1.)) ;
#41639 = DIRECTION('ref_axis',(0.707106781186502,0.707106781186593,-3.1998874496344E-14)) ;
#41640 = DIRECTION('center_axis',(-4.54195640846217E-14,1.66321791214601E-16,
-1.)) ;
#41641 = DIRECTION('ref_axis',(0.707106781186502,0.707106781186593,-3.1998874496344E-14)) ;
#41642 = DIRECTION('center_axis',(-8.32667268460786E-17,-1.,-1.66321791214597E-16)) ;
#41643 = DIRECTION('ref_axis',(-0.707106781186535,-5.87287992268677E-17,0.70710678118656)) ;
#41644 = DIRECTION('center_axis',(0.,1.,0.)) ;
#41645 = DIRECTION('ref_axis',(-1.,0.,0.)) ;
#41646 = DIRECTION('',(8.32667268460786E-17,1.,1.66321791214597E-16)) ;
#41647 = DIRECTION('',(-8.32667268460786E-17,-1.,-1.66321791214597E-16)) ;
#41648 = DIRECTION('center_axis',(-4.54195640846217E-14,1.66321791214601E-16,
-1.)) ;
#41649 = DIRECTION('ref_axis',(-1.,0.,4.54747350886464E-14)) ;
#41650 = DIRECTION('center_axis',(1.,2.84217094304056E-13,0.)) ;
#41651 = DIRECTION('ref_axis',(-2.84217094304056E-13,1.,0.)) ;
#41652 = DIRECTION('center_axis',(4.54195640846217E-14,-1.66321791214601E-16,
1.)) ;
#41653 = DIRECTION('ref_axis',(0.707106781186502,-0.707106781186593,-3.22340890291979E-14)) ;
#41654 = DIRECTION('center_axis',(-4.54195640846217E-14,1.66321791214601E-16,
-1.)) ;
#41655 = DIRECTION('ref_axis',(0.707106781186502,-0.707106781186593,-3.22340890291979E-14)) ;
#41656 = DIRECTION('center_axis',(-1.,1.66533453692587E-16,4.54195640846217E-14)) ;
#41657 = DIRECTION('ref_axis',(3.22342386971791E-14,0.707106781186422,0.707106781186673)) ;
#41658 = DIRECTION('center_axis',(1.,0.,0.)) ;
#41659 = DIRECTION('ref_axis',(0.,1.,0.)) ;
#41660 = DIRECTION('',(1.,-1.66533453692587E-16,-4.54195640846217E-14)) ;
#41661 = DIRECTION('',(-1.,1.66533453692587E-16,4.54195640846217E-14)) ;
#41662 = DIRECTION('center_axis',(-4.54195640846217E-14,1.66321791214601E-16,
-1.)) ;
#41663 = DIRECTION('ref_axis',(-1.,0.,4.54747350886464E-14)) ;
#41664 = DIRECTION('center_axis',(0.,-1.,0.)) ;
#41665 = DIRECTION('ref_axis',(1.,0.,-5.32907051820105E-14)) ;
#41666 = DIRECTION('center_axis',(4.54195640846217E-14,-1.66321791214601E-16,
1.)) ;
#41667 = DIRECTION('ref_axis',(-0.707106781186593,-0.707106781186502,3.19988744963481E-14)) ;
#41668 = DIRECTION('center_axis',(-4.54195640846217E-14,1.66321791214601E-16,
-1.)) ;
#41669 = DIRECTION('ref_axis',(-0.707106781186593,-0.707106781186502,3.19988744963481E-14)) ;
#41670 = DIRECTION('center_axis',(1.66533453692965E-16,1.,1.66321791214593E-16)) ;
#41671 = DIRECTION('ref_axis',(0.707106781186535,-2.35364200827643E-16,0.70710678118656)) ;
#41672 = DIRECTION('center_axis',(0.,-1.,0.)) ;
#41673 = DIRECTION('ref_axis',(1.,0.,0.)) ;
#41674 = DIRECTION('',(-1.66533453692965E-16,-1.,-1.66321791214593E-16)) ;
#41675 = DIRECTION('',(1.66533453692965E-16,1.,1.66321791214593E-16)) ;
#41676 = DIRECTION('center_axis',(-4.54195640846217E-14,1.66321791214601E-16,
-1.)) ;
#41677 = DIRECTION('ref_axis',(-1.,0.,4.54747350886464E-14)) ;
#41678 = DIRECTION('center_axis',(4.54195640846217E-14,-1.66321791214601E-16,
1.)) ;
#41679 = DIRECTION('ref_axis',(-0.707106781186735,0.70710678118636,3.22340890292084E-14)) ;
#41680 = DIRECTION('center_axis',(-4.54195640846217E-14,1.66321791214601E-16,
-1.)) ;
#41681 = DIRECTION('ref_axis',(-0.707106781186735,0.70710678118636,3.22340890292084E-14)) ;
#41682 = DIRECTION('center_axis',(-2.17161023787787E-15,3.83420712807771E-28,
1.)) ;
#41683 = DIRECTION('ref_axis',(0.707106781186543,-0.707106781186552,1.53556032529783E-15)) ;
#41684 = DIRECTION('',(-2.17161023787787E-15,3.83420712807771E-28,1.)) ;
#41685 = DIRECTION('center_axis',(2.17161023787792E-15,-2.90739654573749E-15,
-1.)) ;
#41686 = DIRECTION('ref_axis',(1.35627620245787E-13,-1.,2.90739654573778E-15)) ;
#41687 = DIRECTION('',(2.17161023787787E-15,-3.83420712807771E-28,-1.)) ;
#41688 = DIRECTION('center_axis',(1.,-8.32667268460789E-17,2.17161023787787E-15)) ;
#41689 = DIRECTION('ref_axis',(-8.32667268460789E-17,-1.,3.92101138914083E-28)) ;
#41690 = DIRECTION('',(2.17161023787787E-15,-3.83815143260382E-28,-1.)) ;
#41691 = DIRECTION('',(-8.32667268460789E-17,-1.,3.83780830390118E-28)) ;
#41692 = DIRECTION('center_axis',(2.17161023787787E-15,-3.83815143260382E-28,
-1.)) ;
#41693 = DIRECTION('ref_axis',(0.707106781186452,0.707106781186643,1.53556032529709E-15)) ;
#41694 = DIRECTION('',(-2.17161023787787E-15,3.83815143260382E-28,1.)) ;
#41695 = DIRECTION('center_axis',(2.17161023787746E-15,-7.39616701217516E-14,
-1.)) ;
#41696 = DIRECTION('ref_axis',(1.,-6.48092690624108E-15,2.17161023787794E-15)) ;
#41697 = DIRECTION('center_axis',(1.66533453692966E-16,1.,-3.83386399937507E-28)) ;
#41698 = DIRECTION('ref_axis',(2.1716102378779E-15,-3.83748045690496E-28,
-1.)) ;
#41699 = DIRECTION('',(2.1716102378779E-15,-3.83815143260386E-28,-1.)) ;
#41700 = DIRECTION('',(1.,-1.66533453692966E-16,2.1716102378779E-15)) ;
#41701 = DIRECTION('center_axis',(4.54195640846217E-14,-1.66321791214601E-16,
1.)) ;
#41702 = DIRECTION('ref_axis',(1.75658099177411E-13,1.,1.66321791206623E-16)) ;
#41703 = DIRECTION('',(-1.,1.75658099177411E-13,4.54195640846217E-14)) ;
#41704 = DIRECTION('',(1.75658099177411E-13,1.,1.66321791206623E-16)) ;
#41705 = DIRECTION('',(1.,-1.75658099177411E-13,-4.54195640846217E-14)) ;
#41706 = DIRECTION('',(-1.75658099177411E-13,-1.,-1.66321791206623E-16)) ;
#41707 = DIRECTION('',(-1.,1.66533453692966E-16,4.54195640846217E-14)) ;
#41708 = DIRECTION('center_axis',(4.54195640846217E-14,-1.66321791214601E-16,
1.)) ;
#41709 = DIRECTION('ref_axis',(0.707106781186502,0.707106781186593,-3.1998874496344E-14)) ;
#41710 = DIRECTION('',(1.66533453692965E-16,1.,1.66321791214593E-16)) ;
#41711 = DIRECTION('center_axis',(4.54195640846217E-14,-1.66321791214601E-16,
1.)) ;
#41712 = DIRECTION('ref_axis',(0.707106781186644,-0.707106781186451,-3.22340890292043E-14)) ;
#41713 = DIRECTION('',(1.,-1.66533453692587E-16,-4.54195640846217E-14)) ;
#41714 = DIRECTION('center_axis',(4.54195640846217E-14,-1.66321791214601E-16,
1.)) ;
#41715 = DIRECTION('ref_axis',(-0.707106781186593,-0.707106781186502,3.19988744963481E-14)) ;
#41716 = DIRECTION('',(-8.32667268460786E-17,-1.,-1.66321791214597E-16)) ;
#41717 = DIRECTION('center_axis',(4.54195640846217E-14,-1.66321791214601E-16,
1.)) ;
#41718 = DIRECTION('ref_axis',(-0.707106781186735,0.70710678118636,3.22340890292084E-14)) ;
#41719 = DIRECTION('center_axis',(-2.16239769233719E-14,8.31608956071042E-17,
-1.)) ;
#41720 = DIRECTION('ref_axis',(1.,-9.64599832246215E-47,-2.16239769233719E-14)) ;
#41721 = DIRECTION('center_axis',(1.,-1.66533453692966E-16,-4.54195640846217E-14)) ;
#41722 = DIRECTION('ref_axis',(3.19987248283774E-14,-0.707106781186434,0.707106781186661)) ;
#41723 = DIRECTION('center_axis',(1.,0.,0.)) ;
#41724 = DIRECTION('ref_axis',(0.,0.,1.)) ;
#41725 = DIRECTION('',(1.,-1.66533453692966E-16,-4.54195640846217E-14)) ;
#41726 = DIRECTION('center_axis',(-1.,0.,0.)) ;
#41727 = DIRECTION('ref_axis',(0.,-1.,0.)) ;
#41728 = DIRECTION('center_axis',(-4.54195640846217E-14,1.66321791214601E-16,
-1.)) ;
#41729 = DIRECTION('ref_axis',(-1.,0.,4.54747350886464E-14)) ;
#41730 = DIRECTION('center_axis',(0.,1.,0.)) ;
#41731 = DIRECTION('ref_axis',(-1.,0.,5.32907051820105E-14)) ;
#41732 = DIRECTION('center_axis',(-4.54195640846217E-14,1.66321791214601E-16,
-1.)) ;
#41733 = DIRECTION('ref_axis',(0.707106781186502,0.707106781186593,-3.1998874496344E-14)) ;
#41734 = DIRECTION('center_axis',(-1.66533453692965E-16,-1.,-1.66321791214593E-16)) ;
#41735 = DIRECTION('ref_axis',(-0.707106781186535,1.4966797377543E-19,0.70710678118656)) ;
#41736 = DIRECTION('center_axis',(0.,1.,0.)) ;
#41737 = DIRECTION('ref_axis',(-1.,0.,0.)) ;
#41738 = DIRECTION('',(-1.66533453692965E-16,-1.,-1.66321791214593E-16)) ;
#41739 = DIRECTION('center_axis',(-4.54195640846217E-14,1.66321791214601E-16,
-1.)) ;
#41740 = DIRECTION('ref_axis',(-1.,0.,4.54747350886464E-14)) ;
#41741 = DIRECTION('center_axis',(1.,2.84217094304056E-13,0.)) ;
#41742 = DIRECTION('ref_axis',(-2.84217094304056E-13,1.,0.)) ;
#41743 = DIRECTION('center_axis',(-4.54195640846217E-14,1.66321791214601E-16,
-1.)) ;
#41744 = DIRECTION('ref_axis',(0.707106781186644,-0.707106781186451,-3.22340890292043E-14)) ;
#41745 = DIRECTION('center_axis',(-1.,1.66533453692587E-16,4.54195640846217E-14)) ;
#41746 = DIRECTION('ref_axis',(3.22342386971791E-14,0.707106781186422,0.707106781186673)) ;
#41747 = DIRECTION('center_axis',(1.,0.,0.)) ;
#41748 = DIRECTION('ref_axis',(0.,1.,0.)) ;
#41749 = DIRECTION('',(-1.,1.66533453692587E-16,4.54195640846217E-14)) ;
#41750 = DIRECTION('center_axis',(-4.54195640846217E-14,1.66321791214601E-16,
-1.)) ;
#41751 = DIRECTION('ref_axis',(-1.,0.,4.54747350886464E-14)) ;
#41752 = DIRECTION('center_axis',(0.,-1.,0.)) ;
#41753 = DIRECTION('ref_axis',(1.,0.,-5.32907051820105E-14)) ;
#41754 = DIRECTION('center_axis',(-4.54195640846217E-14,1.66321791214601E-16,
-1.)) ;
#41755 = DIRECTION('ref_axis',(-0.707106781186593,-0.707106781186502,3.19988744963481E-14)) ;
#41756 = DIRECTION('center_axis',(8.32667268460786E-17,1.,1.66321791214597E-16)) ;
#41757 = DIRECTION('ref_axis',(0.707106781186522,-1.76485733627007E-16,0.707106781186573)) ;
#41758 = DIRECTION('center_axis',(0.,-1.,0.)) ;
#41759 = DIRECTION('ref_axis',(1.,0.,1.77635683940035E-14)) ;
#41760 = DIRECTION('center_axis',(-4.54195640846217E-14,1.66321791214601E-16,
-1.)) ;
#41761 = DIRECTION('ref_axis',(-1.,0.,4.54747350886464E-14)) ;
#41762 = DIRECTION('center_axis',(-4.54195640846217E-14,1.66321791214601E-16,
-1.)) ;
#41763 = DIRECTION('ref_axis',(-0.707106781186735,0.70710678118636,3.22340890292084E-14)) ;
#41764 = DIRECTION('center_axis',(-2.1716102378779E-15,3.83420712807775E-28,
1.)) ;
#41765 = DIRECTION('ref_axis',(0.707106781186643,-0.707106781186452,1.53556032529807E-15)) ;
#41766 = DIRECTION('',(-2.1716102378779E-15,3.83420712807775E-28,1.)) ;
#41767 = DIRECTION('center_axis',(2.1716102378779E-15,-3.83420712807775E-28,
-1.)) ;
#41768 = DIRECTION('ref_axis',(0.707106781186656,-0.707106781186439,1.5355603252981E-15)) ;
#41769 = DIRECTION('',(-2.1716102378779E-15,3.83322105194623E-28,1.)) ;
#41770 = DIRECTION('center_axis',(1.,-1.66533453692966E-16,2.1716102378779E-15)) ;
#41771 = DIRECTION('ref_axis',(-1.66533453692966E-16,-1.,3.82783884128008E-28)) ;
#41772 = DIRECTION('',(2.1716102378779E-15,-3.83815143260386E-28,-1.)) ;
#41773 = DIRECTION('',(-1.66533453692966E-16,-1.,3.83386399937507E-28)) ;
#41774 = DIRECTION('center_axis',(1.,-1.66533453692966E-16,2.1716102378779E-15)) ;
#41775 = DIRECTION('ref_axis',(-1.65331725969844E-15,-0.707106781186479,0.707106781186616)) ;
#41776 = DIRECTION('',(2.1716102378779E-15,-3.66854633798134E-28,-1.)) ;
#41777 = DIRECTION('',(-2.1716102378779E-15,3.66854633798134E-28,1.)) ;
#41778 = DIRECTION('center_axis',(1.,-1.66533453692966E-16,2.1716102378779E-15)) ;
#41779 = DIRECTION('ref_axis',(-1.41780339089703E-15,0.707106781186483,0.707106781186612)) ;
#41780 = DIRECTION('',(-1.66533453692966E-16,-1.,3.83386399937507E-28)) ;
#41781 = DIRECTION('center_axis',(2.1716102378779E-15,-3.83815143260386E-28,
-1.)) ;
#41782 = DIRECTION('ref_axis',(0.707106781186552,0.707106781186543,1.53556032529733E-15)) ;
#41783 = DIRECTION('',(2.1716102378779E-15,-3.83815143260386E-28,-1.)) ;
#41784 = DIRECTION('center_axis',(2.1716102378779E-15,-3.83815143260386E-28,
-1.)) ;
#41785 = DIRECTION('ref_axis',(0.707106781186582,0.707106781186513,1.5355603252974E-15)) ;
#41786 = DIRECTION('center_axis',(1.66533453692966E-16,1.,-3.83386399937507E-28)) ;
#41787 = DIRECTION('ref_axis',(2.1716102378779E-15,-3.83748045690496E-28,
-1.)) ;
#41788 = DIRECTION('',(2.17161023787787E-15,-3.83815143260382E-28,-1.)) ;
#41789 = DIRECTION('',(1.,-1.66533453692966E-16,2.1716102378779E-15)) ;
#41790 = DIRECTION('center_axis',(-1.66533453692587E-16,-1.,3.82991969484897E-28)) ;
#41791 = DIRECTION('ref_axis',(2.1716102378779E-15,-3.83353615237885E-28,
-1.)) ;
#41792 = DIRECTION('',(-1.,1.66533453692587E-16,-2.1716102378779E-15)) ;
#41793 = DIRECTION('',(-2.17161023787787E-15,3.83420712807771E-28,1.)) ;
#41794 = DIRECTION('center_axis',(2.17161023787787E-15,-3.83420712807771E-28,
-1.)) ;
#41795 = DIRECTION('ref_axis',(-0.707106781186552,-0.707106781186543,-1.53556032529731E-15)) ;
#41796 = DIRECTION('center_axis',(2.17161023787787E-15,-3.83420712807771E-28,
-1.)) ;
#41797 = DIRECTION('ref_axis',(-0.707106781186582,-0.707106781186513,-1.53556032529738E-15)) ;
#41798 = DIRECTION('center_axis',(-2.17161023787787E-15,3.83815143260382E-28,
1.)) ;
#41799 = DIRECTION('ref_axis',(-0.707106781186643,0.707106781186452,-1.53556032529805E-15)) ;
#41800 = DIRECTION('center_axis',(2.17161023787787E-15,-3.83815143260382E-28,
-1.)) ;
#41801 = DIRECTION('ref_axis',(-0.707106781186656,0.707106781186439,-1.53556032529808E-15)) ;
#41802 = DIRECTION('center_axis',(-1.66533453692587E-16,-1.,3.82991969484897E-28)) ;
#41803 = DIRECTION('ref_axis',(2.1716102378779E-15,-3.83353615237885E-28,
-1.)) ;
#41804 = DIRECTION('',(-1.,1.66533453692587E-16,-2.1716102378779E-15)) ;
#41805 = DIRECTION('',(-2.1716102378779E-15,3.83420712807775E-28,1.)) ;
#41806 = DIRECTION('center_axis',(2.1716102378779E-15,-3.83420712807775E-28,
-1.)) ;
#41807 = DIRECTION('ref_axis',(-0.707106781186452,-0.707106781186643,-1.53556032529712E-15)) ;
#41808 = DIRECTION('center_axis',(2.1716102378779E-15,-3.83420712807775E-28,
-1.)) ;
#41809 = DIRECTION('ref_axis',(-0.70710678118651,-0.707106781186585,-1.53556032529724E-15)) ;
#41810 = DIRECTION('',(2.1716102378779E-15,-3.83420712807775E-28,-1.)) ;
#41811 = DIRECTION('center_axis',(-2.1716102378779E-15,3.83815143260386E-28,
1.)) ;
#41812 = DIRECTION('ref_axis',(-0.707106781186643,0.707106781186452,-1.53556032529807E-15)) ;
#41813 = DIRECTION('',(-2.1716102378779E-15,3.83815143260386E-28,1.)) ;
#41814 = DIRECTION('center_axis',(2.1716102378779E-15,-3.83815143260386E-28,
-1.)) ;
#41815 = DIRECTION('ref_axis',(-0.707106781186656,0.707106781186439,-1.5355603252981E-15)) ;
#41816 = DIRECTION('center_axis',(-1.,1.66533453692966E-16,-2.1716102378779E-15)) ;
#41817 = DIRECTION('ref_axis',(1.66533453692966E-16,1.,-3.82783884128008E-28)) ;
#41818 = DIRECTION('',(1.66533453692966E-16,1.,-3.83386399937507E-28)) ;
#41819 = DIRECTION('center_axis',(2.1716102378779E-15,-3.83815143260386E-28,
-1.)) ;
#41820 = DIRECTION('ref_axis',(1.,-1.66533453692941E-16,2.1716102378779E-15)) ;
#41821 = DIRECTION('center_axis',(-2.1716102378779E-15,3.83815143260386E-28,
1.)) ;
#41822 = DIRECTION('ref_axis',(-1.,-7.33033736753389E-16,-2.1716102378779E-15)) ;
#41823 = DIRECTION('center_axis',(-2.1716102378779E-15,3.66854633798134E-28,
1.)) ;
#41824 = DIRECTION('ref_axis',(0.707106781186452,0.707106781186643,1.53556032529713E-15)) ;
#41825 = DIRECTION('center_axis',(1.88526971141291E-28,-2.90739654573716E-15,
-1.)) ;
#41826 = DIRECTION('ref_axis',(-1.35627620245787E-13,1.,-2.90739654573716E-15)) ;
#41827 = DIRECTION('center_axis',(1.,-1.66533453692587E-16,2.1716102378779E-15)) ;
#41828 = DIRECTION('ref_axis',(1.41780339089714E-15,-0.70710678118655,-0.707106781186545)) ;
#41829 = DIRECTION('center_axis',(1.,1.35627620245787E-13,-2.05796303467862E-28)) ;
#41830 = DIRECTION('ref_axis',(1.35627620245787E-13,-1.,2.90739654573716E-15)) ;
#41831 = DIRECTION('center_axis',(-1.,-1.35627620245747E-13,2.05796303467745E-28)) ;
#41832 = DIRECTION('ref_axis',(1.88526971141291E-28,-2.90739654573716E-15,
-1.)) ;
#41833 = DIRECTION('',(1.,-1.66533453692587E-16,2.1716102378779E-15)) ;
#41834 = DIRECTION('center_axis',(-1.,6.48092690624107E-15,-2.07369595641671E-28)) ;
#41835 = DIRECTION('ref_axis',(0.,-1.,0.)) ;
#41836 = DIRECTION('center_axis',(-1.,7.08071943160919E-13,-2.24717289282075E-27)) ;
#41837 = DIRECTION('ref_axis',(-1.88526971141296E-28,2.90739654573716E-15,
1.)) ;
#41838 = DIRECTION('center_axis',(6.48092690624107E-15,1.,-2.90739654573716E-15)) ;
#41839 = DIRECTION('ref_axis',(1.,-6.48092690624107E-15,2.07369595641671E-28)) ;
#41840 = DIRECTION('center_axis',(-1.66533453692966E-16,-1.,3.83386399937507E-28)) ;
#41841 = DIRECTION('ref_axis',(0.707106781186648,-1.17756934401E-16,-0.707106781186447)) ;
#41842 = DIRECTION('center_axis',(-6.48092690624107E-15,-1.,2.90739654573716E-15)) ;
#41843 = DIRECTION('ref_axis',(1.88526971141291E-28,-2.90739654573716E-15,
-1.)) ;
#41844 = DIRECTION('',(1.66533453692966E-16,1.,-3.83386399937507E-28)) ;
#41845 = DIRECTION('center_axis',(1.,-6.48092690624107E-15,2.07369595641671E-28)) ;
#41846 = DIRECTION('ref_axis',(0.,1.,0.)) ;
#41847 = DIRECTION('center_axis',(1.,-1.48589474058271E-13,-5.59482469102492E-13)) ;
#41848 = DIRECTION('ref_axis',(-1.48589474058269E-13,-1.,2.90739654573716E-15)) ;
#41849 = DIRECTION('center_axis',(6.48092690624107E-15,1.,-2.90739654573716E-15)) ;
#41850 = DIRECTION('ref_axis',(1.88526971141291E-28,-2.90739654573716E-15,
-1.)) ;
#41851 = DIRECTION('center_axis',(-1.,6.48092690624107E-15,-2.07369595641671E-28)) ;
#41852 = DIRECTION('ref_axis',(0.,-1.,0.)) ;
#41853 = DIRECTION('center_axis',(-1.,1.48589474058269E-13,-6.20535494751205E-28)) ;
#41854 = DIRECTION('ref_axis',(1.48589474058269E-13,1.,-2.90739654573716E-15)) ;
#41855 = DIRECTION('center_axis',(-6.48092690624107E-15,-1.,2.90739654573716E-15)) ;
#41856 = DIRECTION('ref_axis',(1.88526971141291E-28,-2.90739654573716E-15,
-1.)) ;
#41857 = DIRECTION('center_axis',(1.88526971141291E-28,-2.90739654573716E-15,
-1.)) ;
#41858 = DIRECTION('ref_axis',(1.,-6.48092690624108E-15,2.07369595641671E-28)) ;
#41859 = DIRECTION('center_axis',(2.1716102378779E-15,-3.66854633798134E-28,
-1.)) ;
#41860 = DIRECTION('ref_axis',(0.707106781186543,-0.707106781186552,1.53556032529784E-15)) ;
#41861 = DIRECTION('',(2.1716102378779E-15,-3.66854633798134E-28,-1.)) ;
#41862 = DIRECTION('center_axis',(-1.66533453692966E-16,-1.,3.83386399937507E-28)) ;
#41863 = DIRECTION('ref_axis',(0.707106781186648,-1.17756934401E-16,-0.707106781186447)) ;
#41864 = DIRECTION('center_axis',(6.48092690628146E-15,1.,-2.90739654573716E-15)) ;
#41865 = DIRECTION('ref_axis',(1.,-6.48092690628146E-15,2.07369595641789E-28)) ;
#41866 = DIRECTION('',(1.66533453692966E-16,1.,-3.83386399937507E-28)) ;
#41867 = DIRECTION('center_axis',(1.,-6.48092690624107E-15,2.07369595641671E-28)) ;
#41868 = DIRECTION('ref_axis',(0.,1.,0.)) ;
#41869 = DIRECTION('center_axis',(1.,-1.48589474058269E-13,6.20535494751205E-28)) ;
#41870 = DIRECTION('ref_axis',(-1.88526971141292E-28,2.90739654573716E-15,
1.)) ;
#41871 = DIRECTION('center_axis',(-6.48092690624107E-15,-1.,2.90739654573716E-15)) ;
#41872 = DIRECTION('ref_axis',(-1.,6.48092690624107E-15,-2.07369595641671E-28)) ;
#41873 = DIRECTION('center_axis',(8.32667268460789E-17,1.,-3.83780830390118E-28)) ;
#41874 = DIRECTION('ref_axis',(-0.707106781186447,5.88784671997906E-17,-0.707106781186648)) ;
#41875 = DIRECTION('center_axis',(6.48092690624107E-15,1.,-2.90739654573716E-15)) ;
#41876 = DIRECTION('ref_axis',(1.88526971141291E-28,-2.90739654573716E-15,
-1.)) ;
#41877 = DIRECTION('',(-8.32667268460789E-17,-1.,3.83780830390118E-28)) ;
#41878 = DIRECTION('center_axis',(-1.,3.33066907386739E-16,-2.1716102378779E-15)) ;
#41879 = DIRECTION('ref_axis',(-1.30004645649559E-15,0.70710678118655,0.707106781186545)) ;
#41880 = DIRECTION('',(-1.,3.33066907386739E-16,-2.1716102378779E-15)) ;
#41881 = DIRECTION('',(1.,-3.33066907386739E-16,2.1716102378779E-15)) ;
#41882 = DIRECTION('center_axis',(8.32667268460789E-17,1.,-3.83780830390118E-28)) ;
#41883 = DIRECTION('ref_axis',(-0.707106781186447,5.88784671997906E-17,-0.707106781186648)) ;
#41884 = DIRECTION('center_axis',(-6.48092690624107E-15,-1.,2.90739654573716E-15)) ;
#41885 = DIRECTION('ref_axis',(-1.,6.48092690624107E-15,-2.07369595641671E-28)) ;
#41886 = DIRECTION('',(-8.32667268460789E-17,-1.,3.83780830390118E-28)) ;
#41887 = DIRECTION('center_axis',(1.,-3.33066907386739E-16,2.1716102378779E-15)) ;
#41888 = DIRECTION('ref_axis',(-1.77107419409959E-15,-0.707106781186545,0.70710678118655)) ;
#41889 = DIRECTION('',(1.,-3.33066907386739E-16,2.1716102378779E-15)) ;
#41890 = DIRECTION('center_axis',(-0.81649658092765,0.408248290464166,0.408248290463711)) ;
#41891 = DIRECTION('ref_axis',(-0.577350269189702,-0.577350269189929,-0.577350269189247)) ;
#41892 = DIRECTION('center_axis',(-0.40824829046392,0.408248290464147,-0.816496580927556)) ;
#41893 = DIRECTION('ref_axis',(0.577350269189076,-0.577350269189986,-0.577350269189815)) ;
#41894 = DIRECTION('center_axis',(1.,-1.66533453692966E-16,2.1716102378779E-15)) ;
#41895 = DIRECTION('ref_axis',(1.65331725969831E-15,0.707106781186545,-0.70710678118655)) ;
#41896 = DIRECTION('center_axis',(1.,1.35627620245787E-13,-2.05796303467862E-28)) ;
#41897 = DIRECTION('ref_axis',(1.8852697114129E-28,-2.90739654573716E-15,
-1.)) ;
#41898 = DIRECTION('',(-1.,1.66533453692966E-16,-2.1716102378779E-15)) ;
#41899 = DIRECTION('center_axis',(-1.,-1.35627620245787E-13,2.05796303467862E-28)) ;
#41900 = DIRECTION('ref_axis',(-1.35627620245787E-13,1.,-2.90739654573716E-15)) ;
#41901 = DIRECTION('center_axis',(0.40824829046392,-0.408248290464147,-0.816496580927556)) ;
#41902 = DIRECTION('ref_axis',(-0.577350269189834,0.577350269189152,-0.577350269189891)) ;
#41903 = DIRECTION('center_axis',(-0.81649658092765,0.408248290464166,-0.408248290463711)) ;
#41904 = DIRECTION('ref_axis',(0.577350269189702,0.577350269189929,-0.577350269189247)) ;
#41905 = DIRECTION('center_axis',(-3.33066907386739E-16,-1.,3.66031460022645E-28)) ;
#41906 = DIRECTION('ref_axis',(-2.17161023787795E-15,3.66754751528624E-28,
1.)) ;
#41907 = DIRECTION('center_axis',(2.1716102378779E-15,-3.83815143260386E-28,
-1.)) ;
#41908 = DIRECTION('ref_axis',(1.,-1.66533453692941E-16,2.1716102378779E-15)) ;
#41909 = DIRECTION('center_axis',(2.1716102378779E-15,-3.83815143260386E-28,
-1.)) ;
#41910 = DIRECTION('ref_axis',(1.,-1.66533453692941E-16,2.1716102378779E-15)) ;
#41911 = DIRECTION('center_axis',(2.1716102378779E-15,-3.83815143260386E-28,
-1.)) ;
#41912 = DIRECTION('ref_axis',(1.,-1.66533453692941E-16,2.1716102378779E-15)) ;
#41913 = DIRECTION('',(-1.66533453692966E-16,-1.,3.83386399937507E-28)) ;
#41914 = DIRECTION('',(1.,-1.66533453692587E-16,2.1716102378779E-15)) ;
#41915 = DIRECTION('',(8.32667268460789E-17,1.,-3.83780830390118E-28)) ;
#41916 = DIRECTION('',(-1.,1.66533453692966E-16,-2.1716102378779E-15)) ;
#41917 = DIRECTION('center_axis',(-0.816496580927764,0.408248290464109,0.408248290463541)) ;
#41918 = DIRECTION('ref_axis',(-0.577350269189531,-0.577350269189986,-0.57735026918936)) ;
#41919 = DIRECTION('center_axis',(1.,1.35627620245787E-13,2.17161023787752E-15)) ;
#41920 = DIRECTION('ref_axis',(1.35627620245787E-13,-1.,2.90739654573778E-15)) ;
#41921 = DIRECTION('center_axis',(6.48092690624107E-15,1.,-2.90739654573747E-15)) ;
#41922 = DIRECTION('ref_axis',(2.17161023787792E-15,-2.90739654573748E-15,
-1.)) ;
#41923 = DIRECTION('center_axis',(0.40824829046392,-0.408248290464147,-0.816496580927556)) ;
#41924 = DIRECTION('ref_axis',(-0.577350269189986,0.577350269189076,-0.577350269189815)) ;
#41925 = DIRECTION('center_axis',(-6.48092690624107E-15,-1.,2.90739654573747E-15)) ;
#41926 = DIRECTION('ref_axis',(-1.,6.48092690624106E-15,-2.17161023787794E-15)) ;
#41927 = DIRECTION('center_axis',(1.,1.35627620245787E-13,2.17161023787752E-15)) ;
#41928 = DIRECTION('ref_axis',(2.17161023787791E-15,-2.90739654573749E-15,
-1.)) ;
#41929 = DIRECTION('center_axis',(1.66533453692966E-16,1.,-3.83386399937507E-28)) ;
#41930 = DIRECTION('ref_axis',(-0.707106781186596,1.17756934400449E-16,-0.707106781186499)) ;
#41931 = DIRECTION('center_axis',(1.,-1.66533453692966E-16,2.1716102378779E-15)) ;
#41932 = DIRECTION('ref_axis',(1.65331725969841E-15,0.707106781186495,-0.7071067811866)) ;
#41933 = DIRECTION('center_axis',(1.,1.35627620245787E-13,2.17161023787752E-15)) ;
#41934 = DIRECTION('ref_axis',(-1.35627620245787E-13,1.,-2.90739654573778E-15)) ;
#41935 = DIRECTION('center_axis',(-1.,1.66533453692587E-16,-2.1716102378779E-15)) ;
#41936 = DIRECTION('ref_axis',(1.41780339089726E-15,-0.707106781186499,-0.707106781186596)) ;
#41937 = DIRECTION('center_axis',(1.,1.35627620245787E-13,2.17161023787752E-15)) ;
#41938 = DIRECTION('ref_axis',(2.17161023787792E-15,-2.90739654573749E-15,
-1.)) ;
#41939 = DIRECTION('center_axis',(-8.32667268460789E-17,-1.,3.83780830390118E-28)) ;
#41940 = DIRECTION('ref_axis',(0.707106781186599,-5.8878467200346E-17,-0.707106781186496)) ;
#41941 = DIRECTION('center_axis',(-6.48092690624107E-15,-1.,2.90739654573747E-15)) ;
#41942 = DIRECTION('ref_axis',(1.,-6.48092690624106E-15,2.17161023787794E-15)) ;
#41943 = DIRECTION('center_axis',(6.48092690624107E-15,1.,-2.90739654573747E-15)) ;
#41944 = DIRECTION('ref_axis',(2.17161023787792E-15,-2.90739654573748E-15,
-1.)) ;
#41945 = DIRECTION('center_axis',(-0.408248290463939,0.408248290464166,-0.816496580927537)) ;
#41946 = DIRECTION('ref_axis',(0.577350269189076,-0.577350269189986,-0.577350269189815)) ;
#41947 = DIRECTION('center_axis',(0.408248290463948,-0.816496580927442,-0.408248290464346)) ;
#41948 = DIRECTION('ref_axis',(0.577350269189304,0.577350269189986,-0.577350269189588)) ;
#41949 = DIRECTION('center_axis',(-2.1716102378779E-15,3.66854633798134E-28,
1.)) ;
#41950 = DIRECTION('ref_axis',(0.707106781186452,0.707106781186643,1.53556032529713E-15)) ;
#41951 = DIRECTION('center_axis',(1.88526971141291E-28,-2.90739654573716E-15,
-1.)) ;
#41952 = DIRECTION('ref_axis',(-1.35627620245787E-13,1.,-2.90739654573716E-15)) ;
#41953 = DIRECTION('center_axis',(1.,-1.66533453692587E-16,2.1716102378779E-15)) ;
#41954 = DIRECTION('ref_axis',(1.41780339089714E-15,-0.70710678118655,-0.707106781186545)) ;
#41955 = DIRECTION('center_axis',(1.,1.35627620245787E-13,-2.05796303467862E-28)) ;
#41956 = DIRECTION('ref_axis',(1.35627620245787E-13,-1.,2.90739654573716E-15)) ;
#41957 = DIRECTION('',(-1.,1.66533453692587E-16,-2.1716102378779E-15)) ;
#41958 = DIRECTION('center_axis',(-1.,-1.35627620245747E-13,2.05796303467745E-28)) ;
#41959 = DIRECTION('ref_axis',(1.88526971141291E-28,-2.90739654573716E-15,
-1.)) ;
#41960 = DIRECTION('',(1.,-1.66533453692587E-16,2.1716102378779E-15)) ;
#41961 = DIRECTION('center_axis',(-1.,6.48092690624107E-15,-2.07369595641671E-28)) ;
#41962 = DIRECTION('ref_axis',(0.,-1.,0.)) ;
#41963 = DIRECTION('center_axis',(-1.,7.08071943160919E-13,-2.24717289282075E-27)) ;
#41964 = DIRECTION('ref_axis',(-1.88526971141296E-28,2.90739654573716E-15,
1.)) ;
#41965 = DIRECTION('center_axis',(6.48092690624107E-15,1.,-2.90739654573716E-15)) ;
#41966 = DIRECTION('ref_axis',(1.,-6.48092690624107E-15,2.07369595641671E-28)) ;
#41967 = DIRECTION('center_axis',(-1.66533453692966E-16,-1.,3.83386399937507E-28)) ;
#41968 = DIRECTION('ref_axis',(0.707106781186648,-1.17756934401E-16,-0.707106781186447)) ;
#41969 = DIRECTION('center_axis',(-6.48092690624107E-15,-1.,2.90739654573716E-15)) ;
#41970 = DIRECTION('ref_axis',(1.88526971141291E-28,-2.90739654573716E-15,
-1.)) ;
#41971 = DIRECTION('',(1.66533453692966E-16,1.,-3.83386399937507E-28)) ;
#41972 = DIRECTION('center_axis',(1.,-6.48092690624107E-15,2.07369595641671E-28)) ;
#41973 = DIRECTION('ref_axis',(0.,1.,0.)) ;
#41974 = DIRECTION('center_axis',(1.,-1.48589474058271E-13,-5.59482469102492E-13)) ;
#41975 = DIRECTION('ref_axis',(-1.48589474058269E-13,-1.,2.90739654573716E-15)) ;
#41976 = DIRECTION('center_axis',(6.48092690624107E-15,1.,-2.90739654573716E-15)) ;
#41977 = DIRECTION('ref_axis',(1.88526971141291E-28,-2.90739654573716E-15,
-1.)) ;
#41978 = DIRECTION('center_axis',(-1.,6.48092690624107E-15,-2.07369595641671E-28)) ;
#41979 = DIRECTION('ref_axis',(0.,-1.,0.)) ;
#41980 = DIRECTION('center_axis',(-1.,1.48589474058269E-13,-6.20535494751205E-28)) ;
#41981 = DIRECTION('ref_axis',(1.48589474058269E-13,1.,-2.90739654573716E-15)) ;
#41982 = DIRECTION('center_axis',(-6.48092690624107E-15,-1.,2.90739654573716E-15)) ;
#41983 = DIRECTION('ref_axis',(1.88526971141291E-28,-2.90739654573716E-15,
-1.)) ;
#41984 = DIRECTION('center_axis',(1.88526971141291E-28,-2.90739654573716E-15,
-1.)) ;
#41985 = DIRECTION('ref_axis',(1.,-6.48092690624108E-15,2.07369595641671E-28)) ;
#41986 = DIRECTION('center_axis',(2.1716102378779E-15,-3.66854633798134E-28,
-1.)) ;
#41987 = DIRECTION('ref_axis',(0.707106781186543,-0.707106781186552,1.53556032529784E-15)) ;
#41988 = DIRECTION('',(2.1716102378779E-15,-3.66854633798134E-28,-1.)) ;
#41989 = DIRECTION('center_axis',(-1.66533453692966E-16,-1.,3.83386399937507E-28)) ;
#41990 = DIRECTION('ref_axis',(0.707106781186648,-1.17756934401E-16,-0.707106781186447)) ;
#41991 = DIRECTION('center_axis',(6.48092690628146E-15,1.,-2.90739654573716E-15)) ;
#41992 = DIRECTION('ref_axis',(1.,-6.48092690628146E-15,2.07369595641789E-28)) ;
#41993 = DIRECTION('',(1.66533453692966E-16,1.,-3.83386399937507E-28)) ;
#41994 = DIRECTION('center_axis',(1.,-6.48092690624107E-15,2.07369595641671E-28)) ;
#41995 = DIRECTION('ref_axis',(0.,1.,0.)) ;
#41996 = DIRECTION('center_axis',(1.,-1.48589474058269E-13,6.20535494751205E-28)) ;
#41997 = DIRECTION('ref_axis',(-1.88526971141292E-28,2.90739654573716E-15,
1.)) ;
#41998 = DIRECTION('center_axis',(-6.48092690624107E-15,-1.,2.90739654573716E-15)) ;
#41999 = DIRECTION('ref_axis',(-1.,6.48092690624107E-15,-2.07369595641671E-28)) ;
#42000 = DIRECTION('center_axis',(8.32667268460789E-17,1.,-3.83780830390118E-28)) ;
#42001 = DIRECTION('ref_axis',(-0.707106781186447,5.88784671997906E-17,-0.707106781186648)) ;
#42002 = DIRECTION('center_axis',(6.48092690624107E-15,1.,-2.90739654573716E-15)) ;
#42003 = DIRECTION('ref_axis',(1.88526971141291E-28,-2.90739654573716E-15,
-1.)) ;
#42004 = DIRECTION('',(-8.32667268460789E-17,-1.,3.83780830390118E-28)) ;
#42005 = DIRECTION('center_axis',(-1.,3.33066907386739E-16,-2.1716102378779E-15)) ;
#42006 = DIRECTION('ref_axis',(-1.30004645649559E-15,0.70710678118655,0.707106781186545)) ;
#42007 = DIRECTION('',(-1.,3.33066907386739E-16,-2.1716102378779E-15)) ;
#42008 = DIRECTION('',(1.,-3.33066907386739E-16,2.1716102378779E-15)) ;
#42009 = DIRECTION('center_axis',(8.32667268460789E-17,1.,-3.83780830390118E-28)) ;
#42010 = DIRECTION('ref_axis',(-0.707106781186447,5.88784671997906E-17,-0.707106781186648)) ;
#42011 = DIRECTION('center_axis',(-6.48092690624107E-15,-1.,2.90739654573716E-15)) ;
#42012 = DIRECTION('ref_axis',(-1.,6.48092690624107E-15,-2.07369595641671E-28)) ;
#42013 = DIRECTION('',(-8.32667268460789E-17,-1.,3.83780830390118E-28)) ;
#42014 = DIRECTION('center_axis',(1.,-3.33066907386739E-16,2.1716102378779E-15)) ;
#42015 = DIRECTION('ref_axis',(-1.77107419409959E-15,-0.707106781186545,0.70710678118655)) ;
#42016 = DIRECTION('',(1.,-3.33066907386739E-16,2.1716102378779E-15)) ;
#42017 = DIRECTION('center_axis',(-0.81649658092765,0.408248290464166,0.408248290463711)) ;
#42018 = DIRECTION('ref_axis',(-0.577350269189702,-0.577350269189929,-0.577350269189247)) ;
#42019 = DIRECTION('center_axis',(2.17161023787787E-15,-3.83420712807771E-28,
-1.)) ;
#42020 = DIRECTION('ref_axis',(-0.707106781186582,-0.707106781186513,-1.53556032529738E-15)) ;
#42021 = DIRECTION('center_axis',(-0.40824829046392,0.408248290464147,-0.816496580927556)) ;
#42022 = DIRECTION('ref_axis',(0.577350269189076,-0.577350269189986,-0.577350269189815)) ;
#42023 = DIRECTION('center_axis',(1.,-1.66533453692966E-16,2.1716102378779E-15)) ;
#42024 = DIRECTION('ref_axis',(1.65331725969831E-15,0.707106781186545,-0.70710678118655)) ;
#42025 = DIRECTION('center_axis',(1.,1.35627620245787E-13,-2.05796303467862E-28)) ;
#42026 = DIRECTION('ref_axis',(1.8852697114129E-28,-2.90739654573716E-15,
-1.)) ;
#42027 = DIRECTION('',(-1.,1.66533453692966E-16,-2.1716102378779E-15)) ;
#42028 = DIRECTION('center_axis',(-1.,-1.35627620245787E-13,2.05796303467862E-28)) ;
#42029 = DIRECTION('ref_axis',(-1.35627620245787E-13,1.,-2.90739654573716E-15)) ;
#42030 = DIRECTION('center_axis',(0.40824829046392,-0.408248290464147,-0.816496580927556)) ;
#42031 = DIRECTION('ref_axis',(-0.577350269189834,0.577350269189152,-0.577350269189891)) ;
#42032 = DIRECTION('center_axis',(2.17161023787787E-15,-3.83815143260382E-28,
-1.)) ;
#42033 = DIRECTION('ref_axis',(-0.707106781186656,0.707106781186439,-1.53556032529808E-15)) ;
#42034 = DIRECTION('center_axis',(-0.81649658092765,0.408248290464166,-0.408248290463711)) ;
#42035 = DIRECTION('ref_axis',(0.577350269189702,0.577350269189929,-0.577350269189247)) ;
#42036 = DIRECTION('center_axis',(-3.33066907386739E-16,-1.,3.66031460022645E-28)) ;
#42037 = DIRECTION('ref_axis',(-2.17161023787795E-15,3.66754751528624E-28,
1.)) ;
#42038 = DIRECTION('center_axis',(2.1716102378779E-15,-3.83815143260386E-28,
-1.)) ;
#42039 = DIRECTION('ref_axis',(1.,-1.66533453692941E-16,2.1716102378779E-15)) ;
#42040 = DIRECTION('center_axis',(2.1716102378779E-15,-3.83815143260386E-28,
-1.)) ;
#42041 = DIRECTION('ref_axis',(1.,-1.66533453692941E-16,2.1716102378779E-15)) ;
#42042 = DIRECTION('center_axis',(2.1716102378779E-15,-3.83815143260386E-28,
-1.)) ;
#42043 = DIRECTION('ref_axis',(1.,-1.66533453692941E-16,2.1716102378779E-15)) ;
#42044 = DIRECTION('',(-1.66533453692966E-16,-1.,3.83386399937507E-28)) ;
#42045 = DIRECTION('',(1.,-1.66533453692587E-16,2.1716102378779E-15)) ;
#42046 = DIRECTION('',(8.32667268460789E-17,1.,-3.83780830390118E-28)) ;
#42047 = DIRECTION('',(-1.,1.66533453692966E-16,-2.1716102378779E-15)) ;
#42048 = DIRECTION('center_axis',(-0.816496580927764,0.408248290464109,0.408248290463541)) ;
#42049 = DIRECTION('ref_axis',(-0.577350269189531,-0.577350269189986,-0.57735026918936)) ;
#42050 = DIRECTION('center_axis',(1.,1.35627620245787E-13,2.17161023787752E-15)) ;
#42051 = DIRECTION('ref_axis',(1.35627620245787E-13,-1.,2.90739654573778E-15)) ;
#42052 = DIRECTION('center_axis',(6.48092690624107E-15,1.,-2.90739654573747E-15)) ;
#42053 = DIRECTION('ref_axis',(2.17161023787792E-15,-2.90739654573748E-15,
-1.)) ;
#42054 = DIRECTION('center_axis',(2.1716102378779E-15,-3.83420712807775E-28,
-1.)) ;
#42055 = DIRECTION('ref_axis',(-0.70710678118651,-0.707106781186585,-1.53556032529724E-15)) ;
#42056 = DIRECTION('center_axis',(0.40824829046392,-0.408248290464147,-0.816496580927556)) ;
#42057 = DIRECTION('ref_axis',(-0.577350269189986,0.577350269189076,-0.577350269189815)) ;
#42058 = DIRECTION('center_axis',(-6.48092690624107E-15,-1.,2.90739654573747E-15)) ;
#42059 = DIRECTION('ref_axis',(-1.,6.48092690624106E-15,-2.17161023787794E-15)) ;
#42060 = DIRECTION('center_axis',(1.,1.35627620245787E-13,2.17161023787752E-15)) ;
#42061 = DIRECTION('ref_axis',(2.17161023787791E-15,-2.90739654573749E-15,
-1.)) ;
#42062 = DIRECTION('center_axis',(2.1716102378779E-15,-3.83815143260386E-28,
-1.)) ;
#42063 = DIRECTION('ref_axis',(-0.707106781186656,0.707106781186439,-1.5355603252981E-15)) ;
#42064 = DIRECTION('center_axis',(1.66533453692966E-16,1.,-3.83386399937507E-28)) ;
#42065 = DIRECTION('ref_axis',(-0.707106781186596,1.17756934400449E-16,-0.707106781186499)) ;
#42066 = DIRECTION('',(1.66533453692966E-16,1.,-3.83386399937507E-28)) ;
#42067 = DIRECTION('center_axis',(1.,-1.66533453692966E-16,2.1716102378779E-15)) ;
#42068 = DIRECTION('ref_axis',(1.65331725969841E-15,0.707106781186495,-0.7071067811866)) ;
#42069 = DIRECTION('center_axis',(1.,1.35627620245787E-13,2.17161023787752E-15)) ;
#42070 = DIRECTION('ref_axis',(-1.35627620245787E-13,1.,-2.90739654573778E-15)) ;
#42071 = DIRECTION('center_axis',(-1.,1.66533453692587E-16,-2.1716102378779E-15)) ;
#42072 = DIRECTION('ref_axis',(1.41780339089726E-15,-0.707106781186499,-0.707106781186596)) ;
#42073 = DIRECTION('',(-1.,1.66533453692587E-16,-2.1716102378779E-15)) ;
#42074 = DIRECTION('center_axis',(1.,1.35627620245787E-13,2.17161023787752E-15)) ;
#42075 = DIRECTION('ref_axis',(2.17161023787792E-15,-2.90739654573749E-15,
-1.)) ;
#42076 = DIRECTION('center_axis',(-8.32667268460789E-17,-1.,3.83780830390118E-28)) ;
#42077 = DIRECTION('ref_axis',(0.707106781186599,-5.8878467200346E-17,-0.707106781186496)) ;
#42078 = DIRECTION('center_axis',(-6.48092690624107E-15,-1.,2.90739654573747E-15)) ;
#42079 = DIRECTION('ref_axis',(1.,-6.48092690624106E-15,2.17161023787794E-15)) ;
#42080 = DIRECTION('center_axis',(6.48092690624107E-15,1.,-2.90739654573747E-15)) ;
#42081 = DIRECTION('ref_axis',(2.17161023787792E-15,-2.90739654573748E-15,
-1.)) ;
#42082 = DIRECTION('center_axis',(-0.408248290463939,0.408248290464166,-0.816496580927537)) ;
#42083 = DIRECTION('ref_axis',(0.577350269189076,-0.577350269189986,-0.577350269189815)) ;
#42084 = DIRECTION('center_axis',(0.408248290463948,-0.816496580927442,-0.408248290464346)) ;
#42085 = DIRECTION('ref_axis',(0.577350269189304,0.577350269189986,-0.577350269189588)) ;
#42086 = DIRECTION('center_axis',(-2.1716102378779E-15,3.66854633798134E-28,
1.)) ;
#42087 = DIRECTION('ref_axis',(0.707106781186452,0.707106781186643,1.53556032529713E-15)) ;
#42088 = DIRECTION('center_axis',(1.88526971141291E-28,-2.90739654573716E-15,
-1.)) ;
#42089 = DIRECTION('ref_axis',(-1.35627620245787E-13,1.,-2.90739654573716E-15)) ;
#42090 = DIRECTION('center_axis',(1.,-1.66533453692587E-16,2.1716102378779E-15)) ;
#42091 = DIRECTION('ref_axis',(1.41780339089714E-15,-0.70710678118655,-0.707106781186545)) ;
#42092 = DIRECTION('center_axis',(1.,1.35627620245787E-13,-2.05796303467862E-28)) ;
#42093 = DIRECTION('ref_axis',(1.35627620245787E-13,-1.,2.90739654573716E-15)) ;
#42094 = DIRECTION('',(-1.,1.66533453692587E-16,-2.1716102378779E-15)) ;
#42095 = DIRECTION('center_axis',(-1.,-1.35627620245747E-13,2.05796303467745E-28)) ;
#42096 = DIRECTION('ref_axis',(1.88526971141291E-28,-2.90739654573716E-15,
-1.)) ;
#42097 = DIRECTION('',(1.,-1.66533453692587E-16,2.1716102378779E-15)) ;
#42098 = DIRECTION('center_axis',(-1.,6.48092690624107E-15,-2.07369595641671E-28)) ;
#42099 = DIRECTION('ref_axis',(0.,-1.,0.)) ;
#42100 = DIRECTION('center_axis',(-1.,7.08071943160919E-13,-2.24717289282075E-27)) ;
#42101 = DIRECTION('ref_axis',(-1.88526971141296E-28,2.90739654573716E-15,
1.)) ;
#42102 = DIRECTION('center_axis',(6.48092690624107E-15,1.,-2.90739654573716E-15)) ;
#42103 = DIRECTION('ref_axis',(1.,-6.48092690624107E-15,2.07369595641671E-28)) ;
#42104 = DIRECTION('center_axis',(-1.66533453692966E-16,-1.,3.83386399937507E-28)) ;
#42105 = DIRECTION('ref_axis',(0.707106781186648,-1.17756934401E-16,-0.707106781186447)) ;
#42106 = DIRECTION('center_axis',(-6.48092690624107E-15,-1.,2.90739654573716E-15)) ;
#42107 = DIRECTION('ref_axis',(1.88526971141291E-28,-2.90739654573716E-15,
-1.)) ;
#42108 = DIRECTION('',(1.66533453692966E-16,1.,-3.83386399937507E-28)) ;
#42109 = DIRECTION('center_axis',(1.,-6.48092690624107E-15,2.07369595641671E-28)) ;
#42110 = DIRECTION('ref_axis',(0.,1.,0.)) ;
#42111 = DIRECTION('center_axis',(1.,-1.48589474058271E-13,-5.59482469102492E-13)) ;
#42112 = DIRECTION('ref_axis',(-1.48589474058269E-13,-1.,2.90739654573716E-15)) ;
#42113 = DIRECTION('center_axis',(6.48092690624107E-15,1.,-2.90739654573716E-15)) ;
#42114 = DIRECTION('ref_axis',(1.88526971141291E-28,-2.90739654573716E-15,
-1.)) ;
#42115 = DIRECTION('center_axis',(-1.,6.48092690624107E-15,-2.07369595641671E-28)) ;
#42116 = DIRECTION('ref_axis',(0.,-1.,0.)) ;
#42117 = DIRECTION('center_axis',(-1.,1.48589474058269E-13,-6.20535494751205E-28)) ;
#42118 = DIRECTION('ref_axis',(1.48589474058269E-13,1.,-2.90739654573716E-15)) ;
#42119 = DIRECTION('center_axis',(-6.48092690624107E-15,-1.,2.90739654573716E-15)) ;
#42120 = DIRECTION('ref_axis',(1.88526971141291E-28,-2.90739654573716E-15,
-1.)) ;
#42121 = DIRECTION('center_axis',(1.88526971141291E-28,-2.90739654573716E-15,
-1.)) ;
#42122 = DIRECTION('ref_axis',(1.,-6.48092690624108E-15,2.07369595641671E-28)) ;
#42123 = DIRECTION('center_axis',(2.1716102378779E-15,-3.66854633798134E-28,
-1.)) ;
#42124 = DIRECTION('ref_axis',(0.707106781186543,-0.707106781186552,1.53556032529784E-15)) ;
#42125 = DIRECTION('',(2.1716102378779E-15,-3.66854633798134E-28,-1.)) ;
#42126 = DIRECTION('center_axis',(-1.66533453692966E-16,-1.,3.83386399937507E-28)) ;
#42127 = DIRECTION('ref_axis',(0.707106781186648,-1.17756934401E-16,-0.707106781186447)) ;
#42128 = DIRECTION('center_axis',(6.48092690628146E-15,1.,-2.90739654573716E-15)) ;
#42129 = DIRECTION('ref_axis',(1.,-6.48092690628146E-15,2.07369595641789E-28)) ;
#42130 = DIRECTION('',(1.66533453692966E-16,1.,-3.83386399937507E-28)) ;
#42131 = DIRECTION('center_axis',(1.,-6.48092690624107E-15,2.07369595641671E-28)) ;
#42132 = DIRECTION('ref_axis',(0.,1.,0.)) ;
#42133 = DIRECTION('center_axis',(1.,-1.48589474058269E-13,6.20535494751205E-28)) ;
#42134 = DIRECTION('ref_axis',(-1.88526971141292E-28,2.90739654573716E-15,
1.)) ;
#42135 = DIRECTION('center_axis',(-6.48092690624107E-15,-1.,2.90739654573716E-15)) ;
#42136 = DIRECTION('ref_axis',(-1.,6.48092690624107E-15,-2.07369595641671E-28)) ;
#42137 = DIRECTION('center_axis',(8.32667268460789E-17,1.,-3.83780830390118E-28)) ;
#42138 = DIRECTION('ref_axis',(-0.707106781186447,5.88784671997906E-17,-0.707106781186648)) ;
#42139 = DIRECTION('center_axis',(6.48092690624107E-15,1.,-2.90739654573716E-15)) ;
#42140 = DIRECTION('ref_axis',(1.88526971141291E-28,-2.90739654573716E-15,
-1.)) ;
#42141 = DIRECTION('',(-8.32667268460789E-17,-1.,3.83780830390118E-28)) ;
#42142 = DIRECTION('center_axis',(-1.,3.33066907386739E-16,-2.1716102378779E-15)) ;
#42143 = DIRECTION('ref_axis',(-1.30004645649559E-15,0.70710678118655,0.707106781186545)) ;
#42144 = DIRECTION('',(-1.,3.33066907386739E-16,-2.1716102378779E-15)) ;
#42145 = DIRECTION('',(1.,-3.33066907386739E-16,2.1716102378779E-15)) ;
#42146 = DIRECTION('center_axis',(8.32667268460789E-17,1.,-3.83780830390118E-28)) ;
#42147 = DIRECTION('ref_axis',(-0.707106781186447,5.88784671997906E-17,-0.707106781186648)) ;
#42148 = DIRECTION('center_axis',(-6.48092690624107E-15,-1.,2.90739654573716E-15)) ;
#42149 = DIRECTION('ref_axis',(-1.,6.48092690624107E-15,-2.07369595641671E-28)) ;
#42150 = DIRECTION('',(-8.32667268460789E-17,-1.,3.83780830390118E-28)) ;
#42151 = DIRECTION('center_axis',(1.,-3.33066907386739E-16,2.1716102378779E-15)) ;
#42152 = DIRECTION('ref_axis',(-1.77107419409959E-15,-0.707106781186545,0.70710678118655)) ;
#42153 = DIRECTION('',(1.,-3.33066907386739E-16,2.1716102378779E-15)) ;
#42154 = DIRECTION('center_axis',(-0.81649658092765,0.408248290464166,0.408248290463711)) ;
#42155 = DIRECTION('ref_axis',(-0.577350269189702,-0.577350269189929,-0.577350269189247)) ;
#42156 = DIRECTION('center_axis',(2.17161023787787E-15,-3.83420712807771E-28,
-1.)) ;
#42157 = DIRECTION('ref_axis',(-0.707106781186582,-0.707106781186513,-1.53556032529738E-15)) ;
#42158 = DIRECTION('center_axis',(-0.40824829046392,0.408248290464147,-0.816496580927556)) ;
#42159 = DIRECTION('ref_axis',(0.577350269189076,-0.577350269189986,-0.577350269189815)) ;
#42160 = DIRECTION('center_axis',(1.,-1.66533453692966E-16,2.1716102378779E-15)) ;
#42161 = DIRECTION('ref_axis',(1.65331725969831E-15,0.707106781186545,-0.70710678118655)) ;
#42162 = DIRECTION('center_axis',(1.,1.35627620245787E-13,-2.05796303467862E-28)) ;
#42163 = DIRECTION('ref_axis',(1.8852697114129E-28,-2.90739654573716E-15,
-1.)) ;
#42164 = DIRECTION('',(-1.,1.66533453692966E-16,-2.1716102378779E-15)) ;
#42165 = DIRECTION('center_axis',(-1.,-1.35627620245787E-13,2.05796303467862E-28)) ;
#42166 = DIRECTION('ref_axis',(-1.35627620245787E-13,1.,-2.90739654573716E-15)) ;
#42167 = DIRECTION('center_axis',(0.40824829046392,-0.408248290464147,-0.816496580927556)) ;
#42168 = DIRECTION('ref_axis',(-0.577350269189834,0.577350269189152,-0.577350269189891)) ;
#42169 = DIRECTION('center_axis',(2.17161023787787E-15,-3.83815143260382E-28,
-1.)) ;
#42170 = DIRECTION('ref_axis',(-0.707106781186656,0.707106781186439,-1.53556032529808E-15)) ;
#42171 = DIRECTION('center_axis',(-0.81649658092765,0.408248290464166,-0.408248290463711)) ;
#42172 = DIRECTION('ref_axis',(0.577350269189702,0.577350269189929,-0.577350269189247)) ;
#42173 = DIRECTION('center_axis',(-3.33066907386739E-16,-1.,3.66031460022645E-28)) ;
#42174 = DIRECTION('ref_axis',(-2.17161023787795E-15,3.66754751528624E-28,
1.)) ;
#42175 = DIRECTION('center_axis',(2.1716102378779E-15,-3.83815143260386E-28,
-1.)) ;
#42176 = DIRECTION('ref_axis',(1.,-1.66533453692941E-16,2.1716102378779E-15)) ;
#42177 = DIRECTION('center_axis',(2.1716102378779E-15,-3.83815143260386E-28,
-1.)) ;
#42178 = DIRECTION('ref_axis',(1.,-1.66533453692941E-16,2.1716102378779E-15)) ;
#42179 = DIRECTION('center_axis',(2.1716102378779E-15,-3.83815143260386E-28,
-1.)) ;
#42180 = DIRECTION('ref_axis',(1.,-1.66533453692941E-16,2.1716102378779E-15)) ;
#42181 = DIRECTION('',(-1.66533453692966E-16,-1.,3.83386399937507E-28)) ;
#42182 = DIRECTION('',(1.,-1.66533453692587E-16,2.1716102378779E-15)) ;
#42183 = DIRECTION('',(8.32667268460789E-17,1.,-3.83780830390118E-28)) ;
#42184 = DIRECTION('',(-1.,1.66533453692966E-16,-2.1716102378779E-15)) ;
#42185 = DIRECTION('center_axis',(-0.816496580927764,0.408248290464109,0.408248290463541)) ;
#42186 = DIRECTION('ref_axis',(-0.577350269189531,-0.577350269189986,-0.57735026918936)) ;
#42187 = DIRECTION('center_axis',(1.,1.35627620245787E-13,2.17161023787752E-15)) ;
#42188 = DIRECTION('ref_axis',(1.35627620245787E-13,-1.,2.90739654573778E-15)) ;
#42189 = DIRECTION('center_axis',(6.48092690624107E-15,1.,-2.90739654573747E-15)) ;
#42190 = DIRECTION('ref_axis',(2.17161023787792E-15,-2.90739654573748E-15,
-1.)) ;
#42191 = DIRECTION('center_axis',(2.1716102378779E-15,-3.83420712807775E-28,
-1.)) ;
#42192 = DIRECTION('ref_axis',(-0.70710678118651,-0.707106781186585,-1.53556032529724E-15)) ;
#42193 = DIRECTION('center_axis',(0.40824829046392,-0.408248290464147,-0.816496580927556)) ;
#42194 = DIRECTION('ref_axis',(-0.577350269189986,0.577350269189076,-0.577350269189815)) ;
#42195 = DIRECTION('center_axis',(-6.48092690624107E-15,-1.,2.90739654573747E-15)) ;
#42196 = DIRECTION('ref_axis',(-1.,6.48092690624106E-15,-2.17161023787794E-15)) ;
#42197 = DIRECTION('center_axis',(1.,1.35627620245787E-13,2.17161023787752E-15)) ;
#42198 = DIRECTION('ref_axis',(2.17161023787791E-15,-2.90739654573749E-15,
-1.)) ;
#42199 = DIRECTION('center_axis',(2.1716102378779E-15,-3.83815143260386E-28,
-1.)) ;
#42200 = DIRECTION('ref_axis',(-0.707106781186656,0.707106781186439,-1.5355603252981E-15)) ;
#42201 = DIRECTION('center_axis',(1.66533453692966E-16,1.,-3.83386399937507E-28)) ;
#42202 = DIRECTION('ref_axis',(-0.707106781186596,1.17756934400449E-16,-0.707106781186499)) ;
#42203 = DIRECTION('',(1.66533453692966E-16,1.,-3.83386399937507E-28)) ;
#42204 = DIRECTION('center_axis',(1.,-1.66533453692966E-16,2.1716102378779E-15)) ;
#42205 = DIRECTION('ref_axis',(1.65331725969841E-15,0.707106781186495,-0.7071067811866)) ;
#42206 = DIRECTION('center_axis',(1.,1.35627620245787E-13,2.17161023787752E-15)) ;
#42207 = DIRECTION('ref_axis',(-1.35627620245787E-13,1.,-2.90739654573778E-15)) ;
#42208 = DIRECTION('center_axis',(-1.,1.66533453692587E-16,-2.1716102378779E-15)) ;
#42209 = DIRECTION('ref_axis',(1.41780339089726E-15,-0.707106781186499,-0.707106781186596)) ;
#42210 = DIRECTION('',(-1.,1.66533453692587E-16,-2.1716102378779E-15)) ;
#42211 = DIRECTION('center_axis',(1.,1.35627620245787E-13,2.17161023787752E-15)) ;
#42212 = DIRECTION('ref_axis',(2.17161023787792E-15,-2.90739654573749E-15,
-1.)) ;
#42213 = DIRECTION('center_axis',(-8.32667268460789E-17,-1.,3.83780830390118E-28)) ;
#42214 = DIRECTION('ref_axis',(0.707106781186599,-5.8878467200346E-17,-0.707106781186496)) ;
#42215 = DIRECTION('center_axis',(-6.48092690624107E-15,-1.,2.90739654573747E-15)) ;
#42216 = DIRECTION('ref_axis',(1.,-6.48092690624106E-15,2.17161023787794E-15)) ;
#42217 = DIRECTION('center_axis',(6.48092690624107E-15,1.,-2.90739654573747E-15)) ;
#42218 = DIRECTION('ref_axis',(2.17161023787792E-15,-2.90739654573748E-15,
-1.)) ;
#42219 = DIRECTION('center_axis',(-0.408248290463939,0.408248290464166,-0.816496580927537)) ;
#42220 = DIRECTION('ref_axis',(0.577350269189076,-0.577350269189986,-0.577350269189815)) ;
#42221 = DIRECTION('center_axis',(0.408248290463948,-0.816496580927442,-0.408248290464346)) ;
#42222 = DIRECTION('ref_axis',(0.577350269189304,0.577350269189986,-0.577350269189588)) ;
#42223 = DIRECTION('center_axis',(-2.1716102378779E-15,3.66854633798134E-28,
1.)) ;
#42224 = DIRECTION('ref_axis',(0.707106781186452,0.707106781186643,1.53556032529713E-15)) ;
#42225 = DIRECTION('center_axis',(1.88526971141291E-28,-2.90739654573716E-15,
-1.)) ;
#42226 = DIRECTION('ref_axis',(-1.35627620245787E-13,1.,-2.90739654573716E-15)) ;
#42227 = DIRECTION('center_axis',(1.,-1.66533453692587E-16,2.1716102378779E-15)) ;
#42228 = DIRECTION('ref_axis',(1.41780339089714E-15,-0.70710678118655,-0.707106781186545)) ;
#42229 = DIRECTION('center_axis',(1.,1.35627620245787E-13,-2.05796303467862E-28)) ;
#42230 = DIRECTION('ref_axis',(1.35627620245787E-13,-1.,2.90739654573716E-15)) ;
#42231 = DIRECTION('',(-1.,1.66533453692587E-16,-2.1716102378779E-15)) ;
#42232 = DIRECTION('center_axis',(-1.,-1.35627620245747E-13,2.05796303467745E-28)) ;
#42233 = DIRECTION('ref_axis',(1.88526971141291E-28,-2.90739654573716E-15,
-1.)) ;
#42234 = DIRECTION('',(1.,-1.66533453692587E-16,2.1716102378779E-15)) ;
#42235 = DIRECTION('center_axis',(-1.,6.48092690624107E-15,-2.07369595641671E-28)) ;
#42236 = DIRECTION('ref_axis',(0.,-1.,0.)) ;
#42237 = DIRECTION('center_axis',(-1.,7.08071943160919E-13,-2.24717289282075E-27)) ;
#42238 = DIRECTION('ref_axis',(-1.88526971141296E-28,2.90739654573716E-15,
1.)) ;
#42239 = DIRECTION('center_axis',(6.48092690624107E-15,1.,-2.90739654573716E-15)) ;
#42240 = DIRECTION('ref_axis',(1.,-6.48092690624107E-15,2.07369595641671E-28)) ;
#42241 = DIRECTION('center_axis',(-1.66533453692966E-16,-1.,3.83386399937507E-28)) ;
#42242 = DIRECTION('ref_axis',(0.707106781186648,-1.17756934401E-16,-0.707106781186447)) ;
#42243 = DIRECTION('center_axis',(-6.48092690624107E-15,-1.,2.90739654573716E-15)) ;
#42244 = DIRECTION('ref_axis',(1.88526971141291E-28,-2.90739654573716E-15,
-1.)) ;
#42245 = DIRECTION('',(1.66533453692966E-16,1.,-3.83386399937507E-28)) ;
#42246 = DIRECTION('center_axis',(1.,-6.48092690624107E-15,2.07369595641671E-28)) ;
#42247 = DIRECTION('ref_axis',(0.,1.,0.)) ;
#42248 = DIRECTION('center_axis',(1.,-1.48589474058271E-13,-5.59482469102492E-13)) ;
#42249 = DIRECTION('ref_axis',(-1.48589474058269E-13,-1.,2.90739654573716E-15)) ;
#42250 = DIRECTION('center_axis',(6.48092690624107E-15,1.,-2.90739654573716E-15)) ;
#42251 = DIRECTION('ref_axis',(1.88526971141291E-28,-2.90739654573716E-15,
-1.)) ;
#42252 = DIRECTION('center_axis',(-1.,6.48092690624107E-15,-2.07369595641671E-28)) ;
#42253 = DIRECTION('ref_axis',(0.,-1.,0.)) ;
#42254 = DIRECTION('center_axis',(-1.,1.48589474058269E-13,-6.20535494751205E-28)) ;
#42255 = DIRECTION('ref_axis',(1.48589474058269E-13,1.,-2.90739654573716E-15)) ;
#42256 = DIRECTION('center_axis',(-6.48092690624107E-15,-1.,2.90739654573716E-15)) ;
#42257 = DIRECTION('ref_axis',(1.88526971141291E-28,-2.90739654573716E-15,
-1.)) ;
#42258 = DIRECTION('center_axis',(1.88526971141291E-28,-2.90739654573716E-15,
-1.)) ;
#42259 = DIRECTION('ref_axis',(1.,-6.48092690624108E-15,2.07369595641671E-28)) ;
#42260 = DIRECTION('center_axis',(2.1716102378779E-15,-3.66854633798134E-28,
-1.)) ;
#42261 = DIRECTION('ref_axis',(0.707106781186543,-0.707106781186552,1.53556032529784E-15)) ;
#42262 = DIRECTION('',(2.1716102378779E-15,-3.66854633798134E-28,-1.)) ;
#42263 = DIRECTION('center_axis',(-1.66533453692966E-16,-1.,3.83386399937507E-28)) ;
#42264 = DIRECTION('ref_axis',(0.707106781186648,-1.17756934401E-16,-0.707106781186447)) ;
#42265 = DIRECTION('center_axis',(6.48092690628146E-15,1.,-2.90739654573716E-15)) ;
#42266 = DIRECTION('ref_axis',(1.,-6.48092690628146E-15,2.07369595641789E-28)) ;
#42267 = DIRECTION('',(1.66533453692966E-16,1.,-3.83386399937507E-28)) ;
#42268 = DIRECTION('center_axis',(1.,-6.48092690624107E-15,2.07369595641671E-28)) ;
#42269 = DIRECTION('ref_axis',(0.,1.,0.)) ;
#42270 = DIRECTION('center_axis',(1.,-1.48589474058269E-13,6.20535494751205E-28)) ;
#42271 = DIRECTION('ref_axis',(-1.88526971141292E-28,2.90739654573716E-15,
1.)) ;
#42272 = DIRECTION('center_axis',(-6.48092690624107E-15,-1.,2.90739654573716E-15)) ;
#42273 = DIRECTION('ref_axis',(-1.,6.48092690624107E-15,-2.07369595641671E-28)) ;
#42274 = DIRECTION('center_axis',(8.32667268460789E-17,1.,-3.83780830390118E-28)) ;
#42275 = DIRECTION('ref_axis',(-0.707106781186447,5.88784671997906E-17,-0.707106781186648)) ;
#42276 = DIRECTION('center_axis',(6.48092690624107E-15,1.,-2.90739654573716E-15)) ;
#42277 = DIRECTION('ref_axis',(1.88526971141291E-28,-2.90739654573716E-15,
-1.)) ;
#42278 = DIRECTION('',(-8.32667268460789E-17,-1.,3.83780830390118E-28)) ;
#42279 = DIRECTION('center_axis',(-1.,3.33066907386739E-16,-2.1716102378779E-15)) ;
#42280 = DIRECTION('ref_axis',(-1.30004645649559E-15,0.70710678118655,0.707106781186545)) ;
#42281 = DIRECTION('',(-1.,3.33066907386739E-16,-2.1716102378779E-15)) ;
#42282 = DIRECTION('',(1.,-3.33066907386739E-16,2.1716102378779E-15)) ;
#42283 = DIRECTION('center_axis',(8.32667268460789E-17,1.,-3.83780830390118E-28)) ;
#42284 = DIRECTION('ref_axis',(-0.707106781186447,5.88784671997906E-17,-0.707106781186648)) ;
#42285 = DIRECTION('center_axis',(-6.48092690624107E-15,-1.,2.90739654573716E-15)) ;
#42286 = DIRECTION('ref_axis',(-1.,6.48092690624107E-15,-2.07369595641671E-28)) ;
#42287 = DIRECTION('',(-8.32667268460789E-17,-1.,3.83780830390118E-28)) ;
#42288 = DIRECTION('center_axis',(1.,-3.33066907386739E-16,2.1716102378779E-15)) ;
#42289 = DIRECTION('ref_axis',(-1.77107419409959E-15,-0.707106781186545,0.70710678118655)) ;
#42290 = DIRECTION('',(1.,-3.33066907386739E-16,2.1716102378779E-15)) ;
#42291 = DIRECTION('center_axis',(-0.81649658092765,0.408248290464166,0.408248290463711)) ;
#42292 = DIRECTION('ref_axis',(-0.577350269189702,-0.577350269189929,-0.577350269189247)) ;
#42293 = DIRECTION('center_axis',(2.17161023787787E-15,-3.83420712807771E-28,
-1.)) ;
#42294 = DIRECTION('ref_axis',(-0.707106781186582,-0.707106781186513,-1.53556032529738E-15)) ;
#42295 = DIRECTION('center_axis',(-0.40824829046392,0.408248290464147,-0.816496580927556)) ;
#42296 = DIRECTION('ref_axis',(0.577350269189076,-0.577350269189986,-0.577350269189815)) ;
#42297 = DIRECTION('center_axis',(1.,-1.66533453692966E-16,2.1716102378779E-15)) ;
#42298 = DIRECTION('ref_axis',(1.65331725969831E-15,0.707106781186545,-0.70710678118655)) ;
#42299 = DIRECTION('center_axis',(1.,1.35627620245787E-13,-2.05796303467862E-28)) ;
#42300 = DIRECTION('ref_axis',(1.8852697114129E-28,-2.90739654573716E-15,
-1.)) ;
#42301 = DIRECTION('',(-1.,1.66533453692966E-16,-2.1716102378779E-15)) ;
#42302 = DIRECTION('center_axis',(-1.,-1.35627620245787E-13,2.05796303467862E-28)) ;
#42303 = DIRECTION('ref_axis',(-1.35627620245787E-13,1.,-2.90739654573716E-15)) ;
#42304 = DIRECTION('center_axis',(0.40824829046392,-0.408248290464147,-0.816496580927556)) ;
#42305 = DIRECTION('ref_axis',(-0.577350269189834,0.577350269189152,-0.577350269189891)) ;
#42306 = DIRECTION('center_axis',(2.17161023787787E-15,-3.83815143260382E-28,
-1.)) ;
#42307 = DIRECTION('ref_axis',(-0.707106781186656,0.707106781186439,-1.53556032529808E-15)) ;
#42308 = DIRECTION('center_axis',(-0.81649658092765,0.408248290464166,-0.408248290463711)) ;
#42309 = DIRECTION('ref_axis',(0.577350269189702,0.577350269189929,-0.577350269189247)) ;
#42310 = DIRECTION('center_axis',(-3.33066907386739E-16,-1.,3.66031460022645E-28)) ;
#42311 = DIRECTION('ref_axis',(-2.17161023787795E-15,3.66754751528624E-28,
1.)) ;
#42312 = DIRECTION('center_axis',(2.1716102378779E-15,-3.83815143260386E-28,
-1.)) ;
#42313 = DIRECTION('ref_axis',(1.,-1.66533453692941E-16,2.1716102378779E-15)) ;
#42314 = DIRECTION('center_axis',(2.1716102378779E-15,-3.83815143260386E-28,
-1.)) ;
#42315 = DIRECTION('ref_axis',(1.,-1.66533453692941E-16,2.1716102378779E-15)) ;
#42316 = DIRECTION('center_axis',(2.1716102378779E-15,-3.83815143260386E-28,
-1.)) ;
#42317 = DIRECTION('ref_axis',(1.,-1.66533453692941E-16,2.1716102378779E-15)) ;
#42318 = DIRECTION('',(-1.66533453692966E-16,-1.,3.83386399937507E-28)) ;
#42319 = DIRECTION('',(1.,-1.66533453692587E-16,2.1716102378779E-15)) ;
#42320 = DIRECTION('',(8.32667268460789E-17,1.,-3.83780830390118E-28)) ;
#42321 = DIRECTION('',(-1.,1.66533453692966E-16,-2.1716102378779E-15)) ;
#42322 = DIRECTION('center_axis',(-0.816496580927764,0.408248290464109,0.408248290463541)) ;
#42323 = DIRECTION('ref_axis',(-0.577350269189531,-0.577350269189986,-0.57735026918936)) ;
#42324 = DIRECTION('center_axis',(1.,1.35627620245787E-13,2.17161023787752E-15)) ;
#42325 = DIRECTION('ref_axis',(1.35627620245787E-13,-1.,2.90739654573778E-15)) ;
#42326 = DIRECTION('center_axis',(6.48092690624107E-15,1.,-2.90739654573747E-15)) ;
#42327 = DIRECTION('ref_axis',(2.17161023787792E-15,-2.90739654573748E-15,
-1.)) ;
#42328 = DIRECTION('center_axis',(2.1716102378779E-15,-3.83420712807775E-28,
-1.)) ;
#42329 = DIRECTION('ref_axis',(-0.70710678118651,-0.707106781186585,-1.53556032529724E-15)) ;
#42330 = DIRECTION('center_axis',(0.40824829046392,-0.408248290464147,-0.816496580927556)) ;
#42331 = DIRECTION('ref_axis',(-0.577350269189986,0.577350269189076,-0.577350269189815)) ;
#42332 = DIRECTION('center_axis',(-6.48092690624107E-15,-1.,2.90739654573747E-15)) ;
#42333 = DIRECTION('ref_axis',(-1.,6.48092690624106E-15,-2.17161023787794E-15)) ;
#42334 = DIRECTION('center_axis',(1.,1.35627620245787E-13,2.17161023787752E-15)) ;
#42335 = DIRECTION('ref_axis',(2.17161023787791E-15,-2.90739654573749E-15,
-1.)) ;
#42336 = DIRECTION('center_axis',(2.1716102378779E-15,-3.83815143260386E-28,
-1.)) ;
#42337 = DIRECTION('ref_axis',(-0.707106781186656,0.707106781186439,-1.5355603252981E-15)) ;
#42338 = DIRECTION('center_axis',(1.66533453692966E-16,1.,-3.83386399937507E-28)) ;
#42339 = DIRECTION('ref_axis',(-0.707106781186596,1.17756934400449E-16,-0.707106781186499)) ;
#42340 = DIRECTION('',(1.66533453692966E-16,1.,-3.83386399937507E-28)) ;
#42341 = DIRECTION('center_axis',(1.,-1.66533453692966E-16,2.1716102378779E-15)) ;
#42342 = DIRECTION('ref_axis',(1.65331725969841E-15,0.707106781186495,-0.7071067811866)) ;
#42343 = DIRECTION('center_axis',(1.,1.35627620245787E-13,2.17161023787752E-15)) ;
#42344 = DIRECTION('ref_axis',(-1.35627620245787E-13,1.,-2.90739654573778E-15)) ;
#42345 = DIRECTION('center_axis',(-1.,1.66533453692587E-16,-2.1716102378779E-15)) ;
#42346 = DIRECTION('ref_axis',(1.41780339089726E-15,-0.707106781186499,-0.707106781186596)) ;
#42347 = DIRECTION('',(-1.,1.66533453692587E-16,-2.1716102378779E-15)) ;
#42348 = DIRECTION('center_axis',(1.,1.35627620245787E-13,2.17161023787752E-15)) ;
#42349 = DIRECTION('ref_axis',(2.17161023787792E-15,-2.90739654573749E-15,
-1.)) ;
#42350 = DIRECTION('center_axis',(-8.32667268460789E-17,-1.,3.83780830390118E-28)) ;
#42351 = DIRECTION('ref_axis',(0.707106781186599,-5.8878467200346E-17,-0.707106781186496)) ;
#42352 = DIRECTION('center_axis',(-6.48092690624107E-15,-1.,2.90739654573747E-15)) ;
#42353 = DIRECTION('ref_axis',(1.,-6.48092690624106E-15,2.17161023787794E-15)) ;
#42354 = DIRECTION('center_axis',(6.48092690624107E-15,1.,-2.90739654573747E-15)) ;
#42355 = DIRECTION('ref_axis',(2.17161023787792E-15,-2.90739654573748E-15,
-1.)) ;
#42356 = DIRECTION('center_axis',(-0.408248290463939,0.408248290464166,-0.816496580927537)) ;
#42357 = DIRECTION('ref_axis',(0.577350269189076,-0.577350269189986,-0.577350269189815)) ;
#42358 = DIRECTION('center_axis',(0.408248290463948,-0.816496580927442,-0.408248290464346)) ;
#42359 = DIRECTION('ref_axis',(0.577350269189304,0.577350269189986,-0.577350269189588)) ;
#42360 = DIRECTION('center_axis',(-2.1716102378779E-15,3.66854633798134E-28,
1.)) ;
#42361 = DIRECTION('ref_axis',(0.707106781186452,0.707106781186643,1.53556032529713E-15)) ;
#42362 = DIRECTION('center_axis',(1.88526971141291E-28,-2.90739654573716E-15,
-1.)) ;
#42363 = DIRECTION('ref_axis',(-1.35627620245787E-13,1.,-2.90739654573716E-15)) ;
#42364 = DIRECTION('center_axis',(1.,-1.66533453692587E-16,2.1716102378779E-15)) ;
#42365 = DIRECTION('ref_axis',(1.41780339089714E-15,-0.70710678118655,-0.707106781186545)) ;
#42366 = DIRECTION('center_axis',(1.,1.35627620245787E-13,-2.05796303467862E-28)) ;
#42367 = DIRECTION('ref_axis',(1.35627620245787E-13,-1.,2.90739654573716E-15)) ;
#42368 = DIRECTION('',(-1.,1.66533453692587E-16,-2.1716102378779E-15)) ;
#42369 = DIRECTION('center_axis',(-1.,-1.35627620245747E-13,2.05796303467745E-28)) ;
#42370 = DIRECTION('ref_axis',(1.88526971141291E-28,-2.90739654573716E-15,
-1.)) ;
#42371 = DIRECTION('',(1.,-1.66533453692587E-16,2.1716102378779E-15)) ;
#42372 = DIRECTION('center_axis',(-1.,6.48092690624107E-15,-2.07369595641671E-28)) ;
#42373 = DIRECTION('ref_axis',(0.,-1.,0.)) ;
#42374 = DIRECTION('center_axis',(-1.,7.08071943160919E-13,-2.24717289282075E-27)) ;
#42375 = DIRECTION('ref_axis',(-1.88526971141296E-28,2.90739654573716E-15,
1.)) ;
#42376 = DIRECTION('center_axis',(6.48092690624107E-15,1.,-2.90739654573716E-15)) ;
#42377 = DIRECTION('ref_axis',(1.,-6.48092690624107E-15,2.07369595641671E-28)) ;
#42378 = DIRECTION('center_axis',(-1.66533453692966E-16,-1.,3.83386399937507E-28)) ;
#42379 = DIRECTION('ref_axis',(0.707106781186648,-1.17756934401E-16,-0.707106781186447)) ;
#42380 = DIRECTION('center_axis',(-6.48092690624107E-15,-1.,2.90739654573716E-15)) ;
#42381 = DIRECTION('ref_axis',(1.88526971141291E-28,-2.90739654573716E-15,
-1.)) ;
#42382 = DIRECTION('',(1.66533453692966E-16,1.,-3.83386399937507E-28)) ;
#42383 = DIRECTION('center_axis',(1.,-6.48092690624107E-15,2.07369595641671E-28)) ;
#42384 = DIRECTION('ref_axis',(0.,1.,0.)) ;
#42385 = DIRECTION('center_axis',(1.,-1.48589474058271E-13,-5.59482469102492E-13)) ;
#42386 = DIRECTION('ref_axis',(-1.48589474058269E-13,-1.,2.90739654573716E-15)) ;
#42387 = DIRECTION('center_axis',(6.48092690624107E-15,1.,-2.90739654573716E-15)) ;
#42388 = DIRECTION('ref_axis',(1.88526971141291E-28,-2.90739654573716E-15,
-1.)) ;
#42389 = DIRECTION('center_axis',(-1.,6.48092690624107E-15,-2.07369595641671E-28)) ;
#42390 = DIRECTION('ref_axis',(0.,-1.,0.)) ;
#42391 = DIRECTION('center_axis',(-1.,1.48589474058269E-13,-6.20535494751205E-28)) ;
#42392 = DIRECTION('ref_axis',(1.48589474058269E-13,1.,-2.90739654573716E-15)) ;
#42393 = DIRECTION('center_axis',(-6.48092690624107E-15,-1.,2.90739654573716E-15)) ;
#42394 = DIRECTION('ref_axis',(1.88526971141291E-28,-2.90739654573716E-15,
-1.)) ;
#42395 = DIRECTION('center_axis',(1.88526971141291E-28,-2.90739654573716E-15,
-1.)) ;
#42396 = DIRECTION('ref_axis',(1.,-6.48092690624108E-15,2.07369595641671E-28)) ;
#42397 = DIRECTION('center_axis',(2.1716102378779E-15,-3.66854633798134E-28,
-1.)) ;
#42398 = DIRECTION('ref_axis',(0.707106781186543,-0.707106781186552,1.53556032529784E-15)) ;
#42399 = DIRECTION('',(2.1716102378779E-15,-3.66854633798134E-28,-1.)) ;
#42400 = DIRECTION('center_axis',(-1.66533453692966E-16,-1.,3.83386399937507E-28)) ;
#42401 = DIRECTION('ref_axis',(0.707106781186648,-1.17756934401E-16,-0.707106781186447)) ;
#42402 = DIRECTION('center_axis',(6.48092690628146E-15,1.,-2.90739654573716E-15)) ;
#42403 = DIRECTION('ref_axis',(1.,-6.48092690628146E-15,2.07369595641789E-28)) ;
#42404 = DIRECTION('',(1.66533453692966E-16,1.,-3.83386399937507E-28)) ;
#42405 = DIRECTION('center_axis',(1.,-6.48092690624107E-15,2.07369595641671E-28)) ;
#42406 = DIRECTION('ref_axis',(0.,1.,0.)) ;
#42407 = DIRECTION('center_axis',(1.,-1.48589474058269E-13,6.20535494751205E-28)) ;
#42408 = DIRECTION('ref_axis',(-1.88526971141292E-28,2.90739654573716E-15,
1.)) ;
#42409 = DIRECTION('center_axis',(-6.48092690624107E-15,-1.,2.90739654573716E-15)) ;
#42410 = DIRECTION('ref_axis',(-1.,6.48092690624107E-15,-2.07369595641671E-28)) ;
#42411 = DIRECTION('center_axis',(8.32667268460789E-17,1.,-3.83780830390118E-28)) ;
#42412 = DIRECTION('ref_axis',(-0.707106781186447,5.88784671997906E-17,-0.707106781186648)) ;
#42413 = DIRECTION('center_axis',(6.48092690624107E-15,1.,-2.90739654573716E-15)) ;
#42414 = DIRECTION('ref_axis',(1.88526971141291E-28,-2.90739654573716E-15,
-1.)) ;
#42415 = DIRECTION('',(-8.32667268460789E-17,-1.,3.83780830390118E-28)) ;
#42416 = DIRECTION('center_axis',(-1.,3.33066907386739E-16,-2.1716102378779E-15)) ;
#42417 = DIRECTION('ref_axis',(-1.30004645649559E-15,0.70710678118655,0.707106781186545)) ;
#42418 = DIRECTION('',(-1.,3.33066907386739E-16,-2.1716102378779E-15)) ;
#42419 = DIRECTION('',(1.,-3.33066907386739E-16,2.1716102378779E-15)) ;
#42420 = DIRECTION('center_axis',(8.32667268460789E-17,1.,-3.83780830390118E-28)) ;
#42421 = DIRECTION('ref_axis',(-0.707106781186447,5.88784671997906E-17,-0.707106781186648)) ;
#42422 = DIRECTION('center_axis',(-6.48092690624107E-15,-1.,2.90739654573716E-15)) ;
#42423 = DIRECTION('ref_axis',(-1.,6.48092690624107E-15,-2.07369595641671E-28)) ;
#42424 = DIRECTION('',(-8.32667268460789E-17,-1.,3.83780830390118E-28)) ;
#42425 = DIRECTION('center_axis',(1.,-3.33066907386739E-16,2.1716102378779E-15)) ;
#42426 = DIRECTION('ref_axis',(-1.77107419409959E-15,-0.707106781186545,0.70710678118655)) ;
#42427 = DIRECTION('',(1.,-3.33066907386739E-16,2.1716102378779E-15)) ;
#42428 = DIRECTION('center_axis',(-0.81649658092765,0.408248290464166,0.408248290463711)) ;
#42429 = DIRECTION('ref_axis',(-0.577350269189702,-0.577350269189929,-0.577350269189247)) ;
#42430 = DIRECTION('center_axis',(2.17161023787787E-15,-3.83420712807771E-28,
-1.)) ;
#42431 = DIRECTION('ref_axis',(-0.707106781186582,-0.707106781186513,-1.53556032529738E-15)) ;
#42432 = DIRECTION('center_axis',(-0.40824829046392,0.408248290464147,-0.816496580927556)) ;
#42433 = DIRECTION('ref_axis',(0.577350269189076,-0.577350269189986,-0.577350269189815)) ;
#42434 = DIRECTION('center_axis',(1.,-1.66533453692966E-16,2.1716102378779E-15)) ;
#42435 = DIRECTION('ref_axis',(1.65331725969831E-15,0.707106781186545,-0.70710678118655)) ;
#42436 = DIRECTION('center_axis',(1.,1.35627620245787E-13,-2.05796303467862E-28)) ;
#42437 = DIRECTION('ref_axis',(1.8852697114129E-28,-2.90739654573716E-15,
-1.)) ;
#42438 = DIRECTION('',(-1.,1.66533453692966E-16,-2.1716102378779E-15)) ;
#42439 = DIRECTION('center_axis',(-1.,-1.35627620245787E-13,2.05796303467862E-28)) ;
#42440 = DIRECTION('ref_axis',(-1.35627620245787E-13,1.,-2.90739654573716E-15)) ;
#42441 = DIRECTION('center_axis',(0.40824829046392,-0.408248290464147,-0.816496580927556)) ;
#42442 = DIRECTION('ref_axis',(-0.577350269189834,0.577350269189152,-0.577350269189891)) ;
#42443 = DIRECTION('center_axis',(2.17161023787787E-15,-3.83815143260382E-28,
-1.)) ;
#42444 = DIRECTION('ref_axis',(-0.707106781186656,0.707106781186439,-1.53556032529808E-15)) ;
#42445 = DIRECTION('center_axis',(-0.81649658092765,0.408248290464166,-0.408248290463711)) ;
#42446 = DIRECTION('ref_axis',(0.577350269189702,0.577350269189929,-0.577350269189247)) ;
#42447 = DIRECTION('center_axis',(-3.33066907386739E-16,-1.,3.66031460022645E-28)) ;
#42448 = DIRECTION('ref_axis',(-2.17161023787795E-15,3.66754751528624E-28,
1.)) ;
#42449 = DIRECTION('center_axis',(2.1716102378779E-15,-3.83815143260386E-28,
-1.)) ;
#42450 = DIRECTION('ref_axis',(1.,-1.66533453692941E-16,2.1716102378779E-15)) ;
#42451 = DIRECTION('center_axis',(2.1716102378779E-15,-3.83815143260386E-28,
-1.)) ;
#42452 = DIRECTION('ref_axis',(1.,-1.66533453692941E-16,2.1716102378779E-15)) ;
#42453 = DIRECTION('center_axis',(2.1716102378779E-15,-3.83815143260386E-28,
-1.)) ;
#42454 = DIRECTION('ref_axis',(1.,-1.66533453692941E-16,2.1716102378779E-15)) ;
#42455 = DIRECTION('',(-1.66533453692966E-16,-1.,3.83386399937507E-28)) ;
#42456 = DIRECTION('',(1.,-1.66533453692587E-16,2.1716102378779E-15)) ;
#42457 = DIRECTION('',(8.32667268460789E-17,1.,-3.83780830390118E-28)) ;
#42458 = DIRECTION('',(-1.,1.66533453692966E-16,-2.1716102378779E-15)) ;
#42459 = DIRECTION('center_axis',(-0.816496580927764,0.408248290464109,0.408248290463541)) ;
#42460 = DIRECTION('ref_axis',(-0.577350269189531,-0.577350269189986,-0.57735026918936)) ;
#42461 = DIRECTION('center_axis',(1.,1.35627620245787E-13,2.17161023787752E-15)) ;
#42462 = DIRECTION('ref_axis',(1.35627620245787E-13,-1.,2.90739654573778E-15)) ;
#42463 = DIRECTION('center_axis',(6.48092690624107E-15,1.,-2.90739654573747E-15)) ;
#42464 = DIRECTION('ref_axis',(2.17161023787792E-15,-2.90739654573748E-15,
-1.)) ;
#42465 = DIRECTION('center_axis',(2.1716102378779E-15,-3.83420712807775E-28,
-1.)) ;
#42466 = DIRECTION('ref_axis',(-0.70710678118651,-0.707106781186585,-1.53556032529724E-15)) ;
#42467 = DIRECTION('center_axis',(0.40824829046392,-0.408248290464147,-0.816496580927556)) ;
#42468 = DIRECTION('ref_axis',(-0.577350269189986,0.577350269189076,-0.577350269189815)) ;
#42469 = DIRECTION('center_axis',(-6.48092690624107E-15,-1.,2.90739654573747E-15)) ;
#42470 = DIRECTION('ref_axis',(-1.,6.48092690624106E-15,-2.17161023787794E-15)) ;
#42471 = DIRECTION('center_axis',(1.,1.35627620245787E-13,2.17161023787752E-15)) ;
#42472 = DIRECTION('ref_axis',(2.17161023787791E-15,-2.90739654573749E-15,
-1.)) ;
#42473 = DIRECTION('center_axis',(2.1716102378779E-15,-3.83815143260386E-28,
-1.)) ;
#42474 = DIRECTION('ref_axis',(-0.707106781186656,0.707106781186439,-1.5355603252981E-15)) ;
#42475 = DIRECTION('center_axis',(1.66533453692966E-16,1.,-3.83386399937507E-28)) ;
#42476 = DIRECTION('ref_axis',(-0.707106781186596,1.17756934400449E-16,-0.707106781186499)) ;
#42477 = DIRECTION('',(1.66533453692966E-16,1.,-3.83386399937507E-28)) ;
#42478 = DIRECTION('center_axis',(1.,-1.66533453692966E-16,2.1716102378779E-15)) ;
#42479 = DIRECTION('ref_axis',(1.65331725969841E-15,0.707106781186495,-0.7071067811866)) ;
#42480 = DIRECTION('center_axis',(1.,1.35627620245787E-13,2.17161023787752E-15)) ;
#42481 = DIRECTION('ref_axis',(-1.35627620245787E-13,1.,-2.90739654573778E-15)) ;
#42482 = DIRECTION('center_axis',(-1.,1.66533453692587E-16,-2.1716102378779E-15)) ;
#42483 = DIRECTION('ref_axis',(1.41780339089726E-15,-0.707106781186499,-0.707106781186596)) ;
#42484 = DIRECTION('',(-1.,1.66533453692587E-16,-2.1716102378779E-15)) ;
#42485 = DIRECTION('center_axis',(1.,1.35627620245787E-13,2.17161023787752E-15)) ;
#42486 = DIRECTION('ref_axis',(2.17161023787792E-15,-2.90739654573749E-15,
-1.)) ;
#42487 = DIRECTION('center_axis',(-8.32667268460789E-17,-1.,3.83780830390118E-28)) ;
#42488 = DIRECTION('ref_axis',(0.707106781186599,-5.8878467200346E-17,-0.707106781186496)) ;
#42489 = DIRECTION('center_axis',(-6.48092690624107E-15,-1.,2.90739654573747E-15)) ;
#42490 = DIRECTION('ref_axis',(1.,-6.48092690624106E-15,2.17161023787794E-15)) ;
#42491 = DIRECTION('center_axis',(6.48092690624107E-15,1.,-2.90739654573747E-15)) ;
#42492 = DIRECTION('ref_axis',(2.17161023787792E-15,-2.90739654573748E-15,
-1.)) ;
#42493 = DIRECTION('center_axis',(-0.408248290463939,0.408248290464166,-0.816496580927537)) ;
#42494 = DIRECTION('ref_axis',(0.577350269189076,-0.577350269189986,-0.577350269189815)) ;
#42495 = DIRECTION('center_axis',(0.408248290463948,-0.816496580927442,-0.408248290464346)) ;
#42496 = DIRECTION('ref_axis',(0.577350269189304,0.577350269189986,-0.577350269189588)) ;
#42497 = DIRECTION('center_axis',(-2.1716102378779E-15,3.66854633798134E-28,
1.)) ;
#42498 = DIRECTION('ref_axis',(0.707106781186452,0.707106781186643,1.53556032529713E-15)) ;
#42499 = DIRECTION('center_axis',(1.88526971141291E-28,-2.90739654573716E-15,
-1.)) ;
#42500 = DIRECTION('ref_axis',(-1.35627620245787E-13,1.,-2.90739654573716E-15)) ;
#42501 = DIRECTION('center_axis',(1.,-1.66533453692587E-16,2.1716102378779E-15)) ;
#42502 = DIRECTION('ref_axis',(1.41780339089714E-15,-0.70710678118655,-0.707106781186545)) ;
#42503 = DIRECTION('center_axis',(1.,1.35627620245787E-13,-2.05796303467862E-28)) ;
#42504 = DIRECTION('ref_axis',(1.35627620245787E-13,-1.,2.90739654573716E-15)) ;
#42505 = DIRECTION('',(-1.,1.66533453692587E-16,-2.1716102378779E-15)) ;
#42506 = DIRECTION('center_axis',(-1.,-1.35627620245747E-13,2.05796303467745E-28)) ;
#42507 = DIRECTION('ref_axis',(1.88526971141291E-28,-2.90739654573716E-15,
-1.)) ;
#42508 = DIRECTION('',(1.,-1.66533453692587E-16,2.1716102378779E-15)) ;
#42509 = DIRECTION('center_axis',(-1.,6.48092690624107E-15,-2.07369595641671E-28)) ;
#42510 = DIRECTION('ref_axis',(0.,-1.,0.)) ;
#42511 = DIRECTION('center_axis',(-1.,7.08071943160919E-13,-2.24717289282075E-27)) ;
#42512 = DIRECTION('ref_axis',(-1.88526971141296E-28,2.90739654573716E-15,
1.)) ;
#42513 = DIRECTION('center_axis',(6.48092690624107E-15,1.,-2.90739654573716E-15)) ;
#42514 = DIRECTION('ref_axis',(1.,-6.48092690624107E-15,2.07369595641671E-28)) ;
#42515 = DIRECTION('center_axis',(-1.66533453692966E-16,-1.,3.83386399937507E-28)) ;
#42516 = DIRECTION('ref_axis',(0.707106781186648,-1.17756934401E-16,-0.707106781186447)) ;
#42517 = DIRECTION('center_axis',(-6.48092690624107E-15,-1.,2.90739654573716E-15)) ;
#42518 = DIRECTION('ref_axis',(1.88526971141291E-28,-2.90739654573716E-15,
-1.)) ;
#42519 = DIRECTION('',(1.66533453692966E-16,1.,-3.83386399937507E-28)) ;
#42520 = DIRECTION('center_axis',(1.,-6.48092690624107E-15,2.07369595641671E-28)) ;
#42521 = DIRECTION('ref_axis',(0.,1.,0.)) ;
#42522 = DIRECTION('center_axis',(1.,-1.48589474058271E-13,-5.59482469102492E-13)) ;
#42523 = DIRECTION('ref_axis',(-1.48589474058269E-13,-1.,2.90739654573716E-15)) ;
#42524 = DIRECTION('center_axis',(6.48092690624107E-15,1.,-2.90739654573716E-15)) ;
#42525 = DIRECTION('ref_axis',(1.88526971141291E-28,-2.90739654573716E-15,
-1.)) ;
#42526 = DIRECTION('center_axis',(-1.,6.48092690624107E-15,-2.07369595641671E-28)) ;
#42527 = DIRECTION('ref_axis',(0.,-1.,0.)) ;
#42528 = DIRECTION('center_axis',(-1.,1.48589474058269E-13,-6.20535494751205E-28)) ;
#42529 = DIRECTION('ref_axis',(1.48589474058269E-13,1.,-2.90739654573716E-15)) ;
#42530 = DIRECTION('center_axis',(-6.48092690624107E-15,-1.,2.90739654573716E-15)) ;
#42531 = DIRECTION('ref_axis',(1.88526971141291E-28,-2.90739654573716E-15,
-1.)) ;
#42532 = DIRECTION('center_axis',(1.88526971141291E-28,-2.90739654573716E-15,
-1.)) ;
#42533 = DIRECTION('ref_axis',(1.,-6.48092690624108E-15,2.07369595641671E-28)) ;
#42534 = DIRECTION('center_axis',(2.1716102378779E-15,-3.66854633798134E-28,
-1.)) ;
#42535 = DIRECTION('ref_axis',(0.707106781186543,-0.707106781186552,1.53556032529784E-15)) ;
#42536 = DIRECTION('',(2.1716102378779E-15,-3.66854633798134E-28,-1.)) ;
#42537 = DIRECTION('center_axis',(-1.66533453692966E-16,-1.,3.83386399937507E-28)) ;
#42538 = DIRECTION('ref_axis',(0.707106781186648,-1.17756934401E-16,-0.707106781186447)) ;
#42539 = DIRECTION('center_axis',(6.48092690628146E-15,1.,-2.90739654573716E-15)) ;
#42540 = DIRECTION('ref_axis',(1.,-6.48092690628146E-15,2.07369595641789E-28)) ;
#42541 = DIRECTION('',(1.66533453692966E-16,1.,-3.83386399937507E-28)) ;
#42542 = DIRECTION('center_axis',(1.,-6.48092690624107E-15,2.07369595641671E-28)) ;
#42543 = DIRECTION('ref_axis',(0.,1.,0.)) ;
#42544 = DIRECTION('center_axis',(1.,-1.48589474058269E-13,6.20535494751205E-28)) ;
#42545 = DIRECTION('ref_axis',(-1.88526971141292E-28,2.90739654573716E-15,
1.)) ;
#42546 = DIRECTION('center_axis',(-6.48092690624107E-15,-1.,2.90739654573716E-15)) ;
#42547 = DIRECTION('ref_axis',(-1.,6.48092690624107E-15,-2.07369595641671E-28)) ;
#42548 = DIRECTION('center_axis',(8.32667268460789E-17,1.,-3.83780830390118E-28)) ;
#42549 = DIRECTION('ref_axis',(-0.707106781186447,5.88784671997906E-17,-0.707106781186648)) ;
#42550 = DIRECTION('center_axis',(6.48092690624107E-15,1.,-2.90739654573716E-15)) ;
#42551 = DIRECTION('ref_axis',(1.88526971141291E-28,-2.90739654573716E-15,
-1.)) ;
#42552 = DIRECTION('',(-8.32667268460789E-17,-1.,3.83780830390118E-28)) ;
#42553 = DIRECTION('center_axis',(-1.,3.33066907386739E-16,-2.1716102378779E-15)) ;
#42554 = DIRECTION('ref_axis',(-1.30004645649559E-15,0.70710678118655,0.707106781186545)) ;
#42555 = DIRECTION('',(-1.,3.33066907386739E-16,-2.1716102378779E-15)) ;
#42556 = DIRECTION('',(1.,-3.33066907386739E-16,2.1716102378779E-15)) ;
#42557 = DIRECTION('center_axis',(8.32667268460789E-17,1.,-3.83780830390118E-28)) ;
#42558 = DIRECTION('ref_axis',(-0.707106781186447,5.88784671997906E-17,-0.707106781186648)) ;
#42559 = DIRECTION('center_axis',(-6.48092690624107E-15,-1.,2.90739654573716E-15)) ;
#42560 = DIRECTION('ref_axis',(-1.,6.48092690624107E-15,-2.07369595641671E-28)) ;
#42561 = DIRECTION('',(-8.32667268460789E-17,-1.,3.83780830390118E-28)) ;
#42562 = DIRECTION('center_axis',(1.,-3.33066907386739E-16,2.1716102378779E-15)) ;
#42563 = DIRECTION('ref_axis',(-1.77107419409959E-15,-0.707106781186545,0.70710678118655)) ;
#42564 = DIRECTION('',(1.,-3.33066907386739E-16,2.1716102378779E-15)) ;
#42565 = DIRECTION('center_axis',(-0.81649658092765,0.408248290464166,0.408248290463711)) ;
#42566 = DIRECTION('ref_axis',(-0.577350269189702,-0.577350269189929,-0.577350269189247)) ;
#42567 = DIRECTION('center_axis',(2.17161023787787E-15,-3.83420712807771E-28,
-1.)) ;
#42568 = DIRECTION('ref_axis',(-0.707106781186582,-0.707106781186513,-1.53556032529738E-15)) ;
#42569 = DIRECTION('center_axis',(-0.40824829046392,0.408248290464147,-0.816496580927556)) ;
#42570 = DIRECTION('ref_axis',(0.577350269189076,-0.577350269189986,-0.577350269189815)) ;
#42571 = DIRECTION('center_axis',(1.,-1.66533453692966E-16,2.1716102378779E-15)) ;
#42572 = DIRECTION('ref_axis',(1.65331725969831E-15,0.707106781186545,-0.70710678118655)) ;
#42573 = DIRECTION('center_axis',(1.,1.35627620245787E-13,-2.05796303467862E-28)) ;
#42574 = DIRECTION('ref_axis',(1.8852697114129E-28,-2.90739654573716E-15,
-1.)) ;
#42575 = DIRECTION('',(-1.,1.66533453692966E-16,-2.1716102378779E-15)) ;
#42576 = DIRECTION('center_axis',(-1.,-1.35627620245787E-13,2.05796303467862E-28)) ;
#42577 = DIRECTION('ref_axis',(-1.35627620245787E-13,1.,-2.90739654573716E-15)) ;
#42578 = DIRECTION('center_axis',(0.40824829046392,-0.408248290464147,-0.816496580927556)) ;
#42579 = DIRECTION('ref_axis',(-0.577350269189834,0.577350269189152,-0.577350269189891)) ;
#42580 = DIRECTION('center_axis',(2.17161023787787E-15,-3.83815143260382E-28,
-1.)) ;
#42581 = DIRECTION('ref_axis',(-0.707106781186656,0.707106781186439,-1.53556032529808E-15)) ;
#42582 = DIRECTION('center_axis',(-0.81649658092765,0.408248290464166,-0.408248290463711)) ;
#42583 = DIRECTION('ref_axis',(0.577350269189702,0.577350269189929,-0.577350269189247)) ;
#42584 = DIRECTION('center_axis',(-3.33066907386739E-16,-1.,3.66031460022645E-28)) ;
#42585 = DIRECTION('ref_axis',(-2.17161023787795E-15,3.66754751528624E-28,
1.)) ;
#42586 = DIRECTION('center_axis',(2.1716102378779E-15,-3.83815143260386E-28,
-1.)) ;
#42587 = DIRECTION('ref_axis',(1.,-1.66533453692941E-16,2.1716102378779E-15)) ;
#42588 = DIRECTION('center_axis',(2.1716102378779E-15,-3.83815143260386E-28,
-1.)) ;
#42589 = DIRECTION('ref_axis',(1.,-1.66533453692941E-16,2.1716102378779E-15)) ;
#42590 = DIRECTION('center_axis',(2.1716102378779E-15,-3.83815143260386E-28,
-1.)) ;
#42591 = DIRECTION('ref_axis',(1.,-1.66533453692941E-16,2.1716102378779E-15)) ;
#42592 = DIRECTION('',(-1.66533453692966E-16,-1.,3.83386399937507E-28)) ;
#42593 = DIRECTION('',(1.,-1.66533453692587E-16,2.1716102378779E-15)) ;
#42594 = DIRECTION('',(8.32667268460789E-17,1.,-3.83780830390118E-28)) ;
#42595 = DIRECTION('',(-1.,1.66533453692966E-16,-2.1716102378779E-15)) ;
#42596 = DIRECTION('center_axis',(-0.816496580927764,0.408248290464109,0.408248290463541)) ;
#42597 = DIRECTION('ref_axis',(-0.577350269189531,-0.577350269189986,-0.57735026918936)) ;
#42598 = DIRECTION('center_axis',(1.,1.35627620245787E-13,2.17161023787752E-15)) ;
#42599 = DIRECTION('ref_axis',(1.35627620245787E-13,-1.,2.90739654573778E-15)) ;
#42600 = DIRECTION('center_axis',(6.48092690624107E-15,1.,-2.90739654573747E-15)) ;
#42601 = DIRECTION('ref_axis',(2.17161023787792E-15,-2.90739654573748E-15,
-1.)) ;
#42602 = DIRECTION('center_axis',(2.1716102378779E-15,-3.83420712807775E-28,
-1.)) ;
#42603 = DIRECTION('ref_axis',(-0.70710678118651,-0.707106781186585,-1.53556032529724E-15)) ;
#42604 = DIRECTION('center_axis',(0.40824829046392,-0.408248290464147,-0.816496580927556)) ;
#42605 = DIRECTION('ref_axis',(-0.577350269189986,0.577350269189076,-0.577350269189815)) ;
#42606 = DIRECTION('center_axis',(-6.48092690624107E-15,-1.,2.90739654573747E-15)) ;
#42607 = DIRECTION('ref_axis',(-1.,6.48092690624106E-15,-2.17161023787794E-15)) ;
#42608 = DIRECTION('center_axis',(1.,1.35627620245787E-13,2.17161023787752E-15)) ;
#42609 = DIRECTION('ref_axis',(2.17161023787791E-15,-2.90739654573749E-15,
-1.)) ;
#42610 = DIRECTION('center_axis',(2.1716102378779E-15,-3.83815143260386E-28,
-1.)) ;
#42611 = DIRECTION('ref_axis',(-0.707106781186656,0.707106781186439,-1.5355603252981E-15)) ;
#42612 = DIRECTION('center_axis',(1.66533453692966E-16,1.,-3.83386399937507E-28)) ;
#42613 = DIRECTION('ref_axis',(-0.707106781186596,1.17756934400449E-16,-0.707106781186499)) ;
#42614 = DIRECTION('',(1.66533453692966E-16,1.,-3.83386399937507E-28)) ;
#42615 = DIRECTION('center_axis',(1.,-1.66533453692966E-16,2.1716102378779E-15)) ;
#42616 = DIRECTION('ref_axis',(1.65331725969841E-15,0.707106781186495,-0.7071067811866)) ;
#42617 = DIRECTION('center_axis',(1.,1.35627620245787E-13,2.17161023787752E-15)) ;
#42618 = DIRECTION('ref_axis',(-1.35627620245787E-13,1.,-2.90739654573778E-15)) ;
#42619 = DIRECTION('center_axis',(-1.,1.66533453692587E-16,-2.1716102378779E-15)) ;
#42620 = DIRECTION('ref_axis',(1.41780339089726E-15,-0.707106781186499,-0.707106781186596)) ;
#42621 = DIRECTION('',(-1.,1.66533453692587E-16,-2.1716102378779E-15)) ;
#42622 = DIRECTION('center_axis',(1.,1.35627620245787E-13,2.17161023787752E-15)) ;
#42623 = DIRECTION('ref_axis',(2.17161023787792E-15,-2.90739654573749E-15,
-1.)) ;
#42624 = DIRECTION('center_axis',(-8.32667268460789E-17,-1.,3.83780830390118E-28)) ;
#42625 = DIRECTION('ref_axis',(0.707106781186599,-5.8878467200346E-17,-0.707106781186496)) ;
#42626 = DIRECTION('center_axis',(-6.48092690624107E-15,-1.,2.90739654573747E-15)) ;
#42627 = DIRECTION('ref_axis',(1.,-6.48092690624106E-15,2.17161023787794E-15)) ;
#42628 = DIRECTION('center_axis',(6.48092690624107E-15,1.,-2.90739654573747E-15)) ;
#42629 = DIRECTION('ref_axis',(2.17161023787792E-15,-2.90739654573748E-15,
-1.)) ;
#42630 = DIRECTION('center_axis',(-0.408248290463939,0.408248290464166,-0.816496580927537)) ;
#42631 = DIRECTION('ref_axis',(0.577350269189076,-0.577350269189986,-0.577350269189815)) ;
#42632 = DIRECTION('center_axis',(0.408248290463948,-0.816496580927442,-0.408248290464346)) ;
#42633 = DIRECTION('ref_axis',(0.577350269189304,0.577350269189986,-0.577350269189588)) ;
#42634 = DIRECTION('center_axis',(-2.1716102378779E-15,3.66854633798134E-28,
1.)) ;
#42635 = DIRECTION('ref_axis',(0.707106781186452,0.707106781186643,1.53556032529713E-15)) ;
#42636 = DIRECTION('center_axis',(1.88526971141291E-28,-2.90739654573716E-15,
-1.)) ;
#42637 = DIRECTION('ref_axis',(-1.35627620245787E-13,1.,-2.90739654573716E-15)) ;
#42638 = DIRECTION('center_axis',(1.,-1.66533453692587E-16,2.1716102378779E-15)) ;
#42639 = DIRECTION('ref_axis',(1.41780339089714E-15,-0.70710678118655,-0.707106781186545)) ;
#42640 = DIRECTION('center_axis',(1.,1.35627620245787E-13,-2.05796303467862E-28)) ;
#42641 = DIRECTION('ref_axis',(1.35627620245787E-13,-1.,2.90739654573716E-15)) ;
#42642 = DIRECTION('',(-1.,1.66533453692587E-16,-2.1716102378779E-15)) ;
#42643 = DIRECTION('center_axis',(-1.,-1.35627620245747E-13,2.05796303467745E-28)) ;
#42644 = DIRECTION('ref_axis',(1.88526971141291E-28,-2.90739654573716E-15,
-1.)) ;
#42645 = DIRECTION('',(1.,-1.66533453692587E-16,2.1716102378779E-15)) ;
#42646 = DIRECTION('center_axis',(-1.,6.48092690624107E-15,-2.07369595641671E-28)) ;
#42647 = DIRECTION('ref_axis',(0.,-1.,0.)) ;
#42648 = DIRECTION('center_axis',(-1.,7.08071943160919E-13,-2.24717289282075E-27)) ;
#42649 = DIRECTION('ref_axis',(-1.88526971141296E-28,2.90739654573716E-15,
1.)) ;
#42650 = DIRECTION('center_axis',(6.48092690624107E-15,1.,-2.90739654573716E-15)) ;
#42651 = DIRECTION('ref_axis',(1.,-6.48092690624107E-15,2.07369595641671E-28)) ;
#42652 = DIRECTION('center_axis',(-1.66533453692966E-16,-1.,3.83386399937507E-28)) ;
#42653 = DIRECTION('ref_axis',(0.707106781186648,-1.17756934401E-16,-0.707106781186447)) ;
#42654 = DIRECTION('center_axis',(-6.48092690624107E-15,-1.,2.90739654573716E-15)) ;
#42655 = DIRECTION('ref_axis',(1.88526971141291E-28,-2.90739654573716E-15,
-1.)) ;
#42656 = DIRECTION('',(1.66533453692966E-16,1.,-3.83386399937507E-28)) ;
#42657 = DIRECTION('center_axis',(1.,-6.48092690624107E-15,2.07369595641671E-28)) ;
#42658 = DIRECTION('ref_axis',(0.,1.,0.)) ;
#42659 = DIRECTION('center_axis',(1.,-1.48589474058271E-13,-5.59482469102492E-13)) ;
#42660 = DIRECTION('ref_axis',(-1.48589474058269E-13,-1.,2.90739654573716E-15)) ;
#42661 = DIRECTION('center_axis',(6.48092690624107E-15,1.,-2.90739654573716E-15)) ;
#42662 = DIRECTION('ref_axis',(1.88526971141291E-28,-2.90739654573716E-15,
-1.)) ;
#42663 = DIRECTION('center_axis',(-1.,6.48092690624107E-15,-2.07369595641671E-28)) ;
#42664 = DIRECTION('ref_axis',(0.,-1.,0.)) ;
#42665 = DIRECTION('center_axis',(-1.,1.48589474058269E-13,-6.20535494751205E-28)) ;
#42666 = DIRECTION('ref_axis',(1.48589474058269E-13,1.,-2.90739654573716E-15)) ;
#42667 = DIRECTION('center_axis',(-6.48092690624107E-15,-1.,2.90739654573716E-15)) ;
#42668 = DIRECTION('ref_axis',(1.88526971141291E-28,-2.90739654573716E-15,
-1.)) ;
#42669 = DIRECTION('center_axis',(1.88526971141291E-28,-2.90739654573716E-15,
-1.)) ;
#42670 = DIRECTION('ref_axis',(1.,-6.48092690624108E-15,2.07369595641671E-28)) ;
#42671 = DIRECTION('center_axis',(2.1716102378779E-15,-3.66854633798134E-28,
-1.)) ;
#42672 = DIRECTION('ref_axis',(0.707106781186543,-0.707106781186552,1.53556032529784E-15)) ;
#42673 = DIRECTION('',(2.1716102378779E-15,-3.66854633798134E-28,-1.)) ;
#42674 = DIRECTION('center_axis',(-1.66533453692966E-16,-1.,3.83386399937507E-28)) ;
#42675 = DIRECTION('ref_axis',(0.707106781186648,-1.17756934401E-16,-0.707106781186447)) ;
#42676 = DIRECTION('center_axis',(6.48092690628146E-15,1.,-2.90739654573716E-15)) ;
#42677 = DIRECTION('ref_axis',(1.,-6.48092690628146E-15,2.07369595641789E-28)) ;
#42678 = DIRECTION('',(1.66533453692966E-16,1.,-3.83386399937507E-28)) ;
#42679 = DIRECTION('center_axis',(1.,-6.48092690624107E-15,2.07369595641671E-28)) ;
#42680 = DIRECTION('ref_axis',(0.,1.,0.)) ;
#42681 = DIRECTION('center_axis',(1.,-1.48589474058269E-13,6.20535494751205E-28)) ;
#42682 = DIRECTION('ref_axis',(-1.88526971141292E-28,2.90739654573716E-15,
1.)) ;
#42683 = DIRECTION('center_axis',(-6.48092690624107E-15,-1.,2.90739654573716E-15)) ;
#42684 = DIRECTION('ref_axis',(-1.,6.48092690624107E-15,-2.07369595641671E-28)) ;
#42685 = DIRECTION('center_axis',(8.32667268460789E-17,1.,-3.83780830390118E-28)) ;
#42686 = DIRECTION('ref_axis',(-0.707106781186447,5.88784671997906E-17,-0.707106781186648)) ;
#42687 = DIRECTION('center_axis',(6.48092690624107E-15,1.,-2.90739654573716E-15)) ;
#42688 = DIRECTION('ref_axis',(1.88526971141291E-28,-2.90739654573716E-15,
-1.)) ;
#42689 = DIRECTION('',(-8.32667268460789E-17,-1.,3.83780830390118E-28)) ;
#42690 = DIRECTION('center_axis',(-1.,3.33066907386739E-16,-2.1716102378779E-15)) ;
#42691 = DIRECTION('ref_axis',(-1.30004645649559E-15,0.70710678118655,0.707106781186545)) ;
#42692 = DIRECTION('',(-1.,3.33066907386739E-16,-2.1716102378779E-15)) ;
#42693 = DIRECTION('',(1.,-3.33066907386739E-16,2.1716102378779E-15)) ;
#42694 = DIRECTION('center_axis',(8.32667268460789E-17,1.,-3.83780830390118E-28)) ;
#42695 = DIRECTION('ref_axis',(-0.707106781186447,5.88784671997906E-17,-0.707106781186648)) ;
#42696 = DIRECTION('center_axis',(-6.48092690624107E-15,-1.,2.90739654573716E-15)) ;
#42697 = DIRECTION('ref_axis',(-1.,6.48092690624107E-15,-2.07369595641671E-28)) ;
#42698 = DIRECTION('',(-8.32667268460789E-17,-1.,3.83780830390118E-28)) ;
#42699 = DIRECTION('center_axis',(1.,-3.33066907386739E-16,2.1716102378779E-15)) ;
#42700 = DIRECTION('ref_axis',(-1.77107419409959E-15,-0.707106781186545,0.70710678118655)) ;
#42701 = DIRECTION('',(1.,-3.33066907386739E-16,2.1716102378779E-15)) ;
#42702 = DIRECTION('center_axis',(-0.81649658092765,0.408248290464166,0.408248290463711)) ;
#42703 = DIRECTION('ref_axis',(-0.577350269189702,-0.577350269189929,-0.577350269189247)) ;
#42704 = DIRECTION('center_axis',(2.17161023787787E-15,-3.83420712807771E-28,
-1.)) ;
#42705 = DIRECTION('ref_axis',(-0.707106781186582,-0.707106781186513,-1.53556032529738E-15)) ;
#42706 = DIRECTION('center_axis',(-0.40824829046392,0.408248290464147,-0.816496580927556)) ;
#42707 = DIRECTION('ref_axis',(0.577350269189076,-0.577350269189986,-0.577350269189815)) ;
#42708 = DIRECTION('center_axis',(1.,-1.66533453692966E-16,2.1716102378779E-15)) ;
#42709 = DIRECTION('ref_axis',(1.65331725969831E-15,0.707106781186545,-0.70710678118655)) ;
#42710 = DIRECTION('center_axis',(1.,1.35627620245787E-13,-2.05796303467862E-28)) ;
#42711 = DIRECTION('ref_axis',(1.8852697114129E-28,-2.90739654573716E-15,
-1.)) ;
#42712 = DIRECTION('',(-1.,1.66533453692966E-16,-2.1716102378779E-15)) ;
#42713 = DIRECTION('center_axis',(-1.,-1.35627620245787E-13,2.05796303467862E-28)) ;
#42714 = DIRECTION('ref_axis',(-1.35627620245787E-13,1.,-2.90739654573716E-15)) ;
#42715 = DIRECTION('center_axis',(0.40824829046392,-0.408248290464147,-0.816496580927556)) ;
#42716 = DIRECTION('ref_axis',(-0.577350269189834,0.577350269189152,-0.577350269189891)) ;
#42717 = DIRECTION('center_axis',(2.17161023787787E-15,-3.83815143260382E-28,
-1.)) ;
#42718 = DIRECTION('ref_axis',(-0.707106781186656,0.707106781186439,-1.53556032529808E-15)) ;
#42719 = DIRECTION('center_axis',(-0.81649658092765,0.408248290464166,-0.408248290463711)) ;
#42720 = DIRECTION('ref_axis',(0.577350269189702,0.577350269189929,-0.577350269189247)) ;
#42721 = DIRECTION('center_axis',(-3.33066907386739E-16,-1.,3.66031460022645E-28)) ;
#42722 = DIRECTION('ref_axis',(-2.17161023787795E-15,3.66754751528624E-28,
1.)) ;
#42723 = DIRECTION('center_axis',(2.1716102378779E-15,-3.83815143260386E-28,
-1.)) ;
#42724 = DIRECTION('ref_axis',(1.,-1.66533453692941E-16,2.1716102378779E-15)) ;
#42725 = DIRECTION('center_axis',(2.1716102378779E-15,-3.83815143260386E-28,
-1.)) ;
#42726 = DIRECTION('ref_axis',(1.,-1.66533453692941E-16,2.1716102378779E-15)) ;
#42727 = DIRECTION('center_axis',(2.1716102378779E-15,-3.83815143260386E-28,
-1.)) ;
#42728 = DIRECTION('ref_axis',(1.,-1.66533453692941E-16,2.1716102378779E-15)) ;
#42729 = DIRECTION('',(-1.66533453692966E-16,-1.,3.83386399937507E-28)) ;
#42730 = DIRECTION('',(1.,-1.66533453692587E-16,2.1716102378779E-15)) ;
#42731 = DIRECTION('',(8.32667268460789E-17,1.,-3.83780830390118E-28)) ;
#42732 = DIRECTION('',(-1.,1.66533453692966E-16,-2.1716102378779E-15)) ;
#42733 = DIRECTION('center_axis',(-0.816496580927764,0.408248290464109,0.408248290463541)) ;
#42734 = DIRECTION('ref_axis',(-0.577350269189531,-0.577350269189986,-0.57735026918936)) ;
#42735 = DIRECTION('center_axis',(1.,1.35627620245787E-13,2.17161023787752E-15)) ;
#42736 = DIRECTION('ref_axis',(1.35627620245787E-13,-1.,2.90739654573778E-15)) ;
#42737 = DIRECTION('center_axis',(6.48092690624107E-15,1.,-2.90739654573747E-15)) ;
#42738 = DIRECTION('ref_axis',(2.17161023787792E-15,-2.90739654573748E-15,
-1.)) ;
#42739 = DIRECTION('center_axis',(2.1716102378779E-15,-3.83420712807775E-28,
-1.)) ;
#42740 = DIRECTION('ref_axis',(-0.70710678118651,-0.707106781186585,-1.53556032529724E-15)) ;
#42741 = DIRECTION('center_axis',(0.40824829046392,-0.408248290464147,-0.816496580927556)) ;
#42742 = DIRECTION('ref_axis',(-0.577350269189986,0.577350269189076,-0.577350269189815)) ;
#42743 = DIRECTION('center_axis',(-6.48092690624107E-15,-1.,2.90739654573747E-15)) ;
#42744 = DIRECTION('ref_axis',(-1.,6.48092690624106E-15,-2.17161023787794E-15)) ;
#42745 = DIRECTION('center_axis',(1.,1.35627620245787E-13,2.17161023787752E-15)) ;
#42746 = DIRECTION('ref_axis',(2.17161023787791E-15,-2.90739654573749E-15,
-1.)) ;
#42747 = DIRECTION('center_axis',(2.1716102378779E-15,-3.83815143260386E-28,
-1.)) ;
#42748 = DIRECTION('ref_axis',(-0.707106781186656,0.707106781186439,-1.5355603252981E-15)) ;
#42749 = DIRECTION('center_axis',(1.66533453692966E-16,1.,-3.83386399937507E-28)) ;
#42750 = DIRECTION('ref_axis',(-0.707106781186596,1.17756934400449E-16,-0.707106781186499)) ;
#42751 = DIRECTION('',(1.66533453692966E-16,1.,-3.83386399937507E-28)) ;
#42752 = DIRECTION('center_axis',(1.,-1.66533453692966E-16,2.1716102378779E-15)) ;
#42753 = DIRECTION('ref_axis',(1.65331725969841E-15,0.707106781186495,-0.7071067811866)) ;
#42754 = DIRECTION('center_axis',(1.,1.35627620245787E-13,2.17161023787752E-15)) ;
#42755 = DIRECTION('ref_axis',(-1.35627620245787E-13,1.,-2.90739654573778E-15)) ;
#42756 = DIRECTION('center_axis',(-1.,1.66533453692587E-16,-2.1716102378779E-15)) ;
#42757 = DIRECTION('ref_axis',(1.41780339089726E-15,-0.707106781186499,-0.707106781186596)) ;
#42758 = DIRECTION('',(-1.,1.66533453692587E-16,-2.1716102378779E-15)) ;
#42759 = DIRECTION('center_axis',(1.,1.35627620245787E-13,2.17161023787752E-15)) ;
#42760 = DIRECTION('ref_axis',(2.17161023787792E-15,-2.90739654573749E-15,
-1.)) ;
#42761 = DIRECTION('center_axis',(-8.32667268460789E-17,-1.,3.83780830390118E-28)) ;
#42762 = DIRECTION('ref_axis',(0.707106781186599,-5.8878467200346E-17,-0.707106781186496)) ;
#42763 = DIRECTION('center_axis',(-6.48092690624107E-15,-1.,2.90739654573747E-15)) ;
#42764 = DIRECTION('ref_axis',(1.,-6.48092690624106E-15,2.17161023787794E-15)) ;
#42765 = DIRECTION('center_axis',(6.48092690624107E-15,1.,-2.90739654573747E-15)) ;
#42766 = DIRECTION('ref_axis',(2.17161023787792E-15,-2.90739654573748E-15,
-1.)) ;
#42767 = DIRECTION('center_axis',(-0.408248290463939,0.408248290464166,-0.816496580927537)) ;
#42768 = DIRECTION('ref_axis',(0.577350269189076,-0.577350269189986,-0.577350269189815)) ;
#42769 = DIRECTION('center_axis',(0.408248290463948,-0.816496580927442,-0.408248290464346)) ;
#42770 = DIRECTION('ref_axis',(0.577350269189304,0.577350269189986,-0.577350269189588)) ;
#42771 = DIRECTION('center_axis',(-2.1716102378779E-15,3.66854633798134E-28,
1.)) ;
#42772 = DIRECTION('ref_axis',(0.707106781186452,0.707106781186643,1.53556032529713E-15)) ;
#42773 = DIRECTION('center_axis',(1.88526971141291E-28,-2.90739654573716E-15,
-1.)) ;
#42774 = DIRECTION('ref_axis',(-1.35627620245787E-13,1.,-2.90739654573716E-15)) ;
#42775 = DIRECTION('center_axis',(1.,-1.66533453692587E-16,2.1716102378779E-15)) ;
#42776 = DIRECTION('ref_axis',(1.41780339089714E-15,-0.70710678118655,-0.707106781186545)) ;
#42777 = DIRECTION('center_axis',(1.,1.35627620245787E-13,-2.05796303467862E-28)) ;
#42778 = DIRECTION('ref_axis',(1.35627620245787E-13,-1.,2.90739654573716E-15)) ;
#42779 = DIRECTION('',(-1.,1.66533453692587E-16,-2.1716102378779E-15)) ;
#42780 = DIRECTION('center_axis',(-1.,-1.35627620245747E-13,2.05796303467745E-28)) ;
#42781 = DIRECTION('ref_axis',(1.88526971141291E-28,-2.90739654573716E-15,
-1.)) ;
#42782 = DIRECTION('',(1.,-1.66533453692587E-16,2.1716102378779E-15)) ;
#42783 = DIRECTION('center_axis',(-1.,6.48092690624107E-15,-2.07369595641671E-28)) ;
#42784 = DIRECTION('ref_axis',(0.,-1.,0.)) ;
#42785 = DIRECTION('center_axis',(-1.,7.08071943160919E-13,-2.24717289282075E-27)) ;
#42786 = DIRECTION('ref_axis',(-1.88526971141296E-28,2.90739654573716E-15,
1.)) ;
#42787 = DIRECTION('center_axis',(6.48092690624107E-15,1.,-2.90739654573716E-15)) ;
#42788 = DIRECTION('ref_axis',(1.,-6.48092690624107E-15,2.07369595641671E-28)) ;
#42789 = DIRECTION('center_axis',(-1.66533453692966E-16,-1.,3.83386399937507E-28)) ;
#42790 = DIRECTION('ref_axis',(0.707106781186648,-1.17756934401E-16,-0.707106781186447)) ;
#42791 = DIRECTION('center_axis',(-6.48092690624107E-15,-1.,2.90739654573716E-15)) ;
#42792 = DIRECTION('ref_axis',(1.88526971141291E-28,-2.90739654573716E-15,
-1.)) ;
#42793 = DIRECTION('',(1.66533453692966E-16,1.,-3.83386399937507E-28)) ;
#42794 = DIRECTION('center_axis',(1.,-6.48092690624107E-15,2.07369595641671E-28)) ;
#42795 = DIRECTION('ref_axis',(0.,1.,0.)) ;
#42796 = DIRECTION('center_axis',(1.,-1.48589474058271E-13,-5.59482469102492E-13)) ;
#42797 = DIRECTION('ref_axis',(-1.48589474058269E-13,-1.,2.90739654573716E-15)) ;
#42798 = DIRECTION('center_axis',(6.48092690624107E-15,1.,-2.90739654573716E-15)) ;
#42799 = DIRECTION('ref_axis',(1.88526971141291E-28,-2.90739654573716E-15,
-1.)) ;
#42800 = DIRECTION('center_axis',(-1.,6.48092690624107E-15,-2.07369595641671E-28)) ;
#42801 = DIRECTION('ref_axis',(0.,-1.,0.)) ;
#42802 = DIRECTION('center_axis',(-1.,1.48589474058269E-13,-6.20535494751205E-28)) ;
#42803 = DIRECTION('ref_axis',(1.48589474058269E-13,1.,-2.90739654573716E-15)) ;
#42804 = DIRECTION('center_axis',(-6.48092690624107E-15,-1.,2.90739654573716E-15)) ;
#42805 = DIRECTION('ref_axis',(1.88526971141291E-28,-2.90739654573716E-15,
-1.)) ;
#42806 = DIRECTION('center_axis',(1.88526971141291E-28,-2.90739654573716E-15,
-1.)) ;
#42807 = DIRECTION('ref_axis',(1.,-6.48092690624108E-15,2.07369595641671E-28)) ;
#42808 = DIRECTION('center_axis',(2.1716102378779E-15,-3.66854633798134E-28,
-1.)) ;
#42809 = DIRECTION('ref_axis',(0.707106781186543,-0.707106781186552,1.53556032529784E-15)) ;
#42810 = DIRECTION('',(2.1716102378779E-15,-3.66854633798134E-28,-1.)) ;
#42811 = DIRECTION('center_axis',(-1.66533453692966E-16,-1.,3.83386399937507E-28)) ;
#42812 = DIRECTION('ref_axis',(0.707106781186648,-1.17756934401E-16,-0.707106781186447)) ;
#42813 = DIRECTION('center_axis',(6.48092690628146E-15,1.,-2.90739654573716E-15)) ;
#42814 = DIRECTION('ref_axis',(1.,-6.48092690628146E-15,2.07369595641789E-28)) ;
#42815 = DIRECTION('',(1.66533453692966E-16,1.,-3.83386399937507E-28)) ;
#42816 = DIRECTION('center_axis',(1.,-6.48092690624107E-15,2.07369595641671E-28)) ;
#42817 = DIRECTION('ref_axis',(0.,1.,0.)) ;
#42818 = DIRECTION('center_axis',(1.,-1.48589474058269E-13,6.20535494751205E-28)) ;
#42819 = DIRECTION('ref_axis',(-1.88526971141292E-28,2.90739654573716E-15,
1.)) ;
#42820 = DIRECTION('center_axis',(-6.48092690624107E-15,-1.,2.90739654573716E-15)) ;
#42821 = DIRECTION('ref_axis',(-1.,6.48092690624107E-15,-2.07369595641671E-28)) ;
#42822 = DIRECTION('center_axis',(8.32667268460789E-17,1.,-3.83780830390118E-28)) ;
#42823 = DIRECTION('ref_axis',(-0.707106781186447,5.88784671997906E-17,-0.707106781186648)) ;
#42824 = DIRECTION('center_axis',(6.48092690624107E-15,1.,-2.90739654573716E-15)) ;
#42825 = DIRECTION('ref_axis',(1.88526971141291E-28,-2.90739654573716E-15,
-1.)) ;
#42826 = DIRECTION('',(-8.32667268460789E-17,-1.,3.83780830390118E-28)) ;
#42827 = DIRECTION('center_axis',(-1.,3.33066907386739E-16,-2.1716102378779E-15)) ;
#42828 = DIRECTION('ref_axis',(-1.30004645649559E-15,0.70710678118655,0.707106781186545)) ;
#42829 = DIRECTION('',(-1.,3.33066907386739E-16,-2.1716102378779E-15)) ;
#42830 = DIRECTION('',(1.,-3.33066907386739E-16,2.1716102378779E-15)) ;
#42831 = DIRECTION('center_axis',(8.32667268460789E-17,1.,-3.83780830390118E-28)) ;
#42832 = DIRECTION('ref_axis',(-0.707106781186447,5.88784671997906E-17,-0.707106781186648)) ;
#42833 = DIRECTION('center_axis',(-6.48092690624107E-15,-1.,2.90739654573716E-15)) ;
#42834 = DIRECTION('ref_axis',(-1.,6.48092690624107E-15,-2.07369595641671E-28)) ;
#42835 = DIRECTION('',(-8.32667268460789E-17,-1.,3.83780830390118E-28)) ;
#42836 = DIRECTION('center_axis',(1.,-3.33066907386739E-16,2.1716102378779E-15)) ;
#42837 = DIRECTION('ref_axis',(-1.77107419409959E-15,-0.707106781186545,0.70710678118655)) ;
#42838 = DIRECTION('',(1.,-3.33066907386739E-16,2.1716102378779E-15)) ;
#42839 = DIRECTION('center_axis',(-0.81649658092765,0.408248290464166,0.408248290463711)) ;
#42840 = DIRECTION('ref_axis',(-0.577350269189702,-0.577350269189929,-0.577350269189247)) ;
#42841 = DIRECTION('center_axis',(2.17161023787787E-15,-3.83420712807771E-28,
-1.)) ;
#42842 = DIRECTION('ref_axis',(-0.707106781186582,-0.707106781186513,-1.53556032529738E-15)) ;
#42843 = DIRECTION('center_axis',(-0.40824829046392,0.408248290464147,-0.816496580927556)) ;
#42844 = DIRECTION('ref_axis',(0.577350269189076,-0.577350269189986,-0.577350269189815)) ;
#42845 = DIRECTION('center_axis',(1.,-1.66533453692966E-16,2.1716102378779E-15)) ;
#42846 = DIRECTION('ref_axis',(1.65331725969831E-15,0.707106781186545,-0.70710678118655)) ;
#42847 = DIRECTION('center_axis',(1.,1.35627620245787E-13,-2.05796303467862E-28)) ;
#42848 = DIRECTION('ref_axis',(1.8852697114129E-28,-2.90739654573716E-15,
-1.)) ;
#42849 = DIRECTION('',(-1.,1.66533453692966E-16,-2.1716102378779E-15)) ;
#42850 = DIRECTION('center_axis',(-1.,-1.35627620245787E-13,2.05796303467862E-28)) ;
#42851 = DIRECTION('ref_axis',(-1.35627620245787E-13,1.,-2.90739654573716E-15)) ;
#42852 = DIRECTION('center_axis',(0.40824829046392,-0.408248290464147,-0.816496580927556)) ;
#42853 = DIRECTION('ref_axis',(-0.577350269189834,0.577350269189152,-0.577350269189891)) ;
#42854 = DIRECTION('center_axis',(2.17161023787787E-15,-3.83815143260382E-28,
-1.)) ;
#42855 = DIRECTION('ref_axis',(-0.707106781186656,0.707106781186439,-1.53556032529808E-15)) ;
#42856 = DIRECTION('center_axis',(-0.81649658092765,0.408248290464166,-0.408248290463711)) ;
#42857 = DIRECTION('ref_axis',(0.577350269189702,0.577350269189929,-0.577350269189247)) ;
#42858 = DIRECTION('center_axis',(-3.33066907386739E-16,-1.,3.66031460022645E-28)) ;
#42859 = DIRECTION('ref_axis',(-2.17161023787795E-15,3.66754751528624E-28,
1.)) ;
#42860 = DIRECTION('center_axis',(2.1716102378779E-15,-3.83815143260386E-28,
-1.)) ;
#42861 = DIRECTION('ref_axis',(1.,-1.66533453692941E-16,2.1716102378779E-15)) ;
#42862 = DIRECTION('center_axis',(2.1716102378779E-15,-3.83815143260386E-28,
-1.)) ;
#42863 = DIRECTION('ref_axis',(1.,-1.66533453692941E-16,2.1716102378779E-15)) ;
#42864 = DIRECTION('center_axis',(2.1716102378779E-15,-3.83815143260386E-28,
-1.)) ;
#42865 = DIRECTION('ref_axis',(1.,-1.66533453692941E-16,2.1716102378779E-15)) ;
#42866 = DIRECTION('',(-1.66533453692966E-16,-1.,3.83386399937507E-28)) ;
#42867 = DIRECTION('',(1.,-1.66533453692587E-16,2.1716102378779E-15)) ;
#42868 = DIRECTION('',(8.32667268460789E-17,1.,-3.83780830390118E-28)) ;
#42869 = DIRECTION('',(-1.,1.66533453692966E-16,-2.1716102378779E-15)) ;
#42870 = DIRECTION('center_axis',(-0.816496580927764,0.408248290464109,0.408248290463541)) ;
#42871 = DIRECTION('ref_axis',(-0.577350269189531,-0.577350269189986,-0.57735026918936)) ;
#42872 = DIRECTION('center_axis',(1.,1.35627620245787E-13,2.17161023787752E-15)) ;
#42873 = DIRECTION('ref_axis',(1.35627620245787E-13,-1.,2.90739654573778E-15)) ;
#42874 = DIRECTION('center_axis',(6.48092690624107E-15,1.,-2.90739654573747E-15)) ;
#42875 = DIRECTION('ref_axis',(2.17161023787792E-15,-2.90739654573748E-15,
-1.)) ;
#42876 = DIRECTION('center_axis',(2.1716102378779E-15,-3.83420712807775E-28,
-1.)) ;
#42877 = DIRECTION('ref_axis',(-0.70710678118651,-0.707106781186585,-1.53556032529724E-15)) ;
#42878 = DIRECTION('center_axis',(0.40824829046392,-0.408248290464147,-0.816496580927556)) ;
#42879 = DIRECTION('ref_axis',(-0.577350269189986,0.577350269189076,-0.577350269189815)) ;
#42880 = DIRECTION('center_axis',(-6.48092690624107E-15,-1.,2.90739654573747E-15)) ;
#42881 = DIRECTION('ref_axis',(-1.,6.48092690624106E-15,-2.17161023787794E-15)) ;
#42882 = DIRECTION('center_axis',(1.,1.35627620245787E-13,2.17161023787752E-15)) ;
#42883 = DIRECTION('ref_axis',(2.17161023787791E-15,-2.90739654573749E-15,
-1.)) ;
#42884 = DIRECTION('center_axis',(2.1716102378779E-15,-3.83815143260386E-28,
-1.)) ;
#42885 = DIRECTION('ref_axis',(-0.707106781186656,0.707106781186439,-1.5355603252981E-15)) ;
#42886 = DIRECTION('center_axis',(1.66533453692966E-16,1.,-3.83386399937507E-28)) ;
#42887 = DIRECTION('ref_axis',(-0.707106781186596,1.17756934400449E-16,-0.707106781186499)) ;
#42888 = DIRECTION('',(1.66533453692966E-16,1.,-3.83386399937507E-28)) ;
#42889 = DIRECTION('center_axis',(1.,-1.66533453692966E-16,2.1716102378779E-15)) ;
#42890 = DIRECTION('ref_axis',(1.65331725969841E-15,0.707106781186495,-0.7071067811866)) ;
#42891 = DIRECTION('center_axis',(1.,1.35627620245787E-13,2.17161023787752E-15)) ;
#42892 = DIRECTION('ref_axis',(-1.35627620245787E-13,1.,-2.90739654573778E-15)) ;
#42893 = DIRECTION('center_axis',(-1.,1.66533453692587E-16,-2.1716102378779E-15)) ;
#42894 = DIRECTION('ref_axis',(1.41780339089726E-15,-0.707106781186499,-0.707106781186596)) ;
#42895 = DIRECTION('',(-1.,1.66533453692587E-16,-2.1716102378779E-15)) ;
#42896 = DIRECTION('center_axis',(1.,1.35627620245787E-13,2.17161023787752E-15)) ;
#42897 = DIRECTION('ref_axis',(2.17161023787792E-15,-2.90739654573749E-15,
-1.)) ;
#42898 = DIRECTION('center_axis',(-8.32667268460789E-17,-1.,3.83780830390118E-28)) ;
#42899 = DIRECTION('ref_axis',(0.707106781186599,-5.8878467200346E-17,-0.707106781186496)) ;
#42900 = DIRECTION('center_axis',(-6.48092690624107E-15,-1.,2.90739654573747E-15)) ;
#42901 = DIRECTION('ref_axis',(1.,-6.48092690624106E-15,2.17161023787794E-15)) ;
#42902 = DIRECTION('center_axis',(6.48092690624107E-15,1.,-2.90739654573747E-15)) ;
#42903 = DIRECTION('ref_axis',(2.17161023787792E-15,-2.90739654573748E-15,
-1.)) ;
#42904 = DIRECTION('center_axis',(-0.408248290463939,0.408248290464166,-0.816496580927537)) ;
#42905 = DIRECTION('ref_axis',(0.577350269189076,-0.577350269189986,-0.577350269189815)) ;
#42906 = DIRECTION('center_axis',(0.408248290463948,-0.816496580927442,-0.408248290464346)) ;
#42907 = DIRECTION('ref_axis',(0.577350269189304,0.577350269189986,-0.577350269189588)) ;
#42908 = DIRECTION('center_axis',(-2.1716102378779E-15,3.66854633798134E-28,
1.)) ;
#42909 = DIRECTION('ref_axis',(0.707106781186452,0.707106781186643,1.53556032529713E-15)) ;
#42910 = DIRECTION('center_axis',(1.88526971141291E-28,-2.90739654573716E-15,
-1.)) ;
#42911 = DIRECTION('ref_axis',(-1.35627620245787E-13,1.,-2.90739654573716E-15)) ;
#42912 = DIRECTION('center_axis',(1.,-1.66533453692587E-16,2.1716102378779E-15)) ;
#42913 = DIRECTION('ref_axis',(1.41780339089714E-15,-0.70710678118655,-0.707106781186545)) ;
#42914 = DIRECTION('center_axis',(1.,1.35627620245787E-13,-2.05796303467862E-28)) ;
#42915 = DIRECTION('ref_axis',(1.35627620245787E-13,-1.,2.90739654573716E-15)) ;
#42916 = DIRECTION('',(-1.,1.66533453692587E-16,-2.1716102378779E-15)) ;
#42917 = DIRECTION('center_axis',(-1.,-1.35627620245747E-13,2.05796303467745E-28)) ;
#42918 = DIRECTION('ref_axis',(1.88526971141291E-28,-2.90739654573716E-15,
-1.)) ;
#42919 = DIRECTION('',(1.,-1.66533453692587E-16,2.1716102378779E-15)) ;
#42920 = DIRECTION('center_axis',(-1.,6.48092690624107E-15,-2.07369595641671E-28)) ;
#42921 = DIRECTION('ref_axis',(0.,-1.,0.)) ;
#42922 = DIRECTION('center_axis',(-1.,7.08071943160919E-13,-2.24717289282075E-27)) ;
#42923 = DIRECTION('ref_axis',(-1.88526971141296E-28,2.90739654573716E-15,
1.)) ;
#42924 = DIRECTION('center_axis',(6.48092690624107E-15,1.,-2.90739654573716E-15)) ;
#42925 = DIRECTION('ref_axis',(1.,-6.48092690624107E-15,2.07369595641671E-28)) ;
#42926 = DIRECTION('center_axis',(-1.66533453692966E-16,-1.,3.83386399937507E-28)) ;
#42927 = DIRECTION('ref_axis',(0.707106781186648,-1.17756934401E-16,-0.707106781186447)) ;
#42928 = DIRECTION('center_axis',(-6.48092690624107E-15,-1.,2.90739654573716E-15)) ;
#42929 = DIRECTION('ref_axis',(1.88526971141291E-28,-2.90739654573716E-15,
-1.)) ;
#42930 = DIRECTION('',(1.66533453692966E-16,1.,-3.83386399937507E-28)) ;
#42931 = DIRECTION('center_axis',(1.,-6.48092690624107E-15,2.07369595641671E-28)) ;
#42932 = DIRECTION('ref_axis',(0.,1.,0.)) ;
#42933 = DIRECTION('center_axis',(1.,-1.48589474058271E-13,-5.59482469102492E-13)) ;
#42934 = DIRECTION('ref_axis',(-1.48589474058269E-13,-1.,2.90739654573716E-15)) ;
#42935 = DIRECTION('center_axis',(6.48092690624107E-15,1.,-2.90739654573716E-15)) ;
#42936 = DIRECTION('ref_axis',(1.88526971141291E-28,-2.90739654573716E-15,
-1.)) ;
#42937 = DIRECTION('center_axis',(-1.,6.48092690624107E-15,-2.07369595641671E-28)) ;
#42938 = DIRECTION('ref_axis',(0.,-1.,0.)) ;
#42939 = DIRECTION('center_axis',(-1.,1.48589474058269E-13,-6.20535494751205E-28)) ;
#42940 = DIRECTION('ref_axis',(1.48589474058269E-13,1.,-2.90739654573716E-15)) ;
#42941 = DIRECTION('center_axis',(-6.48092690624107E-15,-1.,2.90739654573716E-15)) ;
#42942 = DIRECTION('ref_axis',(1.88526971141291E-28,-2.90739654573716E-15,
-1.)) ;
#42943 = DIRECTION('center_axis',(1.88526971141291E-28,-2.90739654573716E-15,
-1.)) ;
#42944 = DIRECTION('ref_axis',(1.,-6.48092690624108E-15,2.07369595641671E-28)) ;
#42945 = DIRECTION('center_axis',(2.1716102378779E-15,-3.66854633798134E-28,
-1.)) ;
#42946 = DIRECTION('ref_axis',(0.707106781186543,-0.707106781186552,1.53556032529784E-15)) ;
#42947 = DIRECTION('',(2.1716102378779E-15,-3.66854633798134E-28,-1.)) ;
#42948 = DIRECTION('center_axis',(-1.66533453692966E-16,-1.,3.83386399937507E-28)) ;
#42949 = DIRECTION('ref_axis',(0.707106781186648,-1.17756934401E-16,-0.707106781186447)) ;
#42950 = DIRECTION('center_axis',(6.48092690628146E-15,1.,-2.90739654573716E-15)) ;
#42951 = DIRECTION('ref_axis',(1.,-6.48092690628146E-15,2.07369595641789E-28)) ;
#42952 = DIRECTION('',(1.66533453692966E-16,1.,-3.83386399937507E-28)) ;
#42953 = DIRECTION('center_axis',(1.,-6.48092690624107E-15,2.07369595641671E-28)) ;
#42954 = DIRECTION('ref_axis',(0.,1.,0.)) ;
#42955 = DIRECTION('center_axis',(1.,-1.48589474058269E-13,6.20535494751205E-28)) ;
#42956 = DIRECTION('ref_axis',(-1.88526971141292E-28,2.90739654573716E-15,
1.)) ;
#42957 = DIRECTION('center_axis',(-6.48092690624107E-15,-1.,2.90739654573716E-15)) ;
#42958 = DIRECTION('ref_axis',(-1.,6.48092690624107E-15,-2.07369595641671E-28)) ;
#42959 = DIRECTION('center_axis',(8.32667268460789E-17,1.,-3.83780830390118E-28)) ;
#42960 = DIRECTION('ref_axis',(-0.707106781186447,5.88784671997906E-17,-0.707106781186648)) ;
#42961 = DIRECTION('center_axis',(6.48092690624107E-15,1.,-2.90739654573716E-15)) ;
#42962 = DIRECTION('ref_axis',(1.88526971141291E-28,-2.90739654573716E-15,
-1.)) ;
#42963 = DIRECTION('',(-8.32667268460789E-17,-1.,3.83780830390118E-28)) ;
#42964 = DIRECTION('center_axis',(-1.,3.33066907386739E-16,-2.1716102378779E-15)) ;
#42965 = DIRECTION('ref_axis',(-1.30004645649559E-15,0.70710678118655,0.707106781186545)) ;
#42966 = DIRECTION('',(-1.,3.33066907386739E-16,-2.1716102378779E-15)) ;
#42967 = DIRECTION('',(1.,-3.33066907386739E-16,2.1716102378779E-15)) ;
#42968 = DIRECTION('center_axis',(8.32667268460789E-17,1.,-3.83780830390118E-28)) ;
#42969 = DIRECTION('ref_axis',(-0.707106781186447,5.88784671997906E-17,-0.707106781186648)) ;
#42970 = DIRECTION('center_axis',(-6.48092690624107E-15,-1.,2.90739654573716E-15)) ;
#42971 = DIRECTION('ref_axis',(-1.,6.48092690624107E-15,-2.07369595641671E-28)) ;
#42972 = DIRECTION('',(-8.32667268460789E-17,-1.,3.83780830390118E-28)) ;
#42973 = DIRECTION('center_axis',(1.,-3.33066907386739E-16,2.1716102378779E-15)) ;
#42974 = DIRECTION('ref_axis',(-1.77107419409959E-15,-0.707106781186545,0.70710678118655)) ;
#42975 = DIRECTION('',(1.,-3.33066907386739E-16,2.1716102378779E-15)) ;
#42976 = DIRECTION('center_axis',(-0.81649658092765,0.408248290464166,0.408248290463711)) ;
#42977 = DIRECTION('ref_axis',(-0.577350269189702,-0.577350269189929,-0.577350269189247)) ;
#42978 = DIRECTION('center_axis',(2.17161023787787E-15,-3.83420712807771E-28,
-1.)) ;
#42979 = DIRECTION('ref_axis',(-0.707106781186582,-0.707106781186513,-1.53556032529738E-15)) ;
#42980 = DIRECTION('center_axis',(-0.40824829046392,0.408248290464147,-0.816496580927556)) ;
#42981 = DIRECTION('ref_axis',(0.577350269189076,-0.577350269189986,-0.577350269189815)) ;
#42982 = DIRECTION('center_axis',(1.,-1.66533453692966E-16,2.1716102378779E-15)) ;
#42983 = DIRECTION('ref_axis',(1.65331725969831E-15,0.707106781186545,-0.70710678118655)) ;
#42984 = DIRECTION('center_axis',(1.,1.35627620245787E-13,-2.05796303467862E-28)) ;
#42985 = DIRECTION('ref_axis',(1.8852697114129E-28,-2.90739654573716E-15,
-1.)) ;
#42986 = DIRECTION('',(-1.,1.66533453692966E-16,-2.1716102378779E-15)) ;
#42987 = DIRECTION('center_axis',(-1.,-1.35627620245787E-13,2.05796303467862E-28)) ;
#42988 = DIRECTION('ref_axis',(-1.35627620245787E-13,1.,-2.90739654573716E-15)) ;
#42989 = DIRECTION('center_axis',(0.40824829046392,-0.408248290464147,-0.816496580927556)) ;
#42990 = DIRECTION('ref_axis',(-0.577350269189834,0.577350269189152,-0.577350269189891)) ;
#42991 = DIRECTION('center_axis',(2.17161023787787E-15,-3.83815143260382E-28,
-1.)) ;
#42992 = DIRECTION('ref_axis',(-0.707106781186656,0.707106781186439,-1.53556032529808E-15)) ;
#42993 = DIRECTION('center_axis',(-0.81649658092765,0.408248290464166,-0.408248290463711)) ;
#42994 = DIRECTION('ref_axis',(0.577350269189702,0.577350269189929,-0.577350269189247)) ;
#42995 = DIRECTION('center_axis',(-3.33066907386739E-16,-1.,3.66031460022645E-28)) ;
#42996 = DIRECTION('ref_axis',(-2.17161023787795E-15,3.66754751528624E-28,
1.)) ;
#42997 = DIRECTION('center_axis',(2.1716102378779E-15,-3.83815143260386E-28,
-1.)) ;
#42998 = DIRECTION('ref_axis',(1.,-1.66533453692941E-16,2.1716102378779E-15)) ;
#42999 = DIRECTION('center_axis',(2.1716102378779E-15,-3.83815143260386E-28,
-1.)) ;
#43000 = DIRECTION('ref_axis',(1.,-1.66533453692941E-16,2.1716102378779E-15)) ;
#43001 = DIRECTION('center_axis',(2.1716102378779E-15,-3.83815143260386E-28,
-1.)) ;
#43002 = DIRECTION('ref_axis',(1.,-1.66533453692941E-16,2.1716102378779E-15)) ;
#43003 = DIRECTION('',(-1.66533453692966E-16,-1.,3.83386399937507E-28)) ;
#43004 = DIRECTION('',(1.,-1.66533453692587E-16,2.1716102378779E-15)) ;
#43005 = DIRECTION('',(8.32667268460789E-17,1.,-3.83780830390118E-28)) ;
#43006 = DIRECTION('',(-1.,1.66533453692966E-16,-2.1716102378779E-15)) ;
#43007 = DIRECTION('center_axis',(-0.816496580927764,0.408248290464109,0.408248290463541)) ;
#43008 = DIRECTION('ref_axis',(-0.577350269189531,-0.577350269189986,-0.57735026918936)) ;
#43009 = DIRECTION('center_axis',(1.,1.35627620245787E-13,2.17161023787752E-15)) ;
#43010 = DIRECTION('ref_axis',(1.35627620245787E-13,-1.,2.90739654573778E-15)) ;
#43011 = DIRECTION('center_axis',(6.48092690624107E-15,1.,-2.90739654573747E-15)) ;
#43012 = DIRECTION('ref_axis',(2.17161023787792E-15,-2.90739654573748E-15,
-1.)) ;
#43013 = DIRECTION('center_axis',(2.1716102378779E-15,-3.83420712807775E-28,
-1.)) ;
#43014 = DIRECTION('ref_axis',(-0.70710678118651,-0.707106781186585,-1.53556032529724E-15)) ;
#43015 = DIRECTION('center_axis',(0.40824829046392,-0.408248290464147,-0.816496580927556)) ;
#43016 = DIRECTION('ref_axis',(-0.577350269189986,0.577350269189076,-0.577350269189815)) ;
#43017 = DIRECTION('center_axis',(-6.48092690624107E-15,-1.,2.90739654573747E-15)) ;
#43018 = DIRECTION('ref_axis',(-1.,6.48092690624106E-15,-2.17161023787794E-15)) ;
#43019 = DIRECTION('center_axis',(1.,1.35627620245787E-13,2.17161023787752E-15)) ;
#43020 = DIRECTION('ref_axis',(2.17161023787791E-15,-2.90739654573749E-15,
-1.)) ;
#43021 = DIRECTION('center_axis',(2.1716102378779E-15,-3.83815143260386E-28,
-1.)) ;
#43022 = DIRECTION('ref_axis',(-0.707106781186656,0.707106781186439,-1.5355603252981E-15)) ;
#43023 = DIRECTION('center_axis',(1.66533453692966E-16,1.,-3.83386399937507E-28)) ;
#43024 = DIRECTION('ref_axis',(-0.707106781186596,1.17756934400449E-16,-0.707106781186499)) ;
#43025 = DIRECTION('',(1.66533453692966E-16,1.,-3.83386399937507E-28)) ;
#43026 = DIRECTION('center_axis',(1.,-1.66533453692966E-16,2.1716102378779E-15)) ;
#43027 = DIRECTION('ref_axis',(1.65331725969841E-15,0.707106781186495,-0.7071067811866)) ;
#43028 = DIRECTION('center_axis',(1.,1.35627620245787E-13,2.17161023787752E-15)) ;
#43029 = DIRECTION('ref_axis',(-1.35627620245787E-13,1.,-2.90739654573778E-15)) ;
#43030 = DIRECTION('center_axis',(-1.,1.66533453692587E-16,-2.1716102378779E-15)) ;
#43031 = DIRECTION('ref_axis',(1.41780339089726E-15,-0.707106781186499,-0.707106781186596)) ;
#43032 = DIRECTION('',(-1.,1.66533453692587E-16,-2.1716102378779E-15)) ;
#43033 = DIRECTION('center_axis',(1.,1.35627620245787E-13,2.17161023787752E-15)) ;
#43034 = DIRECTION('ref_axis',(2.17161023787792E-15,-2.90739654573749E-15,
-1.)) ;
#43035 = DIRECTION('center_axis',(-8.32667268460789E-17,-1.,3.83780830390118E-28)) ;
#43036 = DIRECTION('ref_axis',(0.707106781186599,-5.8878467200346E-17,-0.707106781186496)) ;
#43037 = DIRECTION('center_axis',(-6.48092690624107E-15,-1.,2.90739654573747E-15)) ;
#43038 = DIRECTION('ref_axis',(1.,-6.48092690624106E-15,2.17161023787794E-15)) ;
#43039 = DIRECTION('center_axis',(6.48092690624107E-15,1.,-2.90739654573747E-15)) ;
#43040 = DIRECTION('ref_axis',(2.17161023787792E-15,-2.90739654573748E-15,
-1.)) ;
#43041 = DIRECTION('center_axis',(-0.408248290463939,0.408248290464166,-0.816496580927537)) ;
#43042 = DIRECTION('ref_axis',(0.577350269189076,-0.577350269189986,-0.577350269189815)) ;
#43043 = DIRECTION('center_axis',(0.408248290463948,-0.816496580927442,-0.408248290464346)) ;
#43044 = DIRECTION('ref_axis',(0.577350269189304,0.577350269189986,-0.577350269189588)) ;
#43045 = DIRECTION('center_axis',(-1.,1.75658099177411E-13,4.54195640846217E-14)) ;
#43046 = DIRECTION('ref_axis',(-1.75658099177411E-13,-1.,6.26847853931514E-43)) ;
#43047 = DIRECTION('',(4.54195640846217E-14,-1.7376849751744E-27,1.)) ;
#43048 = DIRECTION('',(-4.54195640846217E-14,1.7376849751744E-27,-1.)) ;
#43049 = DIRECTION('center_axis',(-1.,1.75658099177411E-13,4.54195640846217E-14)) ;
#43050 = DIRECTION('ref_axis',(-1.75658099177411E-13,-1.,6.26847853931514E-43)) ;
#43051 = DIRECTION('',(-4.54195640846217E-14,1.7376849751744E-27,-1.)) ;
#43052 = DIRECTION('',(4.54195640846217E-14,-1.7376849751744E-27,1.)) ;
#43053 = DIRECTION('center_axis',(-1.,1.75658099177411E-13,4.54195640846217E-14)) ;
#43054 = DIRECTION('ref_axis',(-1.75658099177411E-13,-1.,6.26847853931514E-43)) ;
#43055 = DIRECTION('',(-4.54195640846217E-14,1.7376849751744E-27,-1.)) ;
#43056 = DIRECTION('',(4.54195640846217E-14,-1.7376849751744E-27,1.)) ;
#43057 = DIRECTION('center_axis',(-1.,1.75658099177411E-13,4.54195640846217E-14)) ;
#43058 = DIRECTION('ref_axis',(-1.75658099177411E-13,-1.,6.26847853931514E-43)) ;
#43059 = DIRECTION('',(-4.54195640846217E-14,1.7376849751744E-27,-1.)) ;
#43060 = DIRECTION('',(4.54195640846217E-14,-1.7376849751744E-27,1.)) ;
#43061 = DIRECTION('center_axis',(-1.,1.75658099177411E-13,4.54195640846217E-14)) ;
#43062 = DIRECTION('ref_axis',(-1.75658099177411E-13,-1.,6.26847853931514E-43)) ;
#43063 = DIRECTION('',(-4.54195640846217E-14,1.7376849751744E-27,-1.)) ;
#43064 = DIRECTION('',(4.54195640846217E-14,-1.7376849751744E-27,1.)) ;
#43065 = DIRECTION('center_axis',(-1.,1.75658099177411E-13,4.54195640846217E-14)) ;
#43066 = DIRECTION('ref_axis',(-1.75658099177411E-13,-1.,6.26847853931514E-43)) ;
#43067 = DIRECTION('',(-4.54195640846217E-14,1.7376849751744E-27,-1.)) ;
#43068 = DIRECTION('',(4.54195640846217E-14,-1.7376849751744E-27,1.)) ;
#43069 = DIRECTION('center_axis',(-1.,1.75658099177411E-13,4.54195640846217E-14)) ;
#43070 = DIRECTION('ref_axis',(-1.75658099177411E-13,-1.,6.26847853931514E-43)) ;
#43071 = DIRECTION('',(-4.54195640846217E-14,1.7376849751744E-27,-1.)) ;
#43072 = DIRECTION('',(4.54195640846217E-14,-1.7376849751744E-27,1.)) ;
#43073 = DIRECTION('center_axis',(-1.,1.75658099177411E-13,4.54195640846217E-14)) ;
#43074 = DIRECTION('ref_axis',(-1.75658099177411E-13,-1.,6.26847853931514E-43)) ;
#43075 = DIRECTION('',(-4.54195640846217E-14,1.7376849751744E-27,-1.)) ;
#43076 = DIRECTION('',(4.54195640846217E-14,-1.7376849751744E-27,1.)) ;
#43077 = DIRECTION('center_axis',(-1.,1.75658099177411E-13,4.54195640846217E-14)) ;
#43078 = DIRECTION('ref_axis',(-1.75658099177411E-13,-1.,6.26847853931514E-43)) ;
#43079 = DIRECTION('',(-4.54195640846217E-14,1.7376849751744E-27,-1.)) ;
#43080 = DIRECTION('',(4.54195640846217E-14,-1.7376849751744E-27,1.)) ;
#43081 = DIRECTION('center_axis',(-1.75658099177411E-13,-1.,6.24062931739685E-27)) ;
#43082 = DIRECTION('ref_axis',(1.,-1.75658099177411E-13,-4.54195640846217E-14)) ;
#43083 = DIRECTION('',(4.54195640846217E-14,-1.7376849751744E-27,1.)) ;
#43084 = DIRECTION('center_axis',(1.75658099177411E-13,1.,-6.24062931739685E-27)) ;
#43085 = DIRECTION('ref_axis',(-1.,1.75658099177411E-13,4.54195640846217E-14)) ;
#43086 = DIRECTION('',(-4.54195640846217E-14,1.7376849751744E-27,-1.)) ;
#43087 = DIRECTION('center_axis',(1.75658099177411E-13,1.,-6.24062931739685E-27)) ;
#43088 = DIRECTION('ref_axis',(-1.,1.75658099177411E-13,4.54195640846217E-14)) ;
#43089 = DIRECTION('',(-4.54195640846217E-14,1.7376849751744E-27,-1.)) ;
#43090 = DIRECTION('center_axis',(-1.75658099177411E-13,-1.,6.24062931739685E-27)) ;
#43091 = DIRECTION('ref_axis',(1.,-1.75658099177411E-13,-4.54195640846217E-14)) ;
#43092 = DIRECTION('',(4.54195640846217E-14,-1.7376849751744E-27,1.)) ;
#43093 = DIRECTION('center_axis',(1.75658099177411E-13,1.,-6.24062931739685E-27)) ;
#43094 = DIRECTION('ref_axis',(-1.,1.75658099177411E-13,4.54195640846217E-14)) ;
#43095 = DIRECTION('',(-4.54195640846217E-14,1.7376849751744E-27,-1.)) ;
#43096 = DIRECTION('center_axis',(-1.75658099177411E-13,-1.,6.24062931739685E-27)) ;
#43097 = DIRECTION('ref_axis',(1.,-1.75658099177411E-13,-4.54195640846217E-14)) ;
#43098 = DIRECTION('',(4.54195640846217E-14,-1.7376849751744E-27,1.)) ;
#43099 = DIRECTION('center_axis',(-1.75658099177411E-13,-1.,6.24062931739685E-27)) ;
#43100 = DIRECTION('ref_axis',(1.,-1.75658099177411E-13,-4.54195640846217E-14)) ;
#43101 = DIRECTION('',(4.54195640846217E-14,-1.7376849751744E-27,1.)) ;
#43102 = DIRECTION('center_axis',(1.75658099177411E-13,1.,-6.24062931739685E-27)) ;
#43103 = DIRECTION('ref_axis',(-1.,1.75658099177411E-13,4.54195640846217E-14)) ;
#43104 = DIRECTION('',(-4.54195640846217E-14,1.7376849751744E-27,-1.)) ;
#43105 = DIRECTION('center_axis',(-1.75658099177411E-13,-1.,6.24062931739685E-27)) ;
#43106 = DIRECTION('ref_axis',(1.,-1.75658099177411E-13,-4.54195640846217E-14)) ;
#43107 = DIRECTION('',(4.54195640846217E-14,-1.7376849751744E-27,1.)) ;
#43108 = DIRECTION('center_axis',(1.75658099177411E-13,1.,-6.24062931739685E-27)) ;
#43109 = DIRECTION('ref_axis',(-1.,1.75658099177411E-13,4.54195640846217E-14)) ;
#43110 = DIRECTION('',(-4.54195640846217E-14,1.7376849751744E-27,-1.)) ;
#43111 = DIRECTION('center_axis',(1.75658099177411E-13,1.,-6.24062931739685E-27)) ;
#43112 = DIRECTION('ref_axis',(-1.,1.75658099177411E-13,4.54195640846217E-14)) ;
#43113 = DIRECTION('',(-4.54195640846217E-14,1.7376849751744E-27,-1.)) ;
#43114 = DIRECTION('center_axis',(-1.75658099177411E-13,-1.,6.24062931739685E-27)) ;
#43115 = DIRECTION('ref_axis',(1.,-1.75658099177411E-13,-4.54195640846217E-14)) ;
#43116 = DIRECTION('',(4.54195640846217E-14,-1.7376849751744E-27,1.)) ;
#43117 = DIRECTION('center_axis',(1.75658099177411E-13,1.,-6.24062931739685E-27)) ;
#43118 = DIRECTION('ref_axis',(-1.,1.75658099177411E-13,4.54195640846217E-14)) ;
#43119 = DIRECTION('',(-4.54195640846217E-14,1.7376849751744E-27,-1.)) ;
#43120 = DIRECTION('center_axis',(-1.75658099177411E-13,-1.,6.24062931739685E-27)) ;
#43121 = DIRECTION('ref_axis',(1.,-1.75658099177411E-13,-4.54195640846217E-14)) ;
#43122 = DIRECTION('',(4.54195640846217E-14,-1.7376849751744E-27,1.)) ;
#43123 = DIRECTION('center_axis',(1.75658099177411E-13,1.,-6.24062931739685E-27)) ;
#43124 = DIRECTION('ref_axis',(-1.,1.75658099177411E-13,4.54195640846217E-14)) ;
#43125 = DIRECTION('',(-4.54195640846217E-14,1.7376849751744E-27,-1.)) ;
#43126 = DIRECTION('center_axis',(-1.75658099177411E-13,-1.,6.24062931739685E-27)) ;
#43127 = DIRECTION('ref_axis',(1.,-1.75658099177411E-13,-4.54195640846217E-14)) ;
#43128 = DIRECTION('',(4.54195640846217E-14,-1.7376849751744E-27,1.)) ;
#43129 = DIRECTION('center_axis',(-1.75658099177411E-13,-1.,6.24062931739685E-27)) ;
#43130 = DIRECTION('ref_axis',(1.,-1.75658099177411E-13,-4.54195640846217E-14)) ;
#43131 = DIRECTION('',(4.54195640846217E-14,-1.7376849751744E-27,1.)) ;
#43132 = DIRECTION('center_axis',(1.75658099177411E-13,1.,-6.24062931739685E-27)) ;
#43133 = DIRECTION('ref_axis',(-1.,1.75658099177411E-13,4.54195640846217E-14)) ;
#43134 = DIRECTION('',(-4.54195640846217E-14,1.7376849751744E-27,-1.)) ;
#43135 = DIRECTION('center_axis',(-4.54195640846217E-14,1.66321791214601E-16,
-1.)) ;
#43136 = DIRECTION('ref_axis',(-1.,1.75658099177411E-13,4.54195640846217E-14)) ;
#43137 = DIRECTION('',(1.,-3.03555657665211E-13,-4.54195640846217E-14)) ;
#43138 = DIRECTION('',(-5.71613981083074E-11,-1.,-1.66321788618356E-16)) ;
#43139 = DIRECTION('',(-1.,1.75658099177411E-13,4.54195640846217E-14)) ;
#43140 = DIRECTION('',(-1.75658099177411E-13,-1.,-1.53926195610211E-16)) ;
#43141 = DIRECTION('',(1.,-3.04147775991511E-13,-4.54195640846217E-14)) ;
#43142 = DIRECTION('',(-5.71613981083074E-11,-1.,-1.66321788618356E-16)) ;
#43143 = DIRECTION('',(-1.,1.75658099177411E-13,4.54195640846217E-14)) ;
#43144 = DIRECTION('',(-1.75658099177411E-13,-1.,-1.53926195610211E-16)) ;
#43145 = DIRECTION('',(1.,-3.03555657665211E-13,-4.54195640846217E-14)) ;
#43146 = DIRECTION('',(-5.71613981083074E-11,-1.,-1.66321788618356E-16)) ;
#43147 = DIRECTION('',(-1.,1.75658099177411E-13,4.54195640846217E-14)) ;
#43148 = DIRECTION('',(-1.75658099177411E-13,-1.,-1.53926195610211E-16)) ;
#43149 = DIRECTION('',(1.,-3.04147775991511E-13,-4.54195640846217E-14)) ;
#43150 = DIRECTION('',(-5.71613981083074E-11,-1.,-1.66321788618356E-16)) ;
#43151 = DIRECTION('',(-1.,1.75658099177411E-13,4.54195640846217E-14)) ;
#43152 = DIRECTION('',(-1.75658099177411E-13,-1.,-1.53926195610211E-16)) ;
#43153 = DIRECTION('',(1.,-3.03555657665211E-13,-4.54195640846217E-14)) ;
#43154 = DIRECTION('',(-5.71613981083074E-11,-1.,-1.66321788618356E-16)) ;
#43155 = DIRECTION('',(1.,-4.6576303444911E-14,-4.54195640846217E-14)) ;
#43156 = DIRECTION('',(-1.75658099177411E-13,-1.,-1.53926195610211E-16)) ;
#43157 = DIRECTION('',(1.,-3.03555657665211E-13,-4.54195640846217E-14)) ;
#43158 = DIRECTION('',(-5.71613981083074E-11,-1.,-1.66321788618356E-16)) ;
#43159 = DIRECTION('',(1.,-4.77605401030109E-14,-4.54195640846217E-14)) ;
#43160 = DIRECTION('',(-1.75658099177411E-13,-1.,-1.53926195610211E-16)) ;
#43161 = DIRECTION('',(1.,-3.03555657665211E-13,-4.54195640846217E-14)) ;
#43162 = DIRECTION('',(-5.71613981083074E-11,-1.,-1.66321788618356E-16)) ;
#43163 = DIRECTION('',(1.,-4.6576303444911E-14,-4.54195640846217E-14)) ;
#43164 = DIRECTION('',(-1.75658099177411E-13,-1.,-1.53926195610211E-16)) ;
#43165 = DIRECTION('',(1.,-3.03555657665211E-13,-4.54195640846217E-14)) ;
#43166 = DIRECTION('',(-5.71613981083074E-11,-1.,-1.66321788618356E-16)) ;
#43167 = DIRECTION('',(1.,-4.6576304037011E-14,-4.54195640846217E-14)) ;
#43168 = DIRECTION('',(-1.75658099177411E-13,-1.,-1.53926195610211E-16)) ;
#43169 = DIRECTION('',(1.,-3.03555657665211E-13,-4.54195640846217E-14)) ;
#43170 = DIRECTION('',(-5.71613981083074E-11,-1.,-1.66321788618356E-16)) ;
#43171 = DIRECTION('',(-1.,1.73688224296914E-13,4.53957858957841E-14)) ;
#43172 = DIRECTION('',(1.75658099177411E-13,1.,1.53926195610211E-16)) ;
#43173 = DIRECTION('',(-1.,1.73688224296914E-13,4.53957858957841E-14)) ;
#43174 = DIRECTION('',(-5.71613981083074E-11,-1.,-1.66321788618356E-16)) ;
#43175 = DIRECTION('',(1.,-1.75658099177411E-13,-4.54195640846217E-14)) ;
#43176 = DIRECTION('',(-1.75658099177411E-13,-1.,-1.53926195610211E-16)) ;
#43177 = DIRECTION('center_axis',(1.75658099177411E-13,1.,1.66321791206623E-16)) ;
#43178 = DIRECTION('ref_axis',(0.707112705703078,-1.24327680069036E-13,0.707100856620378)) ;
#43179 = DIRECTION('center_axis',(4.97494589055058E-8,0.999847695517053,-0.0174523857749279)) ;
#43180 = DIRECTION('ref_axis',(-1.30137752939697E-5,-0.0174523857728027,-0.999847695432399)) ;
#43181 = DIRECTION('',(1.75658099174892E-13,1.,-5.54473693597788E-11)) ;
#43182 = DIRECTION('center_axis',(4.97533257450734E-8,-0.999847695517151,
-0.0174523857693158)) ;
#43183 = DIRECTION('ref_axis',(1.30102029465389E-5,-0.0174523857671916,0.999847695432543)) ;
#43184 = DIRECTION('center_axis',(-1.74838664905478E-13,-0.999847695156391,
0.0174524064372797)) ;
#43185 = DIRECTION('ref_axis',(4.84783030058612E-14,0.0174524064372797,0.999847695156391)) ;
#43186 = DIRECTION('',(4.84783030059014E-14,0.0174524064375096,0.999847695156387)) ;
#43187 = DIRECTION('',(0.707052927141238,-0.0123416547510578,-0.707052927141252)) ;
#43188 = DIRECTION('',(-4.84783030058629E-14,-0.0174524064372897,-0.999847695156391)) ;
#43189 = DIRECTION('center_axis',(1.75658099177411E-13,1.,1.66321791206623E-16)) ;
#43190 = DIRECTION('ref_axis',(0.70711270570306,-1.24327680069032E-13,0.707100856620396)) ;
#43191 = DIRECTION('',(1.75658099174892E-13,1.,-5.54473693597788E-11)) ;
#43192 = DIRECTION('center_axis',(4.97533257450734E-8,-0.999847695517151,
-0.0174523857693158)) ;
#43193 = DIRECTION('ref_axis',(1.30083962602235E-5,-0.0174523857671921,0.999847695432567)) ;
#43194 = DIRECTION('center_axis',(4.97494589055058E-8,0.999847695517053,-0.0174523857749279)) ;
#43195 = DIRECTION('ref_axis',(-1.30106570826674E-5,-0.0174523857728036,-0.999847695432439)) ;
#43196 = DIRECTION('center_axis',(1.75658099177411E-13,1.,1.66321791206623E-16)) ;
#43197 = DIRECTION('ref_axis',(0.707112705703065,-1.24327680069033E-13,0.707100856620391)) ;
#43198 = DIRECTION('center_axis',(4.97494589055058E-8,0.999847695517053,-0.0174523857749279)) ;
#43199 = DIRECTION('ref_axis',(-1.30137786494106E-5,-0.0174523857728027,-0.999847695432399)) ;
#43200 = DIRECTION('',(1.75658099174892E-13,1.,-5.54473693597788E-11)) ;
#43201 = DIRECTION('center_axis',(4.97533257450734E-8,-0.999847695517151,
-0.0174523857693158)) ;
#43202 = DIRECTION('ref_axis',(1.30100135812283E-5,-0.0174523857671916,0.999847695432546)) ;
#43203 = DIRECTION('center_axis',(1.75658099177411E-13,1.,1.66321791206623E-16)) ;
#43204 = DIRECTION('ref_axis',(0.707112705703077,-1.24327680069035E-13,0.707100856620379)) ;
#43205 = DIRECTION('center_axis',(4.97494470609749E-8,0.999847695517053,-0.0174523857749161)) ;
#43206 = DIRECTION('ref_axis',(-1.30088130075626E-5,-0.0174523857727923,-0.999847695432464)) ;
#43207 = DIRECTION('',(1.75658099174892E-13,1.,-5.54473693597788E-11)) ;
#43208 = DIRECTION('center_axis',(4.97533257450734E-8,-0.999847695517151,
-0.0174523857693158)) ;
#43209 = DIRECTION('ref_axis',(1.30145516036281E-5,-0.0174523857671904,0.999847695432487)) ;
#43210 = DIRECTION('center_axis',(1.75658099177411E-13,1.,1.66321791206623E-16)) ;
#43211 = DIRECTION('ref_axis',(0.707112705703066,-1.24327680069033E-13,0.70710085662039)) ;
#43212 = DIRECTION('',(1.75658099174892E-13,1.,-5.54473693597788E-11)) ;
#43213 = DIRECTION('center_axis',(4.97533257450734E-8,-0.999847695517151,
-0.0174523857693158)) ;
#43214 = DIRECTION('ref_axis',(1.30102029465389E-5,-0.0174523857671916,0.999847695432543)) ;
#43215 = DIRECTION('center_axis',(4.97400119840491E-8,0.999847695516655,-0.0174523857976883)) ;
#43216 = DIRECTION('ref_axis',(-1.30177007513301E-5,-0.0174523857955622,-0.999847695431951)) ;
#43217 = DIRECTION('center_axis',(1.75658099177411E-13,1.,1.66321791206623E-16)) ;
#43218 = DIRECTION('ref_axis',(0.707112705703067,-1.24327680069034E-13,0.707100856620389)) ;
#43219 = DIRECTION('',(1.75658099174892E-13,1.,-5.54473693597788E-11)) ;
#43220 = DIRECTION('center_axis',(4.97533090048031E-8,-0.99984769551715,-0.0174523857693562)) ;
#43221 = DIRECTION('ref_axis',(1.30090361591441E-5,-0.0174523857672323,0.999847695432558)) ;
#43222 = DIRECTION('center_axis',(4.9749430318237E-8,0.999847695517052,-0.0174523857749565)) ;
#43223 = DIRECTION('ref_axis',(-1.30139248551185E-5,-0.0174523857728313,-0.999847695432396)) ;
#43224 = DIRECTION('center_axis',(1.75658099177411E-13,1.,1.66321791206623E-16)) ;
#43225 = DIRECTION('ref_axis',(0.707112705703064,-1.24327680069033E-13,0.707100856620392)) ;
#43226 = DIRECTION('',(1.75658099174892E-13,1.,-5.54473693597788E-11)) ;
#43227 = DIRECTION('center_axis',(4.97533257450734E-8,-0.999847695517151,
-0.0174523857693158)) ;
#43228 = DIRECTION('ref_axis',(1.30096219496208E-5,-0.0174523857671917,0.999847695432551)) ;
#43229 = DIRECTION('center_axis',(4.97494017334358E-8,0.999847695517052,-0.0174523857749851)) ;
#43230 = DIRECTION('ref_axis',(-1.3016906447811E-5,-0.0174523857728591,-0.999847695432357)) ;
#43231 = DIRECTION('center_axis',(1.75658099177411E-13,1.,1.66321791206623E-16)) ;
#43232 = DIRECTION('ref_axis',(0.707112705703086,-1.24327680069037E-13,0.70710085662037)) ;
#43233 = DIRECTION('center_axis',(4.97494589055058E-8,0.999847695517053,-0.0174523857749279)) ;
#43234 = DIRECTION('ref_axis',(-1.30141587811237E-5,-0.0174523857728026,-0.999847695432394)) ;
#43235 = DIRECTION('',(1.75658099174892E-13,1.,-5.54473693597788E-11)) ;
#43236 = DIRECTION('center_axis',(4.97533090048031E-8,-0.99984769551715,-0.0174523857693562)) ;
#43237 = DIRECTION('ref_axis',(1.30078195775241E-5,-0.0174523857672326,0.999847695432574)) ;
#43238 = DIRECTION('center_axis',(1.75658099177411E-13,1.,1.66321791206623E-16)) ;
#43239 = DIRECTION('ref_axis',(0.707112705703071,-1.24327680069034E-13,0.707100856620385)) ;
#43240 = DIRECTION('',(1.75658099174892E-13,1.,-5.54473693597888E-11)) ;
#43241 = DIRECTION('center_axis',(4.96835356766386E-8,-0.999847695515933,
-0.0174523858390597)) ;
#43242 = DIRECTION('ref_axis',(1.30149063904817E-5,-0.0174523858369351,0.999847695431265)) ;
#43243 = DIRECTION('center_axis',(4.97172307340419E-8,0.999847695516491,-0.0174523858071221)) ;
#43244 = DIRECTION('ref_axis',(-1.29996074717629E-5,-0.0174523858050013,-0.999847695432021)) ;
#43245 = DIRECTION('center_axis',(1.76424026290696E-13,0.999847695156391,
0.01745240643728)) ;
#43246 = DIRECTION('ref_axis',(-4.23469899241728E-14,0.01745240643728,-0.999847695156391)) ;
#43247 = DIRECTION('center_axis',(4.97533257450734E-8,-0.999847695517151,
-0.0174523857693158)) ;
#43248 = DIRECTION('ref_axis',(1.30096219496208E-5,-0.0174523857671917,0.999847695432551)) ;
#43249 = DIRECTION('',(4.2346989924171E-14,-0.01745240643729,0.999847695156391)) ;
#43250 = DIRECTION('',(-0.707052927141242,-0.0123416547508096,0.707052927141252)) ;
#43251 = DIRECTION('',(-4.23469899241322E-14,0.0174524064375099,-0.999847695156387)) ;
#43252 = DIRECTION('center_axis',(1.75658099177411E-13,1.,1.66321791206623E-16)) ;
#43253 = DIRECTION('ref_axis',(0.707112705703064,-1.24327680069033E-13,0.707100856620392)) ;
#43254 = DIRECTION('',(1.75658099174892E-13,1.,-5.54473693597788E-11)) ;
#43255 = DIRECTION('center_axis',(4.97494589055058E-8,0.999847695517053,-0.0174523857749279)) ;
#43256 = DIRECTION('ref_axis',(-1.30106494130138E-5,-0.0174523857728036,-0.999847695432439)) ;
#43257 = DIRECTION('center_axis',(0.707106781186554,-1.24326640365109E-13,
0.707106781186541)) ;
#43258 = DIRECTION('ref_axis',(0.707106781186541,-2.04517587165981E-30,-0.707106781186554)) ;
#43259 = DIRECTION('',(1.75658099177411E-13,1.,1.66321791206623E-16)) ;
#43260 = DIRECTION('center_axis',(0.707106781186548,-1.24326640365108E-13,
0.707106781186548)) ;
#43261 = DIRECTION('ref_axis',(0.707106781186548,7.39148474710689E-31,-0.707106781186548)) ;
#43262 = DIRECTION('',(-0.707052927141248,-0.0123416547508095,0.707052927141246)) ;
#43263 = DIRECTION('',(1.75658099177411E-13,1.,1.66321791206623E-16)) ;
#43264 = DIRECTION('',(0.707052927141244,-0.0123416547510577,-0.707052927141246)) ;
#43265 = DIRECTION('',(-1.75658099177411E-13,-1.,-1.66321791206623E-16)) ;
#43266 = DIRECTION('center_axis',(0.707106781186548,-1.24326640365108E-13,
0.707106781186548)) ;
#43267 = DIRECTION('ref_axis',(0.707106781186548,7.39148474710689E-31,-0.707106781186548)) ;
#43268 = DIRECTION('',(-0.707052927141248,-0.0123416547508095,0.707052927141246)) ;
#43269 = DIRECTION('',(1.75658099177411E-13,1.,1.66321791206623E-16)) ;
#43270 = DIRECTION('',(0.707052927141244,-0.0123416547510577,-0.707052927141246)) ;
#43271 = DIRECTION('',(-1.75658099177411E-13,-1.,-1.66321791206623E-16)) ;
#43272 = DIRECTION('center_axis',(0.707106781186554,-1.24326640365109E-13,
0.707106781186541)) ;
#43273 = DIRECTION('ref_axis',(0.707106781186541,-2.04517587165981E-30,-0.707106781186554)) ;
#43274 = DIRECTION('',(-0.707052927141242,-0.0123416547508096,0.707052927141252)) ;
#43275 = DIRECTION('',(1.75658099177411E-13,1.,1.66321791206623E-16)) ;
#43276 = DIRECTION('',(0.707052927141238,-0.0123416547510578,-0.707052927141252)) ;
#43277 = DIRECTION('',(-1.75658099177411E-13,-1.,-1.66321791206623E-16)) ;
#43278 = DIRECTION('center_axis',(0.707106781186548,-1.24326640365108E-13,
0.707106781186548)) ;
#43279 = DIRECTION('ref_axis',(0.707106781186548,7.39148474710689E-31,-0.707106781186548)) ;
#43280 = DIRECTION('',(-0.707052927141248,-0.0123416547508095,0.707052927141246)) ;
#43281 = DIRECTION('',(1.75658099177411E-13,1.,1.66321791206623E-16)) ;
#43282 = DIRECTION('',(0.707052927141244,-0.0123416547510577,-0.707052927141246)) ;
#43283 = DIRECTION('',(-1.75658099177411E-13,-1.,-1.66321791206623E-16)) ;
#43284 = DIRECTION('center_axis',(0.707106781186548,-1.24326640365108E-13,
0.707106781186548)) ;
#43285 = DIRECTION('ref_axis',(0.707106781186548,7.39148474710689E-31,-0.707106781186548)) ;
#43286 = DIRECTION('',(-0.707052927141248,-0.0123416547508095,0.707052927141246)) ;
#43287 = DIRECTION('',(1.75658099177411E-13,1.,1.66321791206623E-16)) ;
#43288 = DIRECTION('',(0.707052927141244,-0.0123416547510577,-0.707052927141246)) ;
#43289 = DIRECTION('',(-1.75658099177411E-13,-1.,-1.66321791206623E-16)) ;
#43290 = DIRECTION('center_axis',(0.707106781186548,-1.24326640365108E-13,
0.707106781186548)) ;
#43291 = DIRECTION('ref_axis',(0.707106781186548,7.39148474710689E-31,-0.707106781186548)) ;
#43292 = DIRECTION('',(-0.707052927141248,-0.0123416547508095,0.707052927141246)) ;
#43293 = DIRECTION('',(1.75658099177411E-13,1.,1.66321791206623E-16)) ;
#43294 = DIRECTION('',(0.707052927141244,-0.0123416547510577,-0.707052927141246)) ;
#43295 = DIRECTION('',(-1.75658099177411E-13,-1.,-1.66321791206623E-16)) ;
#43296 = DIRECTION('center_axis',(0.707106781186548,-1.24326640365108E-13,
0.707106781186548)) ;
#43297 = DIRECTION('ref_axis',(0.707106781186548,7.39148474710689E-31,-0.707106781186548)) ;
#43298 = DIRECTION('',(-0.707052927141248,-0.0123416547508095,0.707052927141246)) ;
#43299 = DIRECTION('',(1.75658099177411E-13,1.,1.66321791206623E-16)) ;
#43300 = DIRECTION('',(0.707052927141244,-0.0123416547510577,-0.707052927141246)) ;
#43301 = DIRECTION('',(-1.75658099177411E-13,-1.,-1.66321791206623E-16)) ;
#43302 = DIRECTION('center_axis',(0.707106781186554,-1.24326640365109E-13,
0.707106781186541)) ;
#43303 = DIRECTION('ref_axis',(0.707106781186541,-2.04517587165981E-30,-0.707106781186554)) ;
#43304 = DIRECTION('',(-0.707052927141242,-0.0123416547508096,0.707052927141252)) ;
#43305 = DIRECTION('',(1.75658099177411E-13,1.,1.66321791206623E-16)) ;
#43306 = DIRECTION('',(0.707052927141238,-0.0123416547510578,-0.707052927141252)) ;
#43307 = DIRECTION('',(-1.75658099177411E-13,-1.,-1.66321791206623E-16)) ;
#43308 = DIRECTION('center_axis',(-1.74838664905478E-13,-0.999847695156391,
0.0174524064372797)) ;
#43309 = DIRECTION('ref_axis',(4.84783030058612E-14,0.0174524064372797,0.999847695156391)) ;
#43310 = DIRECTION('',(-4.84783030058629E-14,-0.0174524064372897,-0.999847695156391)) ;
#43311 = DIRECTION('',(4.84783030057975E-14,0.0174524064369153,0.999847695156398)) ;
#43312 = DIRECTION('center_axis',(1.76424026290696E-13,0.999847695156391,
0.01745240643728)) ;
#43313 = DIRECTION('ref_axis',(-4.23469899241728E-14,0.01745240643728,-0.999847695156391)) ;
#43314 = DIRECTION('',(4.2346989924171E-14,-0.01745240643729,0.999847695156391)) ;
#43315 = DIRECTION('',(1.,-1.75658099177411E-13,-4.54195640846217E-14)) ;
#43316 = DIRECTION('',(-4.23469899241322E-14,0.0174524064375099,-0.999847695156387)) ;
#43317 = DIRECTION('center_axis',(-1.74838664905478E-13,-0.999847695156391,
0.0174524064372797)) ;
#43318 = DIRECTION('ref_axis',(4.84783030058612E-14,0.0174524064372797,0.999847695156391)) ;
#43319 = DIRECTION('',(4.84783030059014E-14,0.0174524064375096,0.999847695156387)) ;
#43320 = DIRECTION('',(-1.,1.75658099177411E-13,4.54195640846217E-14)) ;
#43321 = DIRECTION('',(-4.84783030058629E-14,-0.0174524064372897,-0.999847695156391)) ;
#43322 = DIRECTION('center_axis',(1.76424026290696E-13,0.999847695156391,
0.01745240643728)) ;
#43323 = DIRECTION('ref_axis',(-4.23469899241728E-14,0.01745240643728,-0.999847695156391)) ;
#43324 = DIRECTION('',(4.2346989924171E-14,-0.01745240643729,0.999847695156391)) ;
#43325 = DIRECTION('',(1.,-1.75658099177411E-13,-4.54195640846217E-14)) ;
#43326 = DIRECTION('',(-4.23469899241322E-14,0.0174524064375099,-0.999847695156387)) ;
#43327 = DIRECTION('center_axis',(-1.74838664905478E-13,-0.999847695156391,
0.0174524064372797)) ;
#43328 = DIRECTION('ref_axis',(4.84783030058612E-14,0.0174524064372797,0.999847695156391)) ;
#43329 = DIRECTION('',(4.84783030059014E-14,0.0174524064375096,0.999847695156387)) ;
#43330 = DIRECTION('',(-1.,1.75658099177411E-13,4.54195640846217E-14)) ;
#43331 = DIRECTION('',(-4.84783030058629E-14,-0.0174524064372897,-0.999847695156391)) ;
#43332 = DIRECTION('center_axis',(1.76424026290696E-13,0.999847695156391,
0.01745240643728)) ;
#43333 = DIRECTION('ref_axis',(-4.23469899241728E-14,0.01745240643728,-0.999847695156391)) ;
#43334 = DIRECTION('',(4.2346989924171E-14,-0.01745240643729,0.999847695156391)) ;
#43335 = DIRECTION('',(1.,-1.75658099177411E-13,-4.54195640846217E-14)) ;
#43336 = DIRECTION('',(-4.23469899241322E-14,0.0174524064375099,-0.999847695156387)) ;
#43337 = DIRECTION('center_axis',(-1.74838664905478E-13,-0.999847695156391,
0.0174524064372797)) ;
#43338 = DIRECTION('ref_axis',(4.84783030058612E-14,0.0174524064372797,0.999847695156391)) ;
#43339 = DIRECTION('',(4.84783030059014E-14,0.0174524064375096,0.999847695156387)) ;
#43340 = DIRECTION('',(-1.,1.75658099177411E-13,4.54195640846217E-14)) ;
#43341 = DIRECTION('',(-4.84783030058629E-14,-0.0174524064372897,-0.999847695156391)) ;
#43342 = DIRECTION('center_axis',(1.76424026290696E-13,0.999847695156391,
0.01745240643728)) ;
#43343 = DIRECTION('ref_axis',(-4.23469899241728E-14,0.01745240643728,-0.999847695156391)) ;
#43344 = DIRECTION('',(4.2346989924171E-14,-0.01745240643729,0.999847695156391)) ;
#43345 = DIRECTION('',(1.,-1.75658099177411E-13,-4.54195640846217E-14)) ;
#43346 = DIRECTION('',(-4.23469899241322E-14,0.0174524064375099,-0.999847695156387)) ;
#43347 = DIRECTION('center_axis',(1.74838664905478E-13,0.999847695156391,
-0.0174524064372797)) ;
#43348 = DIRECTION('ref_axis',(-4.84783030058612E-14,-0.0174524064372797,
-0.999847695156391)) ;
#43349 = DIRECTION('',(4.84783030059014E-14,0.0174524064375096,0.999847695156387)) ;
#43350 = DIRECTION('',(-1.,1.75658099177411E-13,4.54195640846217E-14)) ;
#43351 = DIRECTION('',(-4.84783030058629E-14,-0.0174524064372897,-0.999847695156391)) ;
#43352 = DIRECTION('center_axis',(-1.76424026290696E-13,-0.999847695156391,
-0.01745240643728)) ;
#43353 = DIRECTION('ref_axis',(4.23469899241728E-14,-0.01745240643728,0.999847695156391)) ;
#43354 = DIRECTION('',(4.2346989924171E-14,-0.01745240643729,0.999847695156391)) ;
#43355 = DIRECTION('',(1.,-1.75658099177411E-13,-4.54195640846217E-14)) ;
#43356 = DIRECTION('',(-4.23469899241322E-14,0.0174524064375099,-0.999847695156387)) ;
#43357 = DIRECTION('center_axis',(1.74838664905478E-13,0.999847695156391,
-0.0174524064372797)) ;
#43358 = DIRECTION('ref_axis',(-4.84783030058612E-14,-0.0174524064372797,
-0.999847695156391)) ;
#43359 = DIRECTION('',(4.84783030059014E-14,0.0174524064375096,0.999847695156387)) ;
#43360 = DIRECTION('',(-1.,1.75658099177411E-13,4.54195640846217E-14)) ;
#43361 = DIRECTION('',(-4.84783030058629E-14,-0.0174524064372897,-0.999847695156391)) ;
#43362 = DIRECTION('center_axis',(-1.76424026290696E-13,-0.999847695156391,
-0.01745240643728)) ;
#43363 = DIRECTION('ref_axis',(4.23469899241728E-14,-0.01745240643728,0.999847695156391)) ;
#43364 = DIRECTION('',(4.2346989924171E-14,-0.01745240643729,0.999847695156391)) ;
#43365 = DIRECTION('',(1.,-1.75658099177411E-13,-4.54195640846217E-14)) ;
#43366 = DIRECTION('',(-4.23469899241322E-14,0.0174524064375099,-0.999847695156387)) ;
#43367 = DIRECTION('center_axis',(1.74838664905478E-13,0.999847695156391,
-0.0174524064372797)) ;
#43368 = DIRECTION('ref_axis',(-4.84783030058612E-14,-0.0174524064372797,
-0.999847695156391)) ;
#43369 = DIRECTION('',(4.84783030059031E-14,0.0174524064375196,0.999847695156387)) ;
#43370 = DIRECTION('',(-1.,1.75658099177411E-13,4.54195640846217E-14)) ;
#43371 = DIRECTION('',(-4.84783030058629E-14,-0.0174524064372897,-0.999847695156391)) ;
#43372 = DIRECTION('center_axis',(-1.76424026290696E-13,-0.999847695156391,
-0.01745240643728)) ;
#43373 = DIRECTION('ref_axis',(4.23469899241728E-14,-0.01745240643728,0.999847695156391)) ;
#43374 = DIRECTION('',(4.2346989924171E-14,-0.01745240643729,0.999847695156391)) ;
#43375 = DIRECTION('',(1.,-1.75658099177411E-13,-4.54195640846217E-14)) ;
#43376 = DIRECTION('',(-4.23469899241322E-14,0.0174524064375099,-0.999847695156387)) ;
#43377 = DIRECTION('center_axis',(1.74838664905478E-13,0.999847695156391,
-0.0174524064372797)) ;
#43378 = DIRECTION('ref_axis',(-4.84783030058612E-14,-0.0174524064372797,
-0.999847695156391)) ;
#43379 = DIRECTION('',(4.84783030059014E-14,0.0174524064375096,0.999847695156387)) ;
#43380 = DIRECTION('',(-1.,1.75658099177411E-13,4.54195640846217E-14)) ;
#43381 = DIRECTION('',(-4.84783030058629E-14,-0.0174524064372897,-0.999847695156391)) ;
#43382 = DIRECTION('center_axis',(-1.76424026290696E-13,-0.999847695156391,
-0.01745240643728)) ;
#43383 = DIRECTION('ref_axis',(4.23469899241728E-14,-0.01745240643728,0.999847695156391)) ;
#43384 = DIRECTION('',(4.2346989924171E-14,-0.01745240643729,0.999847695156391)) ;
#43385 = DIRECTION('',(1.,-1.75658099177411E-13,-4.54195640846217E-14)) ;
#43386 = DIRECTION('',(-4.23469899241322E-14,0.0174524064375099,-0.999847695156387)) ;
#43387 = DIRECTION('center_axis',(1.74838664905478E-13,0.999847695156391,
-0.0174524064372797)) ;
#43388 = DIRECTION('ref_axis',(-4.84783030058612E-14,-0.0174524064372797,
-0.999847695156391)) ;
#43389 = DIRECTION('',(4.84783030059049E-14,0.0174524064375296,0.999847695156387)) ;
#43390 = DIRECTION('',(-1.,1.75658099177411E-13,4.54195640846217E-14)) ;
#43391 = DIRECTION('',(-4.84783030058647E-14,-0.0174524064372997,-0.999847695156391)) ;
#43392 = DIRECTION('center_axis',(-1.,1.75658099177411E-13,4.54195640846217E-14)) ;
#43393 = DIRECTION('ref_axis',(-1.75658099177411E-13,-1.,6.26847853931514E-43)) ;
#43394 = DIRECTION('center_axis',(-1.,1.73688224296914E-13,4.53957858957841E-14)) ;
#43395 = DIRECTION('ref_axis',(4.53957858957841E-14,2.00890147845606E-41,
1.)) ;
#43396 = DIRECTION('',(-4.2346989924355E-14,0.0174524064362477,-0.999847695156409)) ;
#43397 = DIRECTION('center_axis',(-1.,1.75658099177411E-13,4.54195640846217E-14)) ;
#43398 = DIRECTION('ref_axis',(-1.75658099177411E-13,-1.,6.26847853931514E-43)) ;
#43399 = DIRECTION('',(1.75658099177411E-13,1.,1.66321791206623E-16)) ;
#43400 = DIRECTION('center_axis',(-1.,1.75658099177411E-13,4.54195640846217E-14)) ;
#43401 = DIRECTION('ref_axis',(-1.75658099177411E-13,-1.,6.26847853931514E-43)) ;
#43402 = DIRECTION('',(1.75658099177411E-13,1.,1.66321791206623E-16)) ;
#43403 = DIRECTION('center_axis',(-1.,1.75658099177411E-13,4.54195640846217E-14)) ;
#43404 = DIRECTION('ref_axis',(-1.75658099177411E-13,-1.,6.26847853931514E-43)) ;
#43405 = DIRECTION('',(1.75658099177411E-13,1.,1.66321791206623E-16)) ;
#43406 = DIRECTION('center_axis',(-1.,1.75658099177411E-13,4.54195640846217E-14)) ;
#43407 = DIRECTION('ref_axis',(-1.75658099177411E-13,-1.,6.26847853931514E-43)) ;
#43408 = DIRECTION('',(1.75658099177411E-13,1.,1.66321791206623E-16)) ;
#43409 = DIRECTION('center_axis',(-1.,1.75658099177411E-13,4.54195640846217E-14)) ;
#43410 = DIRECTION('ref_axis',(-1.75658099177411E-13,-1.,6.26847853931514E-43)) ;
#43411 = DIRECTION('',(1.75658099177411E-13,1.,1.66321791206623E-16)) ;
#43412 = DIRECTION('center_axis',(-1.,1.75658099177411E-13,4.54195640846217E-14)) ;
#43413 = DIRECTION('ref_axis',(-1.75658099177411E-13,-1.,6.26847853931514E-43)) ;
#43414 = DIRECTION('',(1.75658099177411E-13,1.,1.66321791206623E-16)) ;
#43415 = DIRECTION('center_axis',(-1.,1.75658099177411E-13,4.54195640846217E-14)) ;
#43416 = DIRECTION('ref_axis',(-1.75658099177411E-13,-1.,6.26847853931514E-43)) ;
#43417 = DIRECTION('',(1.75658099177411E-13,1.,1.66321791206623E-16)) ;
#43418 = DIRECTION('center_axis',(-1.,1.75658099177411E-13,4.54195640846217E-14)) ;
#43419 = DIRECTION('ref_axis',(-1.75658099177411E-13,-1.,6.26847853931514E-43)) ;
#43420 = DIRECTION('',(1.75658099177411E-13,1.,1.66321791206623E-16)) ;
#43421 = DIRECTION('center_axis',(4.54195640846217E-14,-1.66321791214601E-16,
1.)) ;
#43422 = DIRECTION('ref_axis',(1.75658099177411E-13,1.,1.66321791206623E-16)) ;
#43423 = DIRECTION('center_axis',(-2.16239769233719E-14,8.31608956071042E-17,
-1.)) ;
#43424 = DIRECTION('ref_axis',(1.,-9.64599832246215E-47,-2.16239769233719E-14)) ;
#43425 = DIRECTION('center_axis',(-2.17161023787787E-15,3.92492613217813E-28,
1.)) ;
#43426 = DIRECTION('ref_axis',(1.,-1.46338648716481E-13,2.28654138619502E-15)) ;
#43427 = DIRECTION('center_axis',(-2.17161023787787E-15,3.92492613217813E-28,
1.)) ;
#43428 = DIRECTION('ref_axis',(-1.,4.92531066966514E-14,-2.17161023787787E-15)) ;
#43429 = DIRECTION('center_axis',(-2.17161023787787E-15,3.92492613217813E-28,
1.)) ;
#43430 = DIRECTION('ref_axis',(-1.,4.92531066966514E-14,-2.17161023787787E-15)) ;
#43431 = DIRECTION('center_axis',(-1.37192483171701E-13,-1.,9.45640122022591E-29)) ;
#43432 = DIRECTION('ref_axis',(-1.,1.37192483171701E-13,-2.85817673274378E-15)) ;
#43433 = DIRECTION('center_axis',(-2.1716102378779E-15,3.83815143260386E-28,
1.)) ;
#43434 = DIRECTION('ref_axis',(-1.,-9.69015809248849E-15,-2.1716102378779E-15)) ;
#43435 = DIRECTION('center_axis',(2.1716102378779E-15,-3.83815143260386E-28,
-1.)) ;
#43436 = DIRECTION('ref_axis',(-1.,-7.3303373675338E-16,-2.1716102378779E-15)) ;
#43437 = DIRECTION('',(-2.1716102378779E-15,3.83815143260386E-28,1.)) ;
#43438 = DIRECTION('center_axis',(2.1716102378779E-15,-3.83815143260386E-28,
-1.)) ;
#43439 = DIRECTION('ref_axis',(-1.,1.59141680100251E-13,-2.48658875156642E-15)) ;
#43440 = DIRECTION('center_axis',(1.49195325093984E-13,1.,-5.98210478427684E-29)) ;
#43441 = DIRECTION('ref_axis',(1.,-1.49195325093984E-13,1.554117969729E-15)) ;
#43442 = DIRECTION('center_axis',(-1.66533453692587E-16,-1.,3.82991969484897E-28)) ;
#43443 = DIRECTION('ref_axis',(2.1716102378779E-15,-3.83353615237885E-28,
-1.)) ;
#43444 = DIRECTION('',(-2.17161023787787E-15,3.83420712807771E-28,1.)) ;
#43445 = DIRECTION('center_axis',(2.17161023787787E-15,-3.83420712807771E-28,
-1.)) ;
#43446 = DIRECTION('ref_axis',(-0.707106781186552,-0.707106781186543,-1.53556032529731E-15)) ;
#43447 = DIRECTION('center_axis',(4.54195640846217E-14,-1.66321791214601E-16,
1.)) ;
#43448 = DIRECTION('ref_axis',(1.75658099177411E-13,1.,1.66321791206623E-16)) ;
#43449 = DIRECTION('center_axis',(-2.16239769233719E-14,8.31608956071042E-17,
-1.)) ;
#43450 = DIRECTION('ref_axis',(1.,-9.64599832246215E-47,-2.16239769233719E-14)) ;
#43451 = DIRECTION('center_axis',(-2.17161023787787E-15,3.92492613217813E-28,
1.)) ;
#43452 = DIRECTION('ref_axis',(1.,-1.46338648716481E-13,2.28654138619502E-15)) ;
#43453 = DIRECTION('center_axis',(-2.17161023787787E-15,3.92492613217813E-28,
1.)) ;
#43454 = DIRECTION('ref_axis',(-1.,4.92531066966514E-14,-2.17161023787787E-15)) ;
#43455 = DIRECTION('center_axis',(-2.17161023787787E-15,3.92492613217813E-28,
1.)) ;
#43456 = DIRECTION('ref_axis',(-1.,4.92531066966514E-14,-2.17161023787787E-15)) ;
#43457 = DIRECTION('center_axis',(-1.37192483171701E-13,-1.,9.45640122022591E-29)) ;
#43458 = DIRECTION('ref_axis',(-1.,1.37192483171701E-13,-2.85817673274378E-15)) ;
#43459 = DIRECTION('center_axis',(-2.1716102378779E-15,3.83815143260386E-28,
1.)) ;
#43460 = DIRECTION('ref_axis',(-1.,-9.69015809248849E-15,-2.1716102378779E-15)) ;
#43461 = DIRECTION('center_axis',(2.1716102378779E-15,-3.83815143260386E-28,
-1.)) ;
#43462 = DIRECTION('ref_axis',(-1.,-7.3303373675338E-16,-2.1716102378779E-15)) ;
#43463 = DIRECTION('',(-2.1716102378779E-15,3.83815143260386E-28,1.)) ;
#43464 = DIRECTION('center_axis',(2.1716102378779E-15,-3.83815143260386E-28,
-1.)) ;
#43465 = DIRECTION('ref_axis',(-1.,1.59141680100251E-13,-2.48658875156642E-15)) ;
#43466 = DIRECTION('center_axis',(1.49195325093984E-13,1.,-5.98210478427684E-29)) ;
#43467 = DIRECTION('ref_axis',(1.,-1.49195325093984E-13,1.554117969729E-15)) ;
#43468 = DIRECTION('center_axis',(-1.66533453692587E-16,-1.,3.82991969484897E-28)) ;
#43469 = DIRECTION('ref_axis',(2.1716102378779E-15,-3.83353615237885E-28,
-1.)) ;
#43470 = DIRECTION('',(-2.17161023787787E-15,3.83420712807771E-28,1.)) ;
#43471 = DIRECTION('center_axis',(2.17161023787787E-15,-3.83420712807771E-28,
-1.)) ;
#43472 = DIRECTION('ref_axis',(-0.707106781186552,-0.707106781186543,-1.53556032529731E-15)) ;
#43473 = DIRECTION('center_axis',(4.54195640846217E-14,-1.66321791214601E-16,
1.)) ;
#43474 = DIRECTION('ref_axis',(1.75658099177411E-13,1.,1.66321791206623E-16)) ;
#43475 = DIRECTION('center_axis',(-2.16239769233719E-14,8.31608956071042E-17,
-1.)) ;
#43476 = DIRECTION('ref_axis',(1.,-9.64599832246215E-47,-2.16239769233719E-14)) ;
#43477 = DIRECTION('center_axis',(-2.17161023787787E-15,3.92492613217813E-28,
1.)) ;
#43478 = DIRECTION('ref_axis',(1.,-1.46338648716481E-13,2.28654138619502E-15)) ;
#43479 = DIRECTION('center_axis',(-2.17161023787787E-15,3.92492613217813E-28,
1.)) ;
#43480 = DIRECTION('ref_axis',(-1.,4.92531066966514E-14,-2.17161023787787E-15)) ;
#43481 = DIRECTION('center_axis',(-2.17161023787787E-15,3.92492613217813E-28,
1.)) ;
#43482 = DIRECTION('ref_axis',(-1.,4.92531066966514E-14,-2.17161023787787E-15)) ;
#43483 = DIRECTION('center_axis',(-1.37192483171701E-13,-1.,9.45640122022591E-29)) ;
#43484 = DIRECTION('ref_axis',(-1.,1.37192483171701E-13,-2.85817673274378E-15)) ;
#43485 = DIRECTION('center_axis',(-2.1716102378779E-15,3.83815143260386E-28,
1.)) ;
#43486 = DIRECTION('ref_axis',(-1.,-9.69015809248849E-15,-2.1716102378779E-15)) ;
#43487 = DIRECTION('center_axis',(2.1716102378779E-15,-3.83815143260386E-28,
-1.)) ;
#43488 = DIRECTION('ref_axis',(-1.,-7.3303373675338E-16,-2.1716102378779E-15)) ;
#43489 = DIRECTION('',(-2.1716102378779E-15,3.83815143260386E-28,1.)) ;
#43490 = DIRECTION('center_axis',(2.1716102378779E-15,-3.83815143260386E-28,
-1.)) ;
#43491 = DIRECTION('ref_axis',(-1.,1.59141680100251E-13,-2.48658875156642E-15)) ;
#43492 = DIRECTION('center_axis',(1.49195325093984E-13,1.,-5.98210478427684E-29)) ;
#43493 = DIRECTION('ref_axis',(1.,-1.49195325093984E-13,1.554117969729E-15)) ;
#43494 = DIRECTION('center_axis',(-1.66533453692587E-16,-1.,3.82991969484897E-28)) ;
#43495 = DIRECTION('ref_axis',(2.1716102378779E-15,-3.83353615237885E-28,
-1.)) ;
#43496 = DIRECTION('',(-2.17161023787787E-15,3.83420712807771E-28,1.)) ;
#43497 = DIRECTION('center_axis',(2.17161023787787E-15,-3.83420712807771E-28,
-1.)) ;
#43498 = DIRECTION('ref_axis',(-0.707106781186552,-0.707106781186543,-1.53556032529731E-15)) ;
#43499 = DIRECTION('center_axis',(4.54195640846217E-14,-1.66321791214601E-16,
1.)) ;
#43500 = DIRECTION('ref_axis',(1.75658099177411E-13,1.,1.66321791206623E-16)) ;
#43501 = DIRECTION('center_axis',(-2.16239769233719E-14,8.31608956071042E-17,
-1.)) ;
#43502 = DIRECTION('ref_axis',(1.,-9.64599832246215E-47,-2.16239769233719E-14)) ;
#43503 = DIRECTION('center_axis',(-2.17161023787787E-15,3.92492613217813E-28,
1.)) ;
#43504 = DIRECTION('ref_axis',(1.,-1.46338648716481E-13,2.28654138619502E-15)) ;
#43505 = DIRECTION('center_axis',(-2.17161023787787E-15,3.92492613217813E-28,
1.)) ;
#43506 = DIRECTION('ref_axis',(-1.,4.92531066966514E-14,-2.17161023787787E-15)) ;
#43507 = DIRECTION('center_axis',(-2.17161023787787E-15,3.92492613217813E-28,
1.)) ;
#43508 = DIRECTION('ref_axis',(-1.,4.92531066966514E-14,-2.17161023787787E-15)) ;
#43509 = DIRECTION('center_axis',(-1.37192483171701E-13,-1.,9.45640122022591E-29)) ;
#43510 = DIRECTION('ref_axis',(-1.,1.37192483171701E-13,-2.85817673274378E-15)) ;
#43511 = DIRECTION('center_axis',(-2.1716102378779E-15,3.83815143260386E-28,
1.)) ;
#43512 = DIRECTION('ref_axis',(-1.,-9.69015809248849E-15,-2.1716102378779E-15)) ;
#43513 = DIRECTION('center_axis',(2.1716102378779E-15,-3.83815143260386E-28,
-1.)) ;
#43514 = DIRECTION('ref_axis',(-1.,-7.3303373675338E-16,-2.1716102378779E-15)) ;
#43515 = DIRECTION('',(-2.1716102378779E-15,3.83815143260386E-28,1.)) ;
#43516 = DIRECTION('center_axis',(2.1716102378779E-15,-3.83815143260386E-28,
-1.)) ;
#43517 = DIRECTION('ref_axis',(-1.,1.59141680100251E-13,-2.48658875156642E-15)) ;
#43518 = DIRECTION('center_axis',(1.49195325093984E-13,1.,-5.98210478427684E-29)) ;
#43519 = DIRECTION('ref_axis',(1.,-1.49195325093984E-13,1.554117969729E-15)) ;
#43520 = DIRECTION('center_axis',(-1.66533453692587E-16,-1.,3.82991969484897E-28)) ;
#43521 = DIRECTION('ref_axis',(2.1716102378779E-15,-3.83353615237885E-28,
-1.)) ;
#43522 = DIRECTION('',(-2.17161023787787E-15,3.83420712807771E-28,1.)) ;
#43523 = DIRECTION('center_axis',(2.17161023787787E-15,-3.83420712807771E-28,
-1.)) ;
#43524 = DIRECTION('ref_axis',(-0.707106781186552,-0.707106781186543,-1.53556032529731E-15)) ;
#43525 = DIRECTION('center_axis',(4.54195640846217E-14,-1.66321791214601E-16,
1.)) ;
#43526 = DIRECTION('ref_axis',(1.75658099177411E-13,1.,1.66321791206623E-16)) ;
#43527 = DIRECTION('center_axis',(-2.16239769233719E-14,8.31608956071042E-17,
-1.)) ;
#43528 = DIRECTION('ref_axis',(1.,-9.64599832246215E-47,-2.16239769233719E-14)) ;
#43529 = DIRECTION('center_axis',(-2.17161023787787E-15,3.92492613217813E-28,
1.)) ;
#43530 = DIRECTION('ref_axis',(1.,-1.46338648716481E-13,2.28654138619502E-15)) ;
#43531 = DIRECTION('center_axis',(-2.17161023787787E-15,3.92492613217813E-28,
1.)) ;
#43532 = DIRECTION('ref_axis',(-1.,4.92531066966514E-14,-2.17161023787787E-15)) ;
#43533 = DIRECTION('center_axis',(-2.17161023787787E-15,3.92492613217813E-28,
1.)) ;
#43534 = DIRECTION('ref_axis',(-1.,4.92531066966514E-14,-2.17161023787787E-15)) ;
#43535 = DIRECTION('center_axis',(-1.37192483171701E-13,-1.,9.45640122022591E-29)) ;
#43536 = DIRECTION('ref_axis',(-1.,1.37192483171701E-13,-2.85817673274378E-15)) ;
#43537 = DIRECTION('center_axis',(-2.1716102378779E-15,3.83815143260386E-28,
1.)) ;
#43538 = DIRECTION('ref_axis',(-1.,-9.69015809248849E-15,-2.1716102378779E-15)) ;
#43539 = DIRECTION('center_axis',(2.1716102378779E-15,-3.83815143260386E-28,
-1.)) ;
#43540 = DIRECTION('ref_axis',(-1.,-7.3303373675338E-16,-2.1716102378779E-15)) ;
#43541 = DIRECTION('',(-2.1716102378779E-15,3.83815143260386E-28,1.)) ;
#43542 = DIRECTION('center_axis',(2.1716102378779E-15,-3.83815143260386E-28,
-1.)) ;
#43543 = DIRECTION('ref_axis',(-1.,1.59141680100251E-13,-2.48658875156642E-15)) ;
#43544 = DIRECTION('center_axis',(1.49195325093984E-13,1.,-5.98210478427684E-29)) ;
#43545 = DIRECTION('ref_axis',(1.,-1.49195325093984E-13,1.554117969729E-15)) ;
#43546 = DIRECTION('center_axis',(-1.66533453692587E-16,-1.,3.82991969484897E-28)) ;
#43547 = DIRECTION('ref_axis',(2.1716102378779E-15,-3.83353615237885E-28,
-1.)) ;
#43548 = DIRECTION('',(-2.17161023787787E-15,3.83420712807771E-28,1.)) ;
#43549 = DIRECTION('center_axis',(2.17161023787787E-15,-3.83420712807771E-28,
-1.)) ;
#43550 = DIRECTION('ref_axis',(-0.707106781186552,-0.707106781186543,-1.53556032529731E-15)) ;
#43551 = DIRECTION('center_axis',(4.54195640846217E-14,-1.66321791214601E-16,
1.)) ;
#43552 = DIRECTION('ref_axis',(1.75658099177411E-13,1.,1.66321791206623E-16)) ;
#43553 = DIRECTION('center_axis',(-2.16239769233719E-14,8.31608956071042E-17,
-1.)) ;
#43554 = DIRECTION('ref_axis',(1.,-9.64599832246215E-47,-2.16239769233719E-14)) ;
#43555 = DIRECTION('center_axis',(-2.17161023787787E-15,3.92492613217813E-28,
1.)) ;
#43556 = DIRECTION('ref_axis',(1.,-1.46338648716481E-13,2.28654138619502E-15)) ;
#43557 = DIRECTION('center_axis',(-2.17161023787787E-15,3.92492613217813E-28,
1.)) ;
#43558 = DIRECTION('ref_axis',(-1.,4.92531066966514E-14,-2.17161023787787E-15)) ;
#43559 = DIRECTION('center_axis',(-2.17161023787787E-15,3.92492613217813E-28,
1.)) ;
#43560 = DIRECTION('ref_axis',(-1.,4.92531066966514E-14,-2.17161023787787E-15)) ;
#43561 = DIRECTION('center_axis',(-1.37192483171701E-13,-1.,9.45640122022591E-29)) ;
#43562 = DIRECTION('ref_axis',(-1.,1.37192483171701E-13,-2.85817673274378E-15)) ;
#43563 = DIRECTION('center_axis',(-2.1716102378779E-15,3.83815143260386E-28,
1.)) ;
#43564 = DIRECTION('ref_axis',(-1.,-9.69015809248849E-15,-2.1716102378779E-15)) ;
#43565 = DIRECTION('center_axis',(2.1716102378779E-15,-3.83815143260386E-28,
-1.)) ;
#43566 = DIRECTION('ref_axis',(-1.,-7.3303373675338E-16,-2.1716102378779E-15)) ;
#43567 = DIRECTION('',(-2.1716102378779E-15,3.83815143260386E-28,1.)) ;
#43568 = DIRECTION('center_axis',(2.1716102378779E-15,-3.83815143260386E-28,
-1.)) ;
#43569 = DIRECTION('ref_axis',(-1.,1.59141680100251E-13,-2.48658875156642E-15)) ;
#43570 = DIRECTION('center_axis',(1.49195325093984E-13,1.,-5.98210478427684E-29)) ;
#43571 = DIRECTION('ref_axis',(1.,-1.49195325093984E-13,1.554117969729E-15)) ;
#43572 = DIRECTION('center_axis',(-1.66533453692587E-16,-1.,3.82991969484897E-28)) ;
#43573 = DIRECTION('ref_axis',(2.1716102378779E-15,-3.83353615237885E-28,
-1.)) ;
#43574 = DIRECTION('',(-2.17161023787787E-15,3.83420712807771E-28,1.)) ;
#43575 = DIRECTION('center_axis',(2.17161023787787E-15,-3.83420712807771E-28,
-1.)) ;
#43576 = DIRECTION('ref_axis',(-0.707106781186552,-0.707106781186543,-1.53556032529731E-15)) ;
#43577 = DIRECTION('center_axis',(4.54195640846217E-14,-1.66321791214601E-16,
1.)) ;
#43578 = DIRECTION('ref_axis',(1.75658099177411E-13,1.,1.66321791206623E-16)) ;
#43579 = DIRECTION('center_axis',(-2.16239769233719E-14,8.31608956071042E-17,
-1.)) ;
#43580 = DIRECTION('ref_axis',(1.,-9.64599832246215E-47,-2.16239769233719E-14)) ;
#43581 = DIRECTION('center_axis',(-2.17161023787787E-15,3.92492613217813E-28,
1.)) ;
#43582 = DIRECTION('ref_axis',(1.,-1.46338648716481E-13,2.28654138619502E-15)) ;
#43583 = DIRECTION('center_axis',(-2.17161023787787E-15,3.92492613217813E-28,
1.)) ;
#43584 = DIRECTION('ref_axis',(-1.,4.92531066966514E-14,-2.17161023787787E-15)) ;
#43585 = DIRECTION('center_axis',(-2.17161023787787E-15,3.92492613217813E-28,
1.)) ;
#43586 = DIRECTION('ref_axis',(-1.,4.92531066966514E-14,-2.17161023787787E-15)) ;
#43587 = DIRECTION('center_axis',(-1.37192483171701E-13,-1.,9.45640122022591E-29)) ;
#43588 = DIRECTION('ref_axis',(-1.,1.37192483171701E-13,-2.85817673274378E-15)) ;
#43589 = DIRECTION('center_axis',(-2.1716102378779E-15,3.83815143260386E-28,
1.)) ;
#43590 = DIRECTION('ref_axis',(-1.,-9.69015809248849E-15,-2.1716102378779E-15)) ;
#43591 = DIRECTION('center_axis',(2.1716102378779E-15,-3.83815143260386E-28,
-1.)) ;
#43592 = DIRECTION('ref_axis',(-1.,-7.3303373675338E-16,-2.1716102378779E-15)) ;
#43593 = DIRECTION('',(-2.1716102378779E-15,3.83815143260386E-28,1.)) ;
#43594 = DIRECTION('center_axis',(2.1716102378779E-15,-3.83815143260386E-28,
-1.)) ;
#43595 = DIRECTION('ref_axis',(-1.,1.59141680100251E-13,-2.48658875156642E-15)) ;
#43596 = DIRECTION('center_axis',(1.49195325093984E-13,1.,-5.98210478427684E-29)) ;
#43597 = DIRECTION('ref_axis',(1.,-1.49195325093984E-13,1.554117969729E-15)) ;
#43598 = DIRECTION('center_axis',(-1.66533453692587E-16,-1.,3.82991969484897E-28)) ;
#43599 = DIRECTION('ref_axis',(2.1716102378779E-15,-3.83353615237885E-28,
-1.)) ;
#43600 = DIRECTION('',(-2.17161023787787E-15,3.83420712807771E-28,1.)) ;
#43601 = DIRECTION('center_axis',(2.17161023787787E-15,-3.83420712807771E-28,
-1.)) ;
#43602 = DIRECTION('ref_axis',(-0.707106781186552,-0.707106781186543,-1.53556032529731E-15)) ;
#43603 = DIRECTION('center_axis',(4.54195640846217E-14,-1.66321791214601E-16,
1.)) ;
#43604 = DIRECTION('ref_axis',(1.75658099177411E-13,1.,1.66321791206623E-16)) ;
#43605 = DIRECTION('center_axis',(-2.16239769233719E-14,8.31608956071042E-17,
-1.)) ;
#43606 = DIRECTION('ref_axis',(1.,-9.64599832246215E-47,-2.16239769233719E-14)) ;
#43607 = DIRECTION('center_axis',(-2.17161023787787E-15,3.92492613217813E-28,
1.)) ;
#43608 = DIRECTION('ref_axis',(1.,-1.46338648716481E-13,2.28654138619502E-15)) ;
#43609 = DIRECTION('center_axis',(-2.17161023787787E-15,3.92492613217813E-28,
1.)) ;
#43610 = DIRECTION('ref_axis',(-1.,4.92531066966514E-14,-2.17161023787787E-15)) ;
#43611 = DIRECTION('center_axis',(-2.17161023787787E-15,3.92492613217813E-28,
1.)) ;
#43612 = DIRECTION('ref_axis',(-1.,4.92531066966514E-14,-2.17161023787787E-15)) ;
#43613 = DIRECTION('center_axis',(-1.37192483171701E-13,-1.,9.45640122022591E-29)) ;
#43614 = DIRECTION('ref_axis',(-1.,1.37192483171701E-13,-2.85817673274378E-15)) ;
#43615 = DIRECTION('center_axis',(-2.1716102378779E-15,3.83815143260386E-28,
1.)) ;
#43616 = DIRECTION('ref_axis',(-1.,-9.69015809248849E-15,-2.1716102378779E-15)) ;
#43617 = DIRECTION('center_axis',(2.1716102378779E-15,-3.83815143260386E-28,
-1.)) ;
#43618 = DIRECTION('ref_axis',(-1.,-7.3303373675338E-16,-2.1716102378779E-15)) ;
#43619 = DIRECTION('',(-2.1716102378779E-15,3.83815143260386E-28,1.)) ;
#43620 = DIRECTION('center_axis',(2.1716102378779E-15,-3.83815143260386E-28,
-1.)) ;
#43621 = DIRECTION('ref_axis',(-1.,1.59141680100251E-13,-2.48658875156642E-15)) ;
#43622 = DIRECTION('center_axis',(1.49195325093984E-13,1.,-5.98210478427684E-29)) ;
#43623 = DIRECTION('ref_axis',(1.,-1.49195325093984E-13,1.554117969729E-15)) ;
#43624 = DIRECTION('center_axis',(-1.66533453692587E-16,-1.,3.82991969484897E-28)) ;
#43625 = DIRECTION('ref_axis',(2.1716102378779E-15,-3.83353615237885E-28,
-1.)) ;
#43626 = DIRECTION('',(-2.17161023787787E-15,3.83420712807771E-28,1.)) ;
#43627 = DIRECTION('center_axis',(2.17161023787787E-15,-3.83420712807771E-28,
-1.)) ;
#43628 = DIRECTION('ref_axis',(-0.707106781186552,-0.707106781186543,-1.53556032529731E-15)) ;
#43629 = DIRECTION('center_axis',(-2.17161023787787E-15,3.92492613217813E-28,
1.)) ;
#43630 = DIRECTION('ref_axis',(1.,-1.46338648716481E-13,2.28654138619502E-15)) ;
#43631 = DIRECTION('center_axis',(-2.17161023787787E-15,3.92492613217813E-28,
1.)) ;
#43632 = DIRECTION('ref_axis',(-1.,4.92531066966514E-14,-2.17161023787787E-15)) ;
#43633 = DIRECTION('center_axis',(-2.17161023787787E-15,3.92492613217813E-28,
1.)) ;
#43634 = DIRECTION('ref_axis',(-1.,4.92531066966514E-14,-2.17161023787787E-15)) ;
#43635 = DIRECTION('center_axis',(-1.37192483171701E-13,-1.,9.45640122022591E-29)) ;
#43636 = DIRECTION('ref_axis',(-1.,1.37192483171701E-13,-2.85817673274378E-15)) ;
#43637 = DIRECTION('center_axis',(-2.1716102378779E-15,3.83815143260386E-28,
1.)) ;
#43638 = DIRECTION('ref_axis',(-1.,-9.69015809248849E-15,-2.1716102378779E-15)) ;
#43639 = DIRECTION('center_axis',(2.1716102378779E-15,-3.83815143260386E-28,
-1.)) ;
#43640 = DIRECTION('ref_axis',(-1.,-7.3303373675338E-16,-2.1716102378779E-15)) ;
#43641 = DIRECTION('',(-2.1716102378779E-15,3.83815143260386E-28,1.)) ;
#43642 = DIRECTION('center_axis',(2.1716102378779E-15,-3.83815143260386E-28,
-1.)) ;
#43643 = DIRECTION('ref_axis',(-1.,1.59141680100251E-13,-2.48658875156642E-15)) ;
#43644 = DIRECTION('center_axis',(1.49195325093984E-13,1.,-5.98210478427684E-29)) ;
#43645 = DIRECTION('ref_axis',(1.,-1.49195325093984E-13,1.554117969729E-15)) ;
#43646 = DIRECTION('center_axis',(-1.76424026290696E-13,-0.999847695156391,
-0.01745240643728)) ;
#43647 = DIRECTION('ref_axis',(4.23469899241728E-14,-0.01745240643728,0.999847695156391)) ;
#43648 = DIRECTION('',(4.23469899241728E-14,-0.01745240643728,0.999847695156391)) ;
#43649 = DIRECTION('center_axis',(1.,-1.75658099177411E-13,-4.54195640846217E-14)) ;
#43650 = DIRECTION('ref_axis',(-4.54195640846217E-14,1.66321791214601E-16,
-1.)) ;
#43651 = DIRECTION('center_axis',(-2.1716102378779E-15,3.83815143260386E-28,
1.)) ;
#43652 = DIRECTION('ref_axis',(-0.707106781186643,0.707106781186452,-1.53556032529807E-15)) ;
#43653 = DIRECTION('',(-2.1716102378779E-15,3.83815143260386E-28,1.)) ;
#43654 = DIRECTION('center_axis',(-1.,1.66533453692966E-16,-2.1716102378779E-15)) ;
#43655 = DIRECTION('ref_axis',(1.66533453692966E-16,1.,-3.82783884128008E-28)) ;
#43656 = DIRECTION('',(2.1716102378779E-15,-3.83420712807775E-28,-1.)) ;
#43657 = DIRECTION('center_axis',(2.1716102378779E-15,-3.83420712807775E-28,
-1.)) ;
#43658 = DIRECTION('ref_axis',(-0.707106781186452,-0.707106781186643,-1.53556032529712E-15)) ;
#43659 = DIRECTION('',(-2.1716102378779E-15,3.83420712807775E-28,1.)) ;
#43660 = DIRECTION('center_axis',(-1.66533453692587E-16,-1.,3.82991969484897E-28)) ;
#43661 = DIRECTION('ref_axis',(2.1716102378779E-15,-3.83353615237885E-28,
-1.)) ;
#43662 = DIRECTION('center_axis',(-2.17161023787787E-15,3.83815143260382E-28,
1.)) ;
#43663 = DIRECTION('ref_axis',(-0.707106781186643,0.707106781186452,-1.53556032529805E-15)) ;
#43664 = DIRECTION('center_axis',(-2.1716102378779E-15,3.83815143260386E-28,
1.)) ;
#43665 = DIRECTION('ref_axis',(-0.707106781186643,0.707106781186452,-1.53556032529807E-15)) ;
#43666 = DIRECTION('',(-2.1716102378779E-15,3.83815143260386E-28,1.)) ;
#43667 = DIRECTION('center_axis',(-1.,1.66533453692966E-16,-2.1716102378779E-15)) ;
#43668 = DIRECTION('ref_axis',(1.66533453692966E-16,1.,-3.82783884128008E-28)) ;
#43669 = DIRECTION('',(2.1716102378779E-15,-3.83420712807775E-28,-1.)) ;
#43670 = DIRECTION('center_axis',(2.1716102378779E-15,-3.83420712807775E-28,
-1.)) ;
#43671 = DIRECTION('ref_axis',(-0.707106781186452,-0.707106781186643,-1.53556032529712E-15)) ;
#43672 = DIRECTION('',(-2.1716102378779E-15,3.83420712807775E-28,1.)) ;
#43673 = DIRECTION('center_axis',(-1.66533453692587E-16,-1.,3.82991969484897E-28)) ;
#43674 = DIRECTION('ref_axis',(2.1716102378779E-15,-3.83353615237885E-28,
-1.)) ;
#43675 = DIRECTION('center_axis',(-2.17161023787787E-15,3.83815143260382E-28,
1.)) ;
#43676 = DIRECTION('ref_axis',(-0.707106781186643,0.707106781186452,-1.53556032529805E-15)) ;
#43677 = DIRECTION('center_axis',(-2.1716102378779E-15,3.83815143260386E-28,
1.)) ;
#43678 = DIRECTION('ref_axis',(-0.707106781186643,0.707106781186452,-1.53556032529807E-15)) ;
#43679 = DIRECTION('',(-2.1716102378779E-15,3.83815143260386E-28,1.)) ;
#43680 = DIRECTION('center_axis',(-1.,1.66533453692966E-16,-2.1716102378779E-15)) ;
#43681 = DIRECTION('ref_axis',(1.66533453692966E-16,1.,-3.82783884128008E-28)) ;
#43682 = DIRECTION('',(2.1716102378779E-15,-3.83420712807775E-28,-1.)) ;
#43683 = DIRECTION('center_axis',(2.1716102378779E-15,-3.83420712807775E-28,
-1.)) ;
#43684 = DIRECTION('ref_axis',(-0.707106781186452,-0.707106781186643,-1.53556032529712E-15)) ;
#43685 = DIRECTION('',(-2.1716102378779E-15,3.83420712807775E-28,1.)) ;
#43686 = DIRECTION('center_axis',(-1.66533453692587E-16,-1.,3.82991969484897E-28)) ;
#43687 = DIRECTION('ref_axis',(2.1716102378779E-15,-3.83353615237885E-28,
-1.)) ;
#43688 = DIRECTION('center_axis',(-2.17161023787787E-15,3.83815143260382E-28,
1.)) ;
#43689 = DIRECTION('ref_axis',(-0.707106781186643,0.707106781186452,-1.53556032529805E-15)) ;
#43690 = DIRECTION('center_axis',(-2.1716102378779E-15,3.83815143260386E-28,
1.)) ;
#43691 = DIRECTION('ref_axis',(-0.707106781186643,0.707106781186452,-1.53556032529807E-15)) ;
#43692 = DIRECTION('',(-2.1716102378779E-15,3.83815143260386E-28,1.)) ;
#43693 = DIRECTION('center_axis',(-1.,1.66533453692966E-16,-2.1716102378779E-15)) ;
#43694 = DIRECTION('ref_axis',(1.66533453692966E-16,1.,-3.82783884128008E-28)) ;
#43695 = DIRECTION('',(2.1716102378779E-15,-3.83420712807775E-28,-1.)) ;
#43696 = DIRECTION('center_axis',(2.1716102378779E-15,-3.83420712807775E-28,
-1.)) ;
#43697 = DIRECTION('ref_axis',(-0.707106781186452,-0.707106781186643,-1.53556032529712E-15)) ;
#43698 = DIRECTION('',(-2.1716102378779E-15,3.83420712807775E-28,1.)) ;
#43699 = DIRECTION('center_axis',(-1.66533453692587E-16,-1.,3.82991969484897E-28)) ;
#43700 = DIRECTION('ref_axis',(2.1716102378779E-15,-3.83353615237885E-28,
-1.)) ;
#43701 = DIRECTION('center_axis',(-2.17161023787787E-15,3.83815143260382E-28,
1.)) ;
#43702 = DIRECTION('ref_axis',(-0.707106781186643,0.707106781186452,-1.53556032529805E-15)) ;
#43703 = DIRECTION('center_axis',(-2.1716102378779E-15,3.83815143260386E-28,
1.)) ;
#43704 = DIRECTION('ref_axis',(-0.707106781186643,0.707106781186452,-1.53556032529807E-15)) ;
#43705 = DIRECTION('',(-2.1716102378779E-15,3.83815143260386E-28,1.)) ;
#43706 = DIRECTION('center_axis',(-1.,1.66533453692966E-16,-2.1716102378779E-15)) ;
#43707 = DIRECTION('ref_axis',(1.66533453692966E-16,1.,-3.82783884128008E-28)) ;
#43708 = DIRECTION('',(2.1716102378779E-15,-3.83420712807775E-28,-1.)) ;
#43709 = DIRECTION('center_axis',(2.1716102378779E-15,-3.83420712807775E-28,
-1.)) ;
#43710 = DIRECTION('ref_axis',(-0.707106781186452,-0.707106781186643,-1.53556032529712E-15)) ;
#43711 = DIRECTION('',(-2.1716102378779E-15,3.83420712807775E-28,1.)) ;
#43712 = DIRECTION('center_axis',(-1.66533453692587E-16,-1.,3.82991969484897E-28)) ;
#43713 = DIRECTION('ref_axis',(2.1716102378779E-15,-3.83353615237885E-28,
-1.)) ;
#43714 = DIRECTION('center_axis',(-2.17161023787787E-15,3.83815143260382E-28,
1.)) ;
#43715 = DIRECTION('ref_axis',(-0.707106781186643,0.707106781186452,-1.53556032529805E-15)) ;
#43716 = DIRECTION('center_axis',(-2.1716102378779E-15,3.83815143260386E-28,
1.)) ;
#43717 = DIRECTION('ref_axis',(-0.707106781186643,0.707106781186452,-1.53556032529807E-15)) ;
#43718 = DIRECTION('',(-2.1716102378779E-15,3.83815143260386E-28,1.)) ;
#43719 = DIRECTION('center_axis',(-1.,1.66533453692966E-16,-2.1716102378779E-15)) ;
#43720 = DIRECTION('ref_axis',(1.66533453692966E-16,1.,-3.82783884128008E-28)) ;
#43721 = DIRECTION('',(2.1716102378779E-15,-3.83420712807775E-28,-1.)) ;
#43722 = DIRECTION('center_axis',(2.1716102378779E-15,-3.83420712807775E-28,
-1.)) ;
#43723 = DIRECTION('ref_axis',(-0.707106781186452,-0.707106781186643,-1.53556032529712E-15)) ;
#43724 = DIRECTION('',(-2.1716102378779E-15,3.83420712807775E-28,1.)) ;
#43725 = DIRECTION('center_axis',(-1.66533453692587E-16,-1.,3.82991969484897E-28)) ;
#43726 = DIRECTION('ref_axis',(2.1716102378779E-15,-3.83353615237885E-28,
-1.)) ;
#43727 = DIRECTION('center_axis',(-2.17161023787787E-15,3.83815143260382E-28,
1.)) ;
#43728 = DIRECTION('ref_axis',(-0.707106781186643,0.707106781186452,-1.53556032529805E-15)) ;
#43729 = DIRECTION('center_axis',(-2.1716102378779E-15,3.83815143260386E-28,
1.)) ;
#43730 = DIRECTION('ref_axis',(-0.707106781186643,0.707106781186452,-1.53556032529807E-15)) ;
#43731 = DIRECTION('',(-2.1716102378779E-15,3.83815143260386E-28,1.)) ;
#43732 = DIRECTION('center_axis',(-1.,1.66533453692966E-16,-2.1716102378779E-15)) ;
#43733 = DIRECTION('ref_axis',(1.66533453692966E-16,1.,-3.82783884128008E-28)) ;
#43734 = DIRECTION('',(2.1716102378779E-15,-3.83420712807775E-28,-1.)) ;
#43735 = DIRECTION('center_axis',(2.1716102378779E-15,-3.83420712807775E-28,
-1.)) ;
#43736 = DIRECTION('ref_axis',(-0.707106781186452,-0.707106781186643,-1.53556032529712E-15)) ;
#43737 = DIRECTION('',(-2.1716102378779E-15,3.83420712807775E-28,1.)) ;
#43738 = DIRECTION('center_axis',(-1.66533453692587E-16,-1.,3.82991969484897E-28)) ;
#43739 = DIRECTION('ref_axis',(2.1716102378779E-15,-3.83353615237885E-28,
-1.)) ;
#43740 = DIRECTION('center_axis',(-2.17161023787787E-15,3.83815143260382E-28,
1.)) ;
#43741 = DIRECTION('ref_axis',(-0.707106781186643,0.707106781186452,-1.53556032529805E-15)) ;
#43742 = DIRECTION('center_axis',(-2.1716102378779E-15,3.83815143260386E-28,
1.)) ;
#43743 = DIRECTION('ref_axis',(-0.707106781186643,0.707106781186452,-1.53556032529807E-15)) ;
#43744 = DIRECTION('',(-2.1716102378779E-15,3.83815143260386E-28,1.)) ;
#43745 = DIRECTION('center_axis',(-1.,1.66533453692966E-16,-2.1716102378779E-15)) ;
#43746 = DIRECTION('ref_axis',(1.66533453692966E-16,1.,-3.82783884128008E-28)) ;
#43747 = DIRECTION('',(2.1716102378779E-15,-3.83420712807775E-28,-1.)) ;
#43748 = DIRECTION('center_axis',(2.1716102378779E-15,-3.83420712807775E-28,
-1.)) ;
#43749 = DIRECTION('ref_axis',(-0.707106781186452,-0.707106781186643,-1.53556032529712E-15)) ;
#43750 = DIRECTION('',(-2.1716102378779E-15,3.83420712807775E-28,1.)) ;
#43751 = DIRECTION('center_axis',(-1.66533453692587E-16,-1.,3.82991969484897E-28)) ;
#43752 = DIRECTION('ref_axis',(2.1716102378779E-15,-3.83353615237885E-28,
-1.)) ;
#43753 = DIRECTION('center_axis',(-2.17161023787787E-15,3.83815143260382E-28,
1.)) ;
#43754 = DIRECTION('ref_axis',(-0.707106781186643,0.707106781186452,-1.53556032529805E-15)) ;
#43755 = DIRECTION('axis',(0.,0.,1.)) ;
#43756 = DIRECTION('refdir',(1.,0.,0.)) ;
#43757 = DIRECTION('axis',(0.,0.,1.)) ;
#43758 = DIRECTION('refdir',(1.,0.,0.)) ;
#43759 = DIRECTION('center_axis',(-1.05010212975467E-14,-2.51767111096099E-14,
-1.)) ;
#43760 = DIRECTION('ref_axis',(-2.51083656231336E-15,1.,-2.51767111096099E-14)) ;
#43761 = DIRECTION('',(1.05010212975467E-14,2.51767111096099E-14,1.)) ;
#43762 = DIRECTION('center_axis',(-1.05010212975467E-14,-2.51767111096099E-14,
-1.)) ;
#43763 = DIRECTION('ref_axis',(-2.51083656231336E-15,1.,-2.51767111096099E-14)) ;
#43764 = DIRECTION('',(1.05010212975467E-14,2.51767111096099E-14,1.)) ;
#43765 = DIRECTION('center_axis',(-1.05010212975467E-14,-2.51767111096099E-14,
-1.)) ;
#43766 = DIRECTION('ref_axis',(-2.51083656231336E-15,1.,-2.51767111096099E-14)) ;
#43767 = DIRECTION('',(1.05010212975467E-14,2.51767111096099E-14,1.)) ;
#43768 = DIRECTION('center_axis',(-1.05010212975467E-14,-2.51767111096099E-14,
-1.)) ;
#43769 = DIRECTION('ref_axis',(-2.51083656231336E-15,1.,-2.51767111096099E-14)) ;
#43770 = DIRECTION('',(1.05010212975467E-14,2.51767111096099E-14,1.)) ;
#43771 = DIRECTION('center_axis',(-1.05010212975467E-14,-2.51767111096099E-14,
-1.)) ;
#43772 = DIRECTION('ref_axis',(-2.51083656231336E-15,1.,-2.51767111096099E-14)) ;
#43773 = DIRECTION('',(1.05010212975467E-14,2.51767111096099E-14,1.)) ;
#43774 = DIRECTION('center_axis',(-1.05010212975467E-14,-2.51767111096099E-14,
-1.)) ;
#43775 = DIRECTION('ref_axis',(-2.51083656231336E-15,1.,-2.51767111096099E-14)) ;
#43776 = DIRECTION('',(1.05010212975467E-14,2.51767111096099E-14,1.)) ;
#43777 = DIRECTION('center_axis',(-1.05010212975467E-14,-2.51767111096099E-14,
-1.)) ;
#43778 = DIRECTION('ref_axis',(-2.51083656231336E-15,1.,-2.51767111096099E-14)) ;
#43779 = DIRECTION('',(1.05010212975467E-14,2.51767111096099E-14,1.)) ;
#43780 = DIRECTION('center_axis',(-1.05010212975467E-14,-2.51767111096099E-14,
-1.)) ;
#43781 = DIRECTION('ref_axis',(-2.51083656231336E-15,1.,-2.51767111096099E-14)) ;
#43782 = DIRECTION('',(1.05010212975467E-14,2.51767111096099E-14,1.)) ;
#43783 = DIRECTION('center_axis',(-2.0775199119216E-14,2.60214901359506E-13,
-1.)) ;
#43784 = DIRECTION('ref_axis',(-0.15733882491533,-0.987544679583796,-2.53705095969203E-13)) ;
#43785 = DIRECTION('center_axis',(0.,0.,1.)) ;
#43786 = DIRECTION('ref_axis',(1.,0.,0.)) ;
#43787 = DIRECTION('',(0.,0.,-1.)) ;
#43788 = DIRECTION('center_axis',(0.,0.,1.)) ;
#43789 = DIRECTION('ref_axis',(1.,0.,0.)) ;
#43790 = DIRECTION('center_axis',(0.,0.,1.)) ;
#43791 = DIRECTION('ref_axis',(1.,0.,0.)) ;
#43792 = DIRECTION('',(0.,0.,-1.)) ;
#43793 = DIRECTION('center_axis',(0.,0.,1.)) ;
#43794 = DIRECTION('ref_axis',(1.,0.,0.)) ;
#43795 = DIRECTION('',(0.,0.,-1.)) ;
#43796 = DIRECTION('center_axis',(0.,0.,1.)) ;
#43797 = DIRECTION('ref_axis',(1.,0.,0.)) ;
#43798 = DIRECTION('',(0.,0.,-1.)) ;
#43799 = DIRECTION('center_axis',(0.,0.,1.)) ;
#43800 = DIRECTION('ref_axis',(1.,0.,0.)) ;
#43801 = DIRECTION('',(0.,0.,-1.)) ;
#43802 = DIRECTION('center_axis',(0.,0.,1.)) ;
#43803 = DIRECTION('ref_axis',(1.,0.,0.)) ;
#43804 = DIRECTION('',(0.,0.,-1.)) ;
#43805 = DIRECTION('center_axis',(0.,0.,1.)) ;
#43806 = DIRECTION('ref_axis',(1.,0.,0.)) ;
#43807 = DIRECTION('',(0.,0.,-1.)) ;
#43808 = DIRECTION('center_axis',(0.,0.,1.)) ;
#43809 = DIRECTION('ref_axis',(1.,0.,0.)) ;
#43810 = DIRECTION('center_axis',(0.,0.,1.)) ;
#43811 = DIRECTION('ref_axis',(0.38268343236509,0.923879532511287,0.)) ;
#43812 = DIRECTION('center_axis',(-1.05010212975467E-14,-2.51767111096099E-14,
-1.)) ;
#43813 = DIRECTION('ref_axis',(-2.51083656231336E-15,1.,-2.51767111096099E-14)) ;
#43814 = DIRECTION('center_axis',(-2.0775199119216E-14,2.60214901359506E-13,
-1.)) ;
#43815 = DIRECTION('ref_axis',(-0.15733882491533,-0.987544679583796,-2.53705095969203E-13)) ;
#43816 = DIRECTION('center_axis',(0.431213875666469,0.456273348170848,0.778376017861333)) ;
#43817 = DIRECTION('ref_axis',(0.726783280612686,-0.686866845190436,6.1949686306476E-16)) ;
#43818 = DIRECTION('center_axis',(0.78416251235965,0.382514104091566,0.488643136021401)) ;
#43819 = DIRECTION('ref_axis',(0.438419748448915,-0.898770340059122,1.79364045353587E-16)) ;
#43820 = DIRECTION('center_axis',(0.998769717110461,5.59307539516625E-11,
0.0495888312333447)) ;
#43821 = DIRECTION('ref_axis',(5.59996493620929E-11,-1.,1.83348176602366E-27)) ;
#43822 = DIRECTION('center_axis',(1.,0.,-2.77555756156289E-14)) ;
#43823 = DIRECTION('ref_axis',(0.,-1.,0.)) ;
#43824 = DIRECTION('center_axis',(-0.186904608536419,-0.982127159191521,0.0222015874711655)) ;
#43825 = DIRECTION('ref_axis',(0.982190610687812,-0.187262695295954,-0.0153064439762371)) ;
#43826 = DIRECTION('center_axis',(0.,1.,0.)) ;
#43827 = DIRECTION('ref_axis',(0.999909707661035,0.,0.0134378765146677)) ;
#43828 = DIRECTION('center_axis',(-1.,-1.11022302462516E-14,1.80671994062472E-14)) ;
#43829 = DIRECTION('ref_axis',(-5.55111512312583E-15,-0.685234561324452,-0.728322453290084)) ;
#43830 = DIRECTION('',(0.999999958174326,2.12460885215939E-8,-0.00028922542396849)) ;
#43831 = DIRECTION('center_axis',(-1.,0.,-6.17096200035076E-15)) ;
#43832 = DIRECTION('ref_axis',(5.5511151231258E-15,-0.436809046170809,-0.899554254719163)) ;
#43833 = DIRECTION('',(1.,0.,0.)) ;
#43834 = DIRECTION('',(1.,0.,0.)) ;
#43835 = DIRECTION('center_axis',(-0.202274762387573,0.9793288112279,0.)) ;
#43836 = DIRECTION('ref_axis',(-0.81902520534733,-0.169164969825963,0.548252611475353)) ;
#43837 = DIRECTION('center_axis',(-0.796046528300715,-0.164065815817298,0.582573886181473)) ;
#43838 = DIRECTION('ref_axis',(0.60325914550266,-0.292808781282497,0.741849998969643)) ;
#43839 = DIRECTION('center_axis',(0.,4.79371819681639E-16,1.)) ;
#43840 = DIRECTION('ref_axis',(0.,-1.,5.18039323243001E-16)) ;
#43841 = DIRECTION('center_axis',(0.,4.79371819681639E-16,1.)) ;
#43842 = DIRECTION('ref_axis',(0.,-1.,4.79371819681639E-16)) ;
#43843 = DIRECTION('center_axis',(0.79604652830067,0.164065815817297,0.582573886181535)) ;
#43844 = DIRECTION('ref_axis',(0.603259145417311,-0.292808782928713,-0.741849998389284)) ;
#43845 = DIRECTION('center_axis',(0.,2.3968590984082E-16,1.)) ;
#43846 = DIRECTION('ref_axis',(1.,2.46314898699588E-16,-5.90382106021602E-32)) ;
#43847 = DIRECTION('center_axis',(0.796046712982956,-0.164065889510482,0.582573613072345)) ;
#43848 = DIRECTION('ref_axis',(0.600011337901856,0.340121293701446,-0.724088323314276)) ;
#43849 = DIRECTION('center_axis',(0.,4.79371819681639E-16,1.)) ;
#43850 = DIRECTION('ref_axis',(0.,-1.,4.79371819681639E-16)) ;
#43851 = DIRECTION('center_axis',(0.,2.3968590984082E-16,1.)) ;
#43852 = DIRECTION('ref_axis',(-1.,-1.39827749563623E-16,3.35147413751513E-32)) ;
#43853 = DIRECTION('center_axis',(-0.796046712982948,0.164065889510474,0.582573613072357)) ;
#43854 = DIRECTION('ref_axis',(0.60001133781454,0.340121294720491,0.724088322907961)) ;
#43855 = DIRECTION('center_axis',(0.,4.79371819681639E-16,1.)) ;
#43856 = DIRECTION('ref_axis',(0.,-1.,4.79371819681639E-16)) ;
#43857 = DIRECTION('center_axis',(-1.,-1.22464679914735E-16,5.87061164574561E-32)) ;
#43858 = DIRECTION('ref_axis',(-1.22464679914735E-16,1.,-3.23774577026876E-16)) ;
#43859 = DIRECTION('center_axis',(0.,4.79371819681639E-16,1.)) ;
#43860 = DIRECTION('ref_axis',(0.,-1.,4.79371819681639E-16)) ;
#43861 = DIRECTION('center_axis',(0.,2.3968590984082E-16,1.)) ;
#43862 = DIRECTION('ref_axis',(-1.,-9.00424887691599E-15,0.)) ;
#43863 = DIRECTION('center_axis',(0.,0.,-1.)) ;
#43864 = DIRECTION('ref_axis',(-1.,-1.22464679914735E-16,0.)) ;
#43865 = DIRECTION('center_axis',(-0.186904608537131,0.982127159190804,0.0222015874969168)) ;
#43866 = DIRECTION('ref_axis',(0.982190613229004,0.187262692788182,-0.0153063115920336)) ;
#43867 = DIRECTION('center_axis',(0.202274762386253,0.979328811228172,-1.88126629740374E-12)) ;
#43868 = DIRECTION('ref_axis',(-0.81902520534735,0.16916496982587,0.548252611475352)) ;
#43869 = DIRECTION('center_axis',(0.431213875666332,-0.45627334817079,0.778376017861444)) ;
#43870 = DIRECTION('ref_axis',(0.813949131457667,-0.175495689147709,-0.553794252850172)) ;
#43871 = DIRECTION('center_axis',(0.784162512362696,-0.38251410408934,0.488643136018255)) ;
#43872 = DIRECTION('ref_axis',(0.490111180257792,-0.101229659940977,-0.865761853476201)) ;
#43873 = DIRECTION('center_axis',(0.998769717110462,-5.59307539516625E-11,
0.0495888312333392)) ;
#43874 = DIRECTION('ref_axis',(0.0495862470879903,-0.0102088265337294,-0.998717669794889)) ;
#43875 = DIRECTION('center_axis',(1.,-5.55111512312579E-15,1.65423230669149E-12)) ;
#43876 = DIRECTION('ref_axis',(1.65423230669148E-12,-1.57374113740616E-12,
-1.)) ;
#43877 = DIRECTION('center_axis',(0.,-1.,0.)) ;
#43878 = DIRECTION('ref_axis',(0.999909707872585,0.,0.0134378607732635)) ;
#43879 = DIRECTION('',(-0.99999997985201,1.21446614212548E-8,0.000200738584200413)) ;
#43880 = DIRECTION('center_axis',(-1.,-5.55111512312572E-15,7.09951135811084E-14)) ;
#43881 = DIRECTION('ref_axis',(-5.55111512312572E-15,1.,-7.52353615125298E-45)) ;
#43882 = DIRECTION('',(-1.,0.,0.)) ;
#43883 = DIRECTION('center_axis',(-1.,0.,-6.17096200035069E-15)) ;
#43884 = DIRECTION('ref_axis',(0.,1.,0.)) ;
#43885 = DIRECTION('',(-1.,0.,0.)) ;
#43886 = DIRECTION('center_axis',(0.,0.,1.)) ;
#43887 = DIRECTION('ref_axis',(-0.793390388649525,-0.608713143605883,0.)) ;
#43888 = DIRECTION('',(0.,0.,1.)) ;
#43889 = DIRECTION('center_axis',(0.,0.,-1.)) ;
#43890 = DIRECTION('ref_axis',(0.,-1.,0.)) ;
#43891 = DIRECTION('',(0.,0.,-1.)) ;
#43892 = DIRECTION('center_axis',(0.,-1.,0.)) ;
#43893 = DIRECTION('ref_axis',(0.,0.,-1.)) ;
#43894 = DIRECTION('',(-1.,0.,0.)) ;
#43895 = DIRECTION('',(0.0942752822069817,0.,-0.995546167269401)) ;
#43896 = DIRECTION('center_axis',(0.,1.,0.)) ;
#43897 = DIRECTION('ref_axis',(-0.371772155637639,0.,0.928324008249568)) ;
#43898 = DIRECTION('center_axis',(-0.431213875666459,-0.456273348170838,0.778376017861345)) ;
#43899 = DIRECTION('ref_axis',(-0.726783280612687,0.686866845190435,-1.43341183094753E-17)) ;
#43900 = DIRECTION('center_axis',(-0.784162512359631,-0.38251410409158,0.48864313602142)) ;
#43901 = DIRECTION('ref_axis',(-0.438419748448937,0.898770340059111,-2.46822861618048E-16)) ;
#43902 = DIRECTION('center_axis',(-0.998769717110462,-5.59362982373437E-11,
0.0495888312333393)) ;
#43903 = DIRECTION('ref_axis',(-5.6005200477216E-11,1.,-3.39348476170366E-27)) ;
#43904 = DIRECTION('center_axis',(-1.,2.22044604925031E-14,-1.11022302462516E-14)) ;
#43905 = DIRECTION('ref_axis',(2.22044604925031E-14,1.,1.68155815718967E-44)) ;
#43906 = DIRECTION('center_axis',(0.186904608536329,0.982127159191646,0.0222015874663972)) ;
#43907 = DIRECTION('ref_axis',(0.982190613371512,-0.187262692646365,0.0153063041824444)) ;
#43908 = DIRECTION('center_axis',(5.36677285303109E-14,-1.,2.16337548812628E-12)) ;
#43909 = DIRECTION('ref_axis',(0.999909707696494,2.45917157912175E-14,-0.0134378738761801)) ;
#43910 = DIRECTION('center_axis',(1.,-1.11022302462516E-14,-1.04454171887006E-14)) ;
#43911 = DIRECTION('ref_axis',(1.27702679854493E-29,0.685234561324431,-0.728322453290103)) ;
#43912 = DIRECTION('',(-0.999999978906491,-1.27145189198587E-8,-0.000205394783225332)) ;
#43913 = DIRECTION('center_axis',(1.,0.,-1.85128860010521E-14)) ;
#43914 = DIRECTION('ref_axis',(-1.66533453693773E-14,0.436809046170802,-0.899554254719166)) ;
#43915 = DIRECTION('',(-1.,0.,0.)) ;
#43916 = DIRECTION('',(-1.,-2.86503102337282E-14,0.)) ;
#43917 = DIRECTION('center_axis',(0.202274762387575,-0.979328811227899,0.)) ;
#43918 = DIRECTION('ref_axis',(0.81902520534733,0.169164969825965,0.548252611475353)) ;
#43919 = DIRECTION('center_axis',(0.,2.3968590984082E-16,1.)) ;
#43920 = DIRECTION('ref_axis',(1.,0.,0.)) ;
#43921 = DIRECTION('center_axis',(0.,0.,-1.)) ;
#43922 = DIRECTION('ref_axis',(1.,2.63677968348475E-16,0.)) ;
#43923 = DIRECTION('center_axis',(0.186904608537136,-0.982127159191002,0.0222015874881292)) ;
#43924 = DIRECTION('ref_axis',(0.982190613046714,0.187262692968013,0.0153063210892889)) ;
#43925 = DIRECTION('center_axis',(-0.202274762386252,-0.979328811228172,-1.87854811391648E-12)) ;
#43926 = DIRECTION('ref_axis',(0.819025205347352,-0.169164969825868,0.54825261147535)) ;
#43927 = DIRECTION('center_axis',(-0.431213875666327,0.45627334817079,0.778376017861446)) ;
#43928 = DIRECTION('ref_axis',(-0.813949131457668,0.175495689147714,-0.553794252850169)) ;
#43929 = DIRECTION('center_axis',(-0.784162512362691,0.382514104089345,0.488643136018258)) ;
#43930 = DIRECTION('ref_axis',(-0.490111180257797,0.101229659940977,-0.865761853476199)) ;
#43931 = DIRECTION('center_axis',(-0.998769717110461,5.59418425230248E-11,
0.0495888312333449)) ;
#43932 = DIRECTION('ref_axis',(-0.0495862470879959,0.0102088265337349,-0.998717669794889)) ;
#43933 = DIRECTION('center_axis',(-1.,-5.55111512312579E-15,1.64313007644522E-12)) ;
#43934 = DIRECTION('ref_axis',(-1.64313007644523E-12,1.5709655798446E-12,
-1.)) ;
#43935 = DIRECTION('center_axis',(0.,1.,0.)) ;
#43936 = DIRECTION('ref_axis',(0.999909707872585,0.,-0.0134378607732635)) ;
#43937 = DIRECTION('',(0.999999978565477,-1.29200364901908E-8,0.000207048412283444)) ;
#43938 = DIRECTION('center_axis',(1.,1.11022302462514E-14,6.57724049867568E-14)) ;
#43939 = DIRECTION('ref_axis',(1.11022302462514E-14,-1.,1.17986696570242E-44)) ;
#43940 = DIRECTION('',(1.,0.,0.)) ;
#43941 = DIRECTION('center_axis',(1.,0.,-1.23419240007014E-14)) ;
#43942 = DIRECTION('ref_axis',(0.,-1.,0.)) ;
#43943 = DIRECTION('',(1.,0.,0.)) ;
#43944 = DIRECTION('center_axis',(0.,0.,-1.)) ;
#43945 = DIRECTION('ref_axis',(0.793390388649528,0.608713143605879,0.)) ;
#43946 = DIRECTION('',(0.,0.,1.)) ;
#43947 = DIRECTION('center_axis',(0.,0.,1.)) ;
#43948 = DIRECTION('ref_axis',(0.965894315163092,-0.258936617602883,0.)) ;
#43949 = DIRECTION('',(0.,0.,-1.)) ;
#43950 = DIRECTION('center_axis',(0.,-1.,0.)) ;
#43951 = DIRECTION('ref_axis',(0.,0.,-1.)) ;
#43952 = DIRECTION('',(1.,0.,0.)) ;
#43953 = DIRECTION('',(-0.0942752822069811,0.,-0.995546167269401)) ;
#43954 = DIRECTION('center_axis',(0.,-1.,0.)) ;
#43955 = DIRECTION('ref_axis',(0.371772155637639,0.,0.928324008249568)) ;
#43956 = DIRECTION('center_axis',(0.,-1.,0.)) ;
#43957 = DIRECTION('ref_axis',(0.525950052779709,0.,-0.850515456638515)) ;
#43958 = DIRECTION('center_axis',(-0.087142648404439,0.0173337504938603,-0.996045029063886)) ;
#43959 = DIRECTION('ref_axis',(-0.996194698091746,2.77416503886704E-15,0.0871557427476577)) ;
#43960 = DIRECTION('center_axis',(0.0140688745303331,0.999901028487045,-1.40716591575854E-15)) ;
#43961 = DIRECTION('ref_axis',(0.999901028487045,-0.0140688745303331,-6.81169755687964E-34)) ;
#43962 = DIRECTION('center_axis',(-0.369647612382762,-0.929172019950947,3.84741834623491E-16)) ;
#43963 = DIRECTION('ref_axis',(0.929172019950947,-0.369647612382762,4.43338045572624E-34)) ;
#43964 = DIRECTION('center_axis',(0.0871426484044392,-0.0173337504938598,
0.996045029063886)) ;
#43965 = DIRECTION('ref_axis',(-0.976906303124667,0.194318745462638,0.0888498738160223)) ;
#43966 = DIRECTION('',(0.0871426484044392,-0.0173337504938598,0.996045029063886)) ;
#43967 = DIRECTION('center_axis',(-0.0871426484044391,0.0173337504938307,
-0.996045029063886)) ;
#43968 = DIRECTION('ref_axis',(-0.996194698091746,2.77283728287811E-15,0.0871557427476578)) ;
#43969 = DIRECTION('',(-0.0871426484044392,0.0173337504938598,-0.996045029063886)) ;
#43970 = DIRECTION('center_axis',(0.,0.,1.)) ;
#43971 = DIRECTION('ref_axis',(-0.686061634431369,-0.727543423969566,0.)) ;
#43972 = DIRECTION('center_axis',(0.0198801512493583,0.973637907857952,0.227231168566933)) ;
#43973 = DIRECTION('ref_axis',(0.0848581350266343,-0.228099154715644,0.969932921669231)) ;
#43974 = DIRECTION('center_axis',(-0.390791367470215,-0.90489803427529,-0.168646537691927)) ;
#43975 = DIRECTION('ref_axis',(0.0145744118599508,-0.189275895687504,0.981815777949524)) ;
#43976 = DIRECTION('center_axis',(-0.996194698091746,3.51997520523845E-15,
0.0871557427476579)) ;
#43977 = DIRECTION('ref_axis',(0.0871557427476578,-2.56289665819841E-31,0.996194698091746)) ;
#43978 = DIRECTION('center_axis',(0.996194698091746,-3.51997520523845E-15,
-0.0871557427476579)) ;
#43979 = DIRECTION('ref_axis',(0.082689266929588,-0.316018771704214,0.945142645882201)) ;
#43980 = DIRECTION('center_axis',(-0.996194698091746,3.51997520523845E-15,
0.0871557427476579)) ;
#43981 = DIRECTION('ref_axis',(0.082689266929588,-0.316018771704214,0.945142645882201)) ;
#43982 = DIRECTION('center_axis',(-0.996194698091746,3.51997520523845E-15,
0.0871557427476579)) ;
#43983 = DIRECTION('ref_axis',(0.0871557427476579,3.7050998642496E-32,0.996194698091746)) ;
#43984 = DIRECTION('',(3.53342093867907E-15,1.,0.)) ;
#43985 = DIRECTION('center_axis',(-0.996194698091748,-6.11235790402882E-14,
0.0871557427476263)) ;
#43986 = DIRECTION('ref_axis',(0.0827617664630686,-0.31351037143038,0.945971319341923)) ;
#43987 = DIRECTION('center_axis',(3.53342093867907E-15,1.,0.)) ;
#43988 = DIRECTION('ref_axis',(0.675590207615657,-2.3871445855557E-15,-0.737277336810127)) ;
#43989 = DIRECTION('',(-3.53342093867907E-15,-1.,0.)) ;
#43990 = DIRECTION('center_axis',(3.53342093867907E-15,1.,0.)) ;
#43991 = DIRECTION('ref_axis',(0.675590207615657,-2.3871445855557E-15,-0.737277336810127)) ;
#43992 = DIRECTION('center_axis',(-0.0796183978310997,0.406796813220287,-0.910042451471704)) ;
#43993 = DIRECTION('ref_axis',(0.996194698091747,-1.11289992857909E-14,-0.0871557427476466)) ;
#43994 = DIRECTION('center_axis',(-0.0844345745997023,0.247929423057006,-0.965091603836023)) ;
#43995 = DIRECTION('ref_axis',(0.996194698091746,-5.54415204842811E-15,-0.0871557427476577)) ;
#43996 = DIRECTION('center_axis',(0.969995299381892,-0.171397325086558,-0.17242991657542)) ;
#43997 = DIRECTION('ref_axis',(-0.130771520122756,0.230075936076955,-0.96434634502501)) ;
#43998 = DIRECTION('center_axis',(-0.0844006560103685,0.249445165551562,-0.964703912424933)) ;
#43999 = DIRECTION('ref_axis',(0.996194698090483,-8.3278891326026E-15,-0.0871557427620906)) ;
#44000 = DIRECTION('center_axis',(-0.307221196694479,-0.877837780004883,0.367445190875743)) ;
#44001 = DIRECTION('ref_axis',(0.563077209994445,-0.478958069141859,-0.673456177927542)) ;
#44002 = DIRECTION('center_axis',(-0.991017446008435,-0.133732650115511,0.)) ;
#44003 = DIRECTION('ref_axis',(-0.133732650115511,0.991017446008435,0.)) ;
#44004 = DIRECTION('center_axis',(0.307221196683632,-0.877837780010281,0.367445190871915)) ;
#44005 = DIRECTION('ref_axis',(-0.563077209989657,-0.478958069131965,-0.673456177938582)) ;
#44006 = DIRECTION('center_axis',(-0.0844006559966543,-0.249445165539995,
0.964703912429124)) ;
#44007 = DIRECTION('ref_axis',(-0.996194698091746,2.76022795169697E-15,-0.0871557427476577)) ;
#44008 = DIRECTION('center_axis',(0.991017446008434,-0.13373265011552,0.)) ;
#44009 = DIRECTION('ref_axis',(0.13373265011552,0.991017446008434,0.)) ;
#44010 = DIRECTION('center_axis',(6.61271392193231E-15,1.,0.)) ;
#44011 = DIRECTION('ref_axis',(-0.675590207615657,4.46748477142119E-15,-0.737277336810127)) ;
#44012 = DIRECTION('center_axis',(-0.0844345745997158,-0.247929423057003,
0.965091603836023)) ;
#44013 = DIRECTION('ref_axis',(-0.996194698091745,5.56571981562619E-15,-0.0871557427476687)) ;
#44014 = DIRECTION('center_axis',(-0.0796183978311047,-0.406796813220276,
0.910042451471708)) ;
#44015 = DIRECTION('ref_axis',(-0.996194698091747,1.23978847396904E-17,-0.0871557427476467)) ;
#44016 = DIRECTION('center_axis',(-0.969995299381675,-0.171397325087362,-0.172429916575841)) ;
#44017 = DIRECTION('ref_axis',(0.130771521154601,0.23007593125536,-0.964346346035433)) ;
#44018 = DIRECTION('center_axis',(0.99619469809175,-1.09010204657839E-13,
0.0871557427476121)) ;
#44019 = DIRECTION('ref_axis',(0.0827617664618814,0.31351037147169,-0.945971319328336)) ;
#44020 = DIRECTION('center_axis',(0.996194698091746,-6.58755054902644E-15,
0.0871557427476584)) ;
#44021 = DIRECTION('ref_axis',(0.0871557427476584,-3.66128094028344E-32,-0.996194698091746)) ;
#44022 = DIRECTION('center_axis',(-0.996194698091746,6.58755054902644E-15,
-0.0871557427476584)) ;
#44023 = DIRECTION('ref_axis',(-0.0826892669295917,-0.316018771704213,0.945142645882201)) ;
#44024 = DIRECTION('center_axis',(-0.0198801512493482,0.973637907857952,0.22723116856693)) ;
#44025 = DIRECTION('ref_axis',(-0.0848581350266373,-0.22809915471564,0.969932921669232)) ;
#44026 = DIRECTION('center_axis',(0.996194698091746,-6.58755054902644E-15,
0.0871557427476584)) ;
#44027 = DIRECTION('ref_axis',(-0.0826892669295917,-0.316018771704213,0.945142645882201)) ;
#44028 = DIRECTION('center_axis',(0.996194698091746,-6.58755054902644E-15,
0.0871557427476584)) ;
#44029 = DIRECTION('ref_axis',(0.0871557427476584,-3.34096417774836E-32,-0.996194698091746)) ;
#44030 = DIRECTION('',(-6.61271392193231E-15,-1.,0.)) ;
#44031 = DIRECTION('',(0.0871426484044398,0.0173337504938583,-0.996045029063886)) ;
#44032 = DIRECTION('center_axis',(-6.61271392193231E-15,-1.,0.)) ;
#44033 = DIRECTION('ref_axis',(-0.675590207615657,4.46748477142119E-15,-0.737277336810127)) ;
#44034 = DIRECTION('',(6.61271392193231E-15,1.,0.)) ;
#44035 = DIRECTION('center_axis',(0.369647612382746,-0.929172019950953,2.5649455641565E-16)) ;
#44036 = DIRECTION('ref_axis',(-0.929172019950953,-0.369647612382746,4.94162803730509E-33)) ;
#44037 = DIRECTION('center_axis',(0.0871426484044391,0.0173337504938598,-0.996045029063886)) ;
#44038 = DIRECTION('ref_axis',(0.92036389196323,0.381227206369641,0.0871557427476579)) ;
#44039 = DIRECTION('center_axis',(-0.0140688745303202,0.999901028487045,1.39740367298719E-15)) ;
#44040 = DIRECTION('ref_axis',(-0.999901028487045,-0.0140688745303202,2.97151128565353E-34)) ;
#44041 = DIRECTION('center_axis',(-0.0871426484044398,-0.0173337504938583,
0.996045029063886)) ;
#44042 = DIRECTION('ref_axis',(0.976906303124669,0.194318745462627,0.0888498738160226)) ;
#44043 = DIRECTION('',(-0.0871426484044398,-0.0173337504938583,0.996045029063886)) ;
#44044 = DIRECTION('center_axis',(0.0871426484044392,0.0173337504938592,-0.996045029063886)) ;
#44045 = DIRECTION('ref_axis',(0.920363891963231,0.381227206369638,0.0871557427476578)) ;
#44046 = DIRECTION('center_axis',(0.,0.,1.)) ;
#44047 = DIRECTION('ref_axis',(1.,0.,0.)) ;
#44048 = DIRECTION('center_axis',(0.390791367470204,-0.904898034275296,-0.168646537691924)) ;
#44049 = DIRECTION('ref_axis',(-0.0145744118599547,-0.189275895687501,0.981815777949525)) ;
#44050 = DIRECTION('center_axis',(0.92036389196323,0.381227206369639,0.087155742747658)) ;
#44051 = DIRECTION('ref_axis',(-0.382683432365075,0.923879532511293,-6.02752148941637E-17)) ;
#44052 = DIRECTION('',(0.382683432365075,-0.923879532511293,0.)) ;
#44053 = DIRECTION('',(0.0666626913468331,0.066662691346831,-0.995546167269401)) ;
#44054 = DIRECTION('center_axis',(0.92036389196323,0.381227206369639,0.087155742747658)) ;
#44055 = DIRECTION('ref_axis',(0.391063046541469,-0.897215317273461,-0.205120374608636)) ;
#44056 = DIRECTION('',(0.0942752822069809,-5.29059027656374E-18,-0.995546167269401)) ;
#44057 = DIRECTION('center_axis',(-0.92036389196323,-0.381227206369639,-0.087155742747658)) ;
#44058 = DIRECTION('ref_axis',(-0.0315995086952045,-0.149641293808218,0.988235272714764)) ;
#44059 = DIRECTION('center_axis',(0.382683432365075,-0.923879532511293,0.)) ;
#44060 = DIRECTION('ref_axis',(-0.62416396518116,-0.258537179522593,-0.737277336810128)) ;
#44061 = DIRECTION('',(-0.382683432365075,0.923879532511293,0.)) ;
#44062 = DIRECTION('center_axis',(0.884086155524837,-0.467323945041674,-3.24271127339954E-16)) ;
#44063 = DIRECTION('ref_axis',(-0.467323945041674,-0.884086155524837,3.63079830694576E-33)) ;
#44064 = DIRECTION('center_axis',(-0.307221196683633,-0.877837780010277,-0.367445190871924)) ;
#44065 = DIRECTION('ref_axis',(-0.56307720998965,0.478958069131973,-0.673456177938582)) ;
#44066 = DIRECTION('center_axis',(-0.0844006559966506,0.249445165540006,0.964703912429121)) ;
#44067 = DIRECTION('ref_axis',(-0.129175820564643,0.957249345402581,-0.258819045102521)) ;
#44068 = DIRECTION('center_axis',(-1.04325044166935E-14,-1.,0.)) ;
#44069 = DIRECTION('ref_axis',(-0.675590207615657,7.04809782482522E-15,-0.737277336810127)) ;
#44070 = DIRECTION('center_axis',(0.991017446008437,0.133732650115502,0.)) ;
#44071 = DIRECTION('ref_axis',(0.133732650115502,-0.991017446008437,0.)) ;
#44072 = DIRECTION('center_axis',(-0.0844345745996896,0.247929423057007,0.965091603836024)) ;
#44073 = DIRECTION('ref_axis',(-0.162387929710607,0.952177957199453,-0.25881904510252)) ;
#44074 = DIRECTION('center_axis',(-0.969995299381661,0.171397325087379,-0.172429916575904)) ;
#44075 = DIRECTION('ref_axis',(-0.130771520584849,0.230075933918614,0.96434634547729)) ;
#44076 = DIRECTION('center_axis',(-0.079618397831098,0.406796813220277,0.910042451471708)) ;
#44077 = DIRECTION('ref_axis',(-0.15336115832627,0.89707261674463,-0.414416548177999)) ;
#44078 = DIRECTION('center_axis',(0.99619469809175,1.08620882498388E-13,0.0871557427476121)) ;
#44079 = DIRECTION('ref_axis',(0.0827617664602934,-0.31351037152687,-0.945971319310187)) ;
#44080 = DIRECTION('center_axis',(0.,0.,1.)) ;
#44081 = DIRECTION('ref_axis',(1.,0.,0.)) ;
#44082 = DIRECTION('center_axis',(0.,0.,-1.)) ;
#44083 = DIRECTION('ref_axis',(6.99440505513848E-15,1.,0.)) ;
#44084 = DIRECTION('center_axis',(0.969995299381302,0.171397325089019,-0.172429916576296)) ;
#44085 = DIRECTION('ref_axis',(0.130771520826673,0.230075932788573,0.964346345714104)) ;
#44086 = DIRECTION('center_axis',(0.,0.,1.)) ;
#44087 = DIRECTION('ref_axis',(7.04419501764363E-15,1.,0.)) ;
#44088 = DIRECTION('center_axis',(0.,0.,1.)) ;
#44089 = DIRECTION('ref_axis',(1.,0.,0.)) ;
#44090 = DIRECTION('center_axis',(0.,0.,1.)) ;
#44091 = DIRECTION('ref_axis',(7.21644966006352E-15,1.,0.)) ;
#44092 = DIRECTION('center_axis',(0.,0.,1.)) ;
#44093 = DIRECTION('ref_axis',(1.,0.,0.)) ;
#44094 = DIRECTION('center_axis',(0.,0.,-1.)) ;
#44095 = DIRECTION('ref_axis',(7.16665969755837E-15,1.,0.)) ;
#44096 = DIRECTION('center_axis',(-0.991017446008435,0.133732650115516,0.)) ;
#44097 = DIRECTION('ref_axis',(-0.133732650115516,-0.991017446008435,0.)) ;
#44098 = DIRECTION('center_axis',(-1.04325044166935E-14,-1.,0.)) ;
#44099 = DIRECTION('ref_axis',(-0.675590207615657,7.04809782482522E-15,-0.737277336810127)) ;
#44100 = DIRECTION('',(-1.04325044166935E-14,-1.,0.)) ;
#44101 = DIRECTION('center_axis',(0.369647612382771,0.929172019950944,0.)) ;
#44102 = DIRECTION('ref_axis',(-0.929172019950944,0.369647612382771,0.)) ;
#44103 = DIRECTION('',(1.04325044166935E-14,1.,0.)) ;
#44104 = DIRECTION('center_axis',(0.307221196683631,-0.877837780010281,-0.367445190871915)) ;
#44105 = DIRECTION('ref_axis',(0.563077209989657,0.478958069131965,-0.673456177938583)) ;
#44106 = DIRECTION('center_axis',(0.0844006559966532,0.249445165540006,0.964703912429121)) ;
#44107 = DIRECTION('ref_axis',(0.996194698091746,-8.28110794162546E-18,-0.0871557427476575)) ;
#44108 = DIRECTION('center_axis',(2.86369556082085E-16,-1.,0.)) ;
#44109 = DIRECTION('ref_axis',(0.675590207615657,1.93468467848299E-16,-0.737277336810127)) ;
#44110 = DIRECTION('center_axis',(0.0844345745997038,0.247929423057005,0.965091603836023)) ;
#44111 = DIRECTION('ref_axis',(0.996194698091746,-3.65481143962558E-17,-0.0871557427476578)) ;
#44112 = DIRECTION('center_axis',(0.0796183978311159,0.406796813220274,0.910042451471708)) ;
#44113 = DIRECTION('ref_axis',(0.996194698091746,-2.8097871293113E-15,-0.0871557427476576)) ;
#44114 = DIRECTION('center_axis',(-0.996194698091746,-2.45272960483312E-14,
0.0871557427476522)) ;
#44115 = DIRECTION('ref_axis',(0.0827617664579715,0.313510371607444,0.945971319283687)) ;
#44116 = DIRECTION('center_axis',(-0.996194698091746,-2.8527983346386E-16,
0.0871557427476584)) ;
#44117 = DIRECTION('ref_axis',(0.0871557427476583,1.94505549952558E-32,0.996194698091746)) ;
#44118 = DIRECTION('center_axis',(0.996194698091746,2.8527983346386E-16,-0.0871557427476584)) ;
#44119 = DIRECTION('ref_axis',(0.0826892669295895,0.316018771704214,0.945142645882201)) ;
#44120 = DIRECTION('center_axis',(0.0198801512493551,-0.973637907857952,0.227231168566931)) ;
#44121 = DIRECTION('ref_axis',(0.0848581350266359,0.228099154715642,0.969932921669231)) ;
#44122 = DIRECTION('center_axis',(-0.996194698091746,-2.8527983346386E-16,
0.0871557427476584)) ;
#44123 = DIRECTION('ref_axis',(0.0826892669295895,0.316018771704214,0.945142645882201)) ;
#44124 = DIRECTION('center_axis',(-0.996194698091746,-2.8527983346386E-16,
0.0871557427476584)) ;
#44125 = DIRECTION('ref_axis',(0.0871557427476584,-7.26620746443239E-33,0.996194698091746)) ;
#44126 = DIRECTION('',(-2.86369556082085E-16,1.,0.)) ;
#44127 = DIRECTION('',(-0.0871426484044397,-0.0173337504938598,-0.996045029063886)) ;
#44128 = DIRECTION('center_axis',(-2.86369556082085E-16,1.,0.)) ;
#44129 = DIRECTION('ref_axis',(0.675590207615657,1.93468467848299E-16,-0.737277336810127)) ;
#44130 = DIRECTION('',(2.86369556082085E-16,-1.,0.)) ;
#44131 = DIRECTION('center_axis',(-0.369647612382753,0.929172019950951,2.56494556415654E-16)) ;
#44132 = DIRECTION('ref_axis',(0.929172019950951,0.369647612382753,4.719839717894E-33)) ;
#44133 = DIRECTION('center_axis',(-0.087142648404439,-0.0173337504938604,
-0.996045029063886)) ;
#44134 = DIRECTION('ref_axis',(-0.920363891963227,-0.381227206369647,0.0871557427476579)) ;
#44135 = DIRECTION('center_axis',(0.0140688745303267,-0.999901028487045,-1.39252255160153E-15)) ;
#44136 = DIRECTION('ref_axis',(0.999901028487045,0.0140688745303267,-5.60930068162866E-33)) ;
#44137 = DIRECTION('center_axis',(0.0871426484044397,0.0173337504938598,0.996045029063886)) ;
#44138 = DIRECTION('ref_axis',(-0.976906303124668,-0.194318745462633,0.0888498738160228)) ;
#44139 = DIRECTION('',(0.0871426484044397,0.0173337504938598,0.996045029063886)) ;
#44140 = DIRECTION('center_axis',(-0.0871426484044391,-0.0173337504938592,
-0.996045029063886)) ;
#44141 = DIRECTION('ref_axis',(-0.920363891963228,-0.381227206369644,0.0871557427476575)) ;
#44142 = DIRECTION('center_axis',(0.,0.,1.)) ;
#44143 = DIRECTION('ref_axis',(-0.686061634431343,0.72754342396959,0.)) ;
#44144 = DIRECTION('center_axis',(-0.39079136747021,0.904898034275293,-0.168646537691926)) ;
#44145 = DIRECTION('ref_axis',(0.0145744118599526,0.189275895687503,0.981815777949524)) ;
#44146 = DIRECTION('center_axis',(-0.920363891963228,-0.381227206369645,0.0871557427476583)) ;
#44147 = DIRECTION('ref_axis',(0.382683432365081,-0.92387953251129,8.03599596472331E-17)) ;
#44148 = DIRECTION('',(-0.382683432365082,0.92387953251129,0.)) ;
#44149 = DIRECTION('',(-0.0666626913468326,-0.0666626913468325,-0.995546167269401)) ;
#44150 = DIRECTION('center_axis',(-0.920363891963228,-0.381227206369645,0.0871557427476583)) ;
#44151 = DIRECTION('ref_axis',(-0.391063046541475,0.897215317273459,-0.205120374608633)) ;
#44152 = DIRECTION('',(-0.0942752822069815,-5.29059027656383E-18,-0.995546167269401)) ;
#44153 = DIRECTION('center_axis',(0.920363891963228,0.381227206369645,-0.0871557427476583)) ;
#44154 = DIRECTION('ref_axis',(0.0315995086952039,0.149641293808218,0.988235272714764)) ;
#44155 = DIRECTION('center_axis',(-0.382683432365082,0.92387953251129,0.)) ;
#44156 = DIRECTION('ref_axis',(0.624163965181158,0.258537179522598,-0.737277336810128)) ;
#44157 = DIRECTION('',(0.382683432365082,-0.92387953251129,0.)) ;
#44158 = DIRECTION('center_axis',(-0.884086155524841,0.467323945041666,-6.13458003510009E-16)) ;
#44159 = DIRECTION('ref_axis',(0.467323945041666,0.884086155524841,-3.60419358345438E-32)) ;
#44160 = DIRECTION('center_axis',(0.087142648404439,-0.0173337504938606,-0.996045029063886)) ;
#44161 = DIRECTION('ref_axis',(0.996194698091746,-9.7139919131807E-15,0.0871557427476578)) ;
#44162 = DIRECTION('center_axis',(-0.0140688745303435,-0.999901028487045,
-1.38764143021586E-15)) ;
#44163 = DIRECTION('ref_axis',(-0.999901028487044,0.0140688745303435,-4.34518124734398E-32)) ;
#44164 = DIRECTION('center_axis',(-0.087142648404439,0.0173337504938613,0.996045029063886)) ;
#44165 = DIRECTION('ref_axis',(0.976906303124666,-0.194318745462644,0.0888498738160224)) ;
#44166 = DIRECTION('',(-0.087142648404439,0.0173337504938612,0.996045029063886)) ;
#44167 = DIRECTION('center_axis',(0.087142648404439,-0.0173337504937438,-0.996045029063888)) ;
#44168 = DIRECTION('ref_axis',(0.996194698091746,-8.32583325170817E-15,0.0871557427476576)) ;
#44169 = DIRECTION('',(0.087142648404439,-0.0173337504938613,-0.996045029063886)) ;
#44170 = DIRECTION('center_axis',(0.,0.,1.)) ;
#44171 = DIRECTION('ref_axis',(1.,0.,0.)) ;
#44172 = DIRECTION('center_axis',(-0.0198801512493651,-0.973637907857951,
0.227231168566934)) ;
#44173 = DIRECTION('ref_axis',(-0.084858135026633,0.228099154715646,0.969932921669231)) ;
#44174 = DIRECTION('center_axis',(0.390791367470222,0.904898034275287,-0.168646537691928)) ;
#44175 = DIRECTION('ref_axis',(-0.0145744118599494,0.189275895687505,0.981815777949524)) ;
#44176 = DIRECTION('center_axis',(0.996194698091746,-1.03928055877287E-14,
0.0871557427476579)) ;
#44177 = DIRECTION('ref_axis',(0.0871557427476579,2.06998122833165E-31,-0.996194698091746)) ;
#44178 = DIRECTION('center_axis',(-0.996194698091746,1.03928055877287E-14,
-0.0871557427476579)) ;
#44179 = DIRECTION('ref_axis',(-0.0826892669295858,0.316018771704216,0.9451426458822)) ;
#44180 = DIRECTION('center_axis',(-0.382683432365094,-0.923879532511285,0.)) ;
#44181 = DIRECTION('ref_axis',(-0.624163965181155,0.258537179522606,-0.737277336810127)) ;
#44182 = DIRECTION('',(-0.382683432365094,-0.923879532511285,0.)) ;
#44183 = DIRECTION('center_axis',(0.884086155524847,0.467323945041655,-3.24271127339941E-16)) ;
#44184 = DIRECTION('ref_axis',(-0.467323945041655,0.884086155524847,-7.36160927852353E-33)) ;
#44185 = DIRECTION('',(0.382683432365094,0.923879532511285,0.)) ;
#44186 = DIRECTION('center_axis',(-2.25344562200783E-7,0.00122104690338566,
0.999999254521927)) ;
#44187 = DIRECTION('ref_axis',(0.880239547026216,0.474529244989194,-0.000579224539763828)) ;
#44188 = DIRECTION('center_axis',(3.49420756930928E-5,-0.000974753633340996,
0.99999952431709)) ;
#44189 = DIRECTION('ref_axis',(-0.117733043599258,0.993044805378454,0.00097208833143988)) ;
#44190 = DIRECTION('center_axis',(0.,0.,1.)) ;
#44191 = DIRECTION('ref_axis',(1.,0.,0.)) ;
#44192 = DIRECTION('center_axis',(0.,0.,-1.)) ;
#44193 = DIRECTION('ref_axis',(0.38268343236509,0.923879532511287,0.)) ;
#44194 = DIRECTION('center_axis',(2.83928856810258E-5,3.29420197351069E-5,
0.999999999054334)) ;
#44195 = DIRECTION('ref_axis',(0.96762709105351,0.252384253428295,-3.57877724692542E-5)) ;
#44196 = DIRECTION('center_axis',(-5.19405847738775E-5,2.97673798315385E-5,
0.999999998208039)) ;
#44197 = DIRECTION('ref_axis',(0.690866054023378,-0.722982774416375,5.74052898069753E-5)) ;
#44198 = DIRECTION('center_axis',(0.,0.,-1.)) ;
#44199 = DIRECTION('ref_axis',(-1.,0.,0.)) ;
#44200 = DIRECTION('center_axis',(0.218991760123564,0.252536654884624,-0.942479626802441)) ;
#44201 = DIRECTION('ref_axis',(-1.36744941626268E-14,-0.965925826289036,-0.258819045102642)) ;
#44202 = DIRECTION('center_axis',(0.939992844931799,-0.341133990269129,0.00640719596122297)) ;
#44203 = DIRECTION('ref_axis',(0.337451616258958,0.932291946017575,0.130223400642821)) ;
#44204 = DIRECTION('center_axis',(0.942424992012689,-0.333801508271347,0.0202900839243436)) ;
#44205 = DIRECTION('ref_axis',(0.334410493611304,0.940273089931856,-0.0636878176156427)) ;
#44206 = DIRECTION('center_axis',(0.943545137525121,-0.327692396729339,0.0483763018272643)) ;
#44207 = DIRECTION('ref_axis',(0.331217944158533,0.935186145148194,-0.12538559482754)) ;
#44208 = DIRECTION('',(-0.328003666919281,-0.944669970289995,0.00349881691496844)) ;
#44209 = DIRECTION('',(0.846577478048041,0.532254029430749,-0.00349597147443212)) ;
#44210 = DIRECTION('center_axis',(-0.53049404449562,0.844439101982528,-0.0741530295916526)) ;
#44211 = DIRECTION('ref_axis',(0.847670234963863,0.527872145314473,-0.0529733041956474)) ;
#44212 = DIRECTION('center_axis',(-0.523158578258209,0.851633793864804,-0.0320153579128746)) ;
#44213 = DIRECTION('ref_axis',(0.851857027606319,0.521437987961937,-0.0494168921314753)) ;
#44214 = DIRECTION('center_axis',(-0.512178225761606,0.858833907404777,-0.00881955483771457)) ;
#44215 = DIRECTION('ref_axis',(0.849520309205079,0.508082285339014,0.142012800735676)) ;
#44216 = DIRECTION('center_axis',(0.249199500799499,0.0844061683157321,-0.964766918769263)) ;
#44217 = DIRECTION('ref_axis',(-1.08248674634472E-13,-0.996194698093663,-0.0871557427257419)) ;
#44218 = DIRECTION('center_axis',(0.95602568240079,0.13742503062509,0.259093140680714)) ;
#44219 = DIRECTION('ref_axis',(0.256281665748432,0.038083835396144,-0.965851608313994)) ;
#44220 = DIRECTION('center_axis',(-0.852367862727417,-0.245048083800581,-0.461974526586865)) ;
#44221 = DIRECTION('ref_axis',(0.501019754926551,-0.129565454350722,-0.855682182946583)) ;
#44222 = DIRECTION('',(0.249320710565386,0.0844034492993762,-0.964735840025413)) ;
#44223 = DIRECTION('center_axis',(0.249445165540006,0.084400655996652,-0.964703912429121)) ;
#44224 = DIRECTION('ref_axis',(-5.51682469897799E-15,-0.996194698091746,-0.0871557427476577)) ;
#44225 = DIRECTION('',(-0.248916559555376,-0.0870782764297481,0.964602467420201)) ;
#44226 = DIRECTION('center_axis',(0.3263419315863,-0.82640429306137,0.458864781932826)) ;
#44227 = DIRECTION('ref_axis',(-0.478958069131965,-0.563077209989657,-0.673456177938582)) ;
#44228 = DIRECTION('center_axis',(1.,-6.98296267768627E-15,0.)) ;
#44229 = DIRECTION('ref_axis',(-4.71762120519045E-15,-0.675590207615657,-0.737277336810127)) ;
#44230 = DIRECTION('center_axis',(-0.133732650115508,0.991017446008436,0.)) ;
#44231 = DIRECTION('ref_axis',(0.991017446008436,0.133732650115508,0.)) ;
#44232 = DIRECTION('center_axis',(6.9563903964836E-15,0.996194698091746,0.0871557427476574)) ;
#44233 = DIRECTION('ref_axis',(-6.40601855134593E-32,-0.0871557427476574,
0.996194698091746)) ;
#44234 = DIRECTION('',(-1.,6.98296267768627E-15,0.)) ;
#44235 = DIRECTION('',(-0.0173337504938605,-0.0871426484044386,0.996045029063886)) ;
#44236 = DIRECTION('',(1.,-6.98296267768627E-15,0.)) ;
#44237 = DIRECTION('center_axis',(1.,-6.98296267768627E-15,0.)) ;
#44238 = DIRECTION('ref_axis',(4.7176212051905E-15,0.675590207615663,0.737277336810121)) ;
#44239 = DIRECTION('',(1.,-6.98296267768627E-15,0.)) ;
#44240 = DIRECTION('center_axis',(1.,-1.67169584432416E-14,0.)) ;
#44241 = DIRECTION('ref_axis',(0.,0.,1.)) ;
#44242 = DIRECTION('center_axis',(0.,0.,1.)) ;
#44243 = DIRECTION('ref_axis',(-1.,9.64749793678664E-15,0.)) ;
#44244 = DIRECTION('center_axis',(0.,0.,-1.)) ;
#44245 = DIRECTION('ref_axis',(-1.,8.00610789814445E-15,0.)) ;
#44246 = DIRECTION('center_axis',(0.,0.,1.)) ;
#44247 = DIRECTION('ref_axis',(-1.,8.1410746989025E-15,0.)) ;
#44248 = DIRECTION('center_axis',(-0.326341931586305,-0.826404293061363,-0.458864781932835)) ;
#44249 = DIRECTION('ref_axis',(-0.478958069131954,0.563077209989667,-0.673456177938582)) ;
#44250 = DIRECTION('center_axis',(-0.249445165539996,0.084400655996657,0.964703912429124)) ;
#44251 = DIRECTION('ref_axis',(1.12665838577891E-14,0.996194698091745,-0.0871557427476582)) ;
#44252 = DIRECTION('center_axis',(-0.133732650115524,-0.991017446008434,0.)) ;
#44253 = DIRECTION('ref_axis',(0.991017446008434,-0.133732650115524,0.)) ;
#44254 = DIRECTION('center_axis',(1.,-1.01461348606114E-14,0.)) ;
#44255 = DIRECTION('ref_axis',(6.85462935697691E-15,0.675590207615657,-0.737277336810127)) ;
#44256 = DIRECTION('center_axis',(-0.249199500798557,0.0844061683219424,0.964766918768963)) ;
#44257 = DIRECTION('ref_axis',(5.52024668591357E-15,0.996194698093106,-0.0871557427321035)) ;
#44258 = DIRECTION('',(0.248916559555379,-0.0870782764297426,-0.9646024674202)) ;
#44259 = DIRECTION('',(-0.249320710565346,0.0844034492993872,0.964735840025422)) ;
#44260 = DIRECTION('center_axis',(-0.852367862729301,0.245048083794489,-0.461974526586621)) ;
#44261 = DIRECTION('ref_axis',(0.5010197546446,0.129565452553711,-0.855682183383771)) ;
#44262 = DIRECTION('center_axis',(-0.218991760123583,0.252536654884511,0.942479626802467)) ;
#44263 = DIRECTION('ref_axis',(1.66369913122973E-14,0.965925826289068,-0.258819045102521)) ;
#44264 = DIRECTION('center_axis',(0.956025682401039,-0.137425030623654,0.259093140680558)) ;
#44265 = DIRECTION('ref_axis',(0.256281665662312,-0.0380838359928184,-0.965851608313318)) ;
#44266 = DIRECTION('center_axis',(-1.,1.01461348606114E-14,0.)) ;
#44267 = DIRECTION('ref_axis',(-6.85462935697698E-15,-0.675590207615664,0.737277336810121)) ;
#44268 = DIRECTION('',(1.,-1.01461348606114E-14,0.)) ;
#44269 = DIRECTION('center_axis',(1.,-9.20200038935782E-15,2.22044604925031E-14)) ;
#44270 = DIRECTION('ref_axis',(-1.11022302462516E-14,-0.996194698091746,0.0871557427476575)) ;
#44271 = DIRECTION('',(-1.,1.01461348606114E-14,0.)) ;
#44272 = DIRECTION('center_axis',(-1.01075257542649E-14,-0.996194698091746,
0.0871557427476588)) ;
#44273 = DIRECTION('ref_axis',(9.3268358271731E-31,-0.0871557427476588,-0.996194698091745)) ;
#44274 = DIRECTION('',(-1.,1.01461348606114E-14,0.)) ;
#44275 = DIRECTION('',(0.0173337504938584,-0.0871426484044403,-0.996045029063886)) ;
#44276 = DIRECTION('center_axis',(-1.,1.01461348606114E-14,0.)) ;
#44277 = DIRECTION('ref_axis',(6.85462935697691E-15,0.675590207615657,-0.737277336810127)) ;
#44278 = DIRECTION('',(1.,-1.01461348606114E-14,0.)) ;
#44279 = DIRECTION('center_axis',(-0.929172019950953,-0.369647612382748,5.12989112831302E-16)) ;
#44280 = DIRECTION('ref_axis',(-0.369647612382748,0.929172019950953,3.80280772654386E-32)) ;
#44281 = DIRECTION('center_axis',(0.,0.,-1.)) ;
#44282 = DIRECTION('ref_axis',(-1.,0.,0.)) ;
#44283 = DIRECTION('',(-0.923879532511294,-0.382683432365072,0.)) ;
#44284 = DIRECTION('',(1.,0.,0.)) ;
#44285 = DIRECTION('',(-1.,0.,0.)) ;
#44286 = DIRECTION('',(0.923879532511287,-0.38268343236509,0.)) ;
#44287 = DIRECTION('center_axis',(0.0666626913468315,-0.0666626913468327,
-0.995546167269401)) ;
#44288 = DIRECTION('ref_axis',(0.920363891963223,-0.381227206369657,0.0871557427476578)) ;
#44289 = DIRECTION('center_axis',(-0.467323945041676,-0.884086155524836,6.13458003510006E-16)) ;
#44290 = DIRECTION('ref_axis',(-0.884086155524836,0.467323945041676,9.23656027967999E-33)) ;
#44291 = DIRECTION('center_axis',(-0.0666626913468313,0.0666626913468338,
0.995546167269401)) ;
#44292 = DIRECTION('ref_axis',(0.703957445860461,-0.703957445860479,0.0942752822069821)) ;
#44293 = DIRECTION('center_axis',(0.0666626913468288,-0.0666626913468385,
-0.995546167269401)) ;
#44294 = DIRECTION('ref_axis',(0.920363891963223,-0.381227206369658,0.0871557427476576)) ;
#44295 = DIRECTION('',(0.0666626913468313,-0.0666626913468338,-0.995546167269401)) ;
#44296 = DIRECTION('',(-0.0666626913468313,0.0666626913468338,0.995546167269401)) ;
#44297 = DIRECTION('center_axis',(0.382648721133683,0.923893810008795,0.000429001387020652)) ;
#44298 = DIRECTION('ref_axis',(3.3887587197891E-9,-0.000464341932836984,0.999999892193279)) ;
#44299 = DIRECTION('center_axis',(0.920363891963223,-0.381227206369657,0.0871557427476581)) ;
#44300 = DIRECTION('ref_axis',(0.391063046541487,0.897215317273456,-0.205120374608625)) ;
#44301 = DIRECTION('center_axis',(0.0942752822069813,0.,-0.995546167269401)) ;
#44302 = DIRECTION('ref_axis',(0.920363891963223,-0.381227206369657,0.0871557427476577)) ;
#44303 = DIRECTION('center_axis',(-0.762014168288054,0.631273206450739,-0.144320983040126)) ;
#44304 = DIRECTION('ref_axis',(0.647560350336759,0.742848333944369,-0.169829165421638)) ;
#44305 = DIRECTION('center_axis',(-0.0942752822069817,0.,0.995546167269401)) ;
#44306 = DIRECTION('ref_axis',(0.55374779771692,-0.831031649929668,0.0524382812345561)) ;
#44307 = DIRECTION('center_axis',(0.0942752822069761,-1.10527827697982E-14,
-0.995546167269401)) ;
#44308 = DIRECTION('ref_axis',(0.920363891963223,-0.381227206369657,0.0871557427476571)) ;
#44309 = DIRECTION('',(-0.0942752822069817,0.,0.995546167269401)) ;
#44310 = DIRECTION('center_axis',(1.,0.,0.)) ;
#44311 = DIRECTION('ref_axis',(0.,-1.,0.)) ;
#44312 = DIRECTION('center_axis',(-0.388740138376909,-0.916141414187395,0.0978060019907851)) ;
#44313 = DIRECTION('ref_axis',(-0.0425606765102603,0.123898048145669,0.991381794507385)) ;
#44314 = DIRECTION('center_axis',(0.990117129665866,0.,0.140242894801221)) ;
#44315 = DIRECTION('ref_axis',(-0.140242894801221,0.,0.990117129665866)) ;
#44316 = DIRECTION('center_axis',(1.,0.,0.)) ;
#44317 = DIRECTION('ref_axis',(0.,-1.,0.)) ;
#44318 = DIRECTION('center_axis',(0.923873568388754,0.382697789457833,0.000177698394351369)) ;
#44319 = DIRECTION('ref_axis',(7.78311851840014E-16,-0.000464330811650805,
0.999999892198443)) ;
#44320 = DIRECTION('center_axis',(-0.923879532511294,-0.382683432365072,0.)) ;
#44321 = DIRECTION('ref_axis',(-0.258537179522591,0.624163965181161,-0.737277336810127)) ;
#44322 = DIRECTION('',(-0.923879532511294,-0.382683432365072,0.)) ;
#44323 = DIRECTION('center_axis',(0.999901028487045,0.0140688745303215,-1.41204703714418E-15)) ;
#44324 = DIRECTION('ref_axis',(-0.0140688745303215,0.999901028487045,-6.14044914489112E-33)) ;
#44325 = DIRECTION('',(0.923879532511294,0.382683432365072,0.)) ;
#44326 = DIRECTION('center_axis',(0.381227206369636,-0.920363891963232,0.0871557427476586)) ;
#44327 = DIRECTION('ref_axis',(0.923879532511294,0.382683432365072,2.41666793745239E-17)) ;
#44328 = DIRECTION('',(0.923879532511294,0.382683432365072,0.)) ;
#44329 = DIRECTION('',(-0.0173337504938584,0.0871426484044403,0.996045029063886)) ;
#44330 = DIRECTION('center_axis',(1.,0.,0.)) ;
#44331 = DIRECTION('ref_axis',(0.,0.707106781186548,-0.707106781186548)) ;
#44332 = DIRECTION('center_axis',(-0.98591981532733,-0.142582648849442,0.0873630699552131)) ;
#44333 = DIRECTION('ref_axis',(0.16721877210685,-0.840665536837555,0.515091581593703)) ;
#44334 = DIRECTION('center_axis',(-0.017333750493859,0.0871426484044392,0.996045029063886)) ;
#44335 = DIRECTION('ref_axis',(0.381227206369635,-0.920363891963232,0.0871557427476577)) ;
#44336 = DIRECTION('center_axis',(-0.92387953251129,-0.382683432365083,6.19072153925554E-15)) ;
#44337 = DIRECTION('ref_axis',(5.55111512312578E-15,2.77555756156289E-15,
1.)) ;
#44338 = DIRECTION('center_axis',(-0.923879532511294,-0.382683432365072,0.)) ;
#44339 = DIRECTION('ref_axis',(0.258537179522595,-0.62416396518117,0.737277336810118)) ;
#44340 = DIRECTION('center_axis',(-0.0173337504938584,0.0871426484044403,
0.996045029063886)) ;
#44341 = DIRECTION('ref_axis',(0.194318745462623,-0.97690630312467,0.0888498738160231)) ;
#44342 = DIRECTION('center_axis',(-0.0173337504938614,0.0871426484044502,
0.996045029063885)) ;
#44343 = DIRECTION('ref_axis',(-9.71372357808658E-15,-0.996194698091745,0.0871557427476687)) ;
#44344 = DIRECTION('center_axis',(0.0942752822069805,1.3083323619903E-16,
-0.995546167269401)) ;
#44345 = DIRECTION('ref_axis',(-1.38777878078144E-15,1.,4.3924990864866E-31)) ;
#44346 = DIRECTION('center_axis',(0.382648720419747,-0.923893810300393,0.000429010201431217)) ;
#44347 = DIRECTION('ref_axis',(0.920363891963229,0.381227206369639,0.0871557427476688)) ;
#44348 = DIRECTION('center_axis',(-0.762014168288071,-0.631273206450718,-0.144320983040128)) ;
#44349 = DIRECTION('ref_axis',(0.647560350336739,-0.742848333944383,-0.169829165421651)) ;
#44350 = DIRECTION('center_axis',(-0.0942752822069809,0.,0.995546167269401)) ;
#44351 = DIRECTION('ref_axis',(0.553747797716925,0.831031649929665,0.0524382812345561)) ;
#44352 = DIRECTION('center_axis',(0.0942752822069809,0.,-0.995546167269401)) ;
#44353 = DIRECTION('ref_axis',(0.,1.,0.)) ;
#44354 = DIRECTION('',(-0.0942752822069809,0.,0.995546167269401)) ;
#44355 = DIRECTION('center_axis',(1.,0.,0.)) ;
#44356 = DIRECTION('ref_axis',(0.,0.653011882880021,0.757347661789148)) ;
#44357 = DIRECTION('center_axis',(0.990117129665866,0.,0.140242894801223)) ;
#44358 = DIRECTION('ref_axis',(-0.140242894801223,7.9794965316409E-17,0.990117129665866)) ;
#44359 = DIRECTION('center_axis',(-0.388740138376891,0.916141414187403,0.0978060019907881)) ;
#44360 = DIRECTION('ref_axis',(-0.042560676510261,-0.12389804814567,0.991381794507385)) ;
#44361 = DIRECTION('center_axis',(-0.0666626913468331,-0.066662691346831,
0.995546167269401)) ;
#44362 = DIRECTION('ref_axis',(0.703957445860476,0.703957445860465,0.0942752822069814)) ;
#44363 = DIRECTION('center_axis',(0.0666626913468211,0.0666626913468305,-0.995546167269402)) ;
#44364 = DIRECTION('ref_axis',(0.381227219735143,0.920363886377725,0.0871557432686075)) ;
#44365 = DIRECTION('center_axis',(-0.0666626913468326,-0.0666626913468315,
0.995546167269401)) ;
#44366 = DIRECTION('ref_axis',(0.92036389196323,0.381227206369639,0.0871557427476577)) ;
#44367 = DIRECTION('',(-0.0666626913468331,-0.066662691346831,0.995546167269401)) ;
#44368 = DIRECTION('center_axis',(-0.467323945041656,0.884086155524847,6.13458003510013E-16)) ;
#44369 = DIRECTION('ref_axis',(-0.884086155524847,-0.467323945041656,-8.62742891290345E-32)) ;
#44370 = DIRECTION('center_axis',(1.,0.,0.)) ;
#44371 = DIRECTION('ref_axis',(0.,-1.,0.)) ;
#44372 = DIRECTION('center_axis',(0.923873568388748,-0.382697789457847,0.000177698394306731)) ;
#44373 = DIRECTION('ref_axis',(0.381227206369654,0.920363891963224,0.0871557427476576)) ;
#44374 = DIRECTION('center_axis',(0.92036389196323,0.381227206369639,0.087155742747658)) ;
#44375 = DIRECTION('ref_axis',(0.0942752822069809,1.55365773163449E-17,-0.995546167269401)) ;
#44376 = DIRECTION('center_axis',(0.92036389196323,0.381227206369639,0.087155742747658)) ;
#44377 = DIRECTION('ref_axis',(-0.0315995086952045,-0.149641293808218,0.988235272714764)) ;
#44378 = DIRECTION('center_axis',(0.,1.,0.)) ;
#44379 = DIRECTION('ref_axis',(0.,0.,1.)) ;
#44380 = DIRECTION('center_axis',(0.,-1.,0.)) ;
#44381 = DIRECTION('ref_axis',(-0.37177215563764,0.,0.928324008249567)) ;
#44382 = DIRECTION('center_axis',(-0.807964101600016,1.34553052300038E-14,
-0.589231712084201)) ;
#44383 = DIRECTION('ref_axis',(-0.581351145863386,-0.163002279992783,0.797158141099043)) ;
#44384 = DIRECTION('center_axis',(0.,1.,0.)) ;
#44385 = DIRECTION('ref_axis',(-0.37177215563764,0.,0.928324008249567)) ;
#44386 = DIRECTION('center_axis',(0.,-1.,0.)) ;
#44387 = DIRECTION('ref_axis',(0.,0.,-1.)) ;
#44388 = DIRECTION('',(0.,0.,-1.)) ;
#44389 = DIRECTION('center_axis',(0.,-1.,0.)) ;
#44390 = DIRECTION('ref_axis',(-0.525952960008619,0.,-0.850513658831046)) ;
#44391 = DIRECTION('',(1.,0.,0.)) ;
#44392 = DIRECTION('center_axis',(1.,0.,0.)) ;
#44393 = DIRECTION('ref_axis',(0.,-0.707106781186548,-0.707106781186548)) ;
#44394 = DIRECTION('center_axis',(0.381227206369654,0.920363891963224,0.0871557427476574)) ;
#44395 = DIRECTION('ref_axis',(-0.923879532511287,0.38268343236509,8.02781664235613E-17)) ;
#44396 = DIRECTION('',(0.923879532511287,-0.38268343236509,4.83811561633781E-18)) ;
#44397 = DIRECTION('',(0.0173337504938605,0.0871426484044386,-0.996045029063886)) ;
#44398 = DIRECTION('',(-0.923879532511287,0.38268343236509,-4.83811561633781E-18)) ;
#44399 = DIRECTION('center_axis',(-0.985919815327329,0.142582648849448,0.0873630699552218)) ;
#44400 = DIRECTION('ref_axis',(0.167218772106861,0.840665536837553,0.515091581593703)) ;
#44401 = DIRECTION('center_axis',(-0.0173337504938585,-0.0871426484044279,
0.996045029063887)) ;
#44402 = DIRECTION('ref_axis',(6.93831543720529E-15,0.996194698091747,0.0871557427476467)) ;
#44403 = DIRECTION('center_axis',(-0.923879532511282,0.382683432365101,1.13192831841253E-14)) ;
#44404 = DIRECTION('ref_axis',(0.381227206369666,0.920363891963219,0.0871557427476574)) ;
#44405 = DIRECTION('center_axis',(0.923879532511286,-0.382683432365091,0.)) ;
#44406 = DIRECTION('ref_axis',(0.258537179522607,0.624163965181163,0.73727733681012)) ;
#44407 = DIRECTION('center_axis',(-0.0173337504938605,-0.0871426484044386,
0.996045029063886)) ;
#44408 = DIRECTION('ref_axis',(0.194318745462641,0.976906303124666,0.0888498738160219)) ;
#44409 = DIRECTION('center_axis',(-0.0173337504938607,-0.0871426484044388,
0.996045029063886)) ;
#44410 = DIRECTION('ref_axis',(0.381227206369655,0.920363891963224,0.0871557427476577)) ;
#44411 = DIRECTION('center_axis',(0.999901028487045,-0.0140688745303409,2.76552061766038E-15)) ;
#44412 = DIRECTION('ref_axis',(-0.0140688745303409,-0.999901028487045,1.27304684468474E-32)) ;
#44413 = DIRECTION('center_axis',(-0.929172019950944,0.369647612382769,1.28247278207833E-16)) ;
#44414 = DIRECTION('ref_axis',(-0.369647612382769,-0.929172019950944,-9.94337188479288E-33)) ;
#44415 = DIRECTION('center_axis',(1.,-6.98296267768627E-15,0.)) ;
#44416 = DIRECTION('ref_axis',(-4.71762120519044E-15,-0.675590207615656,-0.737277336810128)) ;
#44417 = DIRECTION('',(-1.,6.98296267768627E-15,0.)) ;
#44418 = DIRECTION('center_axis',(0.923879532511286,-0.382683432365091,0.)) ;
#44419 = DIRECTION('ref_axis',(-0.258537179522604,-0.624163965181156,-0.737277336810127)) ;
#44420 = DIRECTION('',(-0.923879532511287,0.38268343236509,0.)) ;
#44421 = DIRECTION('center_axis',(1.,0.,0.)) ;
#44422 = DIRECTION('ref_axis',(0.,0.707106781186548,-0.707106781186548)) ;
#44423 = DIRECTION('',(1.,0.,0.)) ;
#44424 = DIRECTION('',(-1.,0.,0.)) ;
#44425 = DIRECTION('center_axis',(0.762014168288065,0.631273206450725,-0.144320983040127)) ;
#44426 = DIRECTION('ref_axis',(-0.647560350336745,0.742848333944378,-0.169829165421649)) ;
#44427 = DIRECTION('center_axis',(-0.218991760123586,-0.252536654884508,-0.942479626802467)) ;
#44428 = DIRECTION('ref_axis',(-2.81914239016188E-15,0.965925826289068,-0.258819045102521)) ;
#44429 = DIRECTION('center_axis',(-0.939992844966884,0.341133990171559,0.00640719600867651)) ;
#44430 = DIRECTION('ref_axis',(0.337451616159548,0.93229194606199,-0.130223400582445)) ;
#44431 = DIRECTION('center_axis',(-0.942424992002713,0.333801508312564,0.0202900837096207)) ;
#44432 = DIRECTION('ref_axis',(0.334410493637827,0.940273089914465,0.0636878177331398)) ;
#44433 = DIRECTION('center_axis',(-0.943545137507695,0.327692396888825,0.0483763010868215)) ;
#44434 = DIRECTION('ref_axis',(0.331217944217424,0.935186145117652,0.12538559489977)) ;
#44435 = DIRECTION('',(0.328003666872713,0.944669970306165,0.00349881691470218)) ;
#44436 = DIRECTION('',(-0.846577478023147,-0.532254029470342,-0.00349597147476316)) ;
#44437 = DIRECTION('center_axis',(0.530494044393499,-0.844439102113116,-0.0741530288351211)) ;
#44438 = DIRECTION('ref_axis',(0.847670235028008,0.527872145264436,0.0529733036678171)) ;
#44439 = DIRECTION('center_axis',(0.523158578227078,-0.851633793891756,-0.0320153577046641)) ;
#44440 = DIRECTION('ref_axis',(0.851857027623571,0.521437987939093,0.049416892075135)) ;
#44441 = DIRECTION('center_axis',(0.51217822584914,-0.858833907352119,-0.00881955488214049)) ;
#44442 = DIRECTION('ref_axis',(0.849520309139197,0.508082285425671,-0.142012800819747)) ;
#44443 = DIRECTION('center_axis',(-0.249199500799459,-0.0844061683159849,
-0.964766918769251)) ;
#44444 = DIRECTION('ref_axis',(2.76101386392502E-15,0.996194698093643,-0.087155742725975)) ;
#44445 = DIRECTION('center_axis',(-0.956025682401338,-0.137425030622013,0.259093140680327)) ;
#44446 = DIRECTION('ref_axis',(0.25628166568836,0.0380838358104107,0.965851608313599)) ;
#44447 = DIRECTION('center_axis',(0.852367862728953,0.245048083795463,-0.461974526586746)) ;
#44448 = DIRECTION('ref_axis',(0.501019755025973,-0.129565454997057,0.855682182790503)) ;
#44449 = DIRECTION('',(-0.249320710565382,-0.0844034492993914,-0.964735840025412)) ;
#44450 = DIRECTION('center_axis',(-0.249445165543295,-0.0844006560005468,
-0.96470391242793)) ;
#44451 = DIRECTION('ref_axis',(-4.51830490057156E-18,0.996194698091387,-0.0871557427517545)) ;
#44452 = DIRECTION('',(0.248916559555392,0.0870782764297379,0.964602467420198)) ;
#44453 = DIRECTION('center_axis',(0.326341931589371,-0.826404293060443,-0.458864781932311)) ;
#44454 = DIRECTION('ref_axis',(0.478958069134772,0.563077209991019,-0.673456177935448)) ;
#44455 = DIRECTION('center_axis',(-1.,0.,0.)) ;
#44456 = DIRECTION('ref_axis',(0.,0.675590207615657,-0.737277336810127)) ;
#44457 = DIRECTION('center_axis',(0.133732650115514,-0.991017446008435,0.)) ;
#44458 = DIRECTION('ref_axis',(-0.991017446008435,-0.133732650115514,0.)) ;
#44459 = DIRECTION('center_axis',(0.,-0.996194698091746,0.0871557427476584)) ;
#44460 = DIRECTION('ref_axis',(0.,-0.0871557427476584,-0.996194698091746)) ;
#44461 = DIRECTION('',(1.,0.,0.)) ;
#44462 = DIRECTION('',(0.0173337504938599,0.0871426484044397,0.996045029063886)) ;
#44463 = DIRECTION('',(-1.,0.,0.)) ;
#44464 = DIRECTION('center_axis',(-1.,0.,0.)) ;
#44465 = DIRECTION('ref_axis',(0.,-0.675590207615663,0.737277336810121)) ;
#44466 = DIRECTION('',(-1.,0.,0.)) ;
#44467 = DIRECTION('center_axis',(-1.,0.,0.)) ;
#44468 = DIRECTION('ref_axis',(0.,0.,1.)) ;
#44469 = DIRECTION('center_axis',(0.,0.,1.)) ;
#44470 = DIRECTION('ref_axis',(1.,0.,0.)) ;
#44471 = DIRECTION('center_axis',(0.,0.,-1.)) ;
#44472 = DIRECTION('ref_axis',(1.,-1.67349113601944E-15,0.)) ;
#44473 = DIRECTION('center_axis',(0.,0.,1.)) ;
#44474 = DIRECTION('ref_axis',(1.,-1.69309011255336E-15,0.)) ;
#44475 = DIRECTION('center_axis',(-0.326341931586302,-0.826404293061369,0.458864781932826)) ;
#44476 = DIRECTION('ref_axis',(0.478958069131963,-0.563077209989659,-0.673456177938582)) ;
#44477 = DIRECTION('center_axis',(0.249445165540005,-0.084400655996654,0.964703912429121)) ;
#44478 = DIRECTION('ref_axis',(-5.38268147788269E-15,-0.996194698091746,-0.087155742747657)) ;
#44479 = DIRECTION('center_axis',(0.133732650115517,0.991017446008435,0.)) ;
#44480 = DIRECTION('ref_axis',(-0.991017446008435,0.133732650115517,0.)) ;
#44481 = DIRECTION('center_axis',(-1.,3.16317218292511E-15,0.)) ;
#44482 = DIRECTION('ref_axis',(-2.13700815178645E-15,-0.675590207615657,-0.737277336810127)) ;
#44483 = DIRECTION('center_axis',(0.249199500798546,-0.0844061683219426,0.964766918768965)) ;
#44484 = DIRECTION('ref_axis',(-5.55075920992131E-15,-0.996194698093106,-0.0871557427321035)) ;
#44485 = DIRECTION('',(-0.248916559555379,0.0870782764297428,-0.9646024674202)) ;
#44486 = DIRECTION('',(0.249320710565346,-0.0844034492993872,0.964735840025422)) ;
#44487 = DIRECTION('center_axis',(0.852367862729215,-0.245048083794411,-0.461974526586821)) ;
#44488 = DIRECTION('ref_axis',(0.501019754798628,0.129565453540298,0.855682183144197)) ;
#44489 = DIRECTION('center_axis',(0.218991760123595,-0.252536654884593,0.942479626802442)) ;
#44490 = DIRECTION('ref_axis',(-1.77417912264492E-16,-0.965925826289044,-0.258819045102609)) ;
#44491 = DIRECTION('center_axis',(-0.956025682401085,0.137425030623292,0.259093140680579)) ;
#44492 = DIRECTION('ref_axis',(0.256281665788873,-0.0380838351145112,0.965851608314368)) ;
#44493 = DIRECTION('center_axis',(1.,-3.16317218292511E-15,0.)) ;
#44494 = DIRECTION('ref_axis',(2.13700815178647E-15,0.675590207615663,0.737277336810121)) ;
#44495 = DIRECTION('',(-1.,3.16317218292511E-15,0.)) ;
#44496 = DIRECTION('center_axis',(-1.,6.05797912428137E-15,-5.55111512312578E-15)) ;
#44497 = DIRECTION('ref_axis',(5.55111512312579E-15,0.996194698091746,0.0871557427476578)) ;
#44498 = DIRECTION('',(1.,-3.16317218292511E-15,0.)) ;
#44499 = DIRECTION('center_axis',(3.15113535778129E-15,0.996194698091746,
0.0871557427476579)) ;
#44500 = DIRECTION('ref_axis',(-1.82466814306167E-33,-0.0871557427476579,
0.996194698091746)) ;
#44501 = DIRECTION('',(1.,-3.16317218292511E-15,0.)) ;
#44502 = DIRECTION('',(-0.0173337504938591,0.0871426484044392,-0.996045029063886)) ;
#44503 = DIRECTION('center_axis',(1.,-3.16317218292511E-15,0.)) ;
#44504 = DIRECTION('ref_axis',(-2.13700815178645E-15,-0.675590207615657,-0.737277336810127)) ;
#44505 = DIRECTION('',(-1.,3.16317218292511E-15,0.)) ;
#44506 = DIRECTION('center_axis',(0.929172019950952,0.369647612382751,2.56494556415653E-16)) ;
#44507 = DIRECTION('ref_axis',(0.369647612382751,-0.929172019950952,9.32329065219925E-33)) ;
#44508 = DIRECTION('center_axis',(0.,0.,-1.)) ;
#44509 = DIRECTION('ref_axis',(-1.,0.,0.)) ;
#44510 = DIRECTION('',(-0.923879532511289,0.382683432365084,0.)) ;
#44511 = DIRECTION('',(0.923879532511292,0.382683432365078,0.)) ;
#44512 = DIRECTION('',(-1.,0.,0.)) ;
#44513 = DIRECTION('center_axis',(0.0666626913468318,-0.0666626913468324,
0.995546167269401)) ;
#44514 = DIRECTION('ref_axis',(-0.703957445860467,0.703957445860474,0.0942752822069815)) ;
#44515 = DIRECTION('center_axis',(-0.0666626913468308,0.0666626913468347,
-0.995546167269401)) ;
#44516 = DIRECTION('ref_axis',(-0.920363891963225,0.381227206369651,0.0871557427476577)) ;
#44517 = DIRECTION('',(-0.0666626913468318,0.0666626913468324,-0.995546167269401)) ;
#44518 = DIRECTION('center_axis',(0.0666626913468317,-0.0666626913468324,
0.995546167269401)) ;
#44519 = DIRECTION('ref_axis',(-0.381227206369643,0.920363891963229,0.0871557427476577)) ;
#44520 = DIRECTION('',(0.0666626913468317,-0.0666626913468324,0.995546167269401)) ;
#44521 = DIRECTION('center_axis',(0.467323945041671,0.884086155524839,-6.48542254679904E-16)) ;
#44522 = DIRECTION('ref_axis',(0.884086155524839,-0.467323945041671,5.72532255921785E-31)) ;
#44523 = DIRECTION('center_axis',(-0.884086155524845,-0.467323945041659,-6.13458003510012E-16)) ;
#44524 = DIRECTION('ref_axis',(0.467323945041659,-0.884086155524845,8.11346111104324E-33)) ;
#44525 = DIRECTION('center_axis',(-0.382648721138496,-0.923893810006829,0.000429001327519702)) ;
#44526 = DIRECTION('ref_axis',(-3.36632111294574E-9,0.000464341859142652,
0.999999892193313)) ;
#44527 = DIRECTION('center_axis',(-0.920363891963225,0.381227206369651,0.0871557427476577)) ;
#44528 = DIRECTION('ref_axis',(-0.391063046541481,-0.897215317273458,-0.205120374608628)) ;
#44529 = DIRECTION('center_axis',(-0.0942752822069765,1.10527827697982E-14,
-0.995546167269401)) ;
#44530 = DIRECTION('ref_axis',(-0.920363891963225,0.381227206369651,0.0871557427476577)) ;
#44531 = DIRECTION('center_axis',(0.762014168288059,-0.631273206450732,-0.144320983040126)) ;
#44532 = DIRECTION('ref_axis',(-0.647560350336752,-0.742848333944374,-0.16982916542164)) ;
#44533 = DIRECTION('center_axis',(-0.0942752822069811,0.,-0.995546167269401)) ;
#44534 = DIRECTION('ref_axis',(-0.55374779771692,0.831031649929668,0.0524382812345557)) ;
#44535 = DIRECTION('center_axis',(-0.0942752822069763,1.11836160059972E-14,
-0.995546167269401)) ;
#44536 = DIRECTION('ref_axis',(-0.920363891963225,0.381227206369652,0.0871557427476575)) ;
#44537 = DIRECTION('',(0.0942752822069811,0.,0.995546167269401)) ;
#44538 = DIRECTION('center_axis',(1.,0.,0.)) ;
#44539 = DIRECTION('ref_axis',(0.,0.653011882880003,0.757347661789164)) ;
#44540 = DIRECTION('center_axis',(0.388740138376903,0.916141414187398,0.0978060019907864)) ;
#44541 = DIRECTION('ref_axis',(0.04256067651026,-0.123898048145669,0.991381794507385)) ;
#44542 = DIRECTION('center_axis',(-0.990117129665866,0.,0.140242894801221)) ;
#44543 = DIRECTION('ref_axis',(0.140242894801221,0.,0.990117129665866)) ;
#44544 = DIRECTION('center_axis',(1.,0.,0.)) ;
#44545 = DIRECTION('ref_axis',(0.,-1.,0.)) ;
#44546 = DIRECTION('center_axis',(-0.923873568388752,-0.382697789457837,0.000177698394329629)) ;
#44547 = DIRECTION('ref_axis',(-4.6023382439147E-16,0.000464330811593225,
0.999999892198443)) ;
#44548 = DIRECTION('center_axis',(0.382683432365087,0.923879532511288,0.)) ;
#44549 = DIRECTION('ref_axis',(0.624163965181156,-0.258537179522601,-0.737277336810128)) ;
#44550 = DIRECTION('',(0.382683432365087,0.923879532511288,0.)) ;
#44551 = DIRECTION('',(-0.382683432365087,-0.923879532511288,0.)) ;
#44552 = DIRECTION('center_axis',(0.923879532511292,0.382683432365078,0.)) ;
#44553 = DIRECTION('ref_axis',(0.258537179522595,-0.624163965181159,-0.737277336810128)) ;
#44554 = DIRECTION('',(0.923879532511292,0.382683432365078,0.)) ;
#44555 = DIRECTION('center_axis',(-0.999901028487045,-0.0140688745303254,
1.3827603088302E-15)) ;
#44556 = DIRECTION('ref_axis',(0.0140688745303254,-0.999901028487045,3.77607068720447E-33)) ;
#44557 = DIRECTION('',(-0.923879532511292,-0.382683432365078,0.)) ;
#44558 = DIRECTION('center_axis',(-0.381227206369642,0.920363891963229,0.0871557427476577)) ;
#44559 = DIRECTION('ref_axis',(-0.923879532511292,-0.382683432365078,-6.24302505454772E-17)) ;
#44560 = DIRECTION('',(-0.923879532511292,-0.382683432365078,0.)) ;
#44561 = DIRECTION('',(0.0173337504938591,-0.0871426484044392,0.996045029063886)) ;
#44562 = DIRECTION('center_axis',(1.,0.,0.)) ;
#44563 = DIRECTION('ref_axis',(0.,-0.707106781186548,-0.707106781186548)) ;
#44564 = DIRECTION('center_axis',(-0.985919815327333,-0.142582648849427,-0.0873630699552041)) ;
#44565 = DIRECTION('ref_axis',(-0.167218772106832,0.840665536837554,0.515091581593712)) ;
#44566 = DIRECTION('center_axis',(0.0173337504938596,-0.0871426484044392,
0.996045029063886)) ;
#44567 = DIRECTION('ref_axis',(-0.381227206369643,0.920363891963229,0.0871557427476578)) ;
#44568 = DIRECTION('center_axis',(0.923879532511292,0.382683432365077,0.)) ;
#44569 = DIRECTION('ref_axis',(0.,0.,1.)) ;
#44570 = DIRECTION('center_axis',(0.923879532511292,0.382683432365078,0.)) ;
#44571 = DIRECTION('ref_axis',(-0.258537179522597,0.624163965181164,0.737277336810123)) ;
#44572 = DIRECTION('center_axis',(-0.0173337504938596,0.0871426484044391,
-0.996045029063886)) ;
#44573 = DIRECTION('ref_axis',(-0.381227206369642,0.920363891963229,0.0871557427476578)) ;
#44574 = DIRECTION('center_axis',(0.0173337504938591,-0.0871426484044393,
0.996045029063886)) ;
#44575 = DIRECTION('ref_axis',(-0.194318745462631,0.976906303124668,0.0888498738160223)) ;
#44576 = DIRECTION('center_axis',(-0.920363891963225,0.381227206369651,0.0871557427476577)) ;
#44577 = DIRECTION('ref_axis',(-0.382683432365087,-0.923879532511288,6.71680456512626E-17)) ;
#44578 = DIRECTION('center_axis',(0.920363891963225,-0.381227206369651,-0.0871557427476577)) ;
#44579 = DIRECTION('ref_axis',(0.0315995086952024,-0.149641293808218,0.988235272714764)) ;
#44580 = DIRECTION('center_axis',(-0.0942752822069733,1.09219495335991E-14,
-0.995546167269402)) ;
#44581 = DIRECTION('ref_axis',(1.38777878078145E-15,-1.,-1.11022302462515E-14)) ;
#44582 = DIRECTION('center_axis',(-0.382648720419749,0.923893810300391,0.000429010201481)) ;
#44583 = DIRECTION('ref_axis',(-0.920363891963227,-0.381227206369645,0.0871557427476687)) ;
#44584 = DIRECTION('center_axis',(-0.0942752822069815,0.,-0.995546167269401)) ;
#44585 = DIRECTION('ref_axis',(-0.553747797716923,-0.831031649929666,0.0524382812345562)) ;
#44586 = DIRECTION('center_axis',(-0.0942752822069688,-1.30833236199014E-16,
-0.995546167269402)) ;
#44587 = DIRECTION('ref_axis',(1.38777878078145E-15,-1.,-2.81120891065768E-31)) ;
#44588 = DIRECTION('',(0.0942752822069815,0.,0.995546167269401)) ;
#44589 = DIRECTION('center_axis',(1.,0.,0.)) ;
#44590 = DIRECTION('ref_axis',(0.,-1.,0.)) ;
#44591 = DIRECTION('center_axis',(-0.990117129665866,0.,0.140242894801223)) ;
#44592 = DIRECTION('ref_axis',(0.140242894801223,-7.9794965316409E-17,0.990117129665866)) ;
#44593 = DIRECTION('center_axis',(0.388740138376897,-0.9161414141874,0.0978060019907868)) ;
#44594 = DIRECTION('ref_axis',(0.0425606765102615,0.12389804814567,0.991381794507385)) ;
#44595 = DIRECTION('center_axis',(0.0666626913468326,0.0666626913468325,0.995546167269401)) ;
#44596 = DIRECTION('ref_axis',(-0.703957445860472,-0.703957445860469,0.0942752822069821)) ;
#44597 = DIRECTION('center_axis',(-0.0666626913468289,-0.0666626913468395,
-0.995546167269401)) ;
#44598 = DIRECTION('ref_axis',(-0.381227219735137,-0.920363886377726,0.0871557432686186)) ;
#44599 = DIRECTION('center_axis',(0.0666626913468406,0.0666626913468404,0.9955461672694)) ;
#44600 = DIRECTION('ref_axis',(-0.920363891963227,-0.381227206369644,0.0871557427476687)) ;
#44601 = DIRECTION('',(0.0666626913468326,0.0666626913468325,0.995546167269401)) ;
#44602 = DIRECTION('center_axis',(0.467323945041663,-0.884086155524843,-6.1345800351001E-16)) ;
#44603 = DIRECTION('ref_axis',(0.884086155524843,0.467323945041663,-1.13677469639285E-32)) ;
#44604 = DIRECTION('center_axis',(1.,0.,0.)) ;
#44605 = DIRECTION('ref_axis',(0.,-1.,0.)) ;
#44606 = DIRECTION('center_axis',(-0.92387356838875,0.382697789457843,0.000177698394328006)) ;
#44607 = DIRECTION('ref_axis',(-0.381227206369648,-0.920363891963226,0.0871557427476688)) ;
#44608 = DIRECTION('center_axis',(-0.920363891963228,-0.381227206369645,0.0871557427476583)) ;
#44609 = DIRECTION('ref_axis',(0.0942752822069815,-1.5536577316345E-17,0.995546167269401)) ;
#44610 = DIRECTION('center_axis',(-0.920363891963228,-0.381227206369645,0.0871557427476583)) ;
#44611 = DIRECTION('ref_axis',(0.0315995086952039,0.149641293808218,0.988235272714764)) ;
#44612 = DIRECTION('center_axis',(0.,1.,0.)) ;
#44613 = DIRECTION('ref_axis',(0.,0.,1.)) ;
#44614 = DIRECTION('center_axis',(0.,1.,0.)) ;
#44615 = DIRECTION('ref_axis',(0.37177215563764,0.,0.928324008249567)) ;
#44616 = DIRECTION('center_axis',(-0.807964101600017,0.,0.5892317120842)) ;
#44617 = DIRECTION('ref_axis',(0.,-1.,0.)) ;
#44618 = DIRECTION('center_axis',(0.,-1.,0.)) ;
#44619 = DIRECTION('ref_axis',(0.37177215563764,0.,0.928324008249567)) ;
#44620 = DIRECTION('center_axis',(0.,-1.,0.)) ;
#44621 = DIRECTION('ref_axis',(0.,0.,-1.)) ;
#44622 = DIRECTION('',(0.,0.,-1.)) ;
#44623 = DIRECTION('center_axis',(-0.381227206369648,-0.920363891963227,0.0871557427476583)) ;
#44624 = DIRECTION('ref_axis',(0.923879532511289,-0.382683432365084,3.0103033140203E-19)) ;
#44625 = DIRECTION('',(-0.923879532511289,0.382683432365084,0.)) ;
#44626 = DIRECTION('',(-0.0173337504938599,-0.0871426484044397,-0.996045029063886)) ;
#44627 = DIRECTION('',(0.923879532511289,-0.382683432365084,0.)) ;
#44628 = DIRECTION('center_axis',(-0.985919815327331,0.142582648849435,-0.087363069955213)) ;
#44629 = DIRECTION('ref_axis',(-0.167218772106845,-0.840665536837551,0.515091581593712)) ;
#44630 = DIRECTION('center_axis',(0.0173337504938597,0.087142648404439,0.996045029063886)) ;
#44631 = DIRECTION('ref_axis',(2.15180843051778E-18,-0.996194698091746,0.0871557427476576)) ;
#44632 = DIRECTION('center_axis',(0.923879532511289,-0.382683432365085,5.12856164486979E-15)) ;
#44633 = DIRECTION('ref_axis',(-0.381227206369649,-0.920363891963226,0.0871557427476576)) ;
#44634 = DIRECTION('center_axis',(-0.923879532511289,0.382683432365084,0.)) ;
#44635 = DIRECTION('ref_axis',(-0.258537179522602,-0.624163965181165,0.73727733681012)) ;
#44636 = DIRECTION('center_axis',(0.0173337504938599,0.0871426484044397,0.996045029063886)) ;
#44637 = DIRECTION('ref_axis',(-0.194318745462635,-0.976906303124667,0.0888498738160228)) ;
#44638 = DIRECTION('center_axis',(0.0173337504938597,0.087142648404439,0.996045029063886)) ;
#44639 = DIRECTION('ref_axis',(-0.381227206369648,-0.920363891963227,0.0871557427476576)) ;
#44640 = DIRECTION('center_axis',(-0.999901028487045,0.0140688745303331,1.40716591575854E-15)) ;
#44641 = DIRECTION('ref_axis',(0.0140688745303331,0.999901028487045,-1.44407851814174E-34)) ;
#44642 = DIRECTION('center_axis',(0.929172019950948,-0.36964761238276,0.)) ;
#44643 = DIRECTION('ref_axis',(0.36964761238276,0.929172019950948,0.)) ;
#44644 = DIRECTION('center_axis',(-1.,0.,0.)) ;
#44645 = DIRECTION('ref_axis',(0.,0.675590207615656,-0.737277336810128)) ;
#44646 = DIRECTION('',(1.,0.,0.)) ;
#44647 = DIRECTION('center_axis',(-0.923879532511289,0.382683432365084,0.)) ;
#44648 = DIRECTION('ref_axis',(0.258537179522599,0.624163965181158,-0.737277336810127)) ;
#44649 = DIRECTION('',(0.923879532511289,-0.382683432365084,0.)) ;
#44650 = DIRECTION('center_axis',(0.,0.,1.)) ;
#44651 = DIRECTION('ref_axis',(-1.,7.87114109738639E-15,0.)) ;
#44652 = DIRECTION('center_axis',(0.,0.,-1.)) ;
#44653 = DIRECTION('ref_axis',(-1.,8.19721404385209E-15,0.)) ;
#44654 = DIRECTION('center_axis',(6.03394327975752E-16,6.03394327975742E-16,
1.)) ;
#44655 = DIRECTION('ref_axis',(-1.,8.03417757061924E-15,6.03394327975747E-16)) ;
#44656 = DIRECTION('center_axis',(0.,0.,1.)) ;
#44657 = DIRECTION('ref_axis',(1.,0.,0.)) ;
#44658 = DIRECTION('center_axis',(0.,0.,-1.)) ;
#44659 = DIRECTION('ref_axis',(-4.78181680548827E-15,-1.,0.)) ;
#44660 = DIRECTION('center_axis',(-6.03394327975744E-16,6.0339432797575E-16,
1.)) ;
#44661 = DIRECTION('ref_axis',(-4.55012211203708E-15,-1.,6.03394327975747E-16)) ;
#44662 = DIRECTION('center_axis',(0.,0.,1.)) ;
#44663 = DIRECTION('ref_axis',(1.,0.,0.)) ;
#44664 = DIRECTION('center_axis',(0.,0.,-1.)) ;
#44665 = DIRECTION('ref_axis',(1.,-1.73472347597681E-15,0.)) ;
#44666 = DIRECTION('center_axis',(0.,0.,1.)) ;
#44667 = DIRECTION('ref_axis',(1.,-1.69430781773116E-15,0.)) ;
#44668 = DIRECTION('center_axis',(0.920363891963223,-0.381227206369657,0.0871557427476581)) ;
#44669 = DIRECTION('ref_axis',(0.382683432365093,0.923879532511285,-6.76580195217738E-17)) ;
#44670 = DIRECTION('center_axis',(-0.920363891963223,0.381227206369657,-0.0871557427476581)) ;
#44671 = DIRECTION('ref_axis',(-0.0315995086952019,0.149641293808218,0.988235272714764)) ;
#44672 = DIRECTION('center_axis',(0.,0.,1.)) ;
#44673 = DIRECTION('ref_axis',(1.,0.,0.)) ;
#44674 = DIRECTION('center_axis',(0.,0.,1.)) ;
#44675 = DIRECTION('ref_axis',(1.,0.,0.)) ;
#44676 = DIRECTION('center_axis',(0.,1.,0.)) ;
#44677 = DIRECTION('ref_axis',(0.,0.,1.)) ;
#44678 = DIRECTION('center_axis',(0.,1.,0.)) ;
#44679 = DIRECTION('ref_axis',(0.371772155637639,0.,0.928324008249568)) ;
#44680 = DIRECTION('center_axis',(-0.807964101600016,0.,0.589231712084202)) ;
#44681 = DIRECTION('ref_axis',(0.581351145863385,-0.163002279992778,0.797158141099045)) ;
#44682 = DIRECTION('center_axis',(-0.920363891963225,0.381227206369651,0.0871557427476577)) ;
#44683 = DIRECTION('ref_axis',(0.0942752822069811,-1.03577182108966E-17,0.995546167269401)) ;
#44684 = DIRECTION('center_axis',(-0.920363891963225,0.381227206369651,0.0871557427476577)) ;
#44685 = DIRECTION('ref_axis',(0.0315995086952024,-0.149641293808218,0.988235272714764)) ;
#44686 = DIRECTION('center_axis',(3.34743552557144E-30,9.58743639363279E-16,
1.)) ;
#44687 = DIRECTION('ref_axis',(1.,0.,0.)) ;
#44688 = DIRECTION('center_axis',(-5.38716036738172E-30,-1.00092047861322E-15,
-1.)) ;
#44689 = DIRECTION('ref_axis',(-5.27809922139864E-15,-1.,1.00092047861322E-15)) ;
#44690 = DIRECTION('center_axis',(3.34743552557144E-30,9.58743639363279E-16,
1.)) ;
#44691 = DIRECTION('ref_axis',(-5.34959260451127E-15,-1.,9.58743639363279E-16)) ;
#44692 = DIRECTION('center_axis',(0.,0.,1.)) ;
#44693 = DIRECTION('ref_axis',(-0.793390388649525,0.608713143605883,0.)) ;
#44694 = DIRECTION('',(0.,0.,1.)) ;
#44695 = DIRECTION('center_axis',(0.,0.,-1.)) ;
#44696 = DIRECTION('ref_axis',(-0.965894315163092,-0.258936617602884,0.)) ;
#44697 = DIRECTION('center_axis',(1.,-1.83697019872103E-16,0.)) ;
#44698 = DIRECTION('ref_axis',(-1.22464679914735E-16,-1.,4.94506671532915E-16)) ;
#44699 = DIRECTION('center_axis',(0.,4.79371819681639E-16,1.)) ;
#44700 = DIRECTION('ref_axis',(0.,-1.,4.79371819681639E-16)) ;
#44701 = DIRECTION('center_axis',(0.,4.79371819681639E-16,1.)) ;
#44702 = DIRECTION('ref_axis',(0.,-1.,5.18039323243001E-16)) ;
#44703 = DIRECTION('center_axis',(0.,4.79371819681639E-16,1.)) ;
#44704 = DIRECTION('ref_axis',(0.,-1.,4.79371819681639E-16)) ;
#44705 = DIRECTION('center_axis',(0.,0.,-1.)) ;
#44706 = DIRECTION('ref_axis',(-1.,0.,0.)) ;
#44707 = DIRECTION('center_axis',(-0.807964101600022,-4.48510174333462E-15,
-0.589231712084193)) ;
#44708 = DIRECTION('ref_axis',(5.55111512312579E-15,-1.,-3.90782375100986E-30)) ;
#44709 = DIRECTION('center_axis',(0.,1.,0.)) ;
#44710 = DIRECTION('ref_axis',(0.,0.,1.)) ;
#44711 = DIRECTION('center_axis',(0.,-1.,0.)) ;
#44712 = DIRECTION('ref_axis',(-0.371772155637639,0.,0.928324008249568)) ;
#44713 = DIRECTION('center_axis',(0.920363891963223,-0.381227206369657,0.0871557427476581)) ;
#44714 = DIRECTION('ref_axis',(0.0942752822069817,-4.14308728435866E-17,-0.995546167269401)) ;
#44715 = DIRECTION('center_axis',(0.920363891963223,-0.381227206369657,0.0871557427476581)) ;
#44716 = DIRECTION('ref_axis',(-0.0315995086952019,0.149641293808218,0.988235272714764)) ;
#44717 = DIRECTION('center_axis',(0.996194698091746,-1.03928055877287E-14,
0.0871557427476579)) ;
#44718 = DIRECTION('ref_axis',(0.0871557427476579,4.02740903431178E-31,-0.996194698091746)) ;
#44719 = DIRECTION('center_axis',(0.996194698091746,-1.03928055877287E-14,
0.0871557427476579)) ;
#44720 = DIRECTION('ref_axis',(-0.0826892669295858,0.316018771704216,0.9451426458822)) ;
#44721 = DIRECTION('center_axis',(0.,0.,1.)) ;
#44722 = DIRECTION('ref_axis',(5.55111512312579E-15,-1.,0.)) ;
#44723 = DIRECTION('center_axis',(0.,0.,-1.)) ;
#44724 = DIRECTION('ref_axis',(0.793390388649528,-0.608713143605879,0.)) ;
#44725 = DIRECTION('',(0.,0.,1.)) ;
#44726 = DIRECTION('center_axis',(1.,-1.83697019872103E-16,0.)) ;
#44727 = DIRECTION('ref_axis',(-1.22464679914735E-16,-1.,4.94506671532915E-16)) ;
#44728 = DIRECTION('center_axis',(0.,4.79371819681639E-16,1.)) ;
#44729 = DIRECTION('ref_axis',(0.,-1.,4.79371819681639E-16)) ;
#44730 = DIRECTION('center_axis',(0.,4.79371819681639E-16,1.)) ;
#44731 = DIRECTION('ref_axis',(-1.22464679914735E-16,1.,-5.18039323243001E-16)) ;
#44732 = DIRECTION('center_axis',(0.,4.79371819681639E-16,1.)) ;
#44733 = DIRECTION('ref_axis',(0.,-1.,4.79371819681639E-16)) ;
#44734 = DIRECTION('center_axis',(0.,0.,-1.)) ;
#44735 = DIRECTION('ref_axis',(-1.,0.,0.)) ;
#44736 = DIRECTION('center_axis',(0.,0.,1.)) ;
#44737 = DIRECTION('ref_axis',(1.,0.,0.)) ;
#44738 = DIRECTION('',(0.707106781186549,8.65956056235495E-17,-0.707106781186546)) ;
#44739 = DIRECTION('center_axis',(0.,0.,-1.)) ;
#44740 = DIRECTION('ref_axis',(1.,0.,0.)) ;
#44741 = DIRECTION('center_axis',(3.34743552557144E-30,9.58743639363279E-16,
1.)) ;
#44742 = DIRECTION('ref_axis',(7.70749845132874E-46,-1.,9.58743639363279E-16)) ;
#44743 = DIRECTION('center_axis',(4.79371819681639E-16,4.79371819681634E-16,
1.)) ;
#44744 = DIRECTION('ref_axis',(-1.,8.75931951708652E-15,4.79371819681635E-16)) ;
#44745 = DIRECTION('center_axis',(0.,0.,1.)) ;
#44746 = DIRECTION('ref_axis',(1.,0.,0.)) ;
#44747 = DIRECTION('',(2.16840434415311E-19,-6.45693610888265E-16,1.)) ;
#44748 = DIRECTION('',(1.,-1.75535634497497E-13,-2.16840434528653E-19)) ;
#44749 = DIRECTION('',(2.16840434415311E-19,-6.45693610888265E-16,1.)) ;
#44750 = DIRECTION('',(1.,-1.75535634497497E-13,-2.16840434528653E-19)) ;
#44751 = DIRECTION('',(2.16840434415311E-19,-6.45693610888265E-16,1.)) ;
#44752 = DIRECTION('',(1.,-1.75535634497497E-13,-2.16840434528653E-19)) ;
#44753 = DIRECTION('',(2.16840434415311E-19,-6.45693610888265E-16,1.)) ;
#44754 = DIRECTION('',(1.,-1.75535634497497E-13,-2.16840434528653E-19)) ;
#44755 = DIRECTION('',(2.16840434415311E-19,-6.45693610888265E-16,1.)) ;
#44756 = DIRECTION('',(1.,-1.75535634497497E-13,-2.16840434528653E-19)) ;
#44757 = DIRECTION('',(2.16840434415311E-19,-6.45693610888265E-16,1.)) ;
#44758 = DIRECTION('',(1.,-1.75535634497497E-13,-2.16840434528653E-19)) ;
#44759 = DIRECTION('',(2.16840434415311E-19,-6.45693610888265E-16,1.)) ;
#44760 = DIRECTION('',(1.,-1.75535634497497E-13,-2.16840434528653E-19)) ;
#44761 = DIRECTION('',(2.16840434415311E-19,-6.45693610888265E-16,1.)) ;
#44762 = DIRECTION('',(1.,-1.75535634497497E-13,-2.16840434528653E-19)) ;
#44763 = DIRECTION('',(2.16840434415311E-19,-6.45693610888265E-16,1.)) ;
#44764 = DIRECTION('',(1.,-1.75535634497497E-13,-2.16840434528653E-19)) ;
#44765 = DIRECTION('axis',(0.,0.,1.)) ;
#44766 = DIRECTION('refdir',(1.,0.,0.)) ;
#44767 = DIRECTION('axis',(0.,0.,1.)) ;
#44768 = DIRECTION('refdir',(1.,0.,0.)) ;
#44769 = DIRECTION('center_axis',(-3.59212155404594E-15,1.,1.73472347647041E-18)) ;
#44770 = DIRECTION('ref_axis',(-2.70294271660742E-14,-1.7347234765675E-18,
1.)) ;
#44771 = DIRECTION('',(-3.59212155404594E-15,1.,1.73472347647041E-18)) ;
#44772 = DIRECTION('center_axis',(2.90739654573709E-15,-1.,2.17161023787725E-15)) ;
#44773 = DIRECTION('ref_axis',(-2.70294271660742E-14,2.17161023787717E-15,
1.)) ;
#44774 = DIRECTION('center_axis',(-3.59212155404594E-15,1.,1.73472347647041E-18)) ;
#44775 = DIRECTION('ref_axis',(-2.70294271660742E-14,-1.7347234765675E-18,
1.)) ;
#44776 = DIRECTION('',(-3.59212155404594E-15,1.,1.73472347647041E-18)) ;
#44777 = DIRECTION('center_axis',(-3.59212155404594E-15,1.,1.73472347647041E-18)) ;
#44778 = DIRECTION('ref_axis',(-2.70294271660742E-14,-1.7347234765675E-18,
1.)) ;
#44779 = DIRECTION('',(-3.59212155404594E-15,1.,1.73472347647041E-18)) ;
#44780 = DIRECTION('center_axis',(-3.59212155404594E-15,1.,1.73472347647041E-18)) ;
#44781 = DIRECTION('ref_axis',(-2.70294271660742E-14,-1.7347234765675E-18,
1.)) ;
#44782 = DIRECTION('',(-3.59212155404594E-15,1.,1.73472347647041E-18)) ;
#44783 = DIRECTION('center_axis',(-2.9073965457371E-15,1.,-2.17161023787728E-15)) ;
#44784 = DIRECTION('ref_axis',(-2.70294271660742E-14,2.1716102378772E-15,
1.)) ;
#44785 = DIRECTION('center_axis',(-2.9073965457371E-15,1.,-2.17161023787728E-15)) ;
#44786 = DIRECTION('ref_axis',(-1.48422940604576E-13,-2.17161023787771E-15,
-1.)) ;
#44787 = DIRECTION('',(-2.9073965457371E-15,1.,-2.17161023787728E-15)) ;
#44788 = DIRECTION('center_axis',(-2.90739654573709E-15,1.,-2.17161023787725E-15)) ;
#44789 = DIRECTION('ref_axis',(-1.48422940604576E-13,-2.17161023787768E-15,
-1.)) ;
#44790 = DIRECTION('center_axis',(-2.9073965457371E-15,1.,-2.17161023787728E-15)) ;
#44791 = DIRECTION('ref_axis',(-1.48422940604576E-13,-2.17161023787771E-15,
-1.)) ;
#44792 = DIRECTION('',(-2.9073965457371E-15,1.,-2.17161023787728E-15)) ;
#44793 = DIRECTION('center_axis',(-2.9073965457371E-15,1.,-2.17161023787728E-15)) ;
#44794 = DIRECTION('ref_axis',(-1.48422940604576E-13,-2.17161023787771E-15,
-1.)) ;
#44795 = DIRECTION('',(-2.9073965457371E-15,1.,-2.17161023787728E-15)) ;
#44796 = DIRECTION('center_axis',(-2.9073965457371E-15,1.,-2.17161023787728E-15)) ;
#44797 = DIRECTION('ref_axis',(-1.48422940604576E-13,-2.17161023787771E-15,
-1.)) ;
#44798 = DIRECTION('',(-2.9073965457371E-15,1.,-2.17161023787728E-15)) ;
#44799 = DIRECTION('center_axis',(2.9073965457371E-15,-1.,2.17161023787728E-15)) ;
#44800 = DIRECTION('ref_axis',(-1.48422940604576E-13,-2.17161023787771E-15,
-1.)) ;
#44801 = DIRECTION('center_axis',(-2.9073965457371E-15,1.,-2.17161023787728E-15)) ;
#44802 = DIRECTION('ref_axis',(-1.48422940604576E-13,-2.17161023787771E-15,
-1.)) ;
#44803 = DIRECTION('center_axis',(-3.59212155404594E-15,1.,1.73472347647041E-18)) ;
#44804 = DIRECTION('ref_axis',(-2.70294271660742E-14,-1.7347234765675E-18,
1.)) ;
#44805 = DIRECTION('center_axis',(1.48422940604577E-13,2.17161023787771E-15,
1.)) ;
#44806 = DIRECTION('ref_axis',(-0.707106781186548,-0.707106781186548,1.06486428110442E-13)) ;
#44807 = DIRECTION('center_axis',(2.84217094304056E-13,0.,1.)) ;
#44808 = DIRECTION('ref_axis',(-1.,0.,2.84217094304056E-13)) ;
#44809 = DIRECTION('',(1.48422940604577E-13,2.17161023787771E-15,1.)) ;
#44810 = DIRECTION('center_axis',(-2.84217094304016E-13,0.,-1.)) ;
#44811 = DIRECTION('ref_axis',(0.,-1.,0.)) ;
#44812 = DIRECTION('',(-1.48422940604577E-13,-2.17161023787771E-15,-1.)) ;
#44813 = DIRECTION('center_axis',(-1.42108547152028E-13,0.,-1.)) ;
#44814 = DIRECTION('ref_axis',(-1.,0.,1.81318720449162E-13)) ;
#44815 = DIRECTION('center_axis',(5.59482469102649E-13,0.,-1.)) ;
#44816 = DIRECTION('ref_axis',(0.,1.,0.)) ;
#44817 = DIRECTION('center_axis',(1.,0.,-1.42108547152028E-13)) ;
#44818 = DIRECTION('ref_axis',(1.42108547152028E-13,0.,1.)) ;
#44819 = DIRECTION('center_axis',(1.48422940604576E-13,2.17161023787771E-15,
1.)) ;
#44820 = DIRECTION('ref_axis',(-0.707106781186481,0.707106781186614,1.03415307459836E-13)) ;
#44821 = DIRECTION('center_axis',(0.,-1.,0.)) ;
#44822 = DIRECTION('ref_axis',(1.,0.,-2.84217094304056E-13)) ;
#44823 = DIRECTION('center_axis',(-1.,-2.90739654573678E-15,1.48422940604576E-13)) ;
#44824 = DIRECTION('ref_axis',(1.07006707598247E-13,-0.707106781186447,0.707106781186648)) ;
#44825 = DIRECTION('center_axis',(-1.,0.,1.42108547152028E-13)) ;
#44826 = DIRECTION('ref_axis',(0.,-1.,0.)) ;
#44827 = DIRECTION('',(-1.,-2.90739654573678E-15,1.48422940604576E-13)) ;
#44828 = DIRECTION('',(1.,2.90739654573678E-15,-1.48422940604576E-13)) ;
#44829 = DIRECTION('center_axis',(1.42108547152028E-13,0.,1.)) ;
#44830 = DIRECTION('ref_axis',(1.,0.,-1.81318720449162E-13)) ;
#44831 = DIRECTION('center_axis',(0.,-5.59482469102493E-13,1.)) ;
#44832 = DIRECTION('ref_axis',(-1.,0.,0.)) ;
#44833 = DIRECTION('center_axis',(0.,-1.,0.)) ;
#44834 = DIRECTION('ref_axis',(-1.42108547152069E-13,0.,-1.)) ;
#44835 = DIRECTION('center_axis',(-1.48506207331423E-13,-2.17161023787768E-15,
-1.)) ;
#44836 = DIRECTION('ref_axis',(-0.707106781186481,0.707106781186614,1.03474185927037E-13)) ;
#44837 = DIRECTION('center_axis',(1.,0.,-1.42108547152028E-13)) ;
#44838 = DIRECTION('ref_axis',(0.,-1.,0.)) ;
#44839 = DIRECTION('center_axis',(-1.42108547152028E-13,0.,-1.)) ;
#44840 = DIRECTION('ref_axis',(-1.,0.,1.81318720449162E-13)) ;
#44841 = DIRECTION('center_axis',(0.,0.,-1.)) ;
#44842 = DIRECTION('ref_axis',(1.,0.,0.)) ;
#44843 = DIRECTION('center_axis',(0.,-1.,0.)) ;
#44844 = DIRECTION('ref_axis',(1.42108547152028E-13,0.,1.)) ;
#44845 = DIRECTION('center_axis',(1.48422940604576E-13,2.17161023787771E-15,
1.)) ;
#44846 = DIRECTION('ref_axis',(0.707106781186481,0.707106781186614,-1.06486428110432E-13)) ;
#44847 = DIRECTION('center_axis',(-1.,0.,1.42108547152028E-13)) ;
#44848 = DIRECTION('ref_axis',(0.,-1.,0.)) ;
#44849 = DIRECTION('center_axis',(2.90739654573712E-15,-1.,2.17161023787728E-15)) ;
#44850 = DIRECTION('ref_axis',(-0.707106781186447,-5.20279487791395E-16,0.707106781186648)) ;
#44851 = DIRECTION('center_axis',(0.,1.,0.)) ;
#44852 = DIRECTION('ref_axis',(-1.,0.,2.84217094304097E-13)) ;
#44853 = DIRECTION('',(-2.90739654573712E-15,1.,-2.17161023787728E-15)) ;
#44854 = DIRECTION('',(2.90739654573712E-15,-1.,2.17161023787728E-15)) ;
#44855 = DIRECTION('center_axis',(1.48422940604576E-13,2.17161023787771E-15,
1.)) ;
#44856 = DIRECTION('ref_axis',(1.,0.,-1.79034390112784E-13)) ;
#44857 = DIRECTION('center_axis',(0.,-1.,0.)) ;
#44858 = DIRECTION('ref_axis',(1.,0.,-2.84217094304379E-13)) ;
#44859 = DIRECTION('center_axis',(-1.48422940604576E-13,-2.17161023787771E-15,
-1.)) ;
#44860 = DIRECTION('ref_axis',(-2.92171142922377E-14,-1.,2.17161023788205E-15)) ;
#44861 = DIRECTION('center_axis',(1.48422940604576E-13,2.17161023787771E-15,
1.)) ;
#44862 = DIRECTION('ref_axis',(-2.92171142922377E-14,-1.,2.17161023788205E-15)) ;
#44863 = DIRECTION('center_axis',(-2.90739654573712E-15,1.,-2.17161023787728E-15)) ;
#44864 = DIRECTION('ref_axis',(0.707106781186749,3.59140013838637E-15,0.707106781186347)) ;
#44865 = DIRECTION('',(2.90739654573712E-15,-1.,2.17161023787728E-15)) ;
#44866 = DIRECTION('',(-2.90739654573712E-15,1.,-2.17161023787728E-15)) ;
#44867 = DIRECTION('center_axis',(-1.,-2.90739654573678E-15,1.48422940604576E-13)) ;
#44868 = DIRECTION('ref_axis',(1.07006707598247E-13,-0.707106781186447,0.707106781186648)) ;
#44869 = DIRECTION('center_axis',(1.,0.,-1.42108547151988E-13)) ;
#44870 = DIRECTION('ref_axis',(1.42108547151988E-13,0.,1.)) ;
#44871 = DIRECTION('',(1.,2.90739654573678E-15,-1.48422940604576E-13)) ;
#44872 = DIRECTION('',(-1.,-2.90739654573678E-15,1.48422940604576E-13)) ;
#44873 = DIRECTION('center_axis',(1.42108547152028E-13,0.,1.)) ;
#44874 = DIRECTION('ref_axis',(1.,0.,-1.81318720449162E-13)) ;
#44875 = DIRECTION('center_axis',(0.,0.,1.)) ;
#44876 = DIRECTION('ref_axis',(0.,1.,0.)) ;
#44877 = DIRECTION('center_axis',(-1.,0.,1.42108547152028E-13)) ;
#44878 = DIRECTION('ref_axis',(-1.42108547152028E-13,0.,-1.)) ;
#44879 = DIRECTION('center_axis',(-1.48506207331423E-13,-2.17161023787768E-15,
-1.)) ;
#44880 = DIRECTION('ref_axis',(0.707106781186481,0.707106781186614,-1.06545306577632E-13)) ;
#44881 = DIRECTION('center_axis',(0.,-1.,0.)) ;
#44882 = DIRECTION('ref_axis',(-1.,0.,2.84217094304056E-13)) ;
#44883 = DIRECTION('center_axis',(1.,2.90739654573678E-15,-1.48506207331423E-13)) ;
#44884 = DIRECTION('ref_axis',(-1.02953906439241E-13,-0.707106781186648,-0.707106781186447)) ;
#44885 = DIRECTION('center_axis',(1.,0.,-1.42108547152028E-13)) ;
#44886 = DIRECTION('ref_axis',(0.,-1.,0.)) ;
#44887 = DIRECTION('',(1.,2.90739654573678E-15,-1.48506207331423E-13)) ;
#44888 = DIRECTION('',(-1.,-2.90739654573678E-15,1.48506207331423E-13)) ;
#44889 = DIRECTION('center_axis',(2.90739654573712E-15,-1.,2.17161023787725E-15)) ;
#44890 = DIRECTION('ref_axis',(0.707106781186447,5.20279487791416E-16,-0.707106781186648)) ;
#44891 = DIRECTION('center_axis',(0.,1.,0.)) ;
#44892 = DIRECTION('ref_axis',(1.,0.,-2.84217094303895E-13)) ;
#44893 = DIRECTION('',(-2.90739654573712E-15,1.,-2.17161023787725E-15)) ;
#44894 = DIRECTION('',(2.90739654573712E-15,-1.,2.17161023787725E-15)) ;
#44895 = DIRECTION('center_axis',(-1.48506207331423E-13,-2.17161023787768E-15,
-1.)) ;
#44896 = DIRECTION('ref_axis',(-1.,0.,1.79034390112784E-13)) ;
#44897 = DIRECTION('center_axis',(0.,-1.,0.)) ;
#44898 = DIRECTION('ref_axis',(-1.,0.,2.84217094303814E-13)) ;
#44899 = DIRECTION('center_axis',(1.48506207331423E-13,2.17161023787768E-15,
1.)) ;
#44900 = DIRECTION('ref_axis',(-2.67147415300443E-14,-1.,2.17161023788165E-15)) ;
#44901 = DIRECTION('center_axis',(-1.48506207331423E-13,-2.17161023787768E-15,
-1.)) ;
#44902 = DIRECTION('ref_axis',(-2.67147415300443E-14,-1.,2.17161023788165E-15)) ;
#44903 = DIRECTION('center_axis',(-2.90739654573712E-15,1.,-2.17161023787725E-15)) ;
#44904 = DIRECTION('ref_axis',(-0.707106781186648,-3.59140013838627E-15,-0.707106781186447)) ;
#44905 = DIRECTION('',(2.90739654573712E-15,-1.,2.17161023787725E-15)) ;
#44906 = DIRECTION('',(-2.90739654573712E-15,1.,-2.17161023787725E-15)) ;
#44907 = DIRECTION('center_axis',(-1.48256407150882E-13,-2.17161023787771E-15,
-1.)) ;
#44908 = DIRECTION('ref_axis',(0.707106781186548,0.707106781186548,-1.0636867117604E-13)) ;
#44909 = DIRECTION('',(1.48256407150882E-13,2.17161023787771E-15,1.)) ;
#44910 = DIRECTION('',(-1.48256407150882E-13,-2.17161023787771E-15,-1.)) ;
#44911 = DIRECTION('center_axis',(1.,2.90739654573678E-15,-1.48506207331423E-13)) ;
#44912 = DIRECTION('ref_axis',(-1.02953906439241E-13,-0.707106781186648,-0.707106781186447)) ;
#44913 = DIRECTION('center_axis',(-1.,0.,1.42108547152028E-13)) ;
#44914 = DIRECTION('ref_axis',(-1.42108547152028E-13,0.,-1.)) ;
#44915 = DIRECTION('',(-1.,-2.90739654573678E-15,1.48506207331423E-13)) ;
#44916 = DIRECTION('',(1.,2.90739654573678E-15,-1.48506207331423E-13)) ;
#44917 = DIRECTION('center_axis',(1.48256407150882E-13,2.17161023787771E-15,
1.)) ;
#44918 = DIRECTION('ref_axis',(-0.707106781186548,0.707106781186548,1.03297550525445E-13)) ;
#44919 = DIRECTION('',(-1.48256407150882E-13,-2.17161023787771E-15,-1.)) ;
#44920 = DIRECTION('',(1.48256407150882E-13,2.17161023787771E-15,1.)) ;
#44921 = DIRECTION('center_axis',(0.408248290463711,0.408248290463711,-0.816496580927878)) ;
#44922 = DIRECTION('ref_axis',(-0.577350269189815,-0.577350269189702,-0.57735026918936)) ;
#44923 = DIRECTION('center_axis',(2.9073965457371E-15,-1.,2.17161023787725E-15)) ;
#44924 = DIRECTION('ref_axis',(-0.707106781186619,-3.59140013838624E-15,-0.707106781186476)) ;
#44925 = DIRECTION('center_axis',(0.408248290463901,-0.816496580927688,-0.408248290463901)) ;
#44926 = DIRECTION('ref_axis',(-0.577350269189512,-0.577350269189626,0.57735026918974)) ;
#44927 = DIRECTION('center_axis',(2.9073965457371E-15,-1.,2.17161023787728E-15)) ;
#44928 = DIRECTION('ref_axis',(-0.707106781186334,-5.20279487790807E-16,0.707106781186761)) ;
#44929 = DIRECTION('center_axis',(1.48422940604576E-13,2.17161023787771E-15,
1.)) ;
#44930 = DIRECTION('ref_axis',(0.707106781186548,-0.707106781186548,-1.03415307459846E-13)) ;
#44931 = DIRECTION('center_axis',(2.84217094304056E-13,0.,1.)) ;
#44932 = DIRECTION('ref_axis',(0.,-1.,0.)) ;
#44933 = DIRECTION('',(1.48422940604576E-13,2.17161023787771E-15,1.)) ;
#44934 = DIRECTION('center_axis',(-2.84217094304056E-13,0.,-1.)) ;
#44935 = DIRECTION('ref_axis',(1.,0.,-2.84217094304056E-13)) ;
#44936 = DIRECTION('',(-1.48422940604576E-13,-2.17161023787771E-15,-1.)) ;
#44937 = DIRECTION('center_axis',(-0.408248290463711,-0.816496580927764,0.408248290463939)) ;
#44938 = DIRECTION('ref_axis',(0.57735026918955,-0.57735026918955,-0.577350269189777)) ;
#44939 = DIRECTION('center_axis',(2.9073965457371E-15,-1.,2.17161023787725E-15)) ;
#44940 = DIRECTION('ref_axis',(0.707106781186334,5.20279487790828E-16,-0.707106781186761)) ;
#44941 = DIRECTION('center_axis',(0.408248290463901,-0.408248290463674,-0.816496580927802)) ;
#44942 = DIRECTION('ref_axis',(0.57735026918974,-0.577350269189626,0.577350269189512)) ;
#44943 = DIRECTION('center_axis',(2.9073965457371E-15,-1.,2.17161023787728E-15)) ;
#44944 = DIRECTION('ref_axis',(0.707106781186619,3.59140013838626E-15,0.707106781186476)) ;
#44945 = DIRECTION('center_axis',(-1.,-2.9073965457368E-15,1.48256407150882E-13)) ;
#44946 = DIRECTION('ref_axis',(-2.90739654573712E-15,1.,-2.17161023787733E-15)) ;
#44947 = DIRECTION('',(1.48256407150882E-13,2.17161023787776E-15,1.)) ;
#44948 = DIRECTION('center_axis',(-2.9073965457371E-15,1.,-2.17161023787728E-15)) ;
#44949 = DIRECTION('ref_axis',(-0.707106781186347,-5.20279487790871E-16,0.707106781186749)) ;
#44950 = DIRECTION('',(-2.9073965457371E-15,1.,-2.17161023787728E-15)) ;
#44951 = DIRECTION('center_axis',(-2.90739654573709E-15,1.,-2.17161023787725E-15)) ;
#44952 = DIRECTION('ref_axis',(-1.,-2.90739654573647E-15,2.84217094304076E-13)) ;
#44953 = DIRECTION('',(-2.9073965457371E-15,1.,-2.17161023787728E-15)) ;
#44954 = DIRECTION('center_axis',(1.48422940604576E-13,2.17161023787771E-15,
1.)) ;
#44955 = DIRECTION('ref_axis',(-1.,-2.90739654573678E-15,1.48422940604576E-13)) ;
#44956 = DIRECTION('',(2.9073965457371E-15,-1.,2.17161023787728E-15)) ;
#44957 = DIRECTION('',(1.,2.90739654573678E-15,-1.48422940604576E-13)) ;
#44958 = DIRECTION('center_axis',(2.9073965457371E-15,-1.,2.17161023787728E-15)) ;
#44959 = DIRECTION('ref_axis',(0.707106781186648,3.59140013838628E-15,0.707106781186447)) ;
#44960 = DIRECTION('',(-2.9073965457371E-15,1.,-2.17161023787728E-15)) ;
#44961 = DIRECTION('center_axis',(-2.90739654573709E-15,1.,-2.17161023787725E-15)) ;
#44962 = DIRECTION('ref_axis',(1.,2.90739654573647E-15,-2.84217094304036E-13)) ;
#44963 = DIRECTION('center_axis',(1.,2.90739654573678E-15,-1.48422940604576E-13)) ;
#44964 = DIRECTION('ref_axis',(2.9073965457371E-15,-1.,2.17161023787728E-15)) ;
#44965 = DIRECTION('',(2.9073965457371E-15,-1.,2.17161023787725E-15)) ;
#44966 = DIRECTION('',(-1.48422940604576E-13,-2.17161023787768E-15,-1.)) ;
#44967 = DIRECTION('center_axis',(2.9073965457371E-15,-1.,2.17161023787728E-15)) ;
#44968 = DIRECTION('ref_axis',(1.48422940604576E-13,2.17161023787771E-15,
1.)) ;
#44969 = DIRECTION('center_axis',(2.9073965457371E-15,-1.,2.17161023787728E-15)) ;
#44970 = DIRECTION('ref_axis',(1.48422940604576E-13,2.17161023787771E-15,
1.)) ;
#44971 = DIRECTION('center_axis',(1.,2.9073965457368E-15,-1.48256407150882E-13)) ;
#44972 = DIRECTION('ref_axis',(2.90739654573712E-15,-1.,2.17161023787733E-15)) ;
#44973 = DIRECTION('',(1.48256407150883E-13,2.17161023787776E-15,1.)) ;
#44974 = DIRECTION('center_axis',(-1.48256407150882E-13,-2.17161023787776E-15,
-1.)) ;
#44975 = DIRECTION('ref_axis',(1.,-2.20726215083294E-14,-1.48256407150882E-13)) ;
#44976 = DIRECTION('center_axis',(-2.9073965457371E-15,1.,-2.17161023787725E-15)) ;
#44977 = DIRECTION('ref_axis',(0.707106781186347,5.20279487790892E-16,-0.707106781186749)) ;
#44978 = DIRECTION('',(-2.9073965457371E-15,1.,-2.17161023787725E-15)) ;
#44979 = DIRECTION('center_axis',(-1.37109652768972E-44,-1.,2.17161023787773E-15)) ;
#44980 = DIRECTION('ref_axis',(-1.42108547152028E-13,-2.17161023787773E-15,
-1.)) ;
#44981 = DIRECTION('center_axis',(2.9073965457371E-15,-1.,2.17161023787725E-15)) ;
#44982 = DIRECTION('ref_axis',(-0.707106781186648,-3.59140013838626E-15,-0.707106781186447)) ;
#44983 = DIRECTION('',(-2.9073965457371E-15,1.,-2.17161023787725E-15)) ;
#44984 = DIRECTION('center_axis',(-1.37109652768972E-44,-1.,2.17161023787773E-15)) ;
#44985 = DIRECTION('ref_axis',(-1.,6.17208751770548E-28,2.84217094304056E-13)) ;
#44986 = DIRECTION('',(2.9073965457371E-15,-1.,2.17161023787725E-15)) ;
#44987 = DIRECTION('center_axis',(-1.48506207331423E-13,-2.17161023787768E-15,
-1.)) ;
#44988 = DIRECTION('ref_axis',(1.,2.90739654573677E-15,-1.48506207331423E-13)) ;
#44989 = DIRECTION('center_axis',(-1.48506207331423E-13,-2.17161023787768E-15,
-1.)) ;
#44990 = DIRECTION('ref_axis',(0.707106781186497,0.707106781186598,-1.06545306577635E-13)) ;
#44991 = DIRECTION('',(1.,2.90739654573677E-15,-1.48506207331423E-13)) ;
#44992 = DIRECTION('',(2.90739654573709E-15,-1.,2.17161023787725E-15)) ;
#44993 = DIRECTION('',(1.,2.90739654573677E-15,-1.48506207331423E-13)) ;
#44994 = DIRECTION('',(-2.90739654573709E-15,1.,-2.17161023787725E-15)) ;
#44995 = DIRECTION('',(1.,2.90739654573677E-15,-1.48506207331423E-13)) ;
#44996 = DIRECTION('center_axis',(-1.48506207331423E-13,-2.17161023787768E-15,
-1.)) ;
#44997 = DIRECTION('ref_axis',(-0.707106781186522,0.707106781186573,1.03474185927043E-13)) ;
#44998 = DIRECTION('center_axis',(-1.,-2.90739654573678E-15,1.48422940604577E-13)) ;
#44999 = DIRECTION('ref_axis',(2.9073965457371E-15,-1.,2.17161023787728E-15)) ;
#45000 = DIRECTION('',(1.48422940604577E-13,2.17161023787768E-15,1.)) ;
#45001 = DIRECTION('center_axis',(-1.48422940604576E-13,-2.17161023787771E-15,
-1.)) ;
#45002 = DIRECTION('ref_axis',(1.,2.90739654573678E-15,-1.48422940604576E-13)) ;
#45003 = DIRECTION('',(1.,2.90739654573678E-15,-1.48422940604576E-13)) ;
#45004 = DIRECTION('',(2.9073965457371E-15,-1.,2.17161023787728E-15)) ;
#45005 = DIRECTION('',(1.,2.90739654573678E-15,-1.48422940604576E-13)) ;
#45006 = DIRECTION('',(-2.9073965457371E-15,1.,-2.17161023787728E-15)) ;
#45007 = DIRECTION('center_axis',(2.9073965457371E-15,-1.,2.17161023787728E-15)) ;
#45008 = DIRECTION('ref_axis',(1.48422940604576E-13,2.17161023787771E-15,
1.)) ;
#45009 = DIRECTION('',(-1.,-2.90739654573678E-15,1.48422940604576E-13)) ;
#45010 = DIRECTION('',(-1.48422940604576E-13,-2.17161023787771E-15,-1.)) ;
#45011 = DIRECTION('',(1.,2.90739654573678E-15,-1.48506207331423E-13)) ;
#45012 = DIRECTION('',(1.48422940604577E-13,2.17161023787771E-15,1.)) ;
#45013 = DIRECTION('center_axis',(1.48506207331423E-13,2.17161023787768E-15,
1.)) ;
#45014 = DIRECTION('ref_axis',(-1.,-2.90739654573677E-15,1.48506207331423E-13)) ;
#45015 = DIRECTION('',(-1.,-2.90739654573678E-15,1.48506207331423E-13)) ;
#45016 = DIRECTION('',(2.9073965457371E-15,-1.,2.17161023787725E-15)) ;
#45017 = DIRECTION('center_axis',(1.48506207331423E-13,2.17161023787768E-15,
1.)) ;
#45018 = DIRECTION('ref_axis',(-0.707106781186522,0.707106781186573,1.03474185927043E-13)) ;
#45019 = DIRECTION('',(-1.,-2.90739654573677E-15,1.48506207331423E-13)) ;
#45020 = DIRECTION('',(2.90739654573709E-15,-1.,2.17161023787725E-15)) ;
#45021 = DIRECTION('',(1.,3.55570196157628E-15,-1.48506207331423E-13)) ;
#45022 = DIRECTION('',(-2.90739654573709E-15,1.,-2.17161023787725E-15)) ;
#45023 = DIRECTION('',(-1.,-2.90739654573677E-15,1.48506207331423E-13)) ;
#45024 = DIRECTION('center_axis',(1.48506207331423E-13,2.17161023787768E-15,
1.)) ;
#45025 = DIRECTION('ref_axis',(0.707106781186548,0.707106781186548,-1.06545306577642E-13)) ;
#45026 = DIRECTION('',(-2.9073965457371E-15,1.,-2.17161023787725E-15)) ;
#45027 = DIRECTION('center_axis',(-2.90739654573709E-15,1.,-2.17161023787725E-15)) ;
#45028 = DIRECTION('ref_axis',(1.48506207331423E-13,2.17161023787768E-15,
1.)) ;
#45029 = DIRECTION('',(-1.48506207331423E-13,-2.17161023787768E-15,-1.)) ;
#45030 = DIRECTION('',(1.,2.90739654573677E-15,-1.48506207331423E-13)) ;
#45031 = DIRECTION('',(1.48506207331423E-13,2.17161023787768E-15,1.)) ;
#45032 = DIRECTION('',(1.,2.90739654573677E-15,-1.48506207331423E-13)) ;
#45033 = DIRECTION('center_axis',(-1.,-2.90739654573677E-15,1.48506207331423E-13)) ;
#45034 = DIRECTION('ref_axis',(1.02953906439256E-13,0.707106781186549,0.707106781186546)) ;
#45035 = DIRECTION('center_axis',(-1.,-2.90739654573677E-15,1.48506207331423E-13)) ;
#45036 = DIRECTION('ref_axis',(1.02953906439256E-13,0.707106781186543,0.707106781186552)) ;
#45037 = DIRECTION('center_axis',(1.,2.90739654573677E-15,-1.48506207331423E-13)) ;
#45038 = DIRECTION('ref_axis',(1.02953906439253E-13,0.707106781186567,0.707106781186528)) ;
#45039 = DIRECTION('center_axis',(-1.,-2.90739654573677E-15,1.48506207331423E-13)) ;
#45040 = DIRECTION('ref_axis',(-1.07065586065433E-13,0.707106781186549,-0.707106781186546)) ;
#45041 = DIRECTION('center_axis',(-1.,-2.90739654573677E-15,1.48506207331423E-13)) ;
#45042 = DIRECTION('ref_axis',(-1.07065586065431E-13,0.707106781186565,-0.70710678118653)) ;
#45043 = DIRECTION('center_axis',(1.,2.90739654573677E-15,-1.48506207331423E-13)) ;
#45044 = DIRECTION('ref_axis',(-1.07065586065434E-13,0.70710678118654,-0.707106781186555)) ;
#45045 = DIRECTION('center_axis',(1.,2.90739654573678E-15,-1.48422940604576E-13)) ;
#45046 = DIRECTION('ref_axis',(1.02895027972065E-13,0.707106781186482,0.707106781186613)) ;
#45047 = DIRECTION('',(-1.,-2.90739654573678E-15,1.48422940604576E-13)) ;
#45048 = DIRECTION('center_axis',(1.,2.90739654573678E-15,-1.48422940604576E-13)) ;
#45049 = DIRECTION('ref_axis',(-1.07006707598192E-13,0.707106781186829,-0.707106781186266)) ;
#45050 = DIRECTION('',(-1.,-2.90739654573678E-15,1.48422940604576E-13)) ;
#45051 = DIRECTION('center_axis',(1.,2.90739654573678E-15,-1.48422940604576E-13)) ;
#45052 = DIRECTION('ref_axis',(2.9073965457371E-15,-1.,2.17161023787728E-15)) ;
#45053 = DIRECTION('',(1.48422940604576E-13,2.17161023787771E-15,1.)) ;
#45054 = DIRECTION('',(2.9073965457371E-15,-1.,2.17161023787728E-15)) ;
#45055 = DIRECTION('',(-1.48422940604576E-13,-2.17161023787768E-15,-1.)) ;
#45056 = DIRECTION('',(-2.9073965457371E-15,1.,-2.17161023787725E-15)) ;
#45057 = DIRECTION('center_axis',(-2.9073965457371E-15,1.,-2.17161023787728E-15)) ;
#45058 = DIRECTION('ref_axis',(0.707106781186347,5.20279487790871E-16,-0.707106781186749)) ;
#45059 = DIRECTION('center_axis',(2.9073965457371E-15,-1.,2.17161023787728E-15)) ;
#45060 = DIRECTION('ref_axis',(0.707106781186334,5.20279487790807E-16,-0.707106781186761)) ;
#45061 = DIRECTION('center_axis',(-2.90739654573709E-15,1.,-2.17161023787725E-15)) ;
#45062 = DIRECTION('ref_axis',(1.,2.90739654573647E-15,-2.84217094304056E-13)) ;
#45063 = DIRECTION('center_axis',(1.,2.90739654573677E-15,-1.48506207331423E-13)) ;
#45064 = DIRECTION('ref_axis',(2.90739654573709E-15,-1.,2.17161023787725E-15)) ;
#45065 = DIRECTION('',(1.48506207331423E-13,2.17161023787768E-15,1.)) ;
#45066 = DIRECTION('',(2.90739654573709E-15,-1.,2.17161023787725E-15)) ;
#45067 = DIRECTION('center_axis',(-1.,-2.90739654573677E-15,1.48506207331423E-13)) ;
#45068 = DIRECTION('ref_axis',(-1.07065586065434E-13,0.70710678118654,-0.707106781186555)) ;
#45069 = DIRECTION('',(-1.48506207331423E-13,-2.17161023787768E-15,-1.)) ;
#45070 = DIRECTION('center_axis',(-1.,-2.90739654573677E-15,1.48506207331423E-13)) ;
#45071 = DIRECTION('ref_axis',(1.02953906439253E-13,0.707106781186567,0.707106781186528)) ;
#45072 = DIRECTION('',(-2.90739654573709E-15,1.,-2.17161023787725E-15)) ;
#45073 = DIRECTION('center_axis',(-1.,-2.90739654573677E-15,1.48506207331423E-13)) ;
#45074 = DIRECTION('ref_axis',(2.90739654573709E-15,-1.,2.17161023787725E-15)) ;
#45075 = DIRECTION('',(2.90739654573709E-15,-1.,2.17161023787725E-15)) ;
#45076 = DIRECTION('center_axis',(1.,2.90739654573677E-15,-1.48506207331423E-13)) ;
#45077 = DIRECTION('ref_axis',(1.02953906439256E-13,0.707106781186544,0.707106781186551)) ;
#45078 = DIRECTION('',(1.48506207331423E-13,2.17161023787768E-15,1.)) ;
#45079 = DIRECTION('center_axis',(1.,2.90739654573677E-15,-1.48506207331423E-13)) ;
#45080 = DIRECTION('ref_axis',(-1.07065586065431E-13,0.707106781186565,-0.70710678118653)) ;
#45081 = DIRECTION('',(-2.90739654573709E-15,1.,-2.17161023787725E-15)) ;
#45082 = DIRECTION('',(-1.48506207331423E-13,-2.17161023787768E-15,-1.)) ;
#45083 = DIRECTION('center_axis',(2.9073965457371E-15,-1.,2.17161023787728E-15)) ;
#45084 = DIRECTION('ref_axis',(-0.707106781186749,-3.59140013838635E-15,-0.707106781186347)) ;
#45085 = DIRECTION('center_axis',(2.9073965457371E-15,-1.,2.17161023787728E-15)) ;
#45086 = DIRECTION('ref_axis',(-0.70710678118669,-3.59140013838631E-15,-0.707106781186405)) ;
#45087 = DIRECTION('',(-2.9073965457371E-15,1.,-2.17161023787728E-15)) ;
#45088 = DIRECTION('center_axis',(-2.90739654573709E-15,1.,-2.17161023787725E-15)) ;
#45089 = DIRECTION('ref_axis',(-1.,-2.90739654573647E-15,2.84217094304056E-13)) ;
#45090 = DIRECTION('center_axis',(-1.,-2.90739654573678E-15,1.48422940604577E-13)) ;
#45091 = DIRECTION('ref_axis',(2.9073965457371E-15,-1.,2.17161023787728E-15)) ;
#45092 = DIRECTION('',(-1.48422940604577E-13,-2.17161023787771E-15,-1.)) ;
#45093 = DIRECTION('',(2.9073965457371E-15,-1.,2.17161023787725E-15)) ;
#45094 = DIRECTION('',(1.48422940604577E-13,2.17161023787768E-15,1.)) ;
#45095 = DIRECTION('center_axis',(2.90739654573709E-15,-1.,2.17161023787725E-15)) ;
#45096 = DIRECTION('ref_axis',(0.414201389893284,0.,0.910185260598342)) ;
#45097 = DIRECTION('center_axis',(2.84217094304016E-13,2.17161023787773E-15,
1.)) ;
#45098 = DIRECTION('ref_axis',(0.,1.,-2.17161023787773E-15)) ;
#45099 = DIRECTION('center_axis',(2.90739654573709E-15,-1.,2.17161023787725E-15)) ;
#45100 = DIRECTION('ref_axis',(1.,2.90739654573647E-15,-2.84217094304036E-13)) ;
#45101 = DIRECTION('center_axis',(2.90739654573709E-15,-1.,2.17161023787725E-15)) ;
#45102 = DIRECTION('ref_axis',(-0.41420138989285,0.,0.910185260598539)) ;
#45103 = DIRECTION('center_axis',(2.90739654573709E-15,-1.,2.17161023787725E-15)) ;
#45104 = DIRECTION('ref_axis',(-1.,-2.90739654573647E-15,2.84217094304076E-13)) ;
#45105 = DIRECTION('center_axis',(2.84217094304056E-13,2.17161023787773E-15,
1.)) ;
#45106 = DIRECTION('ref_axis',(1.,-6.17208751770549E-28,-2.84217094304056E-13)) ;
#45107 = DIRECTION('center_axis',(2.90739654573709E-15,-1.,2.17161023787725E-15)) ;
#45108 = DIRECTION('ref_axis',(0.,0.,-1.)) ;
#45109 = DIRECTION('center_axis',(2.90739654573709E-15,-1.,2.17161023787725E-15)) ;
#45110 = DIRECTION('ref_axis',(1.,2.90739654573647E-15,-2.84217094304056E-13)) ;
#45111 = DIRECTION('center_axis',(-2.84217094304016E-13,-2.17161023787773E-15,
-1.)) ;
#45112 = DIRECTION('ref_axis',(-1.,6.17208751770461E-28,2.84217094304016E-13)) ;
#45113 = DIRECTION('center_axis',(0.408248290463711,0.408248290463711,-0.816496580927878)) ;
#45114 = DIRECTION('ref_axis',(-0.577350269189815,-0.577350269189702,-0.57735026918936)) ;
#45115 = DIRECTION('center_axis',(2.84217094304056E-13,2.17161023787773E-15,
1.)) ;
#45116 = DIRECTION('ref_axis',(-1.,6.17208751770549E-28,2.84217094304056E-13)) ;
#45117 = DIRECTION('center_axis',(1.,-3.08604375885274E-28,-1.42108547152028E-13)) ;
#45118 = DIRECTION('ref_axis',(1.04928462787225E-43,-1.,2.17161023787773E-15)) ;
#45119 = DIRECTION('center_axis',(2.90739654573709E-15,-1.,2.17161023787725E-15)) ;
#45120 = DIRECTION('ref_axis',(0.,0.,-1.)) ;
#45121 = DIRECTION('center_axis',(-2.84217094304097E-13,-2.17161023787773E-15,
-1.)) ;
#45122 = DIRECTION('ref_axis',(0.,1.,-2.17161023787773E-15)) ;
#45123 = DIRECTION('center_axis',(2.90739654573709E-15,-1.,2.17161023787725E-15)) ;
#45124 = DIRECTION('ref_axis',(-1.,-2.90739654573647E-15,2.84217094304056E-13)) ;
#45125 = DIRECTION('center_axis',(-0.408248290463711,-0.816496580927764,0.408248290463939)) ;
#45126 = DIRECTION('ref_axis',(0.577350269189474,-0.577350269189474,-0.577350269189929)) ;
#45127 = DIRECTION('center_axis',(-1.,3.08604375885274E-28,1.42108547152028E-13)) ;
#45128 = DIRECTION('ref_axis',(-1.42108547152028E-13,-2.17161023787773E-15,
-1.)) ;
#45129 = DIRECTION('center_axis',(2.84217094304056E-13,2.17161023787773E-15,
1.)) ;
#45130 = DIRECTION('ref_axis',(0.,-1.,2.17161023787773E-15)) ;
#45131 = DIRECTION('center_axis',(1.,2.90739654573678E-15,-1.48422940604576E-13)) ;
#45132 = DIRECTION('ref_axis',(-1.02895027972062E-13,-0.707106781186499,-0.707106781186596)) ;
#45133 = DIRECTION('center_axis',(-1.48422940604576E-13,-2.17161023787768E-15,
-1.)) ;
#45134 = DIRECTION('ref_axis',(-0.707106781186497,0.707106781186598,1.03415307459839E-13)) ;
#45135 = DIRECTION('center_axis',(2.84217094304056E-13,-2.82045484066158E-13,
1.)) ;
#45136 = DIRECTION('ref_axis',(-1.,6.17208751770553E-28,2.84217094304056E-13)) ;
#45137 = DIRECTION('',(1.48422940604576E-13,2.17161023787768E-15,1.)) ;
#45138 = DIRECTION('center_axis',(1.48422940604577E-13,2.17161023787768E-15,
1.)) ;
#45139 = DIRECTION('ref_axis',(0.707106781186548,0.707106781186548,-1.06486428110442E-13)) ;
#45140 = DIRECTION('',(-1.48422940604577E-13,-2.17161023787768E-15,-1.)) ;
#45141 = DIRECTION('center_axis',(-6.31373210429172E-30,2.17161023787773E-15,
1.)) ;
#45142 = DIRECTION('ref_axis',(1.37109652768972E-44,1.,-2.17161023787773E-15)) ;
#45143 = DIRECTION('center_axis',(1.,2.90739654573677E-15,-1.48506207331423E-13)) ;
#45144 = DIRECTION('ref_axis',(-1.02953906439233E-13,-0.7071067811867,-0.707106781186395)) ;
#45145 = DIRECTION('center_axis',(1.,-3.08604375885274E-28,-1.42108547152028E-13)) ;
#45146 = DIRECTION('ref_axis',(-1.42108547152028E-13,-2.17161023787773E-15,
-1.)) ;
#45147 = DIRECTION('',(-1.,-2.90739654573677E-15,1.48506207331423E-13)) ;
#45148 = DIRECTION('center_axis',(1.,-3.08604375885274E-28,-1.42108547152028E-13)) ;
#45149 = DIRECTION('ref_axis',(1.04928462787225E-43,-1.,2.17161023787773E-15)) ;
#45150 = DIRECTION('center_axis',(1.,2.90739654573677E-15,-1.48506207331423E-13)) ;
#45151 = DIRECTION('ref_axis',(-1.02953906439233E-13,-0.7071067811867,-0.707106781186395)) ;
#45152 = DIRECTION('center_axis',(-1.,3.08604375885274E-28,1.42108547152028E-13)) ;
#45153 = DIRECTION('ref_axis',(-1.42108547152028E-13,-2.17161023787773E-15,
-1.)) ;
#45154 = DIRECTION('',(-1.,-2.90739654573677E-15,1.48506207331423E-13)) ;
#45155 = DIRECTION('center_axis',(-1.,6.17208751770549E-28,2.84217094304056E-13)) ;
#45156 = DIRECTION('ref_axis',(-7.76657193310222E-43,-1.,2.17161023787773E-15)) ;
#45157 = DIRECTION('center_axis',(2.90739654573709E-15,-1.,2.17161023787725E-15)) ;
#45158 = DIRECTION('ref_axis',(0.707106781186749,3.59140013838632E-15,0.707106781186347)) ;
#45159 = DIRECTION('center_axis',(-1.37109652768972E-44,-1.,2.17161023787773E-15)) ;
#45160 = DIRECTION('ref_axis',(1.42108547152028E-13,2.17161023787773E-15,
1.)) ;
#45161 = DIRECTION('center_axis',(1.37109652768972E-44,1.,-2.17161023787773E-15)) ;
#45162 = DIRECTION('ref_axis',(2.84217094304056E-13,2.17161023787773E-15,
1.)) ;
#45163 = DIRECTION('center_axis',(-1.,-2.90739654573677E-15,1.48506207331423E-13)) ;
#45164 = DIRECTION('ref_axis',(1.62758536466166E-13,0.,1.)) ;
#45165 = DIRECTION('center_axis',(-2.84217094304016E-13,-2.17161023787773E-15,
-1.)) ;
#45166 = DIRECTION('ref_axis',(0.,1.,-2.17161023787773E-15)) ;
#45167 = DIRECTION('center_axis',(1.48506207331423E-13,2.17161023787768E-15,
1.)) ;
#45168 = DIRECTION('ref_axis',(0.707106781186648,0.707106781186447,-1.06545306577657E-13)) ;
#45169 = DIRECTION('center_axis',(-2.84217094304056E-13,-2.17161023787773E-15,
-1.)) ;
#45170 = DIRECTION('ref_axis',(0.,1.,-2.17161023787773E-15)) ;
#45171 = DIRECTION('center_axis',(-1.,-2.90739654573677E-15,1.48506207331423E-13)) ;
#45172 = DIRECTION('ref_axis',(1.62758536466166E-13,0.,1.)) ;
#45173 = DIRECTION('center_axis',(-1.37109652768972E-44,-1.,2.17161023787773E-15)) ;
#45174 = DIRECTION('ref_axis',(-1.42108547152069E-13,-2.17161023787773E-15,
-1.)) ;
#45175 = DIRECTION('center_axis',(-2.90739654573709E-15,1.,-2.17161023787725E-15)) ;
#45176 = DIRECTION('ref_axis',(0.707106781186347,5.20279487790885E-16,-0.707106781186749)) ;
#45177 = DIRECTION('center_axis',(-4.03896783473261E-26,-1.,-1.3993693691415E-13)) ;
#45178 = DIRECTION('ref_axis',(1.,-6.17208751770659E-28,-2.84217094304097E-13)) ;
#45179 = DIRECTION('center_axis',(1.48506207331423E-13,2.17161023787768E-15,
1.)) ;
#45180 = DIRECTION('ref_axis',(0.707106781186548,-0.707106781186548,-1.03474185927047E-13)) ;
#45181 = DIRECTION('center_axis',(2.84217094304056E-13,2.17161023787773E-15,
1.)) ;
#45182 = DIRECTION('ref_axis',(1.,-6.17208751770549E-28,-2.84217094304056E-13)) ;
#45183 = DIRECTION('',(-1.48506207331423E-13,-2.17161023787768E-15,-1.)) ;
#45184 = DIRECTION('center_axis',(-2.84217094304056E-13,-2.17161023787773E-15,
-1.)) ;
#45185 = DIRECTION('ref_axis',(0.,-1.,2.17161023787773E-15)) ;
#45186 = DIRECTION('center_axis',(-1.48506207331423E-13,-2.17161023787768E-15,
-1.)) ;
#45187 = DIRECTION('ref_axis',(-0.707106781186497,-0.707106781186598,1.06545306577635E-13)) ;
#45188 = DIRECTION('center_axis',(-2.84217094304056E-13,-2.17161023787773E-15,
-1.)) ;
#45189 = DIRECTION('ref_axis',(-1.,6.17208751770549E-28,2.84217094304056E-13)) ;
#45190 = DIRECTION('',(1.48506207331423E-13,2.17161023787768E-15,1.)) ;
#45191 = DIRECTION('center_axis',(2.84217094304056E-13,2.17161023787773E-15,
1.)) ;
#45192 = DIRECTION('ref_axis',(0.,-1.,2.17161023787773E-15)) ;
#45193 = DIRECTION('center_axis',(2.90739654573709E-15,-1.,2.17161023787725E-15)) ;
#45194 = DIRECTION('ref_axis',(-0.707106781186648,-3.59140013838625E-15,-0.707106781186447)) ;
#45195 = DIRECTION('center_axis',(7.10542735760242E-14,-1.,2.17161023786763E-15)) ;
#45196 = DIRECTION('ref_axis',(-1.42108547152028E-13,-2.17161023787773E-15,
-1.)) ;
#45197 = DIRECTION('center_axis',(1.37109652768972E-44,1.,-2.17161023787773E-15)) ;
#45198 = DIRECTION('ref_axis',(-2.84217094304056E-13,-2.17161023787773E-15,
-1.)) ;
#45199 = DIRECTION('center_axis',(1.,2.90739654573677E-15,-1.48506207331423E-13)) ;
#45200 = DIRECTION('ref_axis',(-1.42413719407895E-13,0.,-1.)) ;
#45201 = DIRECTION('center_axis',(2.84217094304056E-13,2.17161023787773E-15,
1.)) ;
#45202 = DIRECTION('ref_axis',(0.,1.,-2.17161023787773E-15)) ;
#45203 = DIRECTION('center_axis',(1.48506207331423E-13,2.17161023787768E-15,
1.)) ;
#45204 = DIRECTION('ref_axis',(-0.707106781186548,0.707106781186548,1.03474185927047E-13)) ;
#45205 = DIRECTION('center_axis',(2.84217094304056E-13,-2.82045484066138E-13,
1.)) ;
#45206 = DIRECTION('ref_axis',(0.,1.,2.82045484066138E-13)) ;
#45207 = DIRECTION('center_axis',(1.,2.90739654573677E-15,-1.48506207331423E-13)) ;
#45208 = DIRECTION('ref_axis',(-1.42413719407895E-13,0.,-1.)) ;
#45209 = DIRECTION('center_axis',(-1.37109652768972E-44,-1.,2.17161023787773E-15)) ;
#45210 = DIRECTION('ref_axis',(1.42108547152069E-13,2.17161023787773E-15,
1.)) ;
#45211 = DIRECTION('center_axis',(-2.90739654573709E-15,1.,-2.17161023787725E-15)) ;
#45212 = DIRECTION('ref_axis',(-0.707106781186447,-5.20279487791395E-16,0.707106781186648)) ;
#45213 = DIRECTION('center_axis',(-2.01948391736573E-26,-1.,-6.88826633381363E-14)) ;
#45214 = DIRECTION('ref_axis',(-1.,6.1720875177043E-28,2.84217094304016E-13)) ;
#45215 = DIRECTION('center_axis',(-1.48422940604576E-13,-2.17161023787768E-15,
-1.)) ;
#45216 = DIRECTION('ref_axis',(-0.707106781186497,0.707106781186598,1.03415307459839E-13)) ;
#45217 = DIRECTION('',(1.48422940604576E-13,2.17161023787768E-15,1.)) ;
#45218 = DIRECTION('center_axis',(6.31373210429172E-30,-2.17161023787773E-15,
-1.)) ;
#45219 = DIRECTION('ref_axis',(1.37109652768972E-44,1.,-2.17161023787773E-15)) ;
#45220 = DIRECTION('center_axis',(2.9073965457371E-15,-1.,2.17161023787725E-15)) ;
#45221 = DIRECTION('ref_axis',(0.707106781186749,3.59140013838633E-15,0.707106781186347)) ;
#45222 = DIRECTION('center_axis',(-7.10542735760141E-14,-1.,2.17161023788783E-15)) ;
#45223 = DIRECTION('ref_axis',(1.42108547152028E-13,2.17161023787773E-15,
1.)) ;
#45224 = DIRECTION('center_axis',(-1.37109652768972E-44,-1.,2.17161023787773E-15)) ;
#45225 = DIRECTION('ref_axis',(1.,-6.17208751770548E-28,-2.84217094304056E-13)) ;
#45226 = DIRECTION('center_axis',(1.48422940604576E-13,2.17161023787771E-15,
1.)) ;
#45227 = DIRECTION('ref_axis',(0.707106781186497,-0.707106781186598,-1.03415307459839E-13)) ;
#45228 = DIRECTION('center_axis',(2.84217094304056E-13,2.17161023787773E-15,
1.)) ;
#45229 = DIRECTION('ref_axis',(1.,-6.17208751770549E-28,-2.84217094304056E-13)) ;
#45230 = DIRECTION('center_axis',(-1.48422940604577E-13,-2.17161023787771E-15,
-1.)) ;
#45231 = DIRECTION('ref_axis',(-0.707106781186497,-0.707106781186598,1.06486428110435E-13)) ;
#45232 = DIRECTION('center_axis',(2.84217094304056E-13,2.17161023787773E-15,
1.)) ;
#45233 = DIRECTION('ref_axis',(0.,-1.,2.17161023787773E-15)) ;
#45234 = DIRECTION('center_axis',(-2.9073965457371E-15,1.,-2.17161023787725E-15)) ;
#45235 = DIRECTION('ref_axis',(-0.707106781186447,-5.20279487791402E-16,0.707106781186648)) ;
#45236 = DIRECTION('center_axis',(-1.37109652768972E-44,-1.,2.17161023787773E-15)) ;
#45237 = DIRECTION('ref_axis',(1.42108547152028E-13,2.17161023787773E-15,
1.)) ;
#45238 = DIRECTION('center_axis',(-1.37109652768972E-44,-1.,2.17161023787773E-15)) ;
#45239 = DIRECTION('ref_axis',(-1.,6.17208751770548E-28,2.84217094304056E-13)) ;
#45240 = DIRECTION('center_axis',(-1.,-2.90739654573678E-15,1.48506207331423E-13)) ;
#45241 = DIRECTION('ref_axis',(1.07065586065441E-13,-0.707106781186496,0.707106781186599)) ;
#45242 = DIRECTION('center_axis',(1.,-3.08604375885274E-28,-1.42108547152028E-13)) ;
#45243 = DIRECTION('ref_axis',(1.04928462787225E-43,-1.,2.17161023787773E-15)) ;
#45244 = DIRECTION('center_axis',(-1.,3.08604375885274E-28,1.42108547152028E-13)) ;
#45245 = DIRECTION('ref_axis',(1.42108547152028E-13,2.17161023787773E-15,
1.)) ;
#45246 = DIRECTION('center_axis',(0.408248290463711,-0.816496580927764,-0.408248290463939)) ;
#45247 = DIRECTION('ref_axis',(-0.57735026918955,-0.57735026918955,0.577350269189777)) ;
#45248 = DIRECTION('center_axis',(-0.816496580927688,-0.408248290463958,0.408248290463844)) ;
#45249 = DIRECTION('ref_axis',(0.577350269189702,-0.577350269189702,0.577350269189474)) ;
#45250 = DIRECTION('center_axis',(1.48422940604577E-13,2.17161023787768E-15,
1.)) ;
#45251 = DIRECTION('ref_axis',(0.707106781186548,0.707106781186548,-1.06486428110442E-13)) ;
#45252 = DIRECTION('center_axis',(-2.84217094304056E-13,-2.86388704541914E-13,
-1.)) ;
#45253 = DIRECTION('ref_axis',(1.,-6.17208751770544E-28,-2.84217094304056E-13)) ;
#45254 = DIRECTION('',(-1.48422940604577E-13,-2.17161023787768E-15,-1.)) ;
#45255 = DIRECTION('center_axis',(-1.,-2.90739654573677E-15,1.48506207331423E-13)) ;
#45256 = DIRECTION('ref_axis',(1.07065586065419E-13,-0.707106781186646,0.707106781186449)) ;
#45257 = DIRECTION('center_axis',(-1.,2.84217094304057E-13,1.42108547152027E-13)) ;
#45258 = DIRECTION('ref_axis',(1.42108547152028E-13,2.17161023787773E-15,
1.)) ;
#45259 = DIRECTION('',(1.,2.90739654573677E-15,-1.48506207331423E-13)) ;
#45260 = DIRECTION('center_axis',(-1.,3.08604375885274E-28,1.42108547152028E-13)) ;
#45261 = DIRECTION('ref_axis',(1.04928462787225E-43,-1.,2.17161023787773E-15)) ;
#45262 = DIRECTION('center_axis',(1.42108547152028E-13,2.17161023787773E-15,
1.)) ;
#45263 = DIRECTION('ref_axis',(1.,0.,-1.51582450295488E-13)) ;
#45264 = DIRECTION('center_axis',(-1.,-2.90739654573677E-15,1.48506207331423E-13)) ;
#45265 = DIRECTION('ref_axis',(1.07065586065419E-13,-0.707106781186646,0.707106781186449)) ;
#45266 = DIRECTION('center_axis',(1.,-3.08604375885274E-28,-1.42108547152028E-13)) ;
#45267 = DIRECTION('ref_axis',(1.42108547152028E-13,2.17161023787773E-15,
1.)) ;
#45268 = DIRECTION('',(1.,2.90739654573677E-15,-1.48506207331423E-13)) ;
#45269 = DIRECTION('center_axis',(1.,0.,6.31373210429172E-30)) ;
#45270 = DIRECTION('ref_axis',(-1.37109652768972E-44,-1.,2.17161023787773E-15)) ;
#45271 = DIRECTION('center_axis',(-1.42108547152028E-13,-2.17161023787773E-15,
-1.)) ;
#45272 = DIRECTION('ref_axis',(-1.,0.,1.51582450295488E-13)) ;
#45273 = DIRECTION('center_axis',(-0.408248290463958,-0.408248290463844,-0.816496580927688)) ;
#45274 = DIRECTION('ref_axis',(-0.577350269189815,-0.577350269189474,0.577350269189588)) ;
#45275 = DIRECTION('center_axis',(-0.816496580927726,-0.408248290463977,0.408248290463749)) ;
#45276 = DIRECTION('ref_axis',(0.577350269189588,-0.577350269189702,0.577350269189588)) ;
#45277 = DIRECTION('center_axis',(0.408248290463806,0.408248290463692,-0.81649658092784)) ;
#45278 = DIRECTION('ref_axis',(-0.577350269189777,-0.57735026918955,-0.57735026918955)) ;
#45279 = DIRECTION('center_axis',(-0.408248290463711,-0.816496580927764,0.408248290463939)) ;
#45280 = DIRECTION('ref_axis',(0.57735026918955,-0.57735026918955,-0.577350269189777)) ;
#45281 = DIRECTION('center_axis',(1.42108547152028E-13,2.17161023787773E-15,
1.)) ;
#45282 = DIRECTION('ref_axis',(1.,0.,-1.515824502955E-13)) ;
#45283 = DIRECTION('center_axis',(-1.42108547152028E-13,-2.17161023787773E-15,
-1.)) ;
#45284 = DIRECTION('ref_axis',(-1.,0.,1.51582450295488E-13)) ;
#45285 = DIRECTION('center_axis',(2.9073965457371E-15,-1.,2.17161023787728E-15)) ;
#45286 = DIRECTION('ref_axis',(0.,0.,-1.)) ;
#45287 = DIRECTION('center_axis',(-2.9073965457371E-15,1.,-2.17161023787728E-15)) ;
#45288 = DIRECTION('ref_axis',(-1.49322507795023E-13,-2.17161023787771E-15,
-1.)) ;
#45289 = DIRECTION('center_axis',(-1.,-2.9073965457371E-15,9.03687443371611E-30)) ;
#45290 = DIRECTION('ref_axis',(0.,3.108235939458E-15,1.)) ;
#45291 = DIRECTION('center_axis',(2.9073965457371E-15,-1.,2.17161023787728E-15)) ;
#45292 = DIRECTION('ref_axis',(-1.49322507795023E-13,-2.17161023787771E-15,
-1.)) ;
#45293 = DIRECTION('center_axis',(2.90739654573709E-15,-1.,2.17161023787725E-15)) ;
#45294 = DIRECTION('ref_axis',(-1.48506207331423E-13,-2.17161023787768E-15,
-1.)) ;
#45295 = DIRECTION('center_axis',(2.90739654573709E-15,-1.,2.17161023787725E-15)) ;
#45296 = DIRECTION('ref_axis',(-9.93363673616178E-14,-2.17161023787754E-15,
-1.)) ;
#45297 = DIRECTION('center_axis',(-2.9073965457371E-15,1.,-2.17161023787728E-15)) ;
#45298 = DIRECTION('ref_axis',(-1.58279632150758E-13,-2.17161023787774E-15,
-1.)) ;
#45299 = DIRECTION('center_axis',(-2.90739654573709E-15,1.,-2.17161023787725E-15)) ;
#45300 = DIRECTION('ref_axis',(-9.93363673616178E-14,-2.17161023787754E-15,
-1.)) ;
#45301 = DIRECTION('center_axis',(-2.90739654573709E-15,1.,-2.17161023787725E-15)) ;
#45302 = DIRECTION('ref_axis',(-9.93363673616178E-14,-2.17161023787754E-15,
-1.)) ;
#45303 = DIRECTION('',(2.9073965457371E-15,-1.,2.17161023787728E-15)) ;
#45304 = DIRECTION('center_axis',(-2.90739654573709E-15,1.,-2.17161023787725E-15)) ;
#45305 = DIRECTION('ref_axis',(0.,0.,1.)) ;
#45306 = DIRECTION('center_axis',(1.,2.90739654573709E-15,-8.30985315988538E-30)) ;
#45307 = DIRECTION('ref_axis',(0.,-2.85817673274378E-15,-1.)) ;
#45308 = DIRECTION('center_axis',(2.9073965457371E-15,-1.,2.17161023787728E-15)) ;
#45309 = DIRECTION('ref_axis',(1.48422940604576E-13,2.17161023787771E-15,
1.)) ;
#45310 = DIRECTION('',(1.,-1.48506207331422E-13,4.80539550796049E-28)) ;
#45311 = DIRECTION('',(1.48506207331422E-13,1.,-2.90739654573717E-15)) ;
#45312 = DIRECTION('',(1.,-1.48506207331422E-13,4.80539550796049E-28)) ;
#45313 = DIRECTION('',(1.48506207331422E-13,1.,-2.90739654573717E-15)) ;
#45314 = DIRECTION('',(1.,-1.48506207331422E-13,4.80539550796049E-28)) ;
#45315 = DIRECTION('',(1.48506207331422E-13,1.,-2.90739654573717E-15)) ;
#45316 = DIRECTION('',(1.,-1.48506207331422E-13,4.80539550796049E-28)) ;
#45317 = DIRECTION('',(1.48506207331422E-13,1.,-2.90739654573717E-15)) ;
#45318 = DIRECTION('',(1.,-1.48506207331422E-13,4.80539550796049E-28)) ;
#45319 = DIRECTION('',(1.48506207331422E-13,1.,-2.90739654573717E-15)) ;
#45320 = DIRECTION('',(1.,-1.48506207331422E-13,4.80539550796049E-28)) ;
#45321 = DIRECTION('',(1.48506207331422E-13,1.,-2.90739654573717E-15)) ;
#45322 = DIRECTION('',(1.,-1.48506207331422E-13,4.80539550796049E-28)) ;
#45323 = DIRECTION('',(1.48506207331422E-13,1.,-2.90739654573717E-15)) ;
#45324 = DIRECTION('',(1.,-1.48506207331422E-13,4.80539550796049E-28)) ;
#45325 = DIRECTION('',(1.48506207331422E-13,1.,-2.90739654573717E-15)) ;
#45326 = DIRECTION('',(1.,-1.48506207331422E-13,4.80539550796049E-28)) ;
#45327 = DIRECTION('',(1.48506207331422E-13,1.,-2.90739654573717E-15)) ;
#45328 = DIRECTION('axis',(0.,0.,1.)) ;
#45329 = DIRECTION('refdir',(1.,0.,0.)) ;
#45330 = DIRECTION('axis',(0.,0.,1.)) ;
#45331 = DIRECTION('refdir',(1.,0.,0.)) ;
#45332 = DIRECTION('center_axis',(7.71011961179131E-14,1.,-8.96434510032606E-14)) ;
#45333 = DIRECTION('ref_axis',(-0.597896819887404,1.1795433654226E-13,0.801573073879437)) ;
#45334 = DIRECTION('center_axis',(-5.25111655993446E-9,-1.,5.25108985668226E-9)) ;
#45335 = DIRECTION('ref_axis',(-0.707106793325191,7.42618137461088E-9,0.707106769047904)) ;
#45336 = DIRECTION('center_axis',(-1.73807139389439E-14,1.,1.64443783657369E-14)) ;
#45337 = DIRECTION('ref_axis',(0.5978968198874,2.35732445061274E-14,-0.80157307387944)) ;
#45338 = DIRECTION('center_axis',(2.0085626353944E-13,-1.,-1.93736401307529E-13)) ;
#45339 = DIRECTION('ref_axis',(0.728572555974573,2.79041719628071E-13,-0.684968634815257)) ;
#45340 = DIRECTION('center_axis',(2.7392192633255E-15,1.,-3.67555483654062E-15)) ;
#45341 = DIRECTION('ref_axis',(-0.707106796087576,4.5359302518428E-15,0.707106766285518)) ;
#45342 = DIRECTION('center_axis',(5.25109179432767E-9,-1.,-5.25111813730416E-9)) ;
#45343 = DIRECTION('ref_axis',(-0.728572559766829,-7.42265259074552E-9,0.684968630781593)) ;
#45344 = DIRECTION('center_axis',(1.35274044298125E-14,1.,5.65619335361478E-15)) ;
#45345 = DIRECTION('ref_axis',(-0.801573073879436,1.42250231692097E-14,-0.597896819887406)) ;
#45346 = DIRECTION('center_axis',(-4.03746661613741E-13,-1.,-3.97331887513712E-13)) ;
#45347 = DIRECTION('ref_axis',(-0.684968634815258,5.66038908472849E-13,-0.728572555974572)) ;
#45348 = DIRECTION('center_axis',(2.7392192633255E-15,1.,-3.67555483654062E-15)) ;
#45349 = DIRECTION('ref_axis',(0.801573073879438,1.91814315580942E-18,0.597896819887403)) ;
#45350 = DIRECTION('center_axis',(-2.06334705469751E-13,-1.,-1.9373640471103E-13)) ;
#45351 = DIRECTION('ref_axis',(0.684968634815263,-2.82483829086263E-13,0.728572555974568)) ;
#45352 = DIRECTION('center_axis',(-2.7392192633255E-15,-1.,3.67555483654062E-15)) ;
#45353 = DIRECTION('ref_axis',(-2.02401438901654E-13,-3.67555483654007E-15,
-1.)) ;
#45354 = DIRECTION('center_axis',(-2.7392192633255E-15,-1.,3.67555483654062E-15)) ;
#45355 = DIRECTION('ref_axis',(-0.581108581115083,-1.3994784034356E-15,-0.813826036050958)) ;
#45356 = DIRECTION('',(-2.7392192633255E-15,-1.,3.67555483654062E-15)) ;
#45357 = DIRECTION('center_axis',(-2.17161023787667E-15,-1.,3.15364308176334E-15)) ;
#45358 = DIRECTION('ref_axis',(-0.581108581115083,-1.30457550428349E-15,-0.813826036050958)) ;
#45359 = DIRECTION('center_axis',(2.7392192633255E-15,1.,-3.67555483654062E-15)) ;
#45360 = DIRECTION('ref_axis',(2.02476924116013E-13,3.67555483654007E-15,
1.)) ;
#45361 = DIRECTION('',(1.,-2.73921926332625E-15,-2.02476924116013E-13)) ;
#45362 = DIRECTION('',(2.02476924116013E-13,3.67555483654007E-15,1.)) ;
#45363 = DIRECTION('center_axis',(2.73921926332383E-15,1.,-5.60637748192944E-15)) ;
#45364 = DIRECTION('ref_axis',(1.,-2.73921926337039E-15,-8.30565686121179E-12)) ;
#45365 = DIRECTION('',(-2.02476924116013E-13,-3.67555483654007E-15,-1.)) ;
#45366 = DIRECTION('',(1.,-2.73921926332624E-15,-1.99806052959965E-13)) ;
#45367 = DIRECTION('',(-2.02476924116013E-13,-3.67555483654007E-15,-1.)) ;
#45368 = DIRECTION('',(1.,-2.73921926332625E-15,-2.02476924116013E-13)) ;
#45369 = DIRECTION('center_axis',(1.77380794165008E-15,1.,-4.64096615924138E-15)) ;
#45370 = DIRECTION('ref_axis',(-8.30613956687314E-12,-4.64096615922665E-15,
-1.)) ;
#45371 = DIRECTION('',(-1.,2.73921926332625E-15,2.02476924116013E-13)) ;
#45372 = DIRECTION('',(-2.02476924116013E-13,-3.67555483654007E-15,-1.)) ;
#45373 = DIRECTION('',(-1.,2.73921926332625E-15,2.02476924116013E-13)) ;
#45374 = DIRECTION('',(-2.02476924116013E-13,-3.67555483654007E-15,-1.)) ;
#45375 = DIRECTION('center_axis',(2.73921926332384E-15,1.,-5.60637748192943E-15)) ;
#45376 = DIRECTION('ref_axis',(-1.,2.73921926337041E-15,8.30662227253449E-12)) ;
#45377 = DIRECTION('',(2.02476924116013E-13,3.67555483654007E-15,1.)) ;
#45378 = DIRECTION('',(-1.,2.73921926332625E-15,2.02476924116013E-13)) ;
#45379 = DIRECTION('',(2.02476924116013E-13,3.67555483654007E-15,1.)) ;
#45380 = DIRECTION('',(-1.,2.73921926332625E-15,2.02476924116013E-13)) ;
#45381 = DIRECTION('center_axis',(-1.12242602745208E-15,1.,-3.67555483653727E-15)) ;
#45382 = DIRECTION('ref_axis',(8.31724179708421E-12,3.67555483654661E-15,
1.)) ;
#45383 = DIRECTION('',(1.,-2.73921926332625E-15,-2.02476924116013E-13)) ;
#45384 = DIRECTION('',(2.02476924116013E-13,3.67555483654007E-15,1.)) ;
#45385 = DIRECTION('center_axis',(2.7392192633255E-15,1.,-3.67555483654062E-15)) ;
#45386 = DIRECTION('ref_axis',(2.02476924116013E-13,3.67555483654007E-15,
1.)) ;
#45387 = DIRECTION('',(-1.,2.73921926666159E-15,9.07642502817205E-10)) ;
#45388 = DIRECTION('',(2.02476924116013E-13,3.67555483654007E-15,1.)) ;
#45389 = DIRECTION('',(1.,-2.7392192599909E-15,9.07238034699055E-10)) ;
#45390 = DIRECTION('center_axis',(-2.7392192633255E-15,-1.,3.67555483654062E-15)) ;
#45391 = DIRECTION('ref_axis',(3.52629806639308E-11,-3.67555483663721E-15,
-1.)) ;
#45392 = DIRECTION('center_axis',(2.7392192633255E-15,1.,-3.67555483654062E-15)) ;
#45393 = DIRECTION('ref_axis',(2.02476924116013E-13,3.67555483654007E-15,
1.)) ;
#45394 = DIRECTION('',(-2.02476924116013E-13,-3.67555483654007E-15,-1.)) ;
#45395 = DIRECTION('',(-1.,2.7392192599909E-15,-9.0723803469906E-10)) ;
#45396 = DIRECTION('center_axis',(-2.12242869659861E-15,-1.,4.29234540331102E-15)) ;
#45397 = DIRECTION('ref_axis',(-3.52635974544975E-11,4.29234540338586E-15,
1.)) ;
#45398 = DIRECTION('',(1.,-2.73921926666159E-15,-9.07642017093344E-10)) ;
#45399 = DIRECTION('center_axis',(2.7392192633255E-15,1.,-3.67555483654062E-15)) ;
#45400 = DIRECTION('ref_axis',(2.02476924116013E-13,3.67555483654007E-15,
1.)) ;
#45401 = DIRECTION('',(9.07642017094632E-10,3.67555483405439E-15,1.)) ;
#45402 = DIRECTION('',(1.,-2.73921926332625E-15,-2.02476924116013E-13)) ;
#45403 = DIRECTION('',(9.07238034699055E-10,-3.67555483902575E-15,-1.)) ;
#45404 = DIRECTION('center_axis',(-2.739219263369E-15,-1.,4.90913597003791E-15)) ;
#45405 = DIRECTION('ref_axis',(-1.,2.73921926319589E-15,-3.5262363873364E-11)) ;
#45406 = DIRECTION('center_axis',(2.7392192633255E-15,1.,-3.67555483654062E-15)) ;
#45407 = DIRECTION('ref_axis',(2.02476924116013E-13,3.67555483654007E-15,
1.)) ;
#45408 = DIRECTION('',(-1.,2.73921926332625E-15,2.02476924116013E-13)) ;
#45409 = DIRECTION('',(-9.0723803469906E-10,3.67555483902575E-15,1.)) ;
#45410 = DIRECTION('center_axis',(-2.7392192633255E-15,-1.,3.67555483654062E-15)) ;
#45411 = DIRECTION('ref_axis',(1.,-2.73921926319589E-15,3.52629806639308E-11)) ;
#45412 = DIRECTION('',(-9.07642988539774E-10,-3.67555483405439E-15,-1.)) ;
#45413 = DIRECTION('center_axis',(6.99883249118274E-11,1.,4.68598587806925E-10)) ;
#45414 = DIRECTION('ref_axis',(-2.06578141065567E-13,4.68605298162149E-10,
-1.)) ;
#45415 = DIRECTION('center_axis',(-7.77996834011603E-11,2.60066914135082E-11,
1.)) ;
#45416 = DIRECTION('ref_axis',(-1.,1.5214735684773E-8,-7.77996837968452E-11)) ;
#45417 = DIRECTION('center_axis',(-2.86196449187501E-12,2.73622147742173E-12,
-1.)) ;
#45418 = DIRECTION('ref_axis',(1.,1.38251899120395E-8,-2.86196445404623E-12)) ;
#45419 = DIRECTION('center_axis',(2.7392192633255E-15,1.,-3.67555483654062E-15)) ;
#45420 = DIRECTION('ref_axis',(-1.,2.7392192634357E-15,2.99814340021243E-11)) ;
#45421 = DIRECTION('center_axis',(-2.02476924116013E-13,-3.67555483654007E-15,
-1.)) ;
#45422 = DIRECTION('ref_axis',(-0.707106781186542,0.707106781186553,1.40573796326685E-13)) ;
#45423 = DIRECTION('',(2.02476924116013E-13,3.67555483654007E-15,1.)) ;
#45424 = DIRECTION('center_axis',(2.73952003670914E-13,-6.77995247183616E-14,
1.)) ;
#45425 = DIRECTION('ref_axis',(-1.,-2.6866728060012E-14,2.73952003670912E-13)) ;
#45426 = DIRECTION('center_axis',(2.02476924116013E-13,3.67555483654007E-15,
1.)) ;
#45427 = DIRECTION('ref_axis',(0.707106781186549,0.707106781186546,-1.45771815825768E-13)) ;
#45428 = DIRECTION('center_axis',(2.02476924116013E-13,3.67555483654007E-15,
1.)) ;
#45429 = DIRECTION('ref_axis',(-2.40911704984497E-14,1.,-3.67555483653519E-15)) ;
#45430 = DIRECTION('',(-2.02476924116013E-13,-3.67555483654007E-15,-1.)) ;
#45431 = DIRECTION('center_axis',(4.68612409773722E-10,1.,-6.99878726045723E-11)) ;
#45432 = DIRECTION('ref_axis',(-2.06578141065567E-13,-6.99783452859607E-11,
-1.)) ;
#45433 = DIRECTION('center_axis',(-1.,2.60157134512408E-11,-2.57836941530287E-11)) ;
#45434 = DIRECTION('ref_axis',(2.6015713512402E-11,1.,-2.37208950382905E-9)) ;
#45435 = DIRECTION('center_axis',(-1.,2.8805387413756E-12,2.79437612800868E-12)) ;
#45436 = DIRECTION('ref_axis',(-2.79437608818469E-12,1.38251889757039E-8,
-1.)) ;
#45437 = DIRECTION('center_axis',(5.18773214108251E-16,1.,-3.67555483650711E-15)) ;
#45438 = DIRECTION('ref_axis',(2.99814340021243E-11,3.67555483649156E-15,
1.)) ;
#45439 = DIRECTION('center_axis',(-1.,2.73921926332625E-15,2.02476924116013E-13)) ;
#45440 = DIRECTION('ref_axis',(1.4510972659248E-13,0.707106781186553,0.707106781186542)) ;
#45441 = DIRECTION('',(1.,-2.73921926332625E-15,-2.02476924116013E-13)) ;
#45442 = DIRECTION('center_axis',(1.,-7.42142988182295E-14,-2.73952003670916E-13)) ;
#45443 = DIRECTION('ref_axis',(2.73952003670915E-13,-1.11274188251291E-14,
1.)) ;
#45444 = DIRECTION('center_axis',(1.,-2.77538307019574E-15,-2.0249012323252E-13)) ;
#45445 = DIRECTION('ref_axis',(-1.4121964707169E-13,0.707106781186544,-0.707106781186551)) ;
#45446 = DIRECTION('center_axis',(1.,-1.2782060848441E-13,-7.73955348949296E-14)) ;
#45447 = DIRECTION('ref_axis',(1.2782060848441E-13,1.,1.87556028655978E-15)) ;
#45448 = DIRECTION('',(-1.,2.73921926332625E-15,2.02476924116013E-13)) ;
#45449 = DIRECTION('center_axis',(-6.99814578304714E-11,1.,-4.68613346109296E-10)) ;
#45450 = DIRECTION('ref_axis',(4.44143003290968E-12,4.68622513007238E-10,
1.)) ;
#45451 = DIRECTION('center_axis',(7.77280223498716E-11,2.59905918894472E-11,
-1.)) ;
#45452 = DIRECTION('ref_axis',(1.,1.52147302063345E-8,7.77280227453114E-11)) ;
#45453 = DIRECTION('center_axis',(2.94237395572288E-12,2.66316312194452E-12,
1.)) ;
#45454 = DIRECTION('ref_axis',(-1.,1.38252397993977E-8,2.94237391890401E-12)) ;
#45455 = DIRECTION('center_axis',(2.739219263359E-15,1.,-1.45510878732336E-15)) ;
#45456 = DIRECTION('ref_axis',(1.,-2.73921926340261E-15,-2.9971997106415E-11)) ;
#45457 = DIRECTION('center_axis',(2.02476924116013E-13,3.67555483654007E-15,
1.)) ;
#45458 = DIRECTION('ref_axis',(0.707106781186548,0.707106781186547,-1.45771815825767E-13)) ;
#45459 = DIRECTION('',(-2.02476924116013E-13,-3.67555483654007E-15,-1.)) ;
#45460 = DIRECTION('center_axis',(-2.73952003670918E-13,-7.51506343914451E-14,
-1.)) ;
#45461 = DIRECTION('ref_axis',(1.,-2.73921926332633E-15,-2.73952003670918E-13)) ;
#45462 = DIRECTION('center_axis',(-2.02476924116013E-13,-3.67555483654007E-15,
-1.)) ;
#45463 = DIRECTION('ref_axis',(-0.707106781186546,0.707106781186549,1.40573796326686E-13)) ;
#45464 = DIRECTION('center_axis',(-2.02476924116013E-13,-3.67555483654007E-15,
-1.)) ;
#45465 = DIRECTION('ref_axis',(-1.94652412291771E-14,1.,-3.67555483653613E-15)) ;
#45466 = DIRECTION('',(2.02476924116013E-13,3.67555483654007E-15,1.)) ;
#45467 = DIRECTION('center_axis',(1.,-2.73921926332625E-15,-2.02476924116013E-13)) ;
#45468 = DIRECTION('ref_axis',(-2.73921926332551E-15,-1.,3.67555483654063E-15)) ;
#45469 = DIRECTION('',(-2.02476924116013E-13,-3.67555483654007E-15,-1.)) ;
#45470 = DIRECTION('',(-2.7392192633255E-15,-1.,3.67555483654062E-15)) ;
#45471 = DIRECTION('',(-2.7392192633255E-15,-1.,3.67555483654062E-15)) ;
#45472 = DIRECTION('center_axis',(-1.,2.73921926332625E-15,2.02476924116013E-13)) ;
#45473 = DIRECTION('ref_axis',(2.73921926332551E-15,1.,-3.67555483654063E-15)) ;
#45474 = DIRECTION('',(2.02476924116013E-13,3.67555483654007E-15,1.)) ;
#45475 = DIRECTION('',(-2.73921924526551E-15,-1.,8.91989933532196E-11)) ;
#45476 = DIRECTION('',(-2.7392192633255E-15,-1.,3.67555483654062E-15)) ;
#45477 = DIRECTION('center_axis',(-2.7392192633255E-15,-1.,3.67555483654062E-15)) ;
#45478 = DIRECTION('ref_axis',(1.,-2.73921926332624E-15,-2.02476924116013E-13)) ;
#45479 = DIRECTION('center_axis',(-2.7392192633255E-15,-1.,3.67555483654062E-15)) ;
#45480 = DIRECTION('ref_axis',(-1.,2.73921926332625E-15,2.03032035628326E-13)) ;
#45481 = DIRECTION('center_axis',(-2.02476924116013E-13,-3.67555483654007E-15,
-1.)) ;
#45482 = DIRECTION('ref_axis',(-0.707106781186547,-0.707106781186548,1.45771815825767E-13)) ;
#45483 = DIRECTION('center_axis',(-1.73057417312571E-11,1.71934002942205E-11,
-1.)) ;
#45484 = DIRECTION('ref_axis',(-1.,1.54909559440142E-8,1.73057419975993E-11)) ;
#45485 = DIRECTION('center_axis',(1.22067459616746E-13,-7.67339096627288E-14,
1.)) ;
#45486 = DIRECTION('ref_axis',(4.19967464056558E-15,-1.,-7.67339096627293E-14)) ;
#45487 = DIRECTION('center_axis',(2.0247579896626E-13,3.65514229881304E-15,
1.)) ;
#45488 = DIRECTION('ref_axis',(0.707106781186545,-0.70710678118655,-1.40587434569514E-13)) ;
#45489 = DIRECTION('center_axis',(2.02476924116013E-13,3.67555483654007E-15,
1.)) ;
#45490 = DIRECTION('ref_axis',(1.,1.94652412291775E-14,-2.02476924116013E-13)) ;
#45491 = DIRECTION('center_axis',(2.45592326533471E-10,-7.36846277275853E-11,
1.)) ;
#45492 = DIRECTION('ref_axis',(1.,1.70479272859721E-8,-2.45592325277301E-10)) ;
#45493 = DIRECTION('center_axis',(-6.68032841410509E-11,-1.,4.47277340551685E-10)) ;
#45494 = DIRECTION('ref_axis',(1.79034390085963E-13,4.47295044331018E-10,
1.)) ;
#45495 = DIRECTION('center_axis',(-2.02476924116013E-13,-3.67555483654007E-15,
-1.)) ;
#45496 = DIRECTION('ref_axis',(-2.7392192633255E-15,-1.,3.67555483654062E-15)) ;
#45497 = DIRECTION('',(-2.7392192633255E-15,-1.,3.67555483654062E-15)) ;
#45498 = DIRECTION('',(-1.,2.73921926332625E-15,2.02476924116013E-13)) ;
#45499 = DIRECTION('',(-2.7392192633255E-15,-1.,3.67555483654062E-15)) ;
#45500 = DIRECTION('',(-1.,2.73921926332625E-15,2.02476924116013E-13)) ;
#45501 = DIRECTION('center_axis',(2.02476924116013E-13,3.67555483654007E-15,
1.)) ;
#45502 = DIRECTION('ref_axis',(2.7392192633255E-15,1.,-3.67555483654062E-15)) ;
#45503 = DIRECTION('',(-2.7392192633255E-15,-1.,3.67555483654062E-15)) ;
#45504 = DIRECTION('',(1.,-2.73921926332625E-15,-2.02476924116013E-13)) ;
#45505 = DIRECTION('',(1.70194450455769E-10,-1.,3.67555480207962E-15)) ;
#45506 = DIRECTION('',(1.,-2.73921926332625E-15,-2.02476924116013E-13)) ;
#45507 = DIRECTION('center_axis',(4.47280390523803E-10,-1.,6.68024460996793E-11)) ;
#45508 = DIRECTION('ref_axis',(1.79034390085955E-13,6.68245860995827E-11,
1.)) ;
#45509 = DIRECTION('center_axis',(-1.,-7.98040177460166E-11,7.999583231198E-11)) ;
#45510 = DIRECTION('ref_axis',(7.98040175334014E-11,-1.,-2.65782865320679E-9)) ;
#45511 = DIRECTION('center_axis',(-1.,1.72095703729976E-11,1.73959065004325E-11)) ;
#45512 = DIRECTION('ref_axis',(1.7395906767025E-11,1.54909457781191E-8,1.)) ;
#45513 = DIRECTION('center_axis',(-2.7392192633255E-15,-1.,3.67555483654062E-15)) ;
#45514 = DIRECTION('ref_axis',(2.03032035628326E-13,3.67555483654006E-15,
1.)) ;
#45515 = DIRECTION('center_axis',(-1.,2.73921926332625E-15,2.02476924116013E-13)) ;
#45516 = DIRECTION('ref_axis',(1.41235885559973E-13,-0.707106781186544,0.707106781186551)) ;
#45517 = DIRECTION('center_axis',(1.,-2.95423740964165E-14,-1.75673769282923E-13)) ;
#45518 = DIRECTION('ref_axis',(-2.95423740964141E-14,-1.,1.33900063020159E-14)) ;
#45519 = DIRECTION('center_axis',(1.,-2.73921926332625E-15,-2.02476924116013E-13)) ;
#45520 = DIRECTION('ref_axis',(-1.45109726592481E-13,-0.707106781186552,-0.707106781186543)) ;
#45521 = DIRECTION('center_axis',(1.,-2.73921926332625E-15,-2.02476924116013E-13)) ;
#45522 = DIRECTION('ref_axis',(-2.02476924116013E-13,-3.67555483654007E-15,
-1.)) ;
#45523 = DIRECTION('center_axis',(-1.,2.73921926332625E-15,2.02476924116013E-13)) ;
#45524 = DIRECTION('ref_axis',(2.73921926332551E-15,1.,-3.67555483654063E-15)) ;
#45525 = DIRECTION('',(2.02476924116013E-13,3.67555483654007E-15,1.)) ;
#45526 = DIRECTION('',(-2.7392192633255E-15,-1.,3.67555483654062E-15)) ;
#45527 = DIRECTION('',(-2.7392192633255E-15,-1.,3.67555483654062E-15)) ;
#45528 = DIRECTION('center_axis',(1.,-2.73921926332625E-15,-2.02476924116013E-13)) ;
#45529 = DIRECTION('ref_axis',(-2.73921926332551E-15,-1.,3.67555483654063E-15)) ;
#45530 = DIRECTION('',(-2.02476924116013E-13,-3.67555483654007E-15,-1.)) ;
#45531 = DIRECTION('',(-2.7392192813855E-15,-1.,-8.91916422435465E-11)) ;
#45532 = DIRECTION('',(-2.7392192633255E-15,-1.,3.67555483654062E-15)) ;
#45533 = DIRECTION('center_axis',(-2.7392192633255E-15,-1.,3.67555483654062E-15)) ;
#45534 = DIRECTION('ref_axis',(-1.,2.73921926332624E-15,2.02476924116013E-13)) ;
#45535 = DIRECTION('center_axis',(-2.7392192633255E-15,-1.,3.67555483654062E-15)) ;
#45536 = DIRECTION('ref_axis',(1.,-2.73921926332625E-15,-2.04142258652951E-13)) ;
#45537 = DIRECTION('center_axis',(6.67961373153174E-11,-1.,-4.47275108033656E-10)) ;
#45538 = DIRECTION('ref_axis',(5.41579030010014E-12,4.47272665032237E-10,
-1.)) ;
#45539 = DIRECTION('center_axis',(8.60965078876547E-11,-8.59037569861192E-11,
1.)) ;
#45540 = DIRECTION('ref_axis',(-2.65783506798089E-9,-1.,-8.59037567572889E-11)) ;
#45541 = DIRECTION('center_axis',(1.73959065004326E-11,1.72105067085707E-11,
1.)) ;
#45542 = DIRECTION('ref_axis',(1.,1.5490939363345E-8,-1.73959067670395E-11)) ;
#45543 = DIRECTION('center_axis',(2.02476924116013E-13,3.67555483654007E-15,
1.)) ;
#45544 = DIRECTION('ref_axis',(0.707106781186546,-0.707106781186549,-1.40573796326686E-13)) ;
#45545 = DIRECTION('center_axis',(-1.75673769282924E-13,-3.04787096696305E-14,
-1.)) ;
#45546 = DIRECTION('ref_axis',(6.97523220214981E-15,-1.,3.04787096696293E-14)) ;
#45547 = DIRECTION('center_axis',(-2.02476924116013E-13,-3.67555483654007E-15,
-1.)) ;
#45548 = DIRECTION('ref_axis',(-0.707106781186547,-0.707106781186548,1.45771815825767E-13)) ;
#45549 = DIRECTION('center_axis',(-2.02476924116013E-13,-3.67555483654007E-15,
-1.)) ;
#45550 = DIRECTION('ref_axis',(-1.,-1.94652412291768E-14,2.02476924116013E-13)) ;
#45551 = DIRECTION('center_axis',(2.02476924116013E-13,3.67555483654007E-15,
1.)) ;
#45552 = DIRECTION('ref_axis',(2.7392192633255E-15,1.,-3.67555483654062E-15)) ;
#45553 = DIRECTION('',(1.,-2.73921926332625E-15,-2.02476924116013E-13)) ;
#45554 = DIRECTION('',(-2.7392192633255E-15,-1.,3.67555483654062E-15)) ;
#45555 = DIRECTION('',(-2.7392192633255E-15,-1.,3.67555483654062E-15)) ;
#45556 = DIRECTION('center_axis',(-2.02476924116013E-13,-3.67555483654007E-15,
-1.)) ;
#45557 = DIRECTION('ref_axis',(-2.7392192633255E-15,-1.,3.67555483654062E-15)) ;
#45558 = DIRECTION('',(-1.,2.73921926332625E-15,2.02476924116013E-13)) ;
#45559 = DIRECTION('',(-8.91980570176463E-11,-1.,3.67555485460062E-15)) ;
#45560 = DIRECTION('',(-2.7392192633255E-15,-1.,3.67555483654062E-15)) ;
#45561 = DIRECTION('center_axis',(-2.7392192633255E-15,-1.,3.67555483654062E-15)) ;
#45562 = DIRECTION('ref_axis',(2.02476924116013E-13,3.67555483654007E-15,
1.)) ;
#45563 = DIRECTION('center_axis',(-2.7392192633255E-15,-1.,3.67555483654062E-15)) ;
#45564 = DIRECTION('ref_axis',(-2.03032035628326E-13,-3.67555483654006E-15,
-1.)) ;
#45565 = DIRECTION('center_axis',(1.,-2.73921926332625E-15,-2.02476924116013E-13)) ;
#45566 = DIRECTION('ref_axis',(-1.45109726592481E-13,-0.707106781186552,-0.707106781186543)) ;
#45567 = DIRECTION('center_axis',(1.,1.71943366297936E-11,-1.73057417312572E-11)) ;
#45568 = DIRECTION('ref_axis',(-1.73057419976138E-11,1.54909495292401E-8,
-1.)) ;
#45569 = DIRECTION('center_axis',(-1.,2.73921926332625E-15,2.02476924116013E-13)) ;
#45570 = DIRECTION('ref_axis',(-2.7392192633241E-15,-1.,1.06144487404478E-14)) ;
#45571 = DIRECTION('center_axis',(-1.,2.71880672559922E-15,2.0247579896626E-13)) ;
#45572 = DIRECTION('ref_axis',(1.412495238028E-13,-0.707106781186546,0.707106781186549)) ;
#45573 = DIRECTION('center_axis',(-1.,2.73921926332625E-15,2.02476924116013E-13)) ;
#45574 = DIRECTION('ref_axis',(2.02476924116013E-13,1.47777850827919E-14,
1.)) ;
#45575 = DIRECTION('center_axis',(-1.,-7.3685564063157E-11,2.45592326533472E-10)) ;
#45576 = DIRECTION('ref_axis',(2.45592325277285E-10,1.70479337007462E-8,1.)) ;
#45577 = DIRECTION('center_axis',(-4.4727640421611E-10,-1.,-6.67968693669511E-11)) ;
#45578 = DIRECTION('ref_axis',(1.79034390085963E-13,-6.67798275020642E-11,
1.)) ;
#45579 = DIRECTION('center_axis',(-2.7392192633255E-15,-1.,3.67555483654062E-15)) ;
#45580 = DIRECTION('ref_axis',(-2.02476924116013E-13,-3.67555483654007E-15,
-1.)) ;
#45581 = DIRECTION('center_axis',(4.95966531254277E-15,1.,-3.67555483657413E-15)) ;
#45582 = DIRECTION('ref_axis',(-2.9971997106415E-11,-3.67555483642548E-15,
-1.)) ;
#45583 = DIRECTION('center_axis',(-4.68606931335196E-10,1.,6.99805214948982E-11)) ;
#45584 = DIRECTION('ref_axis',(-2.06578141065567E-13,6.99783452859607E-11,
-1.)) ;
#45585 = DIRECTION('center_axis',(1.,2.60638413228166E-11,2.57300878437945E-11)) ;
#45586 = DIRECTION('ref_axis',(-2.60638413838492E-11,1.,2.3720331178697E-9)) ;
#45587 = DIRECTION('center_axis',(1.,2.66568273286117E-12,-2.93343957085108E-12)) ;
#45588 = DIRECTION('ref_axis',(2.93343953399749E-12,1.38251963268136E-8,1.)) ;
#45589 = DIRECTION('center_axis',(1.,-2.70940101215817E-15,-2.02507881810474E-13)) ;
#45590 = DIRECTION('ref_axis',(-1.41278860643259E-13,0.70710678118655,-0.707106781186545)) ;
#45591 = DIRECTION('center_axis',(-1.,-5.08670904028541E-14,2.56083233782194E-13)) ;
#45592 = DIRECTION('ref_axis',(-2.56083233782195E-13,2.5930392486797E-14,
-1.)) ;
#45593 = DIRECTION('center_axis',(-1.,2.73921926332625E-15,2.02476924116013E-13)) ;
#45594 = DIRECTION('ref_axis',(1.45109726592481E-13,0.707106781186551,0.707106781186544)) ;
#45595 = DIRECTION('center_axis',(-1.,2.73921926332625E-15,2.02476924116013E-13)) ;
#45596 = DIRECTION('ref_axis',(2.73921926332007E-15,1.,-3.05059445983158E-14)) ;
#45597 = DIRECTION('center_axis',(-2.7392192633255E-15,-1.,3.67555483654062E-15)) ;
#45598 = DIRECTION('ref_axis',(-2.02476924116013E-13,-3.67555483654007E-15,
-1.)) ;
#45599 = DIRECTION('center_axis',(-2.7392192633255E-15,-1.,3.67555483654062E-15)) ;
#45600 = DIRECTION('ref_axis',(-2.02476924116013E-13,-3.67555483654007E-15,
-1.)) ;
#45601 = DIRECTION('',(1.,-2.73921926332625E-15,-2.0199120154274E-13)) ;
#45602 = DIRECTION('',(2.02476924116013E-13,3.67555483654007E-15,1.)) ;
#45603 = DIRECTION('',(-1.,2.73921926332625E-15,2.0199120154274E-13)) ;
#45604 = DIRECTION('center_axis',(-2.02476924116013E-13,-3.67555483654007E-15,
-1.)) ;
#45605 = DIRECTION('ref_axis',(-2.7392192633255E-15,-1.,3.67555483654062E-15)) ;
#45606 = DIRECTION('',(1.,-2.73921926332625E-15,-2.02476924116013E-13)) ;
#45607 = DIRECTION('',(8.87904497774877E-12,-1.,3.67555483474227E-15)) ;
#45608 = DIRECTION('',(1.,-2.18410775101367E-15,-2.02546313055052E-13)) ;
#45609 = DIRECTION('center_axis',(2.02476924116013E-13,3.67555483654007E-15,
1.)) ;
#45610 = DIRECTION('ref_axis',(2.7392192633255E-15,1.,-3.67555483654062E-15)) ;
#45611 = DIRECTION('',(-2.73921926312881E-15,-1.,9.75120701384738E-13)) ;
#45612 = DIRECTION('',(-1.,2.73921926332625E-15,2.02962646689287E-13)) ;
#45613 = DIRECTION('',(-2.7392192633255E-15,-1.,3.67555483654062E-15)) ;
#45614 = DIRECTION('',(-1.,2.73921926332625E-15,2.02476924116013E-13)) ;
#45615 = DIRECTION('center_axis',(2.7392192633255E-15,1.,-3.67555483654062E-15)) ;
#45616 = DIRECTION('ref_axis',(-1.,2.73921926332625E-15,2.02673185673349E-13)) ;
#45617 = DIRECTION('center_axis',(-2.7392192633255E-15,-1.,3.67555483654062E-15)) ;
#45618 = DIRECTION('ref_axis',(-1.,2.73921926332625E-15,2.02673185673349E-13)) ;
#45619 = DIRECTION('center_axis',(-1.62899623870035E-15,-1.,3.6755548365404E-15)) ;
#45620 = DIRECTION('ref_axis',(-2.01921812603701E-13,-3.67555483654007E-15,
-1.)) ;
#45621 = DIRECTION('center_axis',(-1.,2.73921926332625E-15,2.02476924116013E-13)) ;
#45622 = DIRECTION('ref_axis',(-2.02476924116013E-13,-3.67555483654007E-15,
-1.)) ;
#45623 = DIRECTION('center_axis',(1.,2.72296279542125E-14,-1.42803113028906E-13)) ;
#45624 = DIRECTION('ref_axis',(-1.42803113028906E-13,-3.67555483654022E-15,
-1.)) ;
#45625 = DIRECTION('center_axis',(-1.,-2.9385320195592E-15,1.63381088479862E-13)) ;
#45626 = DIRECTION('ref_axis',(2.9385320195601E-15,-1.,5.53211507838757E-15)) ;
#45627 = DIRECTION('center_axis',(1.,-2.73921926332625E-15,-2.02476924116013E-13)) ;
#45628 = DIRECTION('ref_axis',(2.02476924116013E-13,3.67555483654007E-15,
1.)) ;
#45629 = DIRECTION('center_axis',(1.,-7.22135217855854E-15,-1.97994791200781E-13)) ;
#45630 = DIRECTION('ref_axis',(-7.2213521785591E-15,-1.,-2.82240600992682E-15)) ;
#45631 = DIRECTION('center_axis',(1.,-2.73921926332625E-15,-2.02476924116013E-13)) ;
#45632 = DIRECTION('ref_axis',(-2.73921926332635E-15,-1.,-5.017057076176E-16)) ;
#45633 = DIRECTION('center_axis',(6.56896527721512E-15,1.,-4.97129876952025E-15)) ;
#45634 = DIRECTION('ref_axis',(-1.79034390112784E-13,0.,-1.)) ;
#45635 = DIRECTION('center_axis',(-2.7392192633255E-15,-1.,3.67555483654062E-15)) ;
#45636 = DIRECTION('ref_axis',(-2.02476924116013E-13,-3.67555483654007E-15,
-1.)) ;
#45637 = DIRECTION('center_axis',(-2.7392192633255E-15,-1.,3.67555483654062E-15)) ;
#45638 = DIRECTION('ref_axis',(-1.,2.73921926332624E-15,2.02476924116013E-13)) ;
#45639 = DIRECTION('',(-2.0199120154274E-13,-3.67555483654007E-15,-1.)) ;
#45640 = DIRECTION('',(1.,-2.73921926332625E-15,-2.02476924116013E-13)) ;
#45641 = DIRECTION('',(2.0199120154274E-13,3.67555483654007E-15,1.)) ;
#45642 = DIRECTION('center_axis',(-1.,2.73921926332625E-15,2.02476924116013E-13)) ;
#45643 = DIRECTION('ref_axis',(2.73921926332551E-15,1.,-3.67555483654063E-15)) ;
#45644 = DIRECTION('',(-2.02476924116013E-13,-3.67555483654007E-15,-1.)) ;
#45645 = DIRECTION('',(-2.73921926512386E-15,-1.,-8.87810864217555E-12)) ;
#45646 = DIRECTION('',(-2.02546313055052E-13,-3.12044332422749E-15,-1.)) ;
#45647 = DIRECTION('center_axis',(1.,-2.73921926332625E-15,-2.02476924116013E-13)) ;
#45648 = DIRECTION('ref_axis',(-2.73921926332551E-15,-1.,3.67555483654063E-15)) ;
#45649 = DIRECTION('',(9.68705927284872E-13,-1.,3.67555483634393E-15)) ;
#45650 = DIRECTION('',(2.02962646689287E-13,3.67555483654007E-15,1.)) ;
#45651 = DIRECTION('',(-2.7392192633255E-15,-1.,3.67555483654062E-15)) ;
#45652 = DIRECTION('',(2.02476924116013E-13,3.67555483654007E-15,1.)) ;
#45653 = DIRECTION('center_axis',(2.7392192633255E-15,1.,-3.67555483654062E-15)) ;
#45654 = DIRECTION('ref_axis',(2.02673185673349E-13,3.67555483654006E-15,
1.)) ;
#45655 = DIRECTION('center_axis',(-2.7392192633255E-15,-1.,3.67555483654062E-15)) ;
#45656 = DIRECTION('ref_axis',(2.02673185673349E-13,3.67555483654006E-15,
1.)) ;
#45657 = DIRECTION('center_axis',(-2.73921926332573E-15,-1.,2.56533181191547E-15)) ;
#45658 = DIRECTION('ref_axis',(-1.,2.73921926332625E-15,2.01921812603701E-13)) ;
#45659 = DIRECTION('center_axis',(2.02476924116013E-13,3.67555483654007E-15,
1.)) ;
#45660 = DIRECTION('ref_axis',(-1.,2.73921926332625E-15,2.02476924116013E-13)) ;
#45661 = DIRECTION('center_axis',(-1.42803113028906E-13,2.62932923809983E-14,
-1.)) ;
#45662 = DIRECTION('ref_axis',(-1.,2.73921926332604E-15,1.42803113028906E-13)) ;
#45663 = DIRECTION('center_axis',(1.63381088479862E-13,-2.00219644634513E-15,
1.)) ;
#45664 = DIRECTION('ref_axis',(-8.82659021478556E-16,-1.,-2.00219644634499E-15)) ;
#45665 = DIRECTION('center_axis',(-2.02476924116013E-13,-3.67555483654007E-15,
-1.)) ;
#45666 = DIRECTION('ref_axis',(1.,-2.73921926332625E-15,-2.02476924116013E-13)) ;
#45667 = DIRECTION('center_axis',(-1.97994791200781E-13,-8.15768775177239E-15,
-1.)) ;
#45668 = DIRECTION('ref_axis',(-9.23718010979295E-15,-1.,8.15768775177422E-15)) ;
#45669 = DIRECTION('center_axis',(-2.02476924116013E-13,-3.67555483654007E-15,
-1.)) ;
#45670 = DIRECTION('ref_axis',(-6.91647980748373E-15,-1.,3.67555483654147E-15)) ;
#45671 = DIRECTION('center_axis',(1.44347533034587E-15,1.,-7.50530085043024E-15)) ;
#45672 = DIRECTION('ref_axis',(1.79034390112784E-13,0.,1.)) ;
#45673 = DIRECTION('center_axis',(-2.7392192633255E-15,-1.,3.67555483654062E-15)) ;
#45674 = DIRECTION('ref_axis',(-2.02476924116013E-13,-3.67555483654007E-15,
-1.)) ;
#45675 = DIRECTION('',(-2.03032035628326E-13,-3.67555483654007E-15,-1.)) ;
#45676 = DIRECTION('',(1.,-2.73921926332625E-15,-2.02476924116013E-13)) ;
#45677 = DIRECTION('',(2.02962646689287E-13,3.67555483654007E-15,1.)) ;
#45678 = DIRECTION('center_axis',(2.7392192633255E-15,1.,-3.67555483654062E-15)) ;
#45679 = DIRECTION('ref_axis',(-1.,2.73921926332624E-15,2.02476924116013E-13)) ;
#45680 = DIRECTION('center_axis',(-1.,2.73921926332625E-15,2.02476924116013E-13)) ;
#45681 = DIRECTION('ref_axis',(2.73921926332551E-15,1.,-3.67555483654063E-15)) ;
#45682 = DIRECTION('',(2.02823868811209E-13,4.23066634885265E-15,1.)) ;
#45683 = DIRECTION('',(9.6870592728667E-13,-1.,8.88545975184844E-12)) ;
#45684 = DIRECTION('',(-2.02476924116013E-13,-3.67555483654007E-15,-1.)) ;
#45685 = DIRECTION('center_axis',(1.,-2.73921926332625E-15,-2.02476924116013E-13)) ;
#45686 = DIRECTION('ref_axis',(-2.73921926332551E-15,-1.,3.67555483654063E-15)) ;
#45687 = DIRECTION('',(-2.02476924116013E-13,-3.67555483654007E-15,-1.)) ;
#45688 = DIRECTION('',(-2.7392192633255E-15,-1.,3.67555483654062E-15)) ;
#45689 = DIRECTION('',(2.02476924116013E-13,3.67555483654007E-15,1.)) ;
#45690 = DIRECTION('',(-2.7392192633255E-15,-1.,3.67555483654062E-15)) ;
#45691 = DIRECTION('center_axis',(2.7392192633255E-15,1.,-3.67555483654062E-15)) ;
#45692 = DIRECTION('ref_axis',(1.,-2.73921926332624E-15,-2.02476924116013E-13)) ;
#45693 = DIRECTION('center_axis',(2.7392192633255E-15,1.,-3.67555483654062E-15)) ;
#45694 = DIRECTION('ref_axis',(-1.,2.73921926332625E-15,2.03032035628326E-13)) ;
#45695 = DIRECTION('center_axis',(-2.7392192633255E-15,-1.,3.67555483654062E-15)) ;
#45696 = DIRECTION('ref_axis',(1.,-2.73921926332624E-15,-2.02476924116013E-13)) ;
#45697 = DIRECTION('center_axis',(-2.02935662438468E-13,-3.51738227745041E-15,
-1.)) ;
#45698 = DIRECTION('ref_axis',(-0.707106781186548,-0.707106781186547,1.45984347915236E-13)) ;
#45699 = DIRECTION('center_axis',(2.28126356985122E-13,-4.09309664761724E-15,
1.)) ;
#45700 = DIRECTION('ref_axis',(-8.82659021478992E-16,-1.,-4.09309664761704E-15)) ;
#45701 = DIRECTION('center_axis',(-2.62150735203121E-13,-3.36444020540783E-14,
-1.)) ;
#45702 = DIRECTION('ref_axis',(-1.,6.45233974702268E-15,2.62150735203121E-13)) ;
#45703 = DIRECTION('center_axis',(2.02476924116013E-13,3.67555483654007E-15,
1.)) ;
#45704 = DIRECTION('ref_axis',(0.707106781186545,-0.70710678118655,-1.40573796326686E-13)) ;
#45705 = DIRECTION('center_axis',(-2.02476924116013E-13,-3.67555483654007E-15,
-1.)) ;
#45706 = DIRECTION('ref_axis',(-4.13163944471158E-15,-1.,3.67555483654091E-15)) ;
#45707 = DIRECTION('center_axis',(-2.06959057031246E-13,8.06578078692253E-16,
-1.)) ;
#45708 = DIRECTION('ref_axis',(-6.91647980748464E-15,-1.,-8.06578078690822E-16)) ;
#45709 = DIRECTION('center_axis',(3.74218483200288E-15,1.,-4.17141315729775E-15)) ;
#45710 = DIRECTION('ref_axis',(-1.79034390112784E-13,0.,-1.)) ;
#45711 = DIRECTION('center_axis',(-2.7392192633255E-15,-1.,3.67555483654062E-15)) ;
#45712 = DIRECTION('ref_axis',(-2.02476924116013E-13,-3.67555483654007E-15,
-1.)) ;
#45713 = DIRECTION('',(1.,-2.73921926332625E-15,-2.02476924116013E-13)) ;
#45714 = DIRECTION('',(2.02476924116013E-13,3.67555483654007E-15,1.)) ;
#45715 = DIRECTION('',(-1.,2.73921926332625E-15,2.02476924116013E-13)) ;
#45716 = DIRECTION('center_axis',(2.7392192633255E-15,1.,-3.67555483654062E-15)) ;
#45717 = DIRECTION('ref_axis',(-2.02476924116013E-13,-3.67555483654007E-15,
-1.)) ;
#45718 = DIRECTION('center_axis',(-2.02476924116013E-13,-3.67555483654007E-15,
-1.)) ;
#45719 = DIRECTION('ref_axis',(-2.7392192633255E-15,-1.,3.67555483654062E-15)) ;
#45720 = DIRECTION('',(-1.,3.29433077563883E-15,2.02407535176974E-13)) ;
#45721 = DIRECTION('',(-8.88452341627542E-12,-1.,3.67555483833898E-15)) ;
#45722 = DIRECTION('',(1.,-2.73921926332625E-15,-2.02476924116013E-13)) ;
#45723 = DIRECTION('center_axis',(2.01505478969466E-13,3.67555483654007E-15,
1.)) ;
#45724 = DIRECTION('ref_axis',(2.7392192633255E-15,1.,-3.67555483654062E-15)) ;
#45725 = DIRECTION('',(1.,-2.73921926332625E-15,-2.0199120154274E-13)) ;
#45726 = DIRECTION('',(-2.7392192633255E-15,-1.,3.67555483654062E-15)) ;
#45727 = DIRECTION('',(-1.,2.73921926332625E-15,2.02476924116013E-13)) ;
#45728 = DIRECTION('',(-2.7392192635222E-15,-1.,-9.67769591711657E-13)) ;
#45729 = DIRECTION('center_axis',(2.7392192633255E-15,1.,-3.67555483654062E-15)) ;
#45730 = DIRECTION('ref_axis',(2.02476924116013E-13,3.67555483654007E-15,
1.)) ;
#45731 = DIRECTION('center_axis',(2.7392192633255E-15,1.,-3.67555483654062E-15)) ;
#45732 = DIRECTION('ref_axis',(-2.02476924116013E-13,-3.67555483654007E-15,
-1.)) ;
#45733 = DIRECTION('center_axis',(-2.7392192633255E-15,-1.,3.67555483654062E-15)) ;
#45734 = DIRECTION('ref_axis',(2.02476924116013E-13,3.67555483654007E-15,
1.)) ;
#45735 = DIRECTION('center_axis',(1.,-2.55781860456987E-15,-2.02516882062598E-13)) ;
#45736 = DIRECTION('ref_axis',(-1.45009711491555E-13,-0.70710678118655,-0.707106781186545)) ;
#45737 = DIRECTION('center_axis',(-1.,-9.51156647651177E-15,2.23644222729441E-13)) ;
#45738 = DIRECTION('ref_axis',(9.51156647651311E-15,-1.,5.99625513884829E-15)) ;
#45739 = DIRECTION('center_axis',(1.,-3.2708066480865E-14,-2.62150735203121E-13)) ;
#45740 = DIRECTION('ref_axis',(-2.62150735203121E-13,3.75656471563051E-17,
-1.)) ;
#45741 = DIRECTION('center_axis',(-1.,2.58104670423658E-15,2.02018185793558E-13)) ;
#45742 = DIRECTION('ref_axis',(1.41023353470504E-13,-0.707106781186545,0.70710678118655)) ;
#45743 = DIRECTION('center_axis',(1.,-2.73921926332625E-15,-2.02476924116013E-13)) ;
#45744 = DIRECTION('ref_axis',(-2.7392192633271E-15,-1.,-4.21482619131383E-15)) ;
#45745 = DIRECTION('center_axis',(1.,1.74291365190604E-15,-2.06959057031246E-13)) ;
#45746 = DIRECTION('ref_axis',(1.74291365190546E-15,-1.,-2.82240600992864E-15)) ;
#45747 = DIRECTION('center_axis',(-2.34486411375479E-15,1.,-2.80866739088387E-15)) ;
#45748 = DIRECTION('ref_axis',(-1.79034390112784E-13,0.,-1.)) ;
#45749 = DIRECTION('center_axis',(1.,-2.73921926332625E-15,-2.02476924116013E-13)) ;
#45750 = DIRECTION('ref_axis',(2.73921926332551E-15,1.,-3.67555483654062E-15)) ;
#45751 = DIRECTION('',(2.7392192633255E-15,1.,-3.67555483654062E-15)) ;
#45752 = DIRECTION('',(-2.7392192633255E-15,-1.,3.67555483654062E-15)) ;
#45753 = DIRECTION('',(2.02476924116013E-13,3.67555483654007E-15,1.)) ;
#45754 = DIRECTION('',(2.02476924116013E-13,3.67555483654007E-15,1.)) ;
#45755 = DIRECTION('',(2.02476924116013E-13,3.67555483654007E-15,1.)) ;
#45756 = DIRECTION('',(2.02476924116013E-13,3.67555483654007E-15,1.)) ;
#45757 = DIRECTION('center_axis',(-1.,2.73921926332625E-15,2.02476924116013E-13)) ;
#45758 = DIRECTION('ref_axis',(-2.73921926332551E-15,-1.,3.67555483654062E-15)) ;
#45759 = DIRECTION('',(2.73921299462249E-15,1.,-3.09600898101992E-8)) ;
#45760 = DIRECTION('',(-2.7392192633255E-15,-1.,3.67555483654062E-15)) ;
#45761 = DIRECTION('',(-2.02476924116013E-13,-3.67555483654007E-15,-1.)) ;
#45762 = DIRECTION('',(-2.02476924116013E-13,-3.67555483654007E-15,-1.)) ;
#45763 = DIRECTION('',(-2.02476924116013E-13,-3.67555483654007E-15,-1.)) ;
#45764 = DIRECTION('',(-2.02476924116013E-13,-3.67555483654007E-15,-1.)) ;
#45765 = DIRECTION('center_axis',(-2.02476924116013E-13,-3.67555483654007E-15,
-1.)) ;
#45766 = DIRECTION('ref_axis',(1.,-2.73921926332625E-15,-2.02476924116013E-13)) ;
#45767 = DIRECTION('',(-6.86270959829528E-15,1.,7.12661513278716E-15)) ;
#45768 = DIRECTION('',(-2.7392192633255E-15,-1.,3.67555483654062E-15)) ;
#45769 = DIRECTION('',(1.,-2.73921926332628E-15,-2.11050196179211E-13)) ;
#45770 = DIRECTION('',(1.,-2.73921926332624E-15,-1.99601878747771E-13)) ;
#45771 = DIRECTION('',(1.,-2.73921926332624E-15,-1.99921328233131E-13)) ;
#45772 = DIRECTION('',(1.,-2.73921926332628E-15,-2.10097610394411E-13)) ;
#45773 = DIRECTION('center_axis',(2.02476924116013E-13,3.67555483654007E-15,
1.)) ;
#45774 = DIRECTION('ref_axis',(-1.,2.73921926332625E-15,2.02476924116013E-13)) ;
#45775 = DIRECTION('',(2.7392192633255E-15,1.,-3.67555483654062E-15)) ;
#45776 = DIRECTION('',(3.09600846192426E-8,-1.,3.67554856783736E-15)) ;
#45777 = DIRECTION('',(-1.,2.73921926332625E-15,2.02476924116013E-13)) ;
#45778 = DIRECTION('',(-1.,2.73921926332625E-15,2.02476924116013E-13)) ;
#45779 = DIRECTION('',(-1.,2.73921926332626E-15,2.05351969484256E-13)) ;
#45780 = DIRECTION('',(-1.,2.73921926332622E-15,1.93903652052816E-13)) ;
#45781 = DIRECTION('center_axis',(-2.7392192633255E-15,-1.,3.67555483654062E-15)) ;
#45782 = DIRECTION('ref_axis',(-2.02476924116013E-13,-3.67555483654007E-15,
-1.)) ;
#45783 = DIRECTION('center_axis',(-7.3207473378131E-15,1.,-1.37355214376752E-14)) ;
#45784 = DIRECTION('ref_axis',(0.801573073879436,1.40805385337468E-14,0.597896819887406)) ;
#45785 = DIRECTION('center_axis',(3.99202076906257E-14,1.,-4.6659502919908E-14)) ;
#45786 = DIRECTION('ref_axis',(-0.597896819887407,6.1269166408667E-14,0.801573073879435)) ;
#45787 = DIRECTION('center_axis',(2.7392192633255E-15,1.,-3.67555483654062E-15)) ;
#45788 = DIRECTION('ref_axis',(-0.70710679608757,4.53593025184281E-15,0.707106766285525)) ;
#45789 = DIRECTION('center_axis',(-1.92665475456957E-15,1.,-9.06964734259742E-15)) ;
#45790 = DIRECTION('ref_axis',(-0.801573073879439,-6.96706787756399E-15,-0.597896819887402)) ;
#45791 = DIRECTION('center_axis',(-7.32074733780901E-15,1.,6.38441176459794E-15)) ;
#45792 = DIRECTION('ref_axis',(0.597896819887408,9.49462411553601E-15,-0.801573073879434)) ;
#45793 = DIRECTION('center_axis',(5.67865126919919E-11,-1.,5.65924766963123E-11)) ;
#45794 = DIRECTION('ref_axis',(0.728572558446093,2.60902348252204E-12,-0.684968632186405)) ;
#45795 = DIRECTION('center_axis',(1.,-2.73921926332625E-15,-2.02476924116013E-13)) ;
#45796 = DIRECTION('ref_axis',(2.73921926332551E-15,1.,-3.67555483654062E-15)) ;
#45797 = DIRECTION('',(2.73916514353843E-15,0.999999999999964,-2.67288669829288E-7)) ;
#45798 = DIRECTION('center_axis',(-2.02476924116013E-13,-3.67555483654007E-15,
-1.)) ;
#45799 = DIRECTION('ref_axis',(1.,-2.73921926332625E-15,-2.02476924116013E-13)) ;
#45800 = DIRECTION('',(2.67288913307799E-7,-0.999999999999964,3.67550071670292E-15)) ;
#45801 = DIRECTION('center_axis',(5.6783473877901E-11,-1.,-5.65819808726216E-11)) ;
#45802 = DIRECTION('ref_axis',(-0.684968632186398,2.32918013337625E-12,-0.728572558446099)) ;
#45803 = DIRECTION('center_axis',(-1.,2.73921926332625E-15,2.02476924116013E-13)) ;
#45804 = DIRECTION('ref_axis',(-2.73921926332551E-15,-1.,3.67555483654062E-15)) ;
#45805 = DIRECTION('',(-2.73927338311502E-15,-0.999999999999964,-2.67288675523886E-7)) ;
#45806 = DIRECTION('center_axis',(-2.02476924116013E-13,-3.67555483654007E-15,
-1.)) ;
#45807 = DIRECTION('ref_axis',(1.,-2.73921926332625E-15,-2.02476924116013E-13)) ;
#45808 = DIRECTION('',(-2.67288663414514E-7,0.999999999999964,-3.67550071675352E-15)) ;
#45809 = DIRECTION('center_axis',(5.2515080430742E-9,-1.,-5.2515034750072E-9)) ;
#45810 = DIRECTION('ref_axis',(-0.728572559766824,-7.42321980239912E-9,0.684968630781598)) ;
#45811 = DIRECTION('center_axis',(-5.25072494542696E-9,-1.,5.25067969529154E-9)) ;
#45812 = DIRECTION('ref_axis',(-0.707106793325164,7.42561443343648E-9,0.707106769047931)) ;
#45813 = DIRECTION('center_axis',(-1.,2.73921926332625E-15,2.02476924116013E-13)) ;
#45814 = DIRECTION('ref_axis',(-2.73921926332551E-15,-1.,3.67555483654062E-15)) ;
#45815 = DIRECTION('',(2.7392965773295E-15,0.999999999999927,3.81841060590217E-7)) ;
#45816 = DIRECTION('center_axis',(2.02476924116013E-13,3.67555483654007E-15,
1.)) ;
#45817 = DIRECTION('ref_axis',(-1.,2.73921926332625E-15,2.02476924116013E-13)) ;
#45818 = DIRECTION('',(-3.81841078221714E-7,-0.999999999999927,3.67563215054682E-15)) ;
#45819 = DIRECTION('center_axis',(-5.64897426180912E-11,-1.,5.68916334461304E-11)) ;
#45820 = DIRECTION('ref_axis',(0.684968632186416,2.75598120034729E-12,0.728572558446082)) ;
#45821 = DIRECTION('center_axis',(1.,-2.73921926332625E-15,-2.02476924116013E-13)) ;
#45822 = DIRECTION('ref_axis',(2.73921926332551E-15,1.,-3.67555483654062E-15)) ;
#45823 = DIRECTION('',(-2.73916514353579E-15,-0.999999999999964,2.67288682874995E-7)) ;
#45824 = DIRECTION('center_axis',(2.02476924116013E-13,3.67555483654007E-15,
1.)) ;
#45825 = DIRECTION('ref_axis',(-1.,2.73921926332625E-15,2.02476924116013E-13)) ;
#45826 = DIRECTION('',(2.67288668892953E-7,0.999999999999964,-3.67560895632747E-15)) ;
#45827 = DIRECTION('center_axis',(-2.7392192633255E-15,-1.,3.67555483654062E-15)) ;
#45828 = DIRECTION('ref_axis',(-0.707106792894461,4.53593025483263E-15,0.707106769478634)) ;
#45829 = DIRECTION('center_axis',(-2.7392192633255E-15,-1.,3.67555483654062E-15)) ;
#45830 = DIRECTION('ref_axis',(0.707106781816028,-4.53593026520576E-15,-0.707106780557067)) ;
#45831 = DIRECTION('center_axis',(-2.7392192633255E-15,-1.,3.67555483654062E-15)) ;
#45832 = DIRECTION('ref_axis',(-0.707106792894461,4.53593025483263E-15,0.707106769478634)) ;
#45833 = DIRECTION('center_axis',(-2.7392192633255E-15,-1.,3.67555483654062E-15)) ;
#45834 = DIRECTION('ref_axis',(-0.707106792894461,4.53593025483263E-15,0.707106769478634)) ;
#45835 = DIRECTION('',(1.75408298996871E-13,1.,-2.90739654573714E-15)) ;
#45836 = DIRECTION('',(-1.,1.75408298996871E-13,-4.93057902841558E-28)) ;
#45837 = DIRECTION('',(1.75408298996871E-13,1.,-2.90739654573714E-15)) ;
#45838 = DIRECTION('',(-1.,1.75408298996871E-13,-4.93057902841558E-28)) ;
#45839 = DIRECTION('',(1.75408298996871E-13,1.,-2.90739654573714E-15)) ;
#45840 = DIRECTION('',(-1.,1.75408298996871E-13,-4.93057902841558E-28)) ;
#45841 = DIRECTION('',(1.75408298996871E-13,1.,-2.90739654573714E-15)) ;
#45842 = DIRECTION('',(-1.,1.75408298996871E-13,-4.93057902841558E-28)) ;
#45843 = DIRECTION('',(1.75408298996871E-13,1.,-2.90739654573714E-15)) ;
#45844 = DIRECTION('',(-1.,1.75408298996871E-13,-4.93057902841558E-28)) ;
#45845 = DIRECTION('',(1.75408298996871E-13,1.,-2.90739654573714E-15)) ;
#45846 = DIRECTION('',(-1.,1.75408298996871E-13,-4.93057902841558E-28)) ;
#45847 = DIRECTION('',(1.75408298996871E-13,1.,-2.90739654573714E-15)) ;
#45848 = DIRECTION('',(-1.,1.75408298996871E-13,-4.93057902841558E-28)) ;
#45849 = DIRECTION('',(1.75408298996871E-13,1.,-2.90739654573714E-15)) ;
#45850 = DIRECTION('',(-1.,1.75408298996871E-13,-4.93057902841558E-28)) ;
#45851 = DIRECTION('',(1.75408298996871E-13,1.,-2.90739654573714E-15)) ;
#45852 = DIRECTION('',(-1.,1.75408298996871E-13,-4.93057902841558E-28)) ;
#45853 = DIRECTION('',(1.13595970351826E-28,-2.00890147845606E-41,1.)) ;
#45854 = DIRECTION('',(1.,-3.21722349341685E-86,-1.13595970351826E-28)) ;
#45855 = DIRECTION('',(0.,0.,1.)) ;
#45856 = DIRECTION('',(1.,0.,0.)) ;
#45857 = DIRECTION('',(0.,0.,1.)) ;
#45858 = DIRECTION('',(1.,0.,0.)) ;
#45859 = DIRECTION('',(0.,0.,1.)) ;
#45860 = DIRECTION('',(1.,0.,0.)) ;
#45861 = DIRECTION('axis',(0.,0.,1.)) ;
#45862 = DIRECTION('refdir',(1.,0.,0.)) ;
#45863 = DIRECTION('center_axis',(-3.21164817626321E-14,0.707106781183433,
-0.707106781189663)) ;
#45864 = DIRECTION('ref_axis',(-1.,4.59435859315612E-29,4.54195640842224E-14)) ;
#45865 = DIRECTION('',(-0.577350269185717,-0.577350269194137,-0.577350269189023)) ;
#45866 = DIRECTION('',(-1.,-4.54195640846222E-14,4.43134223659454E-28)) ;
#45867 = DIRECTION('',(-0.577350269188067,0.577350269192936,0.577350269187875)) ;
#45868 = DIRECTION('',(0.57735026919122,0.577350269191385,0.577350269186272)) ;
#45869 = DIRECTION('',(1.,4.54195640846222E-14,-4.43134223659454E-28)) ;
#45870 = DIRECTION('',(0.577350269190983,-0.577350269191477,-0.577350269186417)) ;
#45871 = DIRECTION('center_axis',(-0.707106781186648,0.707106781186447,-2.17344707950985E-15)) ;
#45872 = DIRECTION('ref_axis',(-3.07371833694259E-15,-1.89978378844695E-30,
1.)) ;
#45873 = DIRECTION('',(0.577350269189617,0.577350269189779,-0.577350269189481)) ;
#45874 = DIRECTION('',(3.03527276676558E-28,3.07371833694377E-15,1.)) ;
#45875 = DIRECTION('',(-0.577350269189562,-0.577350269189728,-0.577350269189587)) ;
#45876 = DIRECTION('',(-0.577350269187503,-0.577350269187665,0.57735026919371)) ;
#45877 = DIRECTION('',(-3.03527276676558E-28,-3.07371833694377E-15,-1.)) ;
#45878 = DIRECTION('center_axis',(-0.707106781186447,-3.42899288422795E-14,
-0.707106781186648)) ;
#45879 = DIRECTION('ref_axis',(-0.707106781186648,-5.24209240922293E-31,0.707106781186447)) ;
#45880 = DIRECTION('',(4.54195640846222E-14,-1.,3.07371833694377E-15)) ;
#45881 = DIRECTION('',(0.577350269189872,0.57735026918927,-0.577350269189736)) ;
#45882 = DIRECTION('',(-0.577350269189744,0.577350269189582,0.577350269189552)) ;
#45883 = DIRECTION('',(-4.54195640846222E-14,1.,-3.07371833694377E-15)) ;
#45884 = DIRECTION('center_axis',(-3.03527276676558E-28,-3.07371833694377E-15,
-1.)) ;
#45885 = DIRECTION('ref_axis',(-4.54195640846222E-14,1.,-3.07371833694377E-15)) ;
#45886 = DIRECTION('',(-4.54195640846222E-14,1.,-3.07371833694377E-15)) ;
#45887 = DIRECTION('',(1.,4.54195640846222E-14,-4.43134223659454E-28)) ;
#45888 = DIRECTION('center_axis',(3.21164817627867E-14,-0.707106781186849,
-0.707106781186246)) ;
#45889 = DIRECTION('ref_axis',(-1.,1.22805031005106E-29,-4.54195640846605E-14)) ;
#45890 = DIRECTION('',(-0.577350269186846,-0.577350269190783,0.577350269191249)) ;
#45891 = DIRECTION('',(-1.,-4.54195640846222E-14,4.43134223659454E-28)) ;
#45892 = DIRECTION('',(-0.577350269189563,0.577350269189398,-0.577350269189916)) ;
#45893 = DIRECTION('',(0.577350269187627,-0.577350269190366,0.577350269190884)) ;
#45894 = DIRECTION('center_axis',(-0.707106781186447,-0.707106781186648,2.1734470795109E-15)) ;
#45895 = DIRECTION('ref_axis',(3.07371833694495E-15,-2.57298801481783E-30,
1.)) ;
#45896 = DIRECTION('',(3.03527276676558E-28,3.07371833694377E-15,1.)) ;
#45897 = DIRECTION('',(0.577350269189561,-0.577350269189399,-0.577350269189917)) ;
#45898 = DIRECTION('',(0.577350269189689,-0.577350269189523,0.577350269189665)) ;
#45899 = DIRECTION('',(-3.03527276676558E-28,-3.07371833694377E-15,-1.)) ;
#45900 = DIRECTION('center_axis',(3.21164817627873E-14,-0.707106781186849,
0.707106781186246)) ;
#45901 = DIRECTION('ref_axis',(1.,-5.21959547942856E-29,-4.54195640846614E-14)) ;
#45902 = DIRECTION('',(-0.577350269188176,0.577350269190091,0.57735026919061)) ;
#45903 = DIRECTION('',(-1.,-4.54195640846222E-14,4.43134223659454E-28)) ;
#45904 = DIRECTION('',(-0.577350269189765,-0.577350269189323,-0.577350269189789)) ;
#45905 = DIRECTION('',(1.,4.54195640846222E-14,-4.43134223659454E-28)) ;
#45906 = DIRECTION('',(0.577350269186844,0.577350269190784,0.57735026919125)) ;
#45907 = DIRECTION('center_axis',(-0.707106781186548,-2.9943034683263E-14,
0.707106781186548)) ;
#45908 = DIRECTION('ref_axis',(0.707106781186548,4.34801313340064E-31,0.707106781186548)) ;
#45909 = DIRECTION('',(-4.54195640846222E-14,1.,-3.07371833694377E-15)) ;
#45910 = DIRECTION('',(0.577350269191675,-0.577350269185553,0.57735026919165)) ;
#45911 = DIRECTION('',(4.54195640846222E-14,-1.,3.07371833694377E-15)) ;
#45912 = DIRECTION('center_axis',(3.03527276676558E-28,3.07371833694377E-15,
1.)) ;
#45913 = DIRECTION('ref_axis',(4.54195640846222E-14,-1.,3.07371833694377E-15)) ;
#45914 = DIRECTION('',(4.54195640846222E-14,-1.,3.07371833694377E-15)) ;
#45915 = DIRECTION('',(1.,4.54195640846222E-14,-4.43134223659454E-28)) ;
#45916 = DIRECTION('center_axis',(0.707106781188055,3.42899288423475E-14,
0.70710678118504)) ;
#45917 = DIRECTION('ref_axis',(0.70710678118504,-2.67373424278474E-31,-0.707106781188055)) ;
#45918 = DIRECTION('',(-0.577350269187484,-0.57735026919142,0.577350269189973)) ;
#45919 = DIRECTION('',(-4.54195640846222E-14,1.,-3.07371833694377E-15)) ;
#45920 = DIRECTION('',(0.57735026918865,-0.577350269189144,-0.577350269191083)) ;
#45921 = DIRECTION('',(0.577350269189981,0.577350269186425,-0.577350269192471)) ;
#45922 = DIRECTION('center_axis',(-3.21164817629419E-14,0.707106781190265,
0.70710678118283)) ;
#45923 = DIRECTION('ref_axis',(1.,-2.00665671353E-30,4.54195640850994E-14)) ;
#45924 = DIRECTION('',(-0.577350269187266,0.577350269187757,-0.577350269193854)) ;
#45925 = DIRECTION('',(-1.,-4.54195640846222E-14,4.43134223659454E-28)) ;
#45926 = DIRECTION('center_axis',(-1.,-4.54195640846222E-14,4.43134223659454E-28)) ;
#45927 = DIRECTION('ref_axis',(4.54195640846222E-14,-1.,3.07371833694377E-15)) ;
#45928 = DIRECTION('center_axis',(4.54195640846222E-14,-1.,3.07371833694377E-15)) ;
#45929 = DIRECTION('ref_axis',(-3.03527276676558E-28,-3.07371833694377E-15,
-1.)) ;
#45930 = DIRECTION('',(-6.99265107823647E-28,-3.07371833694377E-15,-1.)) ;
#45931 = DIRECTION('center_axis',(4.54195640846222E-14,-1.,3.07371833694377E-15)) ;
#45932 = DIRECTION('ref_axis',(6.81575822110954E-28,3.07371833694377E-15,
1.)) ;
#45933 = DIRECTION('center_axis',(4.54195640846222E-14,-1.,3.07371833694377E-15)) ;
#45934 = DIRECTION('ref_axis',(6.81575822110954E-28,3.07371833694377E-15,
1.)) ;
#45935 = DIRECTION('center_axis',(4.54195640846222E-14,-1.,3.07371833694377E-15)) ;
#45936 = DIRECTION('ref_axis',(6.81575822110954E-28,3.07371833694377E-15,
1.)) ;
#45937 = DIRECTION('center_axis',(4.54195640846222E-14,-1.,3.07371833694377E-15)) ;
#45938 = DIRECTION('ref_axis',(6.81575822110954E-28,3.07371833694377E-15,
1.)) ;
#45939 = DIRECTION('center_axis',(4.54195640846222E-14,-1.,3.07371833694377E-15)) ;
#45940 = DIRECTION('ref_axis',(6.81575822110954E-28,3.07371833694377E-15,
1.)) ;
#45941 = DIRECTION('center_axis',(-4.54195640846222E-14,1.,-3.07371833694377E-15)) ;
#45942 = DIRECTION('ref_axis',(3.03527276676558E-28,3.07371833694377E-15,
1.)) ;
#45943 = DIRECTION('',(6.99265107823647E-28,3.07371833694377E-15,1.)) ;
#45944 = DIRECTION('center_axis',(-4.54195640846222E-14,1.,-3.07371833694377E-15)) ;
#45945 = DIRECTION('ref_axis',(6.81575822110954E-28,3.07371833694377E-15,
1.)) ;
#45946 = DIRECTION('center_axis',(-4.54195640846222E-14,1.,-3.07371833694377E-15)) ;
#45947 = DIRECTION('ref_axis',(6.81575822110954E-28,3.07371833694377E-15,
1.)) ;
#45948 = DIRECTION('center_axis',(-4.54195640846222E-14,1.,-3.07371833694377E-15)) ;
#45949 = DIRECTION('ref_axis',(6.81575822110954E-28,3.07371833694377E-15,
1.)) ;
#45950 = DIRECTION('center_axis',(-4.54195640846222E-14,1.,-3.07371833694377E-15)) ;
#45951 = DIRECTION('ref_axis',(6.81575822110954E-28,3.07371833694377E-15,
1.)) ;
#45952 = DIRECTION('center_axis',(-4.54195640846222E-14,1.,-3.07371833694377E-15)) ;
#45953 = DIRECTION('ref_axis',(6.81575822110954E-28,3.07371833694377E-15,
1.)) ;
#45954 = DIRECTION('center_axis',(0.707106781188959,-0.707106781184136,2.17344707950247E-15)) ;
#45955 = DIRECTION('ref_axis',(3.07371833692211E-15,3.40932823150776E-30,
-1.)) ;
#45956 = DIRECTION('',(0.57735026918721,0.57735026919115,0.577350269190517)) ;
#45957 = DIRECTION('',(6.99265107823647E-28,3.07371833694377E-15,1.)) ;
#45958 = DIRECTION('center_axis',(-1.,-4.54195640846222E-14,8.38872054806543E-28)) ;
#45959 = DIRECTION('ref_axis',(4.54195640846222E-14,-1.,2.90739654572917E-15)) ;
#45960 = DIRECTION('',(4.54195640846222E-14,-1.,3.07371833694377E-15)) ;
#45961 = DIRECTION('',(-6.99265107823647E-28,-3.07371833694377E-15,-1.)) ;
#45962 = DIRECTION('center_axis',(0.707106781186849,0.707106781186246,-2.17344707950995E-15)) ;
#45963 = DIRECTION('ref_axis',(-3.07371833694185E-15,-4.33388060696312E-30,
-1.)) ;
#45964 = DIRECTION('',(-0.577350269188377,0.577350269188867,-0.577350269191634)) ;
#45965 = DIRECTION('center_axis',(0.707106781188557,2.99430346833604E-14,
-0.707106781184538)) ;
#45966 = DIRECTION('ref_axis',(-0.707106781184538,-7.37594522657362E-31,-0.707106781188557)) ;
#45967 = DIRECTION('center_axis',(-4.54195640846222E-14,1.,-3.07371833694377E-15)) ;
#45968 = DIRECTION('ref_axis',(6.81575822110954E-28,3.07371833694377E-15,
1.)) ;
#45969 = DIRECTION('',(-4.54195640846222E-14,1.,-3.07371833694377E-15)) ;
#45970 = DIRECTION('center_axis',(-4.54195640846222E-14,1.,-3.07371833694377E-15)) ;
#45971 = DIRECTION('ref_axis',(6.81575822110954E-28,3.07371833694377E-15,
1.)) ;
#45972 = DIRECTION('',(-4.54195640846222E-14,1.,-3.07371833694377E-15)) ;
#45973 = DIRECTION('center_axis',(-4.54195640846222E-14,1.,-3.07371833694377E-15)) ;
#45974 = DIRECTION('ref_axis',(6.81575822110954E-28,3.07371833694377E-15,
1.)) ;
#45975 = DIRECTION('',(-4.54195640846222E-14,1.,-3.07371833694377E-15)) ;
#45976 = DIRECTION('center_axis',(-4.54195640846222E-14,1.,-3.07371833694377E-15)) ;
#45977 = DIRECTION('ref_axis',(6.81575822110954E-28,3.07371833694377E-15,
1.)) ;
#45978 = DIRECTION('',(-4.54195640846222E-14,1.,-3.07371833694377E-15)) ;
#45979 = DIRECTION('center_axis',(-4.54195640846222E-14,1.,-3.07371833694377E-15)) ;
#45980 = DIRECTION('ref_axis',(6.81575822110954E-28,3.07371833694377E-15,
1.)) ;
#45981 = DIRECTION('',(-4.54195640846222E-14,1.,-3.07371833694377E-15)) ;
#45982 = DIRECTION('axis',(0.,0.,1.)) ;
#45983 = DIRECTION('refdir',(1.,0.,0.)) ;
#45984 = DIRECTION('axis',(0.,0.,1.)) ;
#45985 = DIRECTION('refdir',(1.,0.,0.)) ;
#45986 = DIRECTION('axis',(0.,0.,1.)) ;
#45987 = DIRECTION('refdir',(1.,0.,0.)) ;
#45988 = DIRECTION('axis',(0.,0.,1.)) ;
#45989 = DIRECTION('refdir',(1.,0.,0.)) ;
#45990 = DIRECTION('axis',(0.,0.,1.)) ;
#45991 = DIRECTION('refdir',(1.,0.,0.)) ;
#45992 = DIRECTION('center_axis',(0.,0.,1.)) ;
#45993 = DIRECTION('ref_axis',(1.,0.,0.)) ;
#45994 = DIRECTION('',(0.,0.,-1.)) ;
#45995 = DIRECTION('center_axis',(0.,0.,-1.)) ;
#45996 = DIRECTION('ref_axis',(1.,0.,0.)) ;
#45997 = DIRECTION('center_axis',(0.,0.,1.)) ;
#45998 = DIRECTION('ref_axis',(1.,0.,0.)) ;
#45999 = DIRECTION('',(0.,0.,-1.)) ;
#46000 = DIRECTION('center_axis',(0.,0.,1.)) ;
#46001 = DIRECTION('ref_axis',(1.,0.,0.)) ;
#46002 = DIRECTION('',(0.,0.,-1.)) ;
#46003 = DIRECTION('center_axis',(0.,0.,1.)) ;
#46004 = DIRECTION('ref_axis',(1.,0.,0.)) ;
#46005 = DIRECTION('',(0.,0.,-1.)) ;
#46006 = DIRECTION('center_axis',(0.,0.,1.)) ;
#46007 = DIRECTION('ref_axis',(1.,0.,0.)) ;
#46008 = DIRECTION('',(0.,0.,-1.)) ;
#46009 = DIRECTION('center_axis',(0.,0.,1.)) ;
#46010 = DIRECTION('ref_axis',(1.,0.,0.)) ;
#46011 = DIRECTION('',(0.,0.,-1.)) ;
#46012 = DIRECTION('center_axis',(0.,0.,1.)) ;
#46013 = DIRECTION('ref_axis',(1.,0.,0.)) ;
#46014 = DIRECTION('',(0.,0.,-1.)) ;
#46015 = DIRECTION('center_axis',(0.,0.,1.)) ;
#46016 = DIRECTION('ref_axis',(1.,0.,0.)) ;
#46017 = DIRECTION('',(0.,0.,-1.)) ;
#46018 = DIRECTION('center_axis',(0.,0.,1.)) ;
#46019 = DIRECTION('ref_axis',(1.,0.,0.)) ;
#46020 = DIRECTION('',(0.,0.,-1.)) ;
#46021 = DIRECTION('center_axis',(0.,0.,1.)) ;
#46022 = DIRECTION('ref_axis',(1.,0.,0.)) ;
#46023 = DIRECTION('',(0.,0.,-1.)) ;
#46024 = DIRECTION('center_axis',(0.,0.,1.)) ;
#46025 = DIRECTION('ref_axis',(1.,0.,0.)) ;
#46026 = DIRECTION('',(0.,0.,-1.)) ;
#46027 = DIRECTION('center_axis',(0.,0.,1.)) ;
#46028 = DIRECTION('ref_axis',(1.,0.,0.)) ;
#46029 = DIRECTION('',(0.,0.,-1.)) ;
#46030 = DIRECTION('center_axis',(0.,0.,1.)) ;
#46031 = DIRECTION('ref_axis',(1.,0.,0.)) ;
#46032 = DIRECTION('',(0.,0.,-1.)) ;
#46033 = DIRECTION('center_axis',(0.,0.,1.)) ;
#46034 = DIRECTION('ref_axis',(1.,0.,0.)) ;
#46035 = DIRECTION('',(0.,0.,-1.)) ;
#46036 = DIRECTION('center_axis',(0.,0.,1.)) ;
#46037 = DIRECTION('ref_axis',(1.,0.,0.)) ;
#46038 = DIRECTION('',(0.,0.,-1.)) ;
#46039 = DIRECTION('center_axis',(0.,0.,1.)) ;
#46040 = DIRECTION('ref_axis',(1.,0.,0.)) ;
#46041 = DIRECTION('',(0.,0.,-1.)) ;
#46042 = DIRECTION('center_axis',(0.,0.,1.)) ;
#46043 = DIRECTION('ref_axis',(1.,0.,0.)) ;
#46044 = DIRECTION('center_axis',(0.,0.,1.)) ;
#46045 = DIRECTION('ref_axis',(1.,0.,0.)) ;
#46046 = DIRECTION('',(0.,0.,-1.)) ;
#46047 = DIRECTION('center_axis',(0.,0.,1.)) ;
#46048 = DIRECTION('ref_axis',(1.,0.,0.)) ;
#46049 = DIRECTION('',(0.,0.,-1.)) ;
#46050 = DIRECTION('center_axis',(0.,0.,1.)) ;
#46051 = DIRECTION('ref_axis',(1.,0.,0.)) ;
#46052 = DIRECTION('',(0.,0.,-1.)) ;
#46053 = DIRECTION('center_axis',(0.,0.,1.)) ;
#46054 = DIRECTION('ref_axis',(1.,0.,0.)) ;
#46055 = DIRECTION('',(0.,0.,-1.)) ;
#46056 = DIRECTION('center_axis',(0.,0.,1.)) ;
#46057 = DIRECTION('ref_axis',(1.,0.,0.)) ;
#46058 = DIRECTION('',(0.,0.,-1.)) ;
#46059 = DIRECTION('center_axis',(0.,0.,1.)) ;
#46060 = DIRECTION('ref_axis',(1.,0.,0.)) ;
#46061 = DIRECTION('',(0.,0.,-1.)) ;
#46062 = DIRECTION('center_axis',(0.,0.,1.)) ;
#46063 = DIRECTION('ref_axis',(1.,0.,0.)) ;
#46064 = DIRECTION('',(0.,0.,-1.)) ;
#46065 = DIRECTION('center_axis',(0.,0.,1.)) ;
#46066 = DIRECTION('ref_axis',(1.,0.,0.)) ;
#46067 = DIRECTION('',(0.,0.,-1.)) ;
#46068 = DIRECTION('center_axis',(0.,0.,1.)) ;
#46069 = DIRECTION('ref_axis',(1.,0.,0.)) ;
#46070 = DIRECTION('',(0.,0.,-1.)) ;
#46071 = DIRECTION('center_axis',(0.,0.,1.)) ;
#46072 = DIRECTION('ref_axis',(1.,0.,0.)) ;
#46073 = DIRECTION('',(0.,0.,-1.)) ;
#46074 = DIRECTION('center_axis',(0.,0.,1.)) ;
#46075 = DIRECTION('ref_axis',(1.,0.,0.)) ;
#46076 = DIRECTION('',(0.,0.,-1.)) ;
#46077 = DIRECTION('center_axis',(0.,0.,1.)) ;
#46078 = DIRECTION('ref_axis',(1.,0.,0.)) ;
#46079 = DIRECTION('',(0.,0.,-1.)) ;
#46080 = DIRECTION('center_axis',(0.,0.,1.)) ;
#46081 = DIRECTION('ref_axis',(1.,0.,0.)) ;
#46082 = DIRECTION('',(0.,0.,-1.)) ;
#46083 = DIRECTION('center_axis',(0.,0.,1.)) ;
#46084 = DIRECTION('ref_axis',(1.,0.,0.)) ;
#46085 = DIRECTION('',(0.,0.,-1.)) ;
#46086 = DIRECTION('center_axis',(0.,0.,1.)) ;
#46087 = DIRECTION('ref_axis',(1.,0.,0.)) ;
#46088 = DIRECTION('',(0.,0.,-1.)) ;
#46089 = DIRECTION('center_axis',(0.,0.,1.)) ;
#46090 = DIRECTION('ref_axis',(1.,0.,0.)) ;
#46091 = DIRECTION('',(0.707106781186544,8.65956056235489E-17,-0.707106781186551)) ;
#46092 = DIRECTION('center_axis',(0.,0.,1.)) ;
#46093 = DIRECTION('ref_axis',(1.,0.,0.)) ;
#46094 = DIRECTION('center_axis',(0.,0.,1.)) ;
#46095 = DIRECTION('ref_axis',(1.,0.,0.)) ;
#46096 = DIRECTION('center_axis',(0.,0.,1.)) ;
#46097 = DIRECTION('ref_axis',(1.,0.,0.)) ;
#46098 = DIRECTION('center_axis',(0.,0.,1.)) ;
#46099 = DIRECTION('ref_axis',(1.,0.,0.)) ;
#46100 = DIRECTION('center_axis',(0.,0.,1.)) ;
#46101 = DIRECTION('ref_axis',(1.,0.,0.)) ;
#46102 = DIRECTION('center_axis',(0.,0.,1.)) ;
#46103 = DIRECTION('ref_axis',(1.,0.,0.)) ;
#46104 = DIRECTION('center_axis',(0.,0.,1.)) ;
#46105 = DIRECTION('ref_axis',(1.,0.,0.)) ;
#46106 = DIRECTION('center_axis',(-1.37769458707663E-29,-3.94587412439991E-15,
1.)) ;
#46107 = DIRECTION('ref_axis',(6.56371136615486E-45,-1.,-3.94587412439991E-15)) ;
#46108 = DIRECTION('center_axis',(0.,0.,1.)) ;
#46109 = DIRECTION('ref_axis',(1.,0.,0.)) ;
#46110 = DIRECTION('center_axis',(-1.37769458707663E-29,-3.94587412439991E-15,
1.)) ;
#46111 = DIRECTION('ref_axis',(-4.32555501796151E-45,1.,3.94587412439991E-15)) ;
#46112 = DIRECTION('center_axis',(0.,0.,1.)) ;
#46113 = DIRECTION('ref_axis',(1.,0.,0.)) ;
#46114 = DIRECTION('center_axis',(0.,0.,1.)) ;
#46115 = DIRECTION('ref_axis',(1.,0.,0.)) ;
#46116 = DIRECTION('center_axis',(0.,0.,1.)) ;
#46117 = DIRECTION('ref_axis',(-1.,0.,0.)) ;
#46118 = DIRECTION('center_axis',(0.,-1.97293706219996E-15,1.)) ;
#46119 = DIRECTION('ref_axis',(0.,-1.,-1.77635683940025E-15)) ;
#46120 = DIRECTION('center_axis',(0.,-1.97293706219996E-15,1.)) ;
#46121 = DIRECTION('ref_axis',(0.,-1.,-1.97293706219996E-15)) ;
#46122 = DIRECTION('center_axis',(-1.,-1.22464679914735E-16,-2.41615105814236E-31)) ;
#46123 = DIRECTION('ref_axis',(-1.22464679914735E-16,1.,1.85037170770859E-15)) ;
#46124 = DIRECTION('center_axis',(0.,-1.97293706219996E-15,1.)) ;
#46125 = DIRECTION('ref_axis',(0.,-1.,-1.97293706219996E-15)) ;
#46126 = DIRECTION('center_axis',(0.,-1.97293706219996E-15,1.)) ;
#46127 = DIRECTION('ref_axis',(0.,-1.,-1.97293706219996E-15)) ;
#46128 = DIRECTION('center_axis',(-1.,1.83697019872103E-16,0.)) ;
#46129 = DIRECTION('ref_axis',(1.22464679914735E-16,1.,2.10219744307722E-15)) ;
#46130 = DIRECTION('center_axis',(0.,0.,1.)) ;
#46131 = DIRECTION('ref_axis',(-1.,7.99360577730113E-15,0.)) ;
#46132 = DIRECTION('center_axis',(-0.996194698091746,-1.55254059623772E-16,
0.0871557427476584)) ;
#46133 = DIRECTION('ref_axis',(0.0871557427476584,2.43428429401259E-33,0.996194698091746)) ;
#46134 = DIRECTION('center_axis',(-0.920363891963228,-0.381227206369645,0.0871557427476584)) ;
#46135 = DIRECTION('ref_axis',(0.382683432365081,-0.92387953251129,-5.41926931333106E-18)) ;
#46136 = DIRECTION('center_axis',(-0.381227206369648,-0.920363891963227,0.0871557427476584)) ;
#46137 = DIRECTION('ref_axis',(0.923879532511289,-0.382683432365084,-6.23920499234797E-18)) ;
#46138 = DIRECTION('center_axis',(0.,-0.996194698091746,0.0871557427476584)) ;
#46139 = DIRECTION('ref_axis',(0.,-0.0871557427476584,-0.996194698091746)) ;
#46140 = DIRECTION('center_axis',(3.49489393366845E-15,0.996194698091745,
0.0871557427476603)) ;
#46141 = DIRECTION('ref_axis',(1.18266251815146E-32,-0.0871557427476603,0.996194698091745)) ;
#46142 = DIRECTION('center_axis',(-0.381227206369642,0.920363891963229,0.0871557427476609)) ;
#46143 = DIRECTION('ref_axis',(-0.923879532511291,-0.382683432365078,-2.80799776071203E-17)) ;
#46144 = DIRECTION('center_axis',(-0.920363891963225,0.381227206369651,0.0871557427476609)) ;
#46145 = DIRECTION('ref_axis',(-0.382683432365087,-0.923879532511288,7.9370913940361E-17)) ;
#46146 = DIRECTION('center_axis',(-0.996194698091745,3.30624240319137E-15,
0.0871557427476603)) ;
#46147 = DIRECTION('ref_axis',(0.0871557427476603,1.93558059421515E-34,0.996194698091745)) ;
#46148 = DIRECTION('center_axis',(0.996194698091746,-7.14504192696067E-15,
0.0871557427476584)) ;
#46149 = DIRECTION('ref_axis',(0.0871557427476584,1.49618138940667E-31,-0.996194698091746)) ;
#46150 = DIRECTION('center_axis',(0.920363891963231,0.381227206369638,0.0871557427476599)) ;
#46151 = DIRECTION('ref_axis',(-0.382683432365074,0.923879532511293,8.60234787324834E-17)) ;
#46152 = DIRECTION('center_axis',(0.381227206369654,0.920363891963224,0.087155742747662)) ;
#46153 = DIRECTION('ref_axis',(-0.923879532511287,0.38268343236509,7.82165862635586E-17)) ;
#46154 = DIRECTION('center_axis',(6.9563903964836E-15,0.996194698091745,0.0871557427476623)) ;
#46155 = DIRECTION('ref_axis',(-7.29504144019363E-32,-0.0871557427476623,
0.996194698091745)) ;
#46156 = DIRECTION('center_axis',(-1.97293706219996E-15,-1.97293706219993E-15,
1.)) ;
#46157 = DIRECTION('ref_axis',(-1.,-8.84530818399176E-31,-1.97293706219996E-15)) ;
#46158 = DIRECTION('center_axis',(-1.0451284330152E-14,-0.996194698091746,
0.0871557427476564)) ;
#46159 = DIRECTION('ref_axis',(-3.08095231401847E-32,-0.0871557427476564,
-0.996194698091746)) ;
#46160 = DIRECTION('center_axis',(0.381227206369635,-0.920363891963232,0.0871557427476573)) ;
#46161 = DIRECTION('ref_axis',(0.923879532511294,0.382683432365071,8.31057747593213E-17)) ;
#46162 = DIRECTION('center_axis',(0.920363891963223,-0.381227206369657,0.0871557427476594)) ;
#46163 = DIRECTION('ref_axis',(0.382683432365093,0.923879532511285,-7.95739253828632E-17)) ;
#46164 = DIRECTION('center_axis',(0.996194698091745,-1.06065383897758E-14,
0.0871557427476603)) ;
#46165 = DIRECTION('ref_axis',(0.0871557427476603,-6.35553601982602E-32,-0.996194698091745)) ;
#46166 = DIRECTION('center_axis',(0.,0.,-1.)) ;
#46167 = DIRECTION('ref_axis',(-1.,0.,0.)) ;
#46168 = DIRECTION('center_axis',(0.,-1.97293706219996E-15,1.)) ;
#46169 = DIRECTION('ref_axis',(0.,-1.,-1.97293706219996E-15)) ;
#46170 = DIRECTION('',(0.,0.,1.)) ;
#46171 = DIRECTION('center_axis',(0.,-1.97293706219996E-15,1.)) ;
#46172 = DIRECTION('ref_axis',(0.,-1.,-1.97293706219996E-15)) ;
#46173 = DIRECTION('center_axis',(0.,-1.97293706219996E-15,1.)) ;
#46174 = DIRECTION('ref_axis',(0.,-1.,-1.77635683940025E-15)) ;
#46175 = DIRECTION('center_axis',(-1.,-1.22464679914735E-16,-2.41615105814236E-31)) ;
#46176 = DIRECTION('ref_axis',(-1.22464679914735E-16,1.,1.85037170770859E-15)) ;
#46177 = DIRECTION('center_axis',(0.,-1.97293706219996E-15,1.)) ;
#46178 = DIRECTION('ref_axis',(0.,-1.,-1.97293706219996E-15)) ;
#46179 = DIRECTION('center_axis',(0.,0.,-1.)) ;
#46180 = DIRECTION('ref_axis',(-1.,0.,0.)) ;
#46181 = DIRECTION('',(0.,-0.866025403784433,0.50000000000001)) ;
#46182 = DIRECTION('center_axis',(0.,0.,1.)) ;
#46183 = DIRECTION('ref_axis',(1.,0.,0.)) ;
#46184 = DIRECTION('center_axis',(0.,0.,1.)) ;
#46185 = DIRECTION('ref_axis',(1.,0.,0.)) ;
#46186 = DIRECTION('center_axis',(0.,0.,1.)) ;
#46187 = DIRECTION('ref_axis',(1.,0.,0.)) ;
#46188 = DIRECTION('center_axis',(-0.996194698091746,-1.55254059623772E-16,
0.0871557427476584)) ;
#46189 = DIRECTION('ref_axis',(0.0871557427476584,8.9940333441683E-34,0.996194698091746)) ;
#46190 = DIRECTION('',(-1.5584710490948E-16,1.,0.)) ;
#46191 = DIRECTION('',(0.0871426484044397,0.0173337504938598,0.996045029063886)) ;
#46192 = DIRECTION('center_axis',(-0.920363891963228,-0.381227206369645,0.0871557427476583)) ;
#46193 = DIRECTION('ref_axis',(0.382683432365081,-0.92387953251129,3.89840055033188E-19)) ;
#46194 = DIRECTION('',(-0.382683432365081,0.92387953251129,0.)) ;
#46195 = DIRECTION('',(0.0666626913468327,0.0666626913468325,0.995546167269401)) ;
#46196 = DIRECTION('center_axis',(-0.381227206369648,-0.920363891963227,0.0871557427476584)) ;
#46197 = DIRECTION('ref_axis',(0.923879532511289,-0.382683432365084,1.47102406971995E-19)) ;
#46198 = DIRECTION('',(-0.923879532511289,0.382683432365084,0.)) ;
#46199 = DIRECTION('',(0.0173337504938599,0.0871426484044397,0.996045029063886)) ;
#46200 = DIRECTION('center_axis',(0.,-0.996194698091746,0.0871557427476584)) ;
#46201 = DIRECTION('ref_axis',(0.,-0.0871557427476584,-0.996194698091746)) ;
#46202 = DIRECTION('',(-1.,0.,0.)) ;
#46203 = DIRECTION('center_axis',(0.,0.,1.)) ;
#46204 = DIRECTION('ref_axis',(1.,0.,0.)) ;
#46205 = DIRECTION('',(1.,-3.50824386072629E-15,0.)) ;
#46206 = DIRECTION('',(-1.0647053643322E-14,-1.,0.)) ;
#46207 = DIRECTION('',(-0.382683432365094,-0.923879532511285,0.)) ;
#46208 = DIRECTION('',(-0.923879532511294,-0.382683432365071,0.)) ;
#46209 = DIRECTION('',(-1.,1.04912065384126E-14,0.)) ;
#46210 = DIRECTION('center_axis',(0.,0.,1.)) ;
#46211 = DIRECTION('ref_axis',(1.,0.,0.)) ;
#46212 = DIRECTION('',(1.,-6.98296267768627E-15,0.)) ;
#46213 = DIRECTION('',(0.923879532511286,-0.382683432365091,0.)) ;
#46214 = DIRECTION('',(0.382683432365075,-0.923879532511293,0.)) ;
#46215 = DIRECTION('',(-7.17233482636206E-15,-1.,0.)) ;
#46216 = DIRECTION('',(3.31887171205049E-15,1.,0.)) ;
#46217 = DIRECTION('',(0.382683432365087,0.923879532511288,0.)) ;
#46218 = DIRECTION('',(0.923879532511292,0.382683432365078,0.)) ;
#46219 = DIRECTION('center_axis',(3.49489393366845E-15,0.996194698091745,
0.0871557427476603)) ;
#46220 = DIRECTION('ref_axis',(6.11304317578278E-32,-0.0871557427476603,0.996194698091745)) ;
#46221 = DIRECTION('',(0.0173337504938615,-0.0871426484044417,0.996045029063885)) ;
#46222 = DIRECTION('center_axis',(-0.381227206369642,0.920363891963229,0.0871557427476609)) ;
#46223 = DIRECTION('ref_axis',(-0.923879532511292,-0.382683432365078,-6.27744471266564E-17)) ;
#46224 = DIRECTION('',(0.0666626913468342,-0.0666626913468348,0.995546167269401)) ;
#46225 = DIRECTION('center_axis',(-0.920363891963225,0.381227206369651,0.0871557427476609)) ;
#46226 = DIRECTION('ref_axis',(-0.382683432365087,-0.923879532511288,7.9370913940361E-17)) ;
#46227 = DIRECTION('',(0.0871426484044416,-0.0173337504938622,0.996045029063885)) ;
#46228 = DIRECTION('center_axis',(-0.996194698091745,3.30624240319137E-15,
0.0871557427476603)) ;
#46229 = DIRECTION('ref_axis',(0.0871557427476603,4.93097487664857E-32,0.996194698091745)) ;
#46230 = DIRECTION('center_axis',(0.996194698091746,-7.14504192696067E-15,
0.0871557427476584)) ;
#46231 = DIRECTION('ref_axis',(0.0871557427476584,2.47850520354795E-31,-0.996194698091746)) ;
#46232 = DIRECTION('',(-0.0871426484044398,-0.0173337504938632,0.996045029063886)) ;
#46233 = DIRECTION('center_axis',(0.920363891963231,0.381227206369638,0.0871557427476598)) ;
#46234 = DIRECTION('ref_axis',(-0.382683432365074,0.923879532511293,8.02510185058152E-17)) ;
#46235 = DIRECTION('',(-0.0666626913468331,-0.0666626913468359,0.995546167269401)) ;
#46236 = DIRECTION('center_axis',(0.381227206369654,0.920363891963224,0.087155742747662)) ;
#46237 = DIRECTION('ref_axis',(-0.923879532511287,0.38268343236509,7.82165862635586E-17)) ;
#46238 = DIRECTION('',(-0.0173337504938606,-0.0871426484044434,0.996045029063885)) ;
#46239 = DIRECTION('center_axis',(6.9563903964836E-15,0.996194698091745,0.0871557427476623)) ;
#46240 = DIRECTION('ref_axis',(2.56571987506902E-32,-0.0871557427476623,0.996194698091745)) ;
#46241 = DIRECTION('center_axis',(-1.97293706219996E-15,-1.97293706219993E-15,
1.)) ;
#46242 = DIRECTION('ref_axis',(-1.,1.6109676234517E-14,-1.97293706219993E-15)) ;
#46243 = DIRECTION('center_axis',(-1.0451284330152E-14,-0.996194698091746,
0.0871557427476564)) ;
#46244 = DIRECTION('ref_axis',(-3.08095231401847E-32,-0.0871557427476564,
-0.996194698091746)) ;
#46245 = DIRECTION('',(-0.0173337504938609,0.0871426484044379,0.996045029063886)) ;
#46246 = DIRECTION('center_axis',(0.381227206369635,-0.920363891963232,0.0871557427476573)) ;
#46247 = DIRECTION('ref_axis',(0.923879532511295,0.382683432365071,-2.87769700566421E-17)) ;
#46248 = DIRECTION('',(-0.0666626913468338,0.0666626913468314,0.995546167269401)) ;
#46249 = DIRECTION('center_axis',(0.920363891963223,-0.381227206369657,0.0871557427476594)) ;
#46250 = DIRECTION('ref_axis',(0.382683432365093,0.923879532511285,-7.2635031478956E-17)) ;
#46251 = DIRECTION('',(-0.0871426484044414,0.0173337504938589,0.996045029063885)) ;
#46252 = DIRECTION('center_axis',(0.996194698091745,-1.06065383897758E-14,
0.0871557427476603)) ;
#46253 = DIRECTION('ref_axis',(0.0871557427476603,-6.35553601982602E-32,-0.996194698091745)) ;
#46254 = DIRECTION('axis',(0.,0.,1.)) ;
#46255 = DIRECTION('refdir',(1.,0.,0.)) ;
#46256 = DIRECTION('center_axis',(1.,-1.05932475323295E-29,0.)) ;
#46257 = DIRECTION('ref_axis',(0.,0.,-1.)) ;
#46258 = DIRECTION('',(-1.05932475323295E-29,-1.,-1.26161707343768E-16)) ;
#46259 = DIRECTION('',(0.,0.,-1.)) ;
#46260 = DIRECTION('',(1.05932475323295E-29,1.,0.)) ;
#46261 = DIRECTION('',(0.,0.,1.)) ;
#46262 = DIRECTION('center_axis',(0.998026231470406,-0.0627984088423271,3.38208872241338E-5)) ;
#46263 = DIRECTION('ref_axis',(0.0627984088782431,0.998026232041203,3.08440021028225E-21)) ;
#46264 = DIRECTION('',(0.0627984089100395,0.998026232038757,-9.42827069380898E-7)) ;
#46265 = DIRECTION('',(3.37541238321067E-5,-2.12403789334292E-6,-0.999999999428074)) ;
#46266 = DIRECTION('',(-0.0628002171619293,-0.998026118257246,8.88096292981396E-7)) ;
#46267 = DIRECTION('',(-3.37541272928291E-5,2.12398289397303E-6,0.999999999428074)) ;
#46268 = DIRECTION('center_axis',(0.,0.,1.)) ;
#46269 = DIRECTION('ref_axis',(-0.0314147095637551,-0.999506436208904,0.)) ;
#46270 = DIRECTION('axis',(0.,0.,1.)) ;
#46271 = DIRECTION('refdir',(1.,0.,0.)) ;
#46272 = DIRECTION('center_axis',(0.,0.,1.)) ;
#46273 = DIRECTION('ref_axis',(1.,0.,0.)) ;
#46274 = DIRECTION('center_axis',(0.,0.,-1.)) ;
#46275 = DIRECTION('ref_axis',(1.,0.,0.)) ;
#46276 = DIRECTION('center_axis',(1.22464679914735E-16,-1.,0.)) ;
#46277 = DIRECTION('ref_axis',(-1.,-1.22464679914735E-16,0.)) ;
#46278 = DIRECTION('center_axis',(0.,0.,1.)) ;
#46279 = DIRECTION('ref_axis',(1.,0.,0.)) ;
#46280 = DIRECTION('center_axis',(0.,0.,1.)) ;
#46281 = DIRECTION('ref_axis',(1.,0.,0.)) ;
#46282 = DIRECTION('center_axis',(0.,0.,-1.)) ;
#46283 = DIRECTION('ref_axis',(-1.,0.,0.)) ;
#46284 = DIRECTION('center_axis',(0.,0.,-1.)) ;
#46285 = DIRECTION('ref_axis',(1.,0.,0.)) ;
#46286 = DIRECTION('center_axis',(0.,0.,-1.)) ;
#46287 = DIRECTION('ref_axis',(1.,0.,0.)) ;
#46288 = DIRECTION('',(0.,0.,1.)) ;
#46289 = DIRECTION('center_axis',(0.,0.,1.)) ;
#46290 = DIRECTION('ref_axis',(1.,0.,0.)) ;
#46291 = DIRECTION('center_axis',(0.,0.,1.)) ;
#46292 = DIRECTION('ref_axis',(1.,0.,0.)) ;
#46293 = DIRECTION('center_axis',(0.,0.,1.)) ;
#46294 = DIRECTION('ref_axis',(1.,0.,0.)) ;
#46295 = DIRECTION('center_axis',(1.22464679914735E-16,-1.,0.)) ;
#46296 = DIRECTION('ref_axis',(-1.,-1.22464679914735E-16,0.)) ;
#46297 = DIRECTION('center_axis',(0.,0.,1.)) ;
#46298 = DIRECTION('ref_axis',(1.,0.,0.)) ;
#46299 = DIRECTION('center_axis',(0.,0.,1.)) ;
#46300 = DIRECTION('ref_axis',(1.,0.,0.)) ;
#46301 = DIRECTION('center_axis',(0.,0.,1.)) ;
#46302 = DIRECTION('ref_axis',(1.,0.,0.)) ;
#46303 = DIRECTION('center_axis',(0.,0.,-1.)) ;
#46304 = DIRECTION('ref_axis',(-1.,0.,0.)) ;
#46305 = DIRECTION('',(0.,0.,-1.)) ;
#46306 = DIRECTION('',(-1.43938396903601E-5,0.999999999896409,2.16758776537448E-14)) ;
#46307 = DIRECTION('',(-0.999999999896409,-1.43938396903601E-5,1.76246149557724E-13)) ;
#46308 = DIRECTION('',(-1.43938396633383E-5,0.999999999896409,2.13219940646407E-14)) ;
#46309 = DIRECTION('',(-1.73392724841599E-13,2.1319498279769E-14,-1.)) ;
#46310 = DIRECTION('',(1.43938396904894E-5,-0.999999999896409,-2.13358718524534E-14)) ;
#46311 = DIRECTION('',(0.999999999896409,1.43938396904894E-5,-1.75646404491289E-13)) ;
#46312 = DIRECTION('',(-1.43938396903601E-5,0.999999999896409,2.16758776537448E-14)) ;
#46313 = DIRECTION('',(-0.999999999896409,-1.43938396903601E-5,1.76246149557723E-13)) ;
#46314 = DIRECTION('',(-1.43938396633382E-5,0.999999999896409,2.13219940646407E-14)) ;
#46315 = DIRECTION('',(-1.73392724841598E-13,2.1319498279769E-14,-1.)) ;
#46316 = DIRECTION('',(1.43938396904895E-5,-0.999999999896409,-2.13358718524532E-14)) ;
#46317 = DIRECTION('',(0.999999999896409,1.43938396904895E-5,-1.7564640449129E-13)) ;
#46318 = DIRECTION('',(-1.43938396903601E-5,0.999999999896409,2.16758776537447E-14)) ;
#46319 = DIRECTION('',(-0.999999999896409,-1.43938396903601E-5,1.76246149557724E-13)) ;
#46320 = DIRECTION('',(-1.43938396633383E-5,0.999999999896409,2.13219940646406E-14)) ;
#46321 = DIRECTION('',(-1.73392724841599E-13,2.13194982797689E-14,-1.)) ;
#46322 = DIRECTION('',(1.43938396904895E-5,-0.999999999896409,-2.13358718524534E-14)) ;
#46323 = DIRECTION('',(0.999999999896409,1.43938396904895E-5,-1.75646404491289E-13)) ;
#46324 = DIRECTION('',(-1.439383969036E-5,0.999999999896409,2.16758776537447E-14)) ;
#46325 = DIRECTION('',(-0.999999999896409,-1.439383969036E-5,1.76246149557725E-13)) ;
#46326 = DIRECTION('',(-1.43938396633384E-5,0.999999999896409,2.13219940646406E-14)) ;
#46327 = DIRECTION('',(-1.73392724841601E-13,2.13194982797689E-14,-1.)) ;
#46328 = DIRECTION('',(1.43938396904895E-5,-0.999999999896409,-2.13358718524534E-14)) ;
#46329 = DIRECTION('',(0.999999999896409,1.43938396904895E-5,-1.7564640449129E-13)) ;
#46330 = DIRECTION('',(-5.34756645401728E-28,1.,-2.90739654573715E-15)) ;
#46331 = DIRECTION('',(-1.,-2.40488946225695E-29,1.75658099177411E-13)) ;
#46332 = DIRECTION('',(1.55474962365097E-42,-3.94430452610506E-31,1.)) ;
#46333 = DIRECTION('',(1.,9.72346137283751E-63,-1.55474962365097E-42)) ;
#46334 = DIRECTION('',(-1.75646404491189E-13,2.44095865938055E-14,1.)) ;
#46335 = DIRECTION('',(0.999999999896409,-1.439383964507E-5,1.75646755820669E-13)) ;
#46336 = DIRECTION('',(-1.75646404491192E-13,2.4409586593805E-14,1.)) ;
#46337 = DIRECTION('',(0.999999999896409,-1.43938396444593E-5,1.75646755820672E-13)) ;
#46338 = DIRECTION('',(-1.75646402693562E-13,2.61344833787267E-14,1.)) ;
#46339 = DIRECTION('',(0.999999999896409,-1.439383964507E-5,1.75646778850929E-13)) ;
#46340 = DIRECTION('',(-1.7808889514537E-13,2.77741754673589E-14,1.)) ;
#46341 = DIRECTION('',(0.999999999896409,-1.43938396456804E-5,1.78089294903949E-13)) ;
#46342 = DIRECTION('',(0.,0.,1.)) ;
#46343 = DIRECTION('',(1.,0.,0.)) ;
#46344 = DIRECTION('',(1.75408298996871E-13,1.,-2.90739654573714E-15)) ;
#46345 = DIRECTION('',(-1.,1.75408298996871E-13,-4.93057902841558E-28)) ;
#46346 = CARTESIAN_POINT('',(0.,0.,0.)) ;
#46347 = CARTESIAN_POINT('',(0.,0.,0.)) ;
#46348 = CARTESIAN_POINT('',(0.,0.,0.)) ;
#46349 = CARTESIAN_POINT('Origin',(209.138527625422,615.860565160531,-20.372160171761)) ;
#46350 = CARTESIAN_POINT('',(196.738527625422,616.110565160533,-20.3721601717605)) ;
#46351 = CARTESIAN_POINT('',(196.738527625422,615.860565160533,-20.1221601717605)) ;
#46352 = CARTESIAN_POINT('Origin',(196.738527625422,615.860565160533,-20.3721601717605)) ;
#46353 = CARTESIAN_POINT('',(0.238527625422233,615.860565160567,-20.1221601717516)) ;
#46354 = CARTESIAN_POINT('',(209.138527625422,615.860565160531,-20.122160171761)) ;
#46355 = CARTESIAN_POINT('',(0.23852762542226,616.110565160567,-20.3721601717515)) ;
#46356 = CARTESIAN_POINT('Origin',(0.238527625422229,615.860565160567,-20.3721601717515)) ;
#46357 = CARTESIAN_POINT('',(209.138527625422,616.110565160531,-20.372160171761)) ;
#46358 = CARTESIAN_POINT('Origin',(205.888527625422,616.210565160531,-20.1221601717609)) ;
#46359 = CARTESIAN_POINT('',(196.738527625403,506.560565160533,-20.1221601717605)) ;
#46360 = CARTESIAN_POINT('',(196.738527625422,616.210565160533,-20.1221601717605)) ;
#46361 = CARTESIAN_POINT('',(0.238527625403034,506.560565160567,-20.1221601717516)) ;
#46362 = CARTESIAN_POINT('',(209.138527625403,506.560565160531,-20.1221601717611)) ;
#46363 = CARTESIAN_POINT('',(0.2385276254034,508.710565160567,-20.1221601717516)) ;
#46364 = CARTESIAN_POINT('',(0.238527625422229,615.835565160567,-20.1221601717516)) ;
#46365 = CARTESIAN_POINT('',(0.238527625421856,613.710565160567,-20.1221601717515)) ;
#46366 = CARTESIAN_POINT('',(0.238527625417512,588.710565160567,-20.1221601717516)) ;
#46367 = CARTESIAN_POINT('',(0.238527625422229,615.835565160567,-20.1221601717516)) ;
#46368 = CARTESIAN_POINT('',(68.1896090740378,536.698209005427,-20.1221601717547)) ;
#46369 = CARTESIAN_POINT('',(48.6516101218399,517.160211426462,-20.1221601717564)) ;
#46370 = CARTESIAN_POINT('Origin',(44.9784504245142,540.371370334153,-20.1221601717596)) ;
#46371 = CARTESIAN_POINT('',(49.433135115108,512.221667239673,-20.1221601717538)) ;
#46372 = CARTESIAN_POINT('Ctrl Pts',(49.4331351151386,512.22166723948,-20.1221601717538)) ;
#46373 = CARTESIAN_POINT('Ctrl Pts',(49.0637330002203,512.163209431222,-20.122160171973)) ;
#46374 = CARTESIAN_POINT('Ctrl Pts',(47.9122384134768,512.229997790623,-20.1221601726336)) ;
#46375 = CARTESIAN_POINT('Ctrl Pts',(46.385300085782,513.6230574364,-20.1221601733896)) ;
#46376 = CARTESIAN_POINT('Ctrl Pts',(46.5550515020585,516.100143194611,-20.1221601730646)) ;
#46377 = CARTESIAN_POINT('Ctrl Pts',(47.91280440288,517.043294655983,-20.1221601721921)) ;
#46378 = CARTESIAN_POINT('Ctrl Pts',(48.6516084909445,517.16021116837,-20.1221601717537)) ;
#46379 = CARTESIAN_POINT('',(73.1281534675486,535.916685318467,-20.1221601717549)) ;
#46380 = CARTESIAN_POINT('Origin',(44.9784504245142,540.371370334153,-20.1221601717536)) ;
#46381 = CARTESIAN_POINT('Origin',(70.6588812706952,536.307447161957,-20.1221601717603)) ;
#46382 = CARTESIAN_POINT('',(16.8287456930678,535.916695987763,-20.1221601717523)) ;
#46383 = CARTESIAN_POINT('',(21.7672748307833,536.698316071089,-20.122160171752)) ;
#46384 = CARTESIAN_POINT('Ctrl Pts',(16.8287456930845,535.916695987658,-20.1221601717523)) ;
#46385 = CARTESIAN_POINT('Ctrl Pts',(16.7702887385344,536.286093587143,-20.1221601717711)) ;
#46386 = CARTESIAN_POINT('Ctrl Pts',(16.8370747519972,537.437573131114,-20.1221601718281)) ;
#46387 = CARTESIAN_POINT('Ctrl Pts',(18.2300981773897,538.964503729432,-20.1221601718931)) ;
#46388 = CARTESIAN_POINT('Ctrl Pts',(20.7071515274629,538.7948086885,-20.1221601718654)) ;
#46389 = CARTESIAN_POINT('Ctrl Pts',(21.6503315190709,537.437106616922,-20.1221601717903)) ;
#46390 = CARTESIAN_POINT('Ctrl Pts',(21.7672748296711,536.698316071321,-20.1221601717526)) ;
#46391 = CARTESIAN_POINT('',(40.523765408828,512.221667291119,-20.1221601717534)) ;
#46392 = CARTESIAN_POINT('Origin',(44.9784504245142,540.371370334153,-20.1221601717536)) ;
#46393 = CARTESIAN_POINT('',(41.3052890957878,517.16021168463,-20.1221601717534)) ;
#46394 = CARTESIAN_POINT('Origin',(40.9145272523186,514.690939487972,-20.1221601717542)) ;
#46395 = CARTESIAN_POINT('Origin',(44.9784504245141,540.371370334153,-20.1221601717517)) ;
#46396 = CARTESIAN_POINT('',(40.5237715662164,568.521074351592,-20.1221601670422)) ;
#46397 = CARTESIAN_POINT('',(41.3053508856094,563.582538762398,-20.1221601670332)) ;
#46398 = CARTESIAN_POINT('Origin',(40.9145328695252,566.051802069454,-20.1221601615182)) ;
#46399 = CARTESIAN_POINT('',(16.8287473814797,544.826055349839,-20.1221601717523)) ;
#46400 = CARTESIAN_POINT('Origin',(44.9784504245142,540.371370334153,-20.1221601717536)) ;
#46401 = CARTESIAN_POINT('',(21.7672917749906,544.04453166288,-20.1221601717525)) ;
#46402 = CARTESIAN_POINT('Origin',(19.2980195783332,544.435293506349,-20.1221601717457)) ;
#46403 = CARTESIAN_POINT('Origin',(44.9784504245142,540.371370334153,-20.1221601717476)) ;
#46404 = CARTESIAN_POINT('',(31.8295857683878,532.164217462742,-20.122160171753)) ;
#46405 = CARTESIAN_POINT('',(31.8295857683906,548.578523205569,-20.122160171753)) ;
#46406 = CARTESIAN_POINT('Origin',(44.978450424514,540.371370334153,-20.1221601717575)) ;
#46407 = CARTESIAN_POINT('',(26.7397026756955,551.755485607418,-20.1221601717528)) ;
#46408 = CARTESIAN_POINT('Origin',(29.284644222043,550.167004406493,-20.1221601717549)) ;
#46409 = CARTESIAN_POINT('',(26.7397026756915,528.987255060894,-20.1221601717528)) ;
#46410 = CARTESIAN_POINT('Origin',(44.978450424514,540.371370334153,-20.1221601717575)) ;
#46411 = CARTESIAN_POINT('Origin',(29.2846442220397,530.575736261818,-20.1221601717601)) ;
#46412 = CARTESIAN_POINT('',(158.588527625415,572.710565160539,-20.1221601717588)) ;
#46413 = CARTESIAN_POINT('',(158.588527625419,594.710565160539,-20.1221601717587)) ;
#46414 = CARTESIAN_POINT('',(158.58852762542,605.460565160539,-20.1221601717588)) ;
#46415 = CARTESIAN_POINT('',(161.588527625415,572.710565160539,-20.1221601717589)) ;
#46416 = CARTESIAN_POINT('Origin',(160.088527625415,572.710565160539,-20.1221601717588)) ;
#46417 = CARTESIAN_POINT('',(161.588527625419,594.710565160539,-20.1221601717589)) ;
#46418 = CARTESIAN_POINT('',(161.588527625419,594.460565160539,-20.1221601717589)) ;
#46419 = CARTESIAN_POINT('Origin',(160.088527625419,594.710565160539,-20.1221601717588)) ;
#46420 = CARTESIAN_POINT('',(165.588527625415,572.710565160538,-20.1221601717591)) ;
#46421 = CARTESIAN_POINT('',(165.588527625419,594.710565160538,-20.1221601717591)) ;
#46422 = CARTESIAN_POINT('',(165.58852762542,605.460565160538,-20.1221601717591)) ;
#46423 = CARTESIAN_POINT('',(168.588527625415,572.710565160538,-20.1221601717592)) ;
#46424 = CARTESIAN_POINT('Origin',(167.088527625415,572.710565160538,-20.1221601717592)) ;
#46425 = CARTESIAN_POINT('',(168.588527625419,594.710565160538,-20.1221601717592)) ;
#46426 = CARTESIAN_POINT('',(168.588527625419,594.460565160538,-20.1221601717592)) ;
#46427 = CARTESIAN_POINT('Origin',(167.088527625419,594.710565160538,-20.1221601717591)) ;
#46428 = CARTESIAN_POINT('',(172.588527625415,572.710565160537,-20.1221601717594)) ;
#46429 = CARTESIAN_POINT('',(172.588527625419,594.710565160537,-20.1221601717594)) ;
#46430 = CARTESIAN_POINT('',(172.58852762542,605.460565160537,-20.1221601717594)) ;
#46431 = CARTESIAN_POINT('',(175.588527625415,572.710565160536,-20.1221601717595)) ;
#46432 = CARTESIAN_POINT('Origin',(174.088527625415,572.710565160537,-20.1221601717595)) ;
#46433 = CARTESIAN_POINT('',(175.588527625419,594.710565160536,-20.1221601717595)) ;
#46434 = CARTESIAN_POINT('',(175.588527625419,594.460565160536,-20.1221601717595)) ;
#46435 = CARTESIAN_POINT('Origin',(174.088527625419,594.710565160537,-20.1221601717594)) ;
#46436 = CARTESIAN_POINT('',(158.588527625407,527.710565160539,-20.1221601717588)) ;
#46437 = CARTESIAN_POINT('',(158.588527625411,549.710565160539,-20.1221601717588)) ;
#46438 = CARTESIAN_POINT('',(158.588527625417,582.960565160539,-20.1221601717588)) ;
#46439 = CARTESIAN_POINT('',(161.588527625407,527.710565160539,-20.1221601717589)) ;
#46440 = CARTESIAN_POINT('Origin',(160.088527625407,527.710565160539,-20.1221601717588)) ;
#46441 = CARTESIAN_POINT('',(161.588527625411,549.710565160539,-20.1221601717589)) ;
#46442 = CARTESIAN_POINT('',(161.588527625415,571.960565160539,-20.1221601717589)) ;
#46443 = CARTESIAN_POINT('Origin',(160.088527625411,549.710565160539,-20.1221601717588)) ;
#46444 = CARTESIAN_POINT('',(168.588527625411,549.710565160538,-20.1221601717592)) ;
#46445 = CARTESIAN_POINT('',(168.588527625407,527.710565160538,-20.1221601717592)) ;
#46446 = CARTESIAN_POINT('',(168.588527625415,571.960565160538,-20.1221601717592)) ;
#46447 = CARTESIAN_POINT('',(165.588527625411,549.710565160538,-20.1221601717591)) ;
#46448 = CARTESIAN_POINT('Origin',(167.088527625411,549.710565160538,-20.1221601717592)) ;
#46449 = CARTESIAN_POINT('',(165.588527625407,527.710565160538,-20.1221601717591)) ;
#46450 = CARTESIAN_POINT('',(165.588527625416,582.960565160538,-20.1221601717591)) ;
#46451 = CARTESIAN_POINT('Origin',(167.088527625407,527.710565160538,-20.1221601717592)) ;
#46452 = CARTESIAN_POINT('',(172.588527625407,527.710565160537,-20.1221601717594)) ;
#46453 = CARTESIAN_POINT('',(172.588527625411,549.710565160537,-20.1221601717594)) ;
#46454 = CARTESIAN_POINT('',(172.588527625417,582.960565160537,-20.1221601717594)) ;
#46455 = CARTESIAN_POINT('',(175.588527625407,527.710565160536,-20.1221601717595)) ;
#46456 = CARTESIAN_POINT('Origin',(174.088527625407,527.710565160537,-20.1221601717595)) ;
#46457 = CARTESIAN_POINT('',(175.588527625411,549.710565160536,-20.1221601717595)) ;
#46458 = CARTESIAN_POINT('',(175.588527625415,571.960565160536,-20.1221601717595)) ;
#46459 = CARTESIAN_POINT('Origin',(174.088527625411,549.710565160537,-20.1221601717595)) ;
#46460 = CARTESIAN_POINT('',(67.9918523583144,515.591787908231,-20.1221601717546)) ;
#46461 = CARTESIAN_POINT('Origin',(69.8918523583194,515.59178790823,-20.1221601717547)) ;
#46462 = CARTESIAN_POINT('',(17.9918523583232,565.591787908239,-20.1221601717524)) ;
#46463 = CARTESIAN_POINT('Origin',(19.8918523583282,565.591787908239,-20.1221601717525)) ;
#46464 = CARTESIAN_POINT('',(43.5689387445144,545.577405470032,-20.1221601717535)) ;
#46465 = CARTESIAN_POINT('Origin',(44.9831523068878,546.991619032404,-20.1221601717536)) ;
#46466 = CARTESIAN_POINT('',(37.0744829388653,539.087651546757,-20.1221601717532)) ;
#46467 = CARTESIAN_POINT('Origin',(38.4886965012387,540.50186510913,-20.1221601717533)) ;
#46468 = CARTESIAN_POINT('',(43.5642368621325,532.593195741101,-20.1221601717535)) ;
#46469 = CARTESIAN_POINT('Origin',(44.9784504245058,534.007409303474,-20.1221601717536)) ;
#46470 = CARTESIAN_POINT('',(50.0586926677957,539.082949664375,-20.1221601717538)) ;
#46471 = CARTESIAN_POINT('Origin',(51.472906230169,540.497163226748,-20.1221601717539)) ;
#46472 = CARTESIAN_POINT('',(33.5943351512492,522.132622585335,-20.1221601717531)) ;
#46473 = CARTESIAN_POINT('',(36.7712975530989,527.22250567803,-20.1221601717532)) ;
#46474 = CARTESIAN_POINT('Origin',(35.1828163521739,524.677564131682,-20.1221601717657)) ;
#46475 = CARTESIAN_POINT('',(56.3625656977731,522.13262258533,-20.1221601717541)) ;
#46476 = CARTESIAN_POINT('Origin',(44.9784504245142,540.371370334153,-20.1221601717645)) ;
#46477 = CARTESIAN_POINT('',(53.1856032959252,527.222505678027,-20.122160171754)) ;
#46478 = CARTESIAN_POINT('Origin',(54.774084496849,524.677564131679,-20.1221601717641)) ;
#46479 = CARTESIAN_POINT('Origin',(44.9784504245142,540.371370334153,-20.1221601717645)) ;
#46480 = CARTESIAN_POINT('',(63.2171981733329,528.987255060888,-20.1221601717544)) ;
#46481 = CARTESIAN_POINT('',(58.1273150806378,532.164217462738,-20.1221601717542)) ;
#46482 = CARTESIAN_POINT('Origin',(60.6722566269853,530.575736261813,-20.1221601717544)) ;
#46483 = CARTESIAN_POINT('',(63.2171981733369,551.755485607412,-20.1221601717544)) ;
#46484 = CARTESIAN_POINT('Origin',(44.9784504245143,540.371370334153,-20.1221601717496)) ;
#46485 = CARTESIAN_POINT('',(58.1273150806405,548.578523205564,-20.1221601717542)) ;
#46486 = CARTESIAN_POINT('Origin',(60.6722566269887,550.167004406488,-20.1221601717483)) ;
#46487 = CARTESIAN_POINT('Origin',(44.9784504245143,540.371370334153,-20.1221601717496)) ;
#46488 = CARTESIAN_POINT('',(56.3625656977793,558.610118082972,-20.1221601717541)) ;
#46489 = CARTESIAN_POINT('',(53.1856032959296,553.520234990277,-20.122160171754)) ;
#46490 = CARTESIAN_POINT('Origin',(54.7740844968544,556.065176536624,-20.1221601717435)) ;
#46491 = CARTESIAN_POINT('',(33.5943351512553,558.610118082976,-20.1221601717531)) ;
#46492 = CARTESIAN_POINT('Origin',(44.9784504245142,540.371370334153,-20.1221601717427)) ;
#46493 = CARTESIAN_POINT('',(36.7712975531032,553.52023499028,-20.1221601717532)) ;
#46494 = CARTESIAN_POINT('Origin',(35.1828163521793,556.065176536628,-20.1221601717442)) ;
#46495 = CARTESIAN_POINT('Origin',(44.9784504245142,540.371370334153,-20.1221601717427)) ;
#46496 = CARTESIAN_POINT('',(48.6516117532405,563.582528983677,-20.1221601717538)) ;
#46497 = CARTESIAN_POINT('',(68.189609074102,544.044531662882,-20.1221601728767)) ;
#46498 = CARTESIAN_POINT('Origin',(44.9784504245142,540.371370334153,-20.1221601717555)) ;
#46499 = CARTESIAN_POINT('',(73.1281535186845,544.826055026706,-20.1221601728761)) ;
#46500 = CARTESIAN_POINT('Origin',(70.6588813175355,544.435293211616,-20.1221601742775)) ;
#46501 = CARTESIAN_POINT('',(49.4331354401999,568.521073377188,-20.1221601717538)) ;
#46502 = CARTESIAN_POINT('Origin',(44.9784504245142,540.371370334153,-20.1221601717536)) ;
#46503 = CARTESIAN_POINT('Origin',(49.0423735967098,566.051801180334,-20.1221601717518)) ;
#46504 = CARTESIAN_POINT('Origin',(0.238527625417501,588.710565160567,-20.3721601717516)) ;
#46505 = CARTESIAN_POINT('',(-0.0114723745781272,613.710565160567,-20.3721601717515)) ;
#46506 = CARTESIAN_POINT('Origin',(0.238527625421892,613.710565160567,-20.3721601717515)) ;
#46507 = CARTESIAN_POINT('',(-0.0114723745965713,508.710565160567,-20.3721601717516)) ;
#46508 = CARTESIAN_POINT('Origin',(0.238527625403448,508.710565160567,-20.3721601717516)) ;
#46509 = CARTESIAN_POINT('',(-0.0114723745825186,588.710565160567,-20.3721601717515)) ;
#46510 = CARTESIAN_POINT('Origin',(209.138527625403,506.560565160531,-20.3721601717611)) ;
#46511 = CARTESIAN_POINT('',(196.738527625403,506.310565160533,-20.3721601717605)) ;
#46512 = CARTESIAN_POINT('Origin',(196.738527625403,506.560565160533,-20.3721601717605)) ;
#46513 = CARTESIAN_POINT('',(0.238527625402987,506.310565160567,-20.3721601717516)) ;
#46514 = CARTESIAN_POINT('',(209.138527625403,506.310565160531,-20.3721601717611)) ;
#46515 = CARTESIAN_POINT('Origin',(0.238527625403044,506.560565160567,-20.3721601717516)) ;
#46516 = CARTESIAN_POINT('Origin',(212.388527625401,506.31056516053,-69.5221601717612)) ;
#46517 = CARTESIAN_POINT('',(196.738527625403,506.310565160533,-23.5221601717605)) ;
#46518 = CARTESIAN_POINT('',(196.738527625402,506.310565160533,-44.5221601717605)) ;
#46519 = CARTESIAN_POINT('',(196.238527625403,506.310565160533,-24.0221601717605)) ;
#46520 = CARTESIAN_POINT('Origin',(196.238527625403,506.310565160533,-23.5221601717605)) ;
#46521 = CARTESIAN_POINT('',(193.388264603403,506.310565160533,-24.0221601717603)) ;
#46522 = CARTESIAN_POINT('',(203.313527625403,506.310565160532,-24.0221601717608)) ;
#46523 = CARTESIAN_POINT('',(192.388264603403,506.310565160534,-25.0221601717604)) ;
#46524 = CARTESIAN_POINT('Origin',(193.388264603403,506.310565160533,-25.0221601717604)) ;
#46525 = CARTESIAN_POINT('',(192.388264603403,506.310565160534,-27.5221601717603)) ;
#46526 = CARTESIAN_POINT('',(192.388264603403,506.310565160534,-46.7721601717608)) ;
#46527 = CARTESIAN_POINT('',(191.388264603403,506.310565160534,-28.5221601717603)) ;
#46528 = CARTESIAN_POINT('Origin',(191.388264603403,506.310565160534,-27.5221601717603)) ;
#46529 = CARTESIAN_POINT('',(183.388264603403,506.310565160535,-28.5221601717599)) ;
#46530 = CARTESIAN_POINT('',(205.813527625403,506.310565160531,-28.5221601717609)) ;
#46531 = CARTESIAN_POINT('',(182.388264603403,506.310565160535,-27.5221601717599)) ;
#46532 = CARTESIAN_POINT('Origin',(183.388264603403,506.310565160535,-27.5221601717599)) ;
#46533 = CARTESIAN_POINT('',(182.388264603403,506.310565160535,-25.0221601717598)) ;
#46534 = CARTESIAN_POINT('',(182.388264603403,506.310565160535,-49.0221601717605)) ;
#46535 = CARTESIAN_POINT('',(181.388264603403,506.310565160536,-24.0221601717598)) ;
#46536 = CARTESIAN_POINT('Origin',(181.388264603403,506.310565160535,-25.0221601717598)) ;
#46537 = CARTESIAN_POINT('',(12.4885276254027,506.310565160565,-24.0221601717521)) ;
#46538 = CARTESIAN_POINT('',(197.388396114403,506.310565160533,-24.0221601717605)) ;
#46539 = CARTESIAN_POINT('',(11.4885276254026,506.310565160565,-25.0221601717521)) ;
#46540 = CARTESIAN_POINT('Origin',(12.4885276254026,506.310565160565,-25.0221601717521)) ;
#46541 = CARTESIAN_POINT('',(11.4885276254026,506.310565160565,-27.522160171752)) ;
#46542 = CARTESIAN_POINT('',(11.4885276254026,506.310565160565,-46.7721601717567)) ;
#46543 = CARTESIAN_POINT('',(10.4885276254026,506.310565160566,-28.522160171752)) ;
#46544 = CARTESIAN_POINT('Origin',(10.4885276254026,506.310565160565,-27.522160171752)) ;
#46545 = CARTESIAN_POINT('',(1.2385276254026,506.310565160567,-28.5221601717516)) ;
#46546 = CARTESIAN_POINT('',(205.813527625403,506.310565160531,-28.5221601717609)) ;
#46547 = CARTESIAN_POINT('',(0.238527625402662,506.310565160567,-27.5221601717516)) ;
#46548 = CARTESIAN_POINT('Origin',(1.23852762540266,506.310565160567,-27.5221601717516)) ;
#46549 = CARTESIAN_POINT('',(0.23852762540189,506.310565160567,-44.5221601717516)) ;
#46550 = CARTESIAN_POINT('',(188.638264603403,506.310565160534,-24.0203292412001)) ;
#46551 = CARTESIAN_POINT('Origin',(187.388264603403,506.310565160534,-24.0203292412001)) ;
#46552 = CARTESIAN_POINT('',(7.73852762540263,506.310565160566,-24.0221601717538)) ;
#46553 = CARTESIAN_POINT('Origin',(6.48852762540263,506.310565160566,-24.0221601717538)) ;
#46554 = CARTESIAN_POINT('Origin',(155.388527625422,615.96056516054,-20.2721601717586)) ;
#46555 = CARTESIAN_POINT('',(0.23852762542239,616.710565160567,-20.2721601717516)) ;
#46556 = CARTESIAN_POINT('',(0.238527625422287,615.960565160567,-19.5221601717516)) ;
#46557 = CARTESIAN_POINT('Origin',(0.238527625422247,615.960565160567,-20.2721601717516)) ;
#46558 = CARTESIAN_POINT('',(196.738527625422,615.960565160533,-19.5221601717605)) ;
#46559 = CARTESIAN_POINT('',(155.388527625422,615.96056516054,-19.5221601717586)) ;
#46560 = CARTESIAN_POINT('',(196.738527625422,616.710565160533,-20.2721601717605)) ;
#46561 = CARTESIAN_POINT('Origin',(196.738527625422,615.960565160533,-20.2721601717605)) ;
#46562 = CARTESIAN_POINT('',(155.388527625422,616.71056516054,-20.2721601717586)) ;
#46563 = CARTESIAN_POINT('Origin',(0.238527625422194,615.460565160567,-19.5221601717516)) ;
#46564 = CARTESIAN_POINT('',(0.238527625422061,616.710565160567,-27.5221601717515)) ;
#46565 = CARTESIAN_POINT('',(0.238527625421743,616.710565160567,-34.5221601717516)) ;
#46566 = CARTESIAN_POINT('',(0.238527625421935,616.110565160567,-27.5221601717515)) ;
#46567 = CARTESIAN_POINT('',(0.23852762542194,616.085565160567,-27.5221601717515)) ;
#46568 = CARTESIAN_POINT('',(0.238527625421163,616.110565160567,-44.5221601717516)) ;
#46569 = CARTESIAN_POINT('',(0.238527625421886,613.710565160567,-19.5221601717516)) ;
#46570 = CARTESIAN_POINT('',(0.238527625421886,613.710565160567,-19.5221601717516)) ;
#46571 = CARTESIAN_POINT('',(0.238527625422265,615.835565160567,-19.5221601717516)) ;
#46572 = CARTESIAN_POINT('Origin',(104.888527625422,616.710565160549,-34.4971601717606)) ;
#46573 = CARTESIAN_POINT('',(196.738527625422,616.710565160533,-23.5221601717605)) ;
#46574 = CARTESIAN_POINT('',(196.738527625422,616.710565160533,-34.5221601717605)) ;
#46575 = CARTESIAN_POINT('',(196.238527625422,616.710565160533,-24.0221601717605)) ;
#46576 = CARTESIAN_POINT('Origin',(196.238527625422,616.710565160533,-23.5221601717605)) ;
#46577 = CARTESIAN_POINT('',(193.388264603422,616.710565160533,-24.0221601717603)) ;
#46578 = CARTESIAN_POINT('',(149.563527625422,616.710565160541,-24.0221601717583)) ;
#46579 = CARTESIAN_POINT('',(192.388264603422,616.710565160533,-25.0221601717603)) ;
#46580 = CARTESIAN_POINT('Origin',(193.388264603422,616.710565160533,-25.0221601717603)) ;
#46581 = CARTESIAN_POINT('',(192.388264603422,616.710565160533,-27.5221601717598)) ;
#46582 = CARTESIAN_POINT('',(192.388264603422,616.710565160533,-28.7221601717598)) ;
#46583 = CARTESIAN_POINT('',(191.388264603422,616.710565160534,-28.5221601717598)) ;
#46584 = CARTESIAN_POINT('Origin',(191.388264603422,616.710565160532,-27.5221601717598)) ;
#46585 = CARTESIAN_POINT('',(183.388264603422,616.710565160535,-28.5221601717598)) ;
#46586 = CARTESIAN_POINT('',(143.638396114422,616.710565160542,-28.5221601717598)) ;
#46587 = CARTESIAN_POINT('',(182.388264603422,616.710565160535,-27.5221601717598)) ;
#46588 = CARTESIAN_POINT('Origin',(183.388264603422,616.710565160534,-27.5221601717598)) ;
#46589 = CARTESIAN_POINT('',(182.388264603422,616.710565160535,-25.0221601717598)) ;
#46590 = CARTESIAN_POINT('',(182.388264603422,616.710565160535,-19.5221601717598)) ;
#46591 = CARTESIAN_POINT('',(181.388264603422,616.710565160535,-24.0221601717598)) ;
#46592 = CARTESIAN_POINT('Origin',(181.388264603422,616.710565160534,-25.0221601717598)) ;
#46593 = CARTESIAN_POINT('',(12.4885276254221,616.710565160565,-24.0221601717521)) ;
#46594 = CARTESIAN_POINT('',(152.063527625422,616.71056516054,-24.0221601717585)) ;
#46595 = CARTESIAN_POINT('',(11.488527625422,616.710565160565,-25.0221601717521)) ;
#46596 = CARTESIAN_POINT('Origin',(12.488527625422,616.710565160565,-25.0221601717521)) ;
#46597 = CARTESIAN_POINT('',(11.488527625422,616.710565160565,-27.5221601717516)) ;
#46598 = CARTESIAN_POINT('',(11.488527625422,616.710565160565,-19.5221601717561)) ;
#46599 = CARTESIAN_POINT('',(10.488527625422,616.710565160565,-28.5221603701969)) ;
#46600 = CARTESIAN_POINT('Origin',(10.488527625422,616.710565160565,-27.5221601717516)) ;
#46601 = CARTESIAN_POINT('',(1.23852762542205,616.710565160567,-28.5221603701968)) ;
#46602 = CARTESIAN_POINT('',(152.063527625422,616.71056516054,-28.522160767094)) ;
#46603 = CARTESIAN_POINT('Origin',(1.23852762542205,616.710565160567,-27.5221601717516)) ;
#46604 = CARTESIAN_POINT('',(186.138264631837,616.710565160535,-24.0200627128237)) ;
#46605 = CARTESIAN_POINT('Origin',(187.388264603422,616.710565160534,-24.0203292412001)) ;
#46606 = CARTESIAN_POINT('',(7.73852762542202,616.710565160566,-24.0221601717538)) ;
#46607 = CARTESIAN_POINT('Origin',(6.48852762542202,616.710565160566,-24.0221601717538)) ;
#46608 = CARTESIAN_POINT('Origin',(209.138527625403,506.460565160531,-20.2721601717611)) ;
#46609 = CARTESIAN_POINT('',(196.738527625403,505.710565160533,-20.2721601717605)) ;
#46610 = CARTESIAN_POINT('',(196.738527625403,506.460565160533,-19.5221601717605)) ;
#46611 = CARTESIAN_POINT('Origin',(196.738527625403,506.460565160533,-20.2721601717605)) ;
#46612 = CARTESIAN_POINT('',(0.238527625403083,506.460565160567,-19.5221601717516)) ;
#46613 = CARTESIAN_POINT('',(209.138527625403,506.460565160531,-19.5221601717611)) ;
#46614 = CARTESIAN_POINT('',(0.238527625402882,505.710565160567,-20.2721601717516)) ;
#46615 = CARTESIAN_POINT('Origin',(0.238527625403009,506.460565160567,-20.2721601717516)) ;
#46616 = CARTESIAN_POINT('',(209.138527625403,505.710565160531,-20.2721601717611)) ;
#46617 = CARTESIAN_POINT('Origin',(196.738527625422,616.210565160533,-19.5221601717605)) ;
#46618 = CARTESIAN_POINT('',(196.738527625403,505.710565160533,-23.5221601717605)) ;
#46619 = CARTESIAN_POINT('',(196.738527625403,505.710565160533,-9.5221601717605)) ;
#46620 = CARTESIAN_POINT('',(196.738527625422,616.460565160533,-23.5221601717605)) ;
#46621 = CARTESIAN_POINT('',(196.738527625403,506.560565160533,-19.5221601717605)) ;
#46622 = CARTESIAN_POINT('',(196.738527625403,506.560565160533,-19.5221601717605)) ;
#46623 = CARTESIAN_POINT('',(196.738527625422,616.210565160533,-19.5221601717605)) ;
#46624 = CARTESIAN_POINT('Origin',(212.388527625404,505.71056516053,0.477839828238782)) ;
#46625 = CARTESIAN_POINT('',(0.238527625402582,505.710565160567,-27.5221601717516)) ;
#46626 = CARTESIAN_POINT('',(0.238527625403371,505.710565160567,-9.52216017175159)) ;
#46627 = CARTESIAN_POINT('',(1.23852762540249,505.710565160567,-28.5221601717516)) ;
#46628 = CARTESIAN_POINT('Origin',(1.23852762540256,505.710565160567,-27.5221601717516)) ;
#46629 = CARTESIAN_POINT('',(10.4885276254025,505.710565160566,-28.522160171752)) ;
#46630 = CARTESIAN_POINT('',(205.813527625403,505.710565160531,-28.5221601717609)) ;
#46631 = CARTESIAN_POINT('',(11.4885276254025,505.710565160565,-27.522160171752)) ;
#46632 = CARTESIAN_POINT('Origin',(10.4885276254025,505.710565160565,-27.522160171752)) ;
#46633 = CARTESIAN_POINT('',(11.4885276254025,505.710565160565,-25.0221601717521)) ;
#46634 = CARTESIAN_POINT('',(11.4885276254025,505.710565160565,-11.7721601717567)) ;
#46635 = CARTESIAN_POINT('',(12.4885276254026,505.710565160565,-24.0221601717521)) ;
#46636 = CARTESIAN_POINT('Origin',(12.4885276254025,505.710565160564,-25.0221601717521)) ;
#46637 = CARTESIAN_POINT('',(181.388264603403,505.710565160536,-24.0221601717598)) ;
#46638 = CARTESIAN_POINT('',(197.388396114403,505.710565160533,-24.0221601717605)) ;
#46639 = CARTESIAN_POINT('',(182.388264603403,505.710565160535,-25.0221601717598)) ;
#46640 = CARTESIAN_POINT('Origin',(181.388264603403,505.710565160535,-25.0221601717598)) ;
#46641 = CARTESIAN_POINT('',(182.388264603403,505.710565160535,-27.5221601717599)) ;
#46642 = CARTESIAN_POINT('',(182.388264603403,505.710565160535,-14.0221601717605)) ;
#46643 = CARTESIAN_POINT('',(183.388264603403,505.710565160535,-28.5221601717599)) ;
#46644 = CARTESIAN_POINT('Origin',(183.388264603403,505.710565160535,-27.5221601717599)) ;
#46645 = CARTESIAN_POINT('',(191.388264603403,505.710565160534,-28.5221601717603)) ;
#46646 = CARTESIAN_POINT('',(205.813527625403,505.710565160531,-28.5221601717609)) ;
#46647 = CARTESIAN_POINT('',(192.388264603403,505.710565160534,-27.5221601717603)) ;
#46648 = CARTESIAN_POINT('Origin',(191.388264603403,505.710565160534,-27.5221601717603)) ;
#46649 = CARTESIAN_POINT('',(192.388264603403,505.710565160534,-25.0221601717603)) ;
#46650 = CARTESIAN_POINT('',(192.388264603403,505.710565160534,-11.7721601717608)) ;
#46651 = CARTESIAN_POINT('',(193.388264603403,505.710565160533,-24.0221601717603)) ;
#46652 = CARTESIAN_POINT('Origin',(193.388264603403,505.710565160533,-25.0221601717604)) ;
#46653 = CARTESIAN_POINT('',(196.238527625403,505.710565160533,-24.0221601717605)) ;
#46654 = CARTESIAN_POINT('',(203.313527625403,505.710565160532,-24.0221601717608)) ;
#46655 = CARTESIAN_POINT('Origin',(196.238527625403,505.710565160533,-23.5221601717605)) ;
#46656 = CARTESIAN_POINT('',(188.638264603403,505.710565160534,-24.0203292412001)) ;
#46657 = CARTESIAN_POINT('Origin',(187.388264603403,505.710565160534,-24.0203292412001)) ;
#46658 = CARTESIAN_POINT('',(7.73852762540252,505.710565160566,-24.0221601717538)) ;
#46659 = CARTESIAN_POINT('Origin',(6.48852762540252,505.710565160566,-24.0221601717538)) ;
#46660 = CARTESIAN_POINT('Origin',(193.388264603422,616.710565160533,-25.0221601717603)) ;
#46661 = CARTESIAN_POINT('',(193.388264603422,616.110565160533,-24.0221601717603)) ;
#46662 = CARTESIAN_POINT('',(193.388264603422,616.710565160533,-24.0221601717603)) ;
#46663 = CARTESIAN_POINT('',(192.388264603422,616.110565160533,-25.0221601717603)) ;
#46664 = CARTESIAN_POINT('Origin',(193.388264603422,616.110565160533,-25.0221601717603)) ;
#46665 = CARTESIAN_POINT('',(192.388264603422,616.710565160533,-25.0221601717603)) ;
#46666 = CARTESIAN_POINT('Origin',(196.738527625422,616.710565160533,-24.0221601717605)) ;
#46667 = CARTESIAN_POINT('',(196.238527625422,616.110565160533,-24.0221601717605)) ;
#46668 = CARTESIAN_POINT('',(196.238527625412,561.210565160533,-24.0221601717605)) ;
#46669 = CARTESIAN_POINT('',(203.313527625422,616.110565160532,-24.0221601717608)) ;
#46670 = CARTESIAN_POINT('Origin',(193.388264603422,616.710565160533,-25.0221601717603)) ;
#46671 = CARTESIAN_POINT('',(193.388264603422,616.710565160533,-24.0221601717603)) ;
#46672 = CARTESIAN_POINT('',(192.388264603422,616.710565160533,-25.0221601717603)) ;
#46673 = CARTESIAN_POINT('Origin',(196.738527625422,616.710565160533,-24.0221601717605)) ;
#46674 = CARTESIAN_POINT('',(196.238527625422,616.460565160533,-24.0221601717605)) ;
#46675 = CARTESIAN_POINT('Origin',(0.138527625417808,588.897292039156,-20.2721601717516)) ;
#46676 = CARTESIAN_POINT('',(-0.611472374596262,508.710565160568,-20.2721601717515)) ;
#46677 = CARTESIAN_POINT('',(0.138527625403757,508.710565160567,-19.5221601717516)) ;
#46678 = CARTESIAN_POINT('Origin',(0.138527625403723,508.710565160567,-20.2721601717516)) ;
#46679 = CARTESIAN_POINT('',(0.138527625422196,613.710565160567,-19.5221601717516)) ;
#46680 = CARTESIAN_POINT('',(0.138527625417842,588.897292039156,-19.5221601717516)) ;
#46681 = CARTESIAN_POINT('',(-0.611472374577818,613.710565160567,-20.2721601717515)) ;
#46682 = CARTESIAN_POINT('Origin',(0.138527625422167,613.710565160567,-20.2721601717516)) ;
#46683 = CARTESIAN_POINT('',(-0.611472374582177,588.897292039156,-20.2721601717515)) ;
#46684 = CARTESIAN_POINT('Origin',(-0.611472374578105,613.710565160567,-19.5221601717515)) ;
#46685 = CARTESIAN_POINT('',(101.388527625422,613.710565160549,-19.5221601717562)) ;
#46686 = CARTESIAN_POINT('',(-0.0114723745782475,613.710565160567,-23.0221601717516)) ;
#46687 = CARTESIAN_POINT('',(-0.011472374579224,613.710565160567,-44.5221601717516)) ;
#46688 = CARTESIAN_POINT('',(-0.611472374577943,613.710565160567,-23.0221601717515)) ;
#46689 = CARTESIAN_POINT('',(99.3135276254217,613.71056516055,-23.0221601717561)) ;
#46690 = CARTESIAN_POINT('',(-0.611472374578124,613.710565160567,-27.0096601717536)) ;
#46691 = CARTESIAN_POINT('Origin',(205.888527625422,616.210565160531,-19.5221601717609)) ;
#46692 = CARTESIAN_POINT('',(0.238527625403435,508.710565160567,-19.5221601717516)) ;
#46693 = CARTESIAN_POINT('',(101.763527625403,508.71056516055,-19.5221601717562)) ;
#46694 = CARTESIAN_POINT('',(0.238527625403151,506.960565160567,-19.5221601717516)) ;
#46695 = CARTESIAN_POINT('',(196.838527625403,506.560565160533,-19.5221601717605)) ;
#46696 = CARTESIAN_POINT('',(196.838527625403,506.560565160533,-19.5221601717605)) ;
#46697 = CARTESIAN_POINT('',(196.838527625422,615.860565160533,-19.5221601717605)) ;
#46698 = CARTESIAN_POINT('',(196.838527625422,615.360565160533,-19.5221601717605)) ;
#46699 = CARTESIAN_POINT('',(196.738527625422,615.860565160533,-19.5221601717605)) ;
#46700 = CARTESIAN_POINT('',(196.738527625422,615.860565160533,-19.5221601717605)) ;
#46701 = CARTESIAN_POINT('',(196.738527625422,615.460565160533,-19.5221601717605)) ;
#46702 = CARTESIAN_POINT('',(68.189609074102,544.044531662882,-19.5221601728758)) ;
#46703 = CARTESIAN_POINT('',(48.6516117532406,563.582528983677,-19.5221601717538)) ;
#46704 = CARTESIAN_POINT('Origin',(44.9784504245142,540.371370334153,-19.5221601717533)) ;
#46705 = CARTESIAN_POINT('',(49.4331354401999,568.521073377188,-19.5221601717538)) ;
#46706 = CARTESIAN_POINT('Origin',(49.0423735967098,566.051801180334,-19.5221601717518)) ;
#46707 = CARTESIAN_POINT('',(73.1281535186845,544.826055026706,-19.5221601728761)) ;
#46708 = CARTESIAN_POINT('Origin',(44.9784504245142,540.371370334153,-19.5221601717536)) ;
#46709 = CARTESIAN_POINT('Origin',(70.6588813175403,544.435293211585,-19.5221601742775)) ;
#46710 = CARTESIAN_POINT('',(17.3918523583282,565.591787903562,-19.5221601717524)) ;
#46711 = CARTESIAN_POINT('Origin',(19.8918523583282,565.591787908239,-19.5221601717525)) ;
#46712 = CARTESIAN_POINT('',(67.3918523583194,515.591787864358,-19.5221601717546)) ;
#46713 = CARTESIAN_POINT('Origin',(69.8918523583194,515.59178790823,-19.5221601717547)) ;
#46714 = CARTESIAN_POINT('',(158.588527625419,594.710565160539,-19.5221601717588)) ;
#46715 = CARTESIAN_POINT('',(161.588527625419,594.710565160539,-19.5221601717589)) ;
#46716 = CARTESIAN_POINT('Origin',(160.088527625419,594.710565160539,-19.5221601717588)) ;
#46717 = CARTESIAN_POINT('',(161.588527625415,572.710565160539,-19.5221601717589)) ;
#46718 = CARTESIAN_POINT('',(161.588527625415,572.710565160539,-19.5221601717589)) ;
#46719 = CARTESIAN_POINT('',(158.588527625415,572.710565160539,-19.5221601717588)) ;
#46720 = CARTESIAN_POINT('Origin',(160.088527625415,572.710565160539,-19.5221601717588)) ;
#46721 = CARTESIAN_POINT('',(158.588527625419,594.710565160539,-19.5221601717588)) ;
#46722 = CARTESIAN_POINT('',(165.588527625419,594.710565160538,-19.5221601717591)) ;
#46723 = CARTESIAN_POINT('',(168.588527625419,594.710565160538,-19.5221601717592)) ;
#46724 = CARTESIAN_POINT('Origin',(167.088527625419,594.710565160538,-19.5221601717592)) ;
#46725 = CARTESIAN_POINT('',(168.588527625415,572.710565160538,-19.5221601717592)) ;
#46726 = CARTESIAN_POINT('',(168.588527625415,572.710565160538,-19.5221601717592)) ;
#46727 = CARTESIAN_POINT('',(165.588527625415,572.710565160538,-19.5221601717591)) ;
#46728 = CARTESIAN_POINT('Origin',(167.088527625415,572.710565160538,-19.5221601717592)) ;
#46729 = CARTESIAN_POINT('',(165.588527625419,594.710565160538,-19.5221601717591)) ;
#46730 = CARTESIAN_POINT('',(172.588527625419,594.710565160537,-19.5221601717594)) ;
#46731 = CARTESIAN_POINT('',(175.588527625419,594.710565160536,-19.5221601717595)) ;
#46732 = CARTESIAN_POINT('Origin',(174.088527625419,594.710565160537,-19.5221601717595)) ;
#46733 = CARTESIAN_POINT('',(175.588527625415,572.710565160536,-19.5221601717595)) ;
#46734 = CARTESIAN_POINT('',(175.588527625415,572.710565160536,-19.5221601717595)) ;
#46735 = CARTESIAN_POINT('',(172.588527625415,572.710565160537,-19.5221601717594)) ;
#46736 = CARTESIAN_POINT('Origin',(174.088527625415,572.710565160537,-19.5221601717595)) ;
#46737 = CARTESIAN_POINT('',(172.588527625419,594.710565160537,-19.5221601717594)) ;
#46738 = CARTESIAN_POINT('',(158.588527625411,549.710565160539,-19.5221601717588)) ;
#46739 = CARTESIAN_POINT('',(161.588527625411,549.710565160539,-19.5221601717589)) ;
#46740 = CARTESIAN_POINT('Origin',(160.088527625411,549.710565160539,-19.5221601717588)) ;
#46741 = CARTESIAN_POINT('',(161.588527625407,527.710565160539,-19.5221601717589)) ;
#46742 = CARTESIAN_POINT('',(161.588527625407,527.710565160539,-19.5221601717589)) ;
#46743 = CARTESIAN_POINT('',(158.588527625407,527.710565160539,-19.5221601717588)) ;
#46744 = CARTESIAN_POINT('Origin',(160.088527625407,527.710565160539,-19.5221601717588)) ;
#46745 = CARTESIAN_POINT('',(158.588527625411,549.710565160539,-19.5221601717588)) ;
#46746 = CARTESIAN_POINT('',(168.588527625407,527.710565160538,-19.5221601717592)) ;
#46747 = CARTESIAN_POINT('',(165.588527625407,527.710565160538,-19.5221601717591)) ;
#46748 = CARTESIAN_POINT('Origin',(167.088527625407,527.710565160538,-19.5221601717592)) ;
#46749 = CARTESIAN_POINT('',(165.588527625411,549.710565160538,-19.5221601717591)) ;
#46750 = CARTESIAN_POINT('',(165.588527625411,549.710565160538,-19.5221601717591)) ;
#46751 = CARTESIAN_POINT('',(168.588527625411,549.710565160538,-19.5221601717592)) ;
#46752 = CARTESIAN_POINT('Origin',(167.088527625411,549.710565160538,-19.5221601717592)) ;
#46753 = CARTESIAN_POINT('',(168.588527625407,527.710565160538,-19.5221601717592)) ;
#46754 = CARTESIAN_POINT('',(172.588527625411,549.710565160537,-19.5221601717594)) ;
#46755 = CARTESIAN_POINT('',(175.588527625411,549.710565160536,-19.5221601717595)) ;
#46756 = CARTESIAN_POINT('Origin',(174.088527625411,549.710565160537,-19.5221601717595)) ;
#46757 = CARTESIAN_POINT('',(175.588527625407,527.710565160536,-19.5221601717595)) ;
#46758 = CARTESIAN_POINT('',(175.588527625407,527.710565160536,-19.5221601717595)) ;
#46759 = CARTESIAN_POINT('',(172.588527625407,527.710565160537,-19.5221601717594)) ;
#46760 = CARTESIAN_POINT('Origin',(174.088527625407,527.710565160537,-19.5221601717595)) ;
#46761 = CARTESIAN_POINT('',(172.588527625411,549.710565160537,-19.5221601717594)) ;
#46762 = CARTESIAN_POINT('',(50.0586926677957,539.082949664376,-19.5221601717538)) ;
#46763 = CARTESIAN_POINT('Origin',(51.4729062301691,540.497163226748,-19.5221601717539)) ;
#46764 = CARTESIAN_POINT('',(43.5642368621326,532.593195741101,-19.5221601717536)) ;
#46765 = CARTESIAN_POINT('Origin',(44.9784504245059,534.007409303474,-19.5221601717536)) ;
#46766 = CARTESIAN_POINT('',(37.0744829388654,539.087651546757,-19.5221601717532)) ;
#46767 = CARTESIAN_POINT('Origin',(38.4886965012388,540.50186510913,-19.5221601717533)) ;
#46768 = CARTESIAN_POINT('',(43.5689387445145,545.577405470032,-19.5221601717535)) ;
#46769 = CARTESIAN_POINT('Origin',(44.9831523068879,546.991619032405,-19.5221601717536)) ;
#46770 = CARTESIAN_POINT('',(31.8295857683906,548.578523205569,-19.522160171753)) ;
#46771 = CARTESIAN_POINT('',(31.8295857683879,532.164217462742,-19.522160171753)) ;
#46772 = CARTESIAN_POINT('Origin',(44.9784504245141,540.371370334153,-19.5221601717536)) ;
#46773 = CARTESIAN_POINT('',(26.7397026756914,528.987255060894,-19.5221601717528)) ;
#46774 = CARTESIAN_POINT('Origin',(29.2846442220396,530.575736261818,-19.5221601717601)) ;
#46775 = CARTESIAN_POINT('',(26.7397026756954,551.755485607418,-19.5221601717528)) ;
#46776 = CARTESIAN_POINT('Origin',(44.978450424514,540.371370334153,-19.5221601717575)) ;
#46777 = CARTESIAN_POINT('Origin',(29.284644222043,550.167004406493,-19.5221601717549)) ;
#46778 = CARTESIAN_POINT('',(36.7712975530987,527.22250567803,-19.5221601717532)) ;
#46779 = CARTESIAN_POINT('',(33.5943351512492,522.132622585334,-19.5221601717531)) ;
#46780 = CARTESIAN_POINT('Origin',(35.182816352174,524.677564131682,-19.5221601717552)) ;
#46781 = CARTESIAN_POINT('',(53.1856032959254,527.222505678027,-19.522160171754)) ;
#46782 = CARTESIAN_POINT('Origin',(44.9784504245142,540.371370334153,-19.5221601717536)) ;
#46783 = CARTESIAN_POINT('',(56.362565697773,522.13262258533,-19.5221601717541)) ;
#46784 = CARTESIAN_POINT('Origin',(54.7740844968491,524.677564131679,-19.5221601717613)) ;
#46785 = CARTESIAN_POINT('Origin',(44.9784504245142,540.371370334153,-19.5221601717575)) ;
#46786 = CARTESIAN_POINT('',(58.1273150806378,532.164217462738,-19.5221601717542)) ;
#46787 = CARTESIAN_POINT('',(63.217198173333,528.987255060888,-19.5221601717544)) ;
#46788 = CARTESIAN_POINT('Origin',(60.6722566269854,530.575736261813,-19.5221601717564)) ;
#46789 = CARTESIAN_POINT('',(58.1273150806405,548.578523205564,-19.5221601717542)) ;
#46790 = CARTESIAN_POINT('Origin',(44.9784504245143,540.371370334153,-19.5221601717536)) ;
#46791 = CARTESIAN_POINT('',(63.217198173337,551.755485607412,-19.5221601717544)) ;
#46792 = CARTESIAN_POINT('Origin',(60.6722566269888,550.167004406488,-19.5221601717615)) ;
#46793 = CARTESIAN_POINT('Origin',(44.9784504245144,540.371370334153,-19.5221601717575)) ;
#46794 = CARTESIAN_POINT('',(53.1856032959298,553.520234990277,-19.522160171754)) ;
#46795 = CARTESIAN_POINT('',(56.3625656977793,558.610118082972,-19.5221601717541)) ;
#46796 = CARTESIAN_POINT('Origin',(54.7740844968545,556.065176536624,-19.5221601717561)) ;
#46797 = CARTESIAN_POINT('',(36.7712975531031,553.52023499028,-19.5221601717532)) ;
#46798 = CARTESIAN_POINT('Origin',(44.9784504245142,540.371370334153,-19.5221601717536)) ;
#46799 = CARTESIAN_POINT('',(33.5943351512555,558.610118082976,-19.5221601717531)) ;
#46800 = CARTESIAN_POINT('Origin',(35.1828163521794,556.065176536628,-19.5221601717604)) ;
#46801 = CARTESIAN_POINT('Origin',(44.9784504245142,540.371370334153,-19.5221601717575)) ;
#46802 = CARTESIAN_POINT('',(41.3053508856094,563.582538762398,-19.5221601670358)) ;
#46803 = CARTESIAN_POINT('',(21.7672917749906,544.04453166288,-19.5221601717525)) ;
#46804 = CARTESIAN_POINT('Origin',(44.9784504245142,540.371370334153,-19.5221601717533)) ;
#46805 = CARTESIAN_POINT('',(16.8287473814797,544.826055349839,-19.5221601717524)) ;
#46806 = CARTESIAN_POINT('Origin',(19.2980195783332,544.435293506349,-19.5221601717457)) ;
#46807 = CARTESIAN_POINT('',(40.5237715662165,568.521074351593,-19.5221601670422)) ;
#46808 = CARTESIAN_POINT('Origin',(44.9784504245142,540.371370334153,-19.5221601717536)) ;
#46809 = CARTESIAN_POINT('Origin',(40.9145328695602,566.05180206946,-19.5221601615182)) ;
#46810 = CARTESIAN_POINT('',(21.7672748311997,536.698316068459,-19.5221601717524)) ;
#46811 = CARTESIAN_POINT('',(41.3052890957879,517.16021168463,-19.5221601717534)) ;
#46812 = CARTESIAN_POINT('Origin',(44.9784504245142,540.371370334153,-19.5221601717533)) ;
#46813 = CARTESIAN_POINT('',(40.523765408828,512.221667291119,-19.5221601717534)) ;
#46814 = CARTESIAN_POINT('Origin',(40.9145272523186,514.690939487972,-19.5221601717542)) ;
#46815 = CARTESIAN_POINT('',(16.8287456930818,535.916695987675,-19.5221601717523)) ;
#46816 = CARTESIAN_POINT('Origin',(44.9784504245142,540.371370334153,-19.5221601717536)) ;
#46817 = CARTESIAN_POINT('Ctrl Pts',(21.7672748300875,536.698316068691,-19.5221601717526)) ;
#46818 = CARTESIAN_POINT('Ctrl Pts',(21.6503315201662,537.437106614635,-19.5221601717903)) ;
#46819 = CARTESIAN_POINT('Ctrl Pts',(20.7071515293286,538.794808687501,-19.5221601718653)) ;
#46820 = CARTESIAN_POINT('Ctrl Pts',(18.2300981784228,538.964503729857,-19.5221601718932)) ;
#46821 = CARTESIAN_POINT('Ctrl Pts',(16.8370747520978,537.437573131344,-19.522160171828)) ;
#46822 = CARTESIAN_POINT('Ctrl Pts',(16.7702887385542,536.286093586995,-19.5221601717711)) ;
#46823 = CARTESIAN_POINT('Ctrl Pts',(16.828745693126,535.916695987396,-19.5221601717522)) ;
#46824 = CARTESIAN_POINT('',(48.6516101199294,517.160211426159,-19.5221601717537)) ;
#46825 = CARTESIAN_POINT('',(68.1896090740379,536.698209005427,-19.5221601717547)) ;
#46826 = CARTESIAN_POINT('Origin',(44.9784504245142,540.371370334153,-19.5221601717533)) ;
#46827 = CARTESIAN_POINT('',(73.1281534675487,535.916685318467,-19.5221601717549)) ;
#46828 = CARTESIAN_POINT('Origin',(70.6588812706952,536.307447161957,-19.5221601717603)) ;
#46829 = CARTESIAN_POINT('',(49.4331351147273,512.221667239613,-19.5221601717538)) ;
#46830 = CARTESIAN_POINT('Origin',(44.9784504245142,540.371370334153,-19.5221601717536)) ;
#46831 = CARTESIAN_POINT('Ctrl Pts',(48.6516084871238,517.160211167766,-19.5221601717538)) ;
#46832 = CARTESIAN_POINT('Ctrl Pts',(47.9128043995578,517.043294654392,-19.5221601721921)) ;
#46833 = CARTESIAN_POINT('Ctrl Pts',(46.5550515006054,516.100143191902,-19.5221601730645)) ;
#46834 = CARTESIAN_POINT('Ctrl Pts',(46.3853000863992,513.623057434898,-19.5221601733897)) ;
#46835 = CARTESIAN_POINT('Ctrl Pts',(47.9122384138109,512.229997790477,-19.5221601726333)) ;
#46836 = CARTESIAN_POINT('Ctrl Pts',(49.0637330000058,512.163209431194,-19.5221601719729)) ;
#46837 = CARTESIAN_POINT('Ctrl Pts',(49.4331351147579,512.22166723942,-19.5221601717538)) ;
#46838 = CARTESIAN_POINT('Origin',(212.38852762542,616.11056516053,-69.5221601717612)) ;
#46839 = CARTESIAN_POINT('',(1.23852762542194,616.110565160567,-28.5221601717516)) ;
#46840 = CARTESIAN_POINT('Origin',(1.23852762542194,616.110565160567,-27.5221601717516)) ;
#46841 = CARTESIAN_POINT('',(10.4885276254219,616.110565160565,-28.5221601717516)) ;
#46842 = CARTESIAN_POINT('',(106.938527625421,616.110565160549,-28.5221601717516)) ;
#46843 = CARTESIAN_POINT('',(11.4885276254219,616.110565160565,-27.5221601717516)) ;
#46844 = CARTESIAN_POINT('Origin',(10.4885276254219,616.110565160565,-27.5221601717516)) ;
#46845 = CARTESIAN_POINT('',(11.4885276254219,616.110565160565,-25.0221601717521)) ;
#46846 = CARTESIAN_POINT('',(11.4885276254219,616.110565160565,-49.0221601717564)) ;
#46847 = CARTESIAN_POINT('',(12.488527625422,616.110565160565,-24.0221601717521)) ;
#46848 = CARTESIAN_POINT('Origin',(12.4885276254219,616.110565160565,-25.0221601717521)) ;
#46849 = CARTESIAN_POINT('',(181.388264603422,616.110565160535,-24.0221601717598)) ;
#46850 = CARTESIAN_POINT('',(205.813527625422,616.110565160531,-24.0221601717609)) ;
#46851 = CARTESIAN_POINT('',(182.388264603422,616.110565160535,-25.0221601717598)) ;
#46852 = CARTESIAN_POINT('Origin',(181.388264603422,616.110565160536,-25.0221601717598)) ;
#46853 = CARTESIAN_POINT('',(182.388264603422,616.110565160535,-27.5221601717598)) ;
#46854 = CARTESIAN_POINT('',(182.388264603422,616.110565160535,-49.0221601717605)) ;
#46855 = CARTESIAN_POINT('',(183.388264603422,616.110565160535,-28.5221601717598)) ;
#46856 = CARTESIAN_POINT('Origin',(183.388264603422,616.110565160535,-27.5221601717598)) ;
#46857 = CARTESIAN_POINT('',(191.388264603422,616.110565160534,-28.5221601717598)) ;
#46858 = CARTESIAN_POINT('',(197.388396114421,616.110565160533,-28.5221601717598)) ;
#46859 = CARTESIAN_POINT('',(192.388264603422,616.110565160533,-27.5221601717598)) ;
#46860 = CARTESIAN_POINT('Origin',(191.388264603422,616.110565160534,-27.5221601717598)) ;
#46861 = CARTESIAN_POINT('',(192.388264603422,616.110565160533,-49.1221601717605)) ;
#46862 = CARTESIAN_POINT('',(196.738527625422,616.110565160533,-23.5221601717605)) ;
#46863 = CARTESIAN_POINT('Origin',(196.238527625422,616.110565160533,-23.5221601717605)) ;
#46864 = CARTESIAN_POINT('',(196.738527625421,616.110565160533,-44.5221601717605)) ;
#46865 = CARTESIAN_POINT('',(186.138264631837,616.110565160535,-24.0200627128237)) ;
#46866 = CARTESIAN_POINT('Origin',(187.388264603422,616.110565160534,-24.0203292412001)) ;
#46867 = CARTESIAN_POINT('',(7.73852762542192,616.110565160566,-24.0221601717538)) ;
#46868 = CARTESIAN_POINT('Origin',(6.48852762542192,616.110565160566,-24.0221601717538)) ;
#46869 = CARTESIAN_POINT('Origin',(-0.0114723745895816,561.210565160567,-69.5221601717516)) ;
#46870 = CARTESIAN_POINT('',(-0.0114723745966916,508.710565160567,-23.0221601717516)) ;
#46871 = CARTESIAN_POINT('',(-0.0114723745976681,508.710565160567,-44.5221601717516)) ;
#46872 = CARTESIAN_POINT('',(-0.0114723745966299,509.210565160567,-23.5221601717516)) ;
#46873 = CARTESIAN_POINT('Origin',(-0.0114723745966039,509.210565160567,-23.0221601717516)) ;
#46874 = CARTESIAN_POINT('',(-0.0114723745783614,613.210565160567,-23.5221601717515)) ;
#46875 = CARTESIAN_POINT('',(-0.0114723745923263,533.710565160567,-23.5221601717516)) ;
#46876 = CARTESIAN_POINT('Origin',(-0.0114723745783429,613.210565160567,-23.0221601717516)) ;
#46877 = CARTESIAN_POINT('Origin',(49.042373596694,566.051801180341,-256.918732177553)) ;
#46878 = CARTESIAN_POINT('',(49.4331354401894,568.521073377188,-256.918732177553)) ;
#46879 = CARTESIAN_POINT('',(48.6516117532405,563.582528983677,-20.2721601717532)) ;
#46880 = CARTESIAN_POINT('Origin',(44.9784504245142,540.371370334153,-19.5221601717536)) ;
#46881 = CARTESIAN_POINT('',(73.1281535186845,544.826055026706,-19.5221601717548)) ;
#46882 = CARTESIAN_POINT('Origin',(40.9145328695602,566.05180206946,-19.5221601717534)) ;
#46883 = CARTESIAN_POINT('',(40.5237715662164,568.521074351593,-19.5221601717534)) ;
#46884 = CARTESIAN_POINT('',(41.3053508855747,563.582538762618,-19.5221601717534)) ;
#46885 = CARTESIAN_POINT('Origin',(44.9784504245142,540.371370334153,-19.5221601717536)) ;
#46886 = CARTESIAN_POINT('',(16.8287473814692,544.826055349839,-256.918732177552)) ;
#46887 = CARTESIAN_POINT('Origin',(19.2980195783158,544.435293506344,-256.918732177552)) ;
#46888 = CARTESIAN_POINT('',(21.7672917749906,544.04453166288,-20.272160171752)) ;
#46889 = CARTESIAN_POINT('Ctrl Pts',(21.7672748300875,536.698316068691,-19.5221601716228)) ;
#46890 = CARTESIAN_POINT('Ctrl Pts',(21.7672748301048,536.698316068582,-19.7221601716661)) ;
#46891 = CARTESIAN_POINT('Ctrl Pts',(21.7672748296538,536.698316071431,-19.9221601717093)) ;
#46892 = CARTESIAN_POINT('Ctrl Pts',(21.7672748296711,536.698316071321,-20.1221601717526)) ;
#46893 = CARTESIAN_POINT('Ctrl Pts',(21.6503315201662,537.437106614635,-19.5221601716605)) ;
#46894 = CARTESIAN_POINT('Ctrl Pts',(21.6503315202122,537.43710661454,-19.7221601717038)) ;
#46895 = CARTESIAN_POINT('Ctrl Pts',(21.6503315190249,537.437106617018,-19.922160171747)) ;
#46896 = CARTESIAN_POINT('Ctrl Pts',(21.6503315190709,537.437106616922,-20.1221601717903)) ;
#46897 = CARTESIAN_POINT('Ctrl Pts',(20.7071515293285,538.794808687501,-19.5221601717356)) ;
#46898 = CARTESIAN_POINT('Ctrl Pts',(20.7071515294062,538.794808687459,-19.7221601717788)) ;
#46899 = CARTESIAN_POINT('Ctrl Pts',(20.7071515273852,538.794808688543,-19.9221601718221)) ;
#46900 = CARTESIAN_POINT('Ctrl Pts',(20.707151527463,538.794808688501,-20.1221601718653)) ;
#46901 = CARTESIAN_POINT('Ctrl Pts',(18.2300981784228,538.964503729856,-19.5221601717634)) ;
#46902 = CARTESIAN_POINT('Ctrl Pts',(18.230098178466,538.964503729874,-19.7221601718066)) ;
#46903 = CARTESIAN_POINT('Ctrl Pts',(18.2300981773464,538.964503729414,-19.9221601718499)) ;
#46904 = CARTESIAN_POINT('Ctrl Pts',(18.2300981773896,538.964503729431,-20.1221601718932)) ;
#46905 = CARTESIAN_POINT('Ctrl Pts',(16.8370747520978,537.437573131345,-19.5221601716982)) ;
#46906 = CARTESIAN_POINT('Ctrl Pts',(16.8370747521019,537.437573131355,-19.7221601717414)) ;
#46907 = CARTESIAN_POINT('Ctrl Pts',(16.8370747519932,537.437573131106,-19.9221601717847)) ;
#46908 = CARTESIAN_POINT('Ctrl Pts',(16.8370747519973,537.437573131115,-20.122160171828)) ;
#46909 = CARTESIAN_POINT('Ctrl Pts',(16.7702887385542,536.286093586995,-19.5221601716413)) ;
#46910 = CARTESIAN_POINT('Ctrl Pts',(16.7702887385554,536.286093586989,-19.7221601716846)) ;
#46911 = CARTESIAN_POINT('Ctrl Pts',(16.7702887385333,536.286093587149,-19.9221601717279)) ;
#46912 = CARTESIAN_POINT('Ctrl Pts',(16.7702887385344,536.286093587143,-20.1221601717712)) ;
#46913 = CARTESIAN_POINT('Ctrl Pts',(16.828745693126,535.916695987396,-19.5221601716224)) ;
#46914 = CARTESIAN_POINT('Ctrl Pts',(16.8287456931277,535.916695987385,-19.7221601716657)) ;
#46915 = CARTESIAN_POINT('Ctrl Pts',(16.8287456930828,535.916695987669,-19.922160171709)) ;
#46916 = CARTESIAN_POINT('Ctrl Pts',(16.8287456930845,535.916695987658,-20.1221601717523)) ;
#46917 = CARTESIAN_POINT('',(16.828745693126,535.916695987396,-19.5221601716224)) ;
#46918 = CARTESIAN_POINT('',(21.7672748296711,536.698316071321,-20.1221601717508)) ;
#46919 = CARTESIAN_POINT('Origin',(44.9784504245142,540.371370334153,-19.5221601717536)) ;
#46920 = CARTESIAN_POINT('',(40.5237654088175,512.221667291119,-256.918732177553)) ;
#46921 = CARTESIAN_POINT('Origin',(40.9145272523129,514.690939487966,-256.918732177553)) ;
#46922 = CARTESIAN_POINT('',(41.3052890957878,517.16021168463,-20.2721601717529)) ;
#46923 = CARTESIAN_POINT('Ctrl Pts',(48.6516084871238,517.160211167766,-19.5221601702455)) ;
#46924 = CARTESIAN_POINT('Ctrl Pts',(48.6516084883974,517.160211167967,-19.7221601707483)) ;
#46925 = CARTESIAN_POINT('Ctrl Pts',(48.651608489671,517.160211168169,-19.922160171251)) ;
#46926 = CARTESIAN_POINT('Ctrl Pts',(48.6516084909445,517.16021116837,-20.1221601717538)) ;
#46927 = CARTESIAN_POINT('Ctrl Pts',(47.9128043995578,517.043294654392,-19.5221601706839)) ;
#46928 = CARTESIAN_POINT('Ctrl Pts',(47.9128044006695,517.043294654927,-19.7221601711867)) ;
#46929 = CARTESIAN_POINT('Ctrl Pts',(47.9128044017683,517.043294655448,-19.9221601716894)) ;
#46930 = CARTESIAN_POINT('Ctrl Pts',(47.91280440288,517.043294655983,-20.1221601721921)) ;
#46931 = CARTESIAN_POINT('Ctrl Pts',(46.5550515006053,516.100143191901,-19.5221601715563)) ;
#46932 = CARTESIAN_POINT('Ctrl Pts',(46.555051501089,516.100143192805,-19.722160172059)) ;
#46933 = CARTESIAN_POINT('Ctrl Pts',(46.5550515015749,516.100143193707,-19.9221601725618)) ;
#46934 = CARTESIAN_POINT('Ctrl Pts',(46.5550515020586,516.100143194611,-20.1221601730645)) ;
#46935 = CARTESIAN_POINT('Ctrl Pts',(46.3853000863992,513.623057434898,-19.5221601718814)) ;
#46936 = CARTESIAN_POINT('Ctrl Pts',(46.3853000861961,513.623057435401,-19.7221601723842)) ;
#46937 = CARTESIAN_POINT('Ctrl Pts',(46.385300085985,513.623057435896,-19.922160172887)) ;
#46938 = CARTESIAN_POINT('Ctrl Pts',(46.385300085782,513.623057436399,-20.1221601733897)) ;
#46939 = CARTESIAN_POINT('Ctrl Pts',(47.912238413811,512.229997790477,-19.5221601711252)) ;
#46940 = CARTESIAN_POINT('Ctrl Pts',(47.9122384136994,512.229997790525,-19.7221601716279)) ;
#46941 = CARTESIAN_POINT('Ctrl Pts',(47.9122384135884,512.229997790576,-19.9221601721307)) ;
#46942 = CARTESIAN_POINT('Ctrl Pts',(47.9122384134769,512.229997790623,-20.1221601726335)) ;
#46943 = CARTESIAN_POINT('Ctrl Pts',(49.0637330000058,512.163209431194,-19.5221601704647)) ;
#46944 = CARTESIAN_POINT('Ctrl Pts',(49.0637330000785,512.163209431207,-19.7221601709675)) ;
#46945 = CARTESIAN_POINT('Ctrl Pts',(49.0637330001476,512.163209431209,-19.9221601714703)) ;
#46946 = CARTESIAN_POINT('Ctrl Pts',(49.0637330002203,512.163209431222,-20.122160171973)) ;
#46947 = CARTESIAN_POINT('Ctrl Pts',(49.4331351147579,512.22166723942,-19.5221601702455)) ;
#46948 = CARTESIAN_POINT('Ctrl Pts',(49.4331351148848,512.22166723944,-19.7221601707483)) ;
#46949 = CARTESIAN_POINT('Ctrl Pts',(49.4331351150117,512.22166723946,-19.9221601712511)) ;
#46950 = CARTESIAN_POINT('Ctrl Pts',(49.4331351151386,512.22166723948,-20.1221601717539)) ;
#46951 = CARTESIAN_POINT('',(49.4331351147579,512.22166723942,-19.5221601717538)) ;
#46952 = CARTESIAN_POINT('',(48.6516117532324,517.160211684628,-20.2721601717537)) ;
#46953 = CARTESIAN_POINT('Origin',(44.9784504245142,540.371370334153,-19.5221601717536)) ;
#46954 = CARTESIAN_POINT('',(73.1281534675381,535.916685318467,-256.918732177554)) ;
#46955 = CARTESIAN_POINT('Origin',(70.658881270691,536.307447161963,-256.918732177554)) ;
#46956 = CARTESIAN_POINT('',(68.1896090740378,536.698209005427,-20.2721601717541)) ;
#46957 = CARTESIAN_POINT('Origin',(70.6588813175403,544.435293211585,-19.5221601717547)) ;
#46958 = CARTESIAN_POINT('',(68.189609074039,544.044531662871,-20.2721601717546)) ;
#46959 = CARTESIAN_POINT('Origin',(99.3135276254216,613.21056516055,-23.0221601717561)) ;
#46960 = CARTESIAN_POINT('',(-0.611472374578058,613.210565160567,-23.5221601717515)) ;
#46961 = CARTESIAN_POINT('',(99.3135276254216,613.21056516055,-23.5221601717561)) ;
#46962 = CARTESIAN_POINT('Origin',(-0.611472374578028,613.210565160567,-23.0221601717515)) ;
#46963 = CARTESIAN_POINT('Origin',(199.238527625403,506.210565160532,-23.5221601717606)) ;
#46964 = CARTESIAN_POINT('',(-0.611472374596327,509.210565160567,-23.5221601717515)) ;
#46965 = CARTESIAN_POINT('',(99.6885276254034,509.21056516055,-23.5221601717561)) ;
#46966 = CARTESIAN_POINT('',(-0.61147237459199,533.897292039156,-23.5221601717515)) ;
#46967 = CARTESIAN_POINT('Origin',(99.6885276254034,509.21056516055,-23.0221601717561)) ;
#46968 = CARTESIAN_POINT('',(-0.611472374596387,508.710565160568,-23.0221601717515)) ;
#46969 = CARTESIAN_POINT('',(99.6885276254033,508.71056516055,-23.0221601717561)) ;
#46970 = CARTESIAN_POINT('Origin',(-0.611472374596307,509.210565160567,-23.0221601717515)) ;
#46971 = CARTESIAN_POINT('Origin',(0.138527625403477,508.710565160567,-19.5221601717516)) ;
#46972 = CARTESIAN_POINT('',(-0.611472374596568,508.710565160568,-27.0096601717537)) ;
#46973 = CARTESIAN_POINT('',(0.238527625403442,508.710565160567,-19.5221601717516)) ;
#46974 = CARTESIAN_POINT('Origin',(196.238527625422,616.460565160533,-23.5221601717605)) ;
#46975 = CARTESIAN_POINT('Origin',(204.238527625403,507.060565160531,-25.4221601717608)) ;
#46976 = CARTESIAN_POINT('',(196.988527625403,506.560565160533,-25.4221601717605)) ;
#46977 = CARTESIAN_POINT('',(196.988527625403,507.060565160533,-25.9221601717605)) ;
#46978 = CARTESIAN_POINT('Origin',(196.988527625403,507.060565160533,-25.4221601717605)) ;
#46979 = CARTESIAN_POINT('',(197.588527625403,507.060565160533,-25.9221601717605)) ;
#46980 = CARTESIAN_POINT('',(204.238527625403,507.060565160531,-25.9221601717608)) ;
#46981 = CARTESIAN_POINT('',(197.588527625403,506.560565160533,-25.4221601717605)) ;
#46982 = CARTESIAN_POINT('Origin',(197.588527625403,507.060565160533,-25.4221601717605)) ;
#46983 = CARTESIAN_POINT('',(204.238527625403,506.560565160532,-25.4221601717608)) ;
#46984 = CARTESIAN_POINT('Origin',(208.388527625422,616.210565160531,-25.922160171761)) ;
#46985 = CARTESIAN_POINT('',(196.988527625422,615.360565160533,-25.9221601717605)) ;
#46986 = CARTESIAN_POINT('',(196.988527625422,616.210565160533,-25.9221601717605)) ;
#46987 = CARTESIAN_POINT('',(197.588527625422,615.360565160533,-25.9221601717605)) ;
#46988 = CARTESIAN_POINT('',(203.863527625422,615.360565160531,-25.9221601717608)) ;
#46989 = CARTESIAN_POINT('',(197.588527625422,616.068993308983,-25.9221601717605)) ;
#46990 = CARTESIAN_POINT('Origin',(196.988527625421,616.210565160533,-43.5221601717605)) ;
#46991 = CARTESIAN_POINT('',(196.988527625403,506.560565160533,-20.3721601717605)) ;
#46992 = CARTESIAN_POINT('',(196.988527625403,506.560565160533,-31.5221601717605)) ;
#46993 = CARTESIAN_POINT('',(196.988527625422,615.860565160533,-20.3721601717605)) ;
#46994 = CARTESIAN_POINT('',(196.988527625422,616.210565160533,-20.3721601717605)) ;
#46995 = CARTESIAN_POINT('',(196.988527625422,615.860565160533,-25.4221601717605)) ;
#46996 = CARTESIAN_POINT('',(196.988527625422,615.860565160533,-31.5221601717605)) ;
#46997 = CARTESIAN_POINT('Origin',(196.988527625422,615.360565160533,-25.4221601717605)) ;
#46998 = CARTESIAN_POINT('Origin',(203.863527625422,615.360565160531,-25.4221601717608)) ;
#46999 = CARTESIAN_POINT('',(197.588527625422,615.860565160533,-25.4221601717605)) ;
#47000 = CARTESIAN_POINT('Origin',(197.588527625422,615.360565160533,-25.4221601717605)) ;
#47001 = CARTESIAN_POINT('',(203.863527625422,615.860565160531,-25.4221601717608)) ;
#47002 = CARTESIAN_POINT('Origin',(199.338527625422,615.860565160532,-19.5221601717606)) ;
#47003 = CARTESIAN_POINT('',(197.588527625422,615.860565160533,-20.2721601717605)) ;
#47004 = CARTESIAN_POINT('Origin',(196.838527625422,615.860565160533,-20.2721601717605)) ;
#47005 = CARTESIAN_POINT('',(197.588527625422,615.860565160533,-20.2721601717605)) ;
#47006 = CARTESIAN_POINT('Origin',(196.738527625422,615.860565160533,-20.3721601717605)) ;
#47007 = CARTESIAN_POINT('',(196.738527625422,615.860565160533,-19.5221601717605)) ;
#47008 = CARTESIAN_POINT('Origin',(196.238527625412,561.210565160533,-23.5221601717605)) ;
#47009 = CARTESIAN_POINT('',(196.738527625412,561.210565160533,-23.5221601717605)) ;
#47010 = CARTESIAN_POINT('Origin',(196.738527625422,616.210565160533,-19.5221601717605)) ;
#47011 = CARTESIAN_POINT('Origin',(191.388264603412,561.460565160534,-27.5221601717602)) ;
#47012 = CARTESIAN_POINT('',(191.388264603412,561.460565160534,-28.5221601717602)) ;
#47013 = CARTESIAN_POINT('',(192.388264603412,561.460565160534,-27.5221601717602)) ;
#47014 = CARTESIAN_POINT('Origin',(199.238527625403,506.210565160532,-28.5221601717606)) ;
#47015 = CARTESIAN_POINT('',(183.388264603403,506.335565160535,-28.5221601717599)) ;
#47016 = CARTESIAN_POINT('Origin',(181.388264603403,506.460565160535,-25.0221601717598)) ;
#47017 = CARTESIAN_POINT('',(182.388264603403,506.460565160535,-25.0221601717598)) ;
#47018 = CARTESIAN_POINT('',(181.388264603403,506.460565160535,-24.0221601717598)) ;
#47019 = CARTESIAN_POINT('Origin',(182.388264603403,506.460565160535,-28.5221601717599)) ;
#47020 = CARTESIAN_POINT('',(182.388264603403,506.335565160535,-27.5221601717599)) ;
#47021 = CARTESIAN_POINT('Origin',(183.388264603403,506.335565160535,-27.5221601717599)) ;
#47022 = CARTESIAN_POINT('Origin',(10.4885276254026,506.335565160565,-27.522160171752)) ;
#47023 = CARTESIAN_POINT('',(10.4885276254026,506.335565160565,-28.522160171752)) ;
#47024 = CARTESIAN_POINT('',(11.4885276254026,506.335565160565,-27.522160171752)) ;
#47025 = CARTESIAN_POINT('Origin',(199.238527625403,506.210565160532,-28.5221601717606)) ;
#47026 = CARTESIAN_POINT('',(1.2385276254122,560.835565160567,-28.5221601717516)) ;
#47027 = CARTESIAN_POINT('Origin',(12.4885276254027,506.460565160565,-25.0221601717521)) ;
#47028 = CARTESIAN_POINT('',(12.4885276254027,506.460565160565,-24.0221601717521)) ;
#47029 = CARTESIAN_POINT('',(11.4885276254027,506.460565160565,-25.0221601717521)) ;
#47030 = CARTESIAN_POINT('Origin',(182.388264603403,506.460565160535,-24.0221601717598)) ;
#47031 = CARTESIAN_POINT('Origin',(1.23852762541224,560.835565160567,-27.5221601717516)) ;
#47032 = CARTESIAN_POINT('',(0.238527625412235,560.835565160567,-27.5221601717516)) ;
#47033 = CARTESIAN_POINT('Origin',(12.4885276254123,561.460565160565,-25.0221601717521)) ;
#47034 = CARTESIAN_POINT('',(11.4885276254123,561.460565160565,-25.0221601717521)) ;
#47035 = CARTESIAN_POINT('',(12.4885276254124,561.460565160565,-24.0221601717521)) ;
#47036 = CARTESIAN_POINT('Origin',(11.488527625422,616.710565160565,-28.5221601717516)) ;
#47037 = CARTESIAN_POINT('',(11.488527625422,616.710565160565,-27.5221601717516)) ;
#47038 = CARTESIAN_POINT('Origin',(10.488527625422,616.710565160565,-27.5221601717516)) ;
#47039 = CARTESIAN_POINT('',(10.488527625422,616.710565160565,-28.5221601717516)) ;
#47040 = CARTESIAN_POINT('Origin',(1.48852762542202,616.710565160567,-28.5221601717516)) ;
#47041 = CARTESIAN_POINT('',(1.23852762542194,616.085565160567,-28.5221601717516)) ;
#47042 = CARTESIAN_POINT('Origin',(1.23852762542194,616.085565160567,-27.5221601717516)) ;
#47043 = CARTESIAN_POINT('Origin',(181.388264603412,561.460565160536,-25.0221601717598)) ;
#47044 = CARTESIAN_POINT('',(182.388264603412,561.460565160535,-25.0221601717598)) ;
#47045 = CARTESIAN_POINT('',(181.388264603412,561.460565160536,-24.0221601717598)) ;
#47046 = CARTESIAN_POINT('Origin',(182.388264603422,616.710565160535,-28.5221601717598)) ;
#47047 = CARTESIAN_POINT('',(182.388264603422,616.710565160535,-27.5221601717598)) ;
#47048 = CARTESIAN_POINT('Origin',(183.388264603422,616.710565160535,-27.5221601717598)) ;
#47049 = CARTESIAN_POINT('',(183.388264603422,616.710565160535,-28.5221601717598)) ;
#47050 = CARTESIAN_POINT('Origin',(192.388264603422,616.710565160533,-24.0221601717603)) ;
#47051 = CARTESIAN_POINT('',(192.388264603422,616.710565160533,-27.5221601717598)) ;
#47052 = CARTESIAN_POINT('Origin',(191.388264603422,616.710565160534,-27.5221601717598)) ;
#47053 = CARTESIAN_POINT('',(191.388264603422,616.710565160534,-28.5221601717598)) ;
#47054 = CARTESIAN_POINT('Origin',(182.388264603422,616.710565160535,-28.5221601717598)) ;
#47055 = CARTESIAN_POINT('Origin',(196.738527625422,616.210565160533,-20.3721601717605)) ;
#47056 = CARTESIAN_POINT('Origin',(196.738527625403,506.560565160533,-20.3721601717605)) ;
#47057 = CARTESIAN_POINT('Origin',(200.088527625403,506.560565160532,-19.5221601717607)) ;
#47058 = CARTESIAN_POINT('',(197.588527625403,506.560565160533,-20.2721601717605)) ;
#47059 = CARTESIAN_POINT('',(197.588527625403,506.560565160533,-20.2721601717605)) ;
#47060 = CARTESIAN_POINT('Origin',(196.838527625403,506.560565160533,-20.2721601717605)) ;
#47061 = CARTESIAN_POINT('Origin',(0.238527625422194,615.460565160567,-19.5221601717516)) ;
#47062 = CARTESIAN_POINT('Origin',(192.388264603422,616.710565160533,-24.0221601717603)) ;
#47063 = CARTESIAN_POINT('Origin',(6.48852762542202,616.710565160566,-24.0221601717538)) ;
#47064 = CARTESIAN_POINT('',(7.73852762542202,616.710565160566,-24.0221601717538)) ;
#47065 = CARTESIAN_POINT('Origin',(187.388264603422,616.710565160534,-24.0203292412001)) ;
#47066 = CARTESIAN_POINT('',(188.638264603422,616.710565160534,-24.0203292412001)) ;
#47067 = CARTESIAN_POINT('Origin',(11.4885276254027,506.460565160565,-24.0221601717521)) ;
#47068 = CARTESIAN_POINT('Origin',(6.48852762542202,616.710565160566,-24.0221601717538)) ;
#47069 = CARTESIAN_POINT('',(7.73852762542202,616.710565160566,-24.0221601717538)) ;
#47070 = CARTESIAN_POINT('Origin',(29.2846442220398,550.16700440648,-256.918732177554)) ;
#47071 = CARTESIAN_POINT('',(31.8295857683906,548.578523205569,-19.5221601717539)) ;
#47072 = CARTESIAN_POINT('',(26.7397026756954,551.755485607418,-19.522160171754)) ;
#47073 = CARTESIAN_POINT('Origin',(29.2846442220421,530.575736261811,-256.918732177554)) ;
#47074 = CARTESIAN_POINT('',(26.7397026756914,528.987255060894,-19.5221601717534)) ;
#47075 = CARTESIAN_POINT('',(31.8295857683878,532.164217462742,-20.2721601717535)) ;
#47076 = CARTESIAN_POINT('Origin',(44.978450424514,540.371370334142,-256.918732177554)) ;
#47077 = CARTESIAN_POINT('Origin',(44.978450424514,540.371370334142,-256.918732177554)) ;
#47078 = CARTESIAN_POINT('Origin',(44.9784504245044,540.371370334145,-256.918732177554)) ;
#47079 = CARTESIAN_POINT('Origin',(19.8918523583282,565.591787908239,-19.6319951288125)) ;
#47080 = CARTESIAN_POINT('',(17.5016873153832,565.591787908239,-19.6319951288124)) ;
#47081 = CARTESIAN_POINT('Origin',(69.8918523583194,515.59178790823,-19.6319951288147)) ;
#47082 = CARTESIAN_POINT('',(67.5016873153744,515.59178790823,-19.6319951288146)) ;
#47083 = CARTESIAN_POINT('Origin',(199.238527625403,506.210565160532,-24.0221601717606)) ;
#47084 = CARTESIAN_POINT('Origin',(-0.61147237458762,561.584018917744,-34.4971601717558)) ;
#47085 = CARTESIAN_POINT('Origin',(44.983152306877,546.991619032405,-256.918732177554)) ;
#47086 = CARTESIAN_POINT('',(43.5689387445037,545.577405470032,-256.918732177554)) ;
#47087 = CARTESIAN_POINT('Origin',(38.4886965012279,540.50186510913,-256.918732177553)) ;
#47088 = CARTESIAN_POINT('',(37.0744829388546,539.087651546757,-256.918732177553)) ;
#47089 = CARTESIAN_POINT('Origin',(44.9784504244951,534.007409303474,-256.918732177554)) ;
#47090 = CARTESIAN_POINT('',(43.5642368621218,532.593195741101,-256.918732177554)) ;
#47091 = CARTESIAN_POINT('Origin',(51.4729062301583,540.497163226748,-256.918732177554)) ;
#47092 = CARTESIAN_POINT('',(50.058692667785,539.082949664375,-256.918732177554)) ;
#47093 = CARTESIAN_POINT('Origin',(174.088527625396,527.710565160537,-256.918732177559)) ;
#47094 = CARTESIAN_POINT('',(175.588527625407,527.710565160536,-19.5221601717595)) ;
#47095 = CARTESIAN_POINT('',(172.588527625407,527.710565160537,-20.2721601717594)) ;
#47096 = CARTESIAN_POINT('Origin',(175.588527625396,527.710565160536,-256.91873217756)) ;
#47097 = CARTESIAN_POINT('',(175.588527625411,549.710565160536,-20.2721601717595)) ;
#47098 = CARTESIAN_POINT('Origin',(174.0885276254,549.710565160537,-256.918732177559)) ;
#47099 = CARTESIAN_POINT('',(172.588527625411,549.710565160537,-19.5221601717594)) ;
#47100 = CARTESIAN_POINT('Origin',(172.5885276254,549.710565160537,-256.918732177559)) ;
#47101 = CARTESIAN_POINT('Origin',(167.0885276254,549.710565160538,-256.918732177559)) ;
#47102 = CARTESIAN_POINT('',(165.588527625411,549.710565160538,-19.5221601717591)) ;
#47103 = CARTESIAN_POINT('',(168.588527625411,549.710565160538,-20.2721601717592)) ;
#47104 = CARTESIAN_POINT('Origin',(165.5885276254,549.710565160538,-256.918732177559)) ;
#47105 = CARTESIAN_POINT('',(165.588527625407,527.710565160538,-20.2721601717591)) ;
#47106 = CARTESIAN_POINT('Origin',(167.088527625396,527.710565160538,-256.918732177559)) ;
#47107 = CARTESIAN_POINT('',(168.588527625407,527.710565160538,-19.5221601717592)) ;
#47108 = CARTESIAN_POINT('Origin',(168.588527625396,527.710565160538,-256.918732177559)) ;
#47109 = CARTESIAN_POINT('Origin',(160.088527625396,527.710565160539,-256.918732177559)) ;
#47110 = CARTESIAN_POINT('',(161.588527625407,527.710565160539,-19.5221601717589)) ;
#47111 = CARTESIAN_POINT('',(158.588527625407,527.710565160539,-20.2721601717588)) ;
#47112 = CARTESIAN_POINT('Origin',(161.588527625396,527.710565160539,-256.918732177559)) ;
#47113 = CARTESIAN_POINT('',(161.588527625411,549.710565160539,-20.2721601717589)) ;
#47114 = CARTESIAN_POINT('Origin',(160.0885276254,549.710565160539,-256.918732177559)) ;
#47115 = CARTESIAN_POINT('',(158.588527625411,549.710565160539,-19.5221601717588)) ;
#47116 = CARTESIAN_POINT('Origin',(158.5885276254,549.71056516054,-256.918732177559)) ;
#47117 = CARTESIAN_POINT('Origin',(174.088527625404,572.710565160537,-256.918732177559)) ;
#47118 = CARTESIAN_POINT('',(175.588527625415,572.710565160536,-19.5221601717595)) ;
#47119 = CARTESIAN_POINT('',(172.588527625415,572.710565160537,-20.2721601717594)) ;
#47120 = CARTESIAN_POINT('Origin',(175.588527625404,572.710565160536,-256.91873217756)) ;
#47121 = CARTESIAN_POINT('',(175.588527625419,594.710565160536,-20.2721601717595)) ;
#47122 = CARTESIAN_POINT('Origin',(174.088527625408,594.710565160537,-256.918732177559)) ;
#47123 = CARTESIAN_POINT('',(172.588527625419,594.710565160537,-19.5221601717594)) ;
#47124 = CARTESIAN_POINT('Origin',(172.588527625408,594.710565160537,-256.918732177559)) ;
#47125 = CARTESIAN_POINT('Origin',(167.088527625404,572.710565160538,-256.918732177559)) ;
#47126 = CARTESIAN_POINT('',(168.588527625415,572.710565160538,-19.5221601717592)) ;
#47127 = CARTESIAN_POINT('',(165.588527625415,572.710565160538,-20.2721601717591)) ;
#47128 = CARTESIAN_POINT('Origin',(168.588527625404,572.710565160538,-256.918732177559)) ;
#47129 = CARTESIAN_POINT('',(168.588527625419,594.710565160538,-20.2721601717592)) ;
#47130 = CARTESIAN_POINT('Origin',(167.088527625408,594.710565160538,-256.918732177559)) ;
#47131 = CARTESIAN_POINT('',(165.588527625419,594.710565160538,-19.5221601717591)) ;
#47132 = CARTESIAN_POINT('Origin',(165.588527625408,594.710565160538,-256.918732177559)) ;
#47133 = CARTESIAN_POINT('Origin',(160.088527625404,572.710565160539,-256.918732177559)) ;
#47134 = CARTESIAN_POINT('',(161.588527625415,572.710565160539,-19.5221601717589)) ;
#47135 = CARTESIAN_POINT('',(158.588527625415,572.710565160539,-20.2721601717588)) ;
#47136 = CARTESIAN_POINT('Origin',(161.588527625404,572.710565160539,-256.918732177559)) ;
#47137 = CARTESIAN_POINT('',(161.588527625419,594.710565160539,-20.2721601717589)) ;
#47138 = CARTESIAN_POINT('Origin',(160.088527625408,594.710565160539,-256.918732177559)) ;
#47139 = CARTESIAN_POINT('',(158.588527625419,594.710565160539,-19.5221601717588)) ;
#47140 = CARTESIAN_POINT('Origin',(158.588527625408,594.71056516054,-256.918732177559)) ;
#47141 = CARTESIAN_POINT('Origin',(196.838527625447,759.606565160533,-20.2721601717605)) ;
#47142 = CARTESIAN_POINT('',(197.588527625403,507.060565160533,-20.2721601717605)) ;
#47143 = CARTESIAN_POINT('Origin',(197.588527625422,615.927421457433,-27.7686821023705)) ;
#47144 = CARTESIAN_POINT('Origin',(187.388264603402,504.210565160534,-24.0203292412001)) ;
#47145 = CARTESIAN_POINT('',(186.138264631817,504.210565160534,-24.0200627128238)) ;
#47146 = CARTESIAN_POINT('Origin',(44.9784504245116,540.371370334154,-256.918732177554)) ;
#47147 = CARTESIAN_POINT('Origin',(44.9784504245024,540.371370334161,-256.918732177554)) ;
#47148 = CARTESIAN_POINT('Origin',(44.9784504244953,540.371370334152,-256.918732177554)) ;
#47149 = CARTESIAN_POINT('Origin',(35.1828163521764,524.67756413169,-256.918732177554)) ;
#47150 = CARTESIAN_POINT('',(36.7712975530987,527.22250567803,-19.5221601717541)) ;
#47151 = CARTESIAN_POINT('',(33.5943351512492,522.132622585334,-19.5221601717543)) ;
#47152 = CARTESIAN_POINT('Origin',(54.774084496846,524.677564131692,-256.918732177555)) ;
#47153 = CARTESIAN_POINT('',(56.362565697773,522.13262258533,-19.5221601717548)) ;
#47154 = CARTESIAN_POINT('',(53.1856032959251,527.222505678027,-20.2721601717544)) ;
#47155 = CARTESIAN_POINT('Origin',(44.9784504245142,540.371370334164,-256.918732177554)) ;
#47156 = CARTESIAN_POINT('Origin',(44.9784504245142,540.371370334164,-256.918732177554)) ;
#47157 = CARTESIAN_POINT('Origin',(60.672256626967,530.575736261826,-256.918732177555)) ;
#47158 = CARTESIAN_POINT('',(58.1273150806378,532.164217462738,-19.5221601717551)) ;
#47159 = CARTESIAN_POINT('',(63.217198173333,528.987255060888,-19.5221601717556)) ;
#47160 = CARTESIAN_POINT('Origin',(60.6722566269648,550.167004406496,-256.918732177555)) ;
#47161 = CARTESIAN_POINT('',(63.217198173337,551.755485607412,-19.5221601717551)) ;
#47162 = CARTESIAN_POINT('',(58.1273150806405,548.578523205564,-20.2721601717547)) ;
#47163 = CARTESIAN_POINT('Origin',(44.9784504244929,540.371370334164,-256.918732177554)) ;
#47164 = CARTESIAN_POINT('Origin',(44.9784504244929,540.371370334164,-256.918732177554)) ;
#47165 = CARTESIAN_POINT('Origin',(54.7740844968305,556.065176536617,-256.918732177555)) ;
#47166 = CARTESIAN_POINT('',(53.1856032959298,553.520234990277,-19.5221601717548)) ;
#47167 = CARTESIAN_POINT('',(56.3625656977793,558.610118082972,-19.5221601717553)) ;
#47168 = CARTESIAN_POINT('Origin',(35.1828163521609,556.065176536615,-256.918732177554)) ;
#47169 = CARTESIAN_POINT('',(33.5943351512555,558.610118082976,-19.5221601717537)) ;
#47170 = CARTESIAN_POINT('',(36.7712975531033,553.52023499028,-20.2721601717537)) ;
#47171 = CARTESIAN_POINT('Origin',(44.9784504244926,540.371370334143,-256.918732177554)) ;
#47172 = CARTESIAN_POINT('Origin',(44.9784504244926,540.371370334143,-256.918732177554)) ;
#47173 = CARTESIAN_POINT('',(0.,0.,0.)) ;
#47174 = CARTESIAN_POINT('',(0.,0.,0.)) ;
#47175 = CARTESIAN_POINT('',(0.,0.,0.)) ;
#47176 = CARTESIAN_POINT('Origin',(3.46944695195362E-16,1.71875,2.77555756156289E-16)) ;
#47177 = CARTESIAN_POINT('',(2.68827523286988E-13,-0.999999999999967,1.17524047358083)) ;
#47178 = CARTESIAN_POINT('',(2.03174352947591E-13,-1.06249999999997,1.17524047358083)) ;
#47179 = CARTESIAN_POINT('',(5.49963941970804E-16,1.71875,1.17524047358083)) ;
#47180 = CARTESIAN_POINT('',(-1.16245326511946,-1.17524047358083,0.172894699616842)) ;
#47181 = CARTESIAN_POINT('Ctrl Pts',(4.05798741953211E-13,-1.06249999999997,
1.17524047358083)) ;
#47182 = CARTESIAN_POINT('Ctrl Pts',(-0.105160340523186,-1.06895765188846,
1.17524047358083)) ;
#47183 = CARTESIAN_POINT('Ctrl Pts',(-0.210026376843711,-1.07589739920494,
1.16113285033081)) ;
#47184 = CARTESIAN_POINT('Ctrl Pts',(-0.461547030634828,-1.09379678097625,
1.09191353201678)) ;
#47185 = CARTESIAN_POINT('Ctrl Pts',(-0.601609669732423,-1.10489587260588,
1.02145069830121)) ;
#47186 = CARTESIAN_POINT('Ctrl Pts',(-0.841642087198107,-1.1262899253027,
0.833763281857878)) ;
#47187 = CARTESIAN_POINT('Ctrl Pts',(-0.94076791668668,-1.13640781439979,
0.72007138829596)) ;
#47188 = CARTESIAN_POINT('Ctrl Pts',(-1.09077083296657,-1.15476396114588,
0.462134782296477)) ;
#47189 = CARTESIAN_POINT('Ctrl Pts',(-1.14052623621597,-1.16478687965435,
0.32032053973826)) ;
#47190 = CARTESIAN_POINT('Ctrl Pts',(-1.16245326511978,-1.17524047358099,
0.172894699614671)) ;
#47191 = CARTESIAN_POINT('',(-0.943477955795636,-1.17524047358083,-0.700742119235164)) ;
#47192 = CARTESIAN_POINT('Origin',(8.46545056276682E-15,-1.17524047358084,
1.90819582357449E-15)) ;
#47193 = CARTESIAN_POINT('Ctrl Pts',(-0.943477955795635,-1.17524047358084,
-0.700742119235159)) ;
#47194 = CARTESIAN_POINT('Ctrl Pts',(-1.02492263848393,-1.16635139543542,
-0.591085141833767)) ;
#47195 = CARTESIAN_POINT('Ctrl Pts',(-1.08661800606201,-1.15819168045143,
-0.468098475031939)) ;
#47196 = CARTESIAN_POINT('Ctrl Pts',(-1.16970670338323,-1.13852263168986,
-0.190708128854841)) ;
#47197 = CARTESIAN_POINT('Ctrl Pts',(-1.1845688827545,-1.12762622677339,-0.0370373759624758)) ;
#47198 = CARTESIAN_POINT('Ctrl Pts',(-1.15431629966392,-1.10583767984718,
0.270244010535864)) ;
#47199 = CARTESIAN_POINT('Ctrl Pts',(-1.10834405084586,-1.09516180730449,
0.420804620571442)) ;
#47200 = CARTESIAN_POINT('Ctrl Pts',(-0.963542949730392,-1.07613113704493,
0.689191987712228)) ;
#47201 = CARTESIAN_POINT('Ctrl Pts',(-0.868446230221078,-1.06642890978637,
0.8057548264429)) ;
#47202 = CARTESIAN_POINT('Ctrl Pts',(-0.635333585436618,-1.04520090824001,
1.00074403996173)) ;
#47203 = CARTESIAN_POINT('Ctrl Pts',(-0.498182457666835,-1.03412422046949,
1.07561784109633)) ;
#47204 = CARTESIAN_POINT('Ctrl Pts',(-0.236805129209574,-1.01517846693789,
1.15727862072953)) ;
#47205 = CARTESIAN_POINT('Ctrl Pts',(-0.118658074201543,-1.00728651631539,
1.17524047358083)) ;
#47206 = CARTESIAN_POINT('Ctrl Pts',(5.37157124336218E-13,-0.999999999999967,
1.17524047358083)) ;
#47207 = CARTESIAN_POINT('Origin',(3.46944695195362E-16,1.71875,2.77555756156289E-16)) ;
#47208 = CARTESIAN_POINT('',(6.06086644654604E-14,-0.499999999999992,1.17524047358083)) ;
#47209 = CARTESIAN_POINT('',(2.08586854750403E-13,-0.562499999999971,1.17524047358083)) ;
#47210 = CARTESIAN_POINT('',(5.49963941970804E-16,1.71875,1.17524047358083)) ;
#47211 = CARTESIAN_POINT('Ctrl Pts',(4.16923440216266E-13,-0.562499999999972,
1.17524047358083)) ;
#47212 = CARTESIAN_POINT('Ctrl Pts',(-0.127484578485998,-0.570328531411307,
1.17524047358083)) ;
#47213 = CARTESIAN_POINT('Ctrl Pts',(-0.254283442227845,-0.578850073610016,
1.15450587698244)) ;
#47214 = CARTESIAN_POINT('Ctrl Pts',(-0.5217889700627,-0.598474486389227,
1.06431734245669)) ;
#47215 = CARTESIAN_POINT('Ctrl Pts',(-0.656966876910855,-0.609529920381951,
0.986625301628538)) ;
#47216 = CARTESIAN_POINT('Ctrl Pts',(-0.885467738610519,-0.630639702939782,
0.786982703254743)) ;
#47217 = CARTESIAN_POINT('Ctrl Pts',(-0.977970250751646,-0.640095776533645,
0.668536344435955)) ;
#47218 = CARTESIAN_POINT('Ctrl Pts',(-1.11701382207316,-0.659333626638224,
0.397227143624959)) ;
#47219 = CARTESIAN_POINT('Ctrl Pts',(-1.15979113888618,-0.670077776473707,
0.245703626734443)) ;
#47220 = CARTESIAN_POINT('Ctrl Pts',(-1.18349158051387,-0.691886539798171,
-0.0618628693174395)) ;
#47221 = CARTESIAN_POINT('Ctrl Pts',(-1.1654693373561,-0.702736099361235,
-0.214872967545919)) ;
#47222 = CARTESIAN_POINT('Ctrl Pts',(-1.07274162977296,-0.723158461972726,
-0.502887212831953)) ;
#47223 = CARTESIAN_POINT('Ctrl Pts',(-0.999931264413838,-0.731959214886923,
-0.635457257089622)) ;
#47224 = CARTESIAN_POINT('Ctrl Pts',(-0.803974158692238,-0.752358883134125,
-0.871437972397242)) ;
#47225 = CARTESIAN_POINT('Ctrl Pts',(-0.680675739361065,-0.763452971793481,
-0.970796173861973)) ;
#47226 = CARTESIAN_POINT('Ctrl Pts',(-0.40768984714355,-0.785241465149558,
-1.11253200080152)) ;
#47227 = CARTESIAN_POINT('Ctrl Pts',(-0.261667978082255,-0.795736410110075,
-1.15563272262566)) ;
#47228 = CARTESIAN_POINT('Ctrl Pts',(0.0417334207484942,-0.815392380307785,
-1.18453788613565)) ;
#47229 = CARTESIAN_POINT('Ctrl Pts',(0.196297491712523,-0.824778579904694,
-1.16891088513489)) ;
#47230 = CARTESIAN_POINT('Ctrl Pts',(0.491595152909961,-0.846111929617692,
-1.07865785321067)) ;
#47231 = CARTESIAN_POINT('Ctrl Pts',(0.62928314668341,-0.857193583476491,
-1.00457385892074)) ;
#47232 = CARTESIAN_POINT('Ctrl Pts',(0.863670959414044,-0.87845389091461,
-0.810882088475935)) ;
#47233 = CARTESIAN_POINT('Ctrl Pts',(0.959488170589128,-0.888230928035835,
-0.694836089616553)) ;
#47234 = CARTESIAN_POINT('Ctrl Pts',(1.10587053390409,-0.907204032554159,
-0.4272605655436)) ;
#47235 = CARTESIAN_POINT('Ctrl Pts',(1.15271823191445,-0.917860247976333,
-0.276977177631598)) ;
#47236 = CARTESIAN_POINT('Ctrl Pts',(1.18477406093944,-0.93964147802051,0.0302010197158971)) ;
#47237 = CARTESIAN_POINT('Ctrl Pts',(1.17078511730657,-0.950549976117892,
0.18404232135617)) ;
#47238 = CARTESIAN_POINT('Ctrl Pts',(1.08561597823129,-0.971132107238879,
0.474309763667351)) ;
#47239 = CARTESIAN_POINT('Ctrl Pts',(1.01658369044885,-0.979975436753446,
0.608346112577959)) ;
#47240 = CARTESIAN_POINT('Ctrl Pts',(0.82715575640286,-1.00015916197285,0.849544845288862)) ;
#47241 = CARTESIAN_POINT('Ctrl Pts',(0.706221498175738,-1.01123358263976,
0.9524431430051)) ;
#47242 = CARTESIAN_POINT('Ctrl Pts',(0.436336729474218,-1.03309702358497,
1.10166422799825)) ;
#47243 = CARTESIAN_POINT('Ctrl Pts',(0.291099603261814,-1.04368051403565,
1.14862165815867)) ;
#47244 = CARTESIAN_POINT('Ctrl Pts',(0.0940702185782331,-1.0566233702501,
1.17241999650976)) ;
#47245 = CARTESIAN_POINT('Ctrl Pts',(0.0470118755424141,-1.05961311008155,
1.17524047358083)) ;
#47246 = CARTESIAN_POINT('Ctrl Pts',(4.05798741953211E-13,-1.06249999999997,
1.17524047358083)) ;
#47247 = CARTESIAN_POINT('Ctrl Pts',(5.37105082632005E-13,-0.999999999999967,
1.17524047358083)) ;
#47248 = CARTESIAN_POINT('Ctrl Pts',(0.034994624013179,-0.997851061543523,
1.17524047358083)) ;
#47249 = CARTESIAN_POINT('Ctrl Pts',(0.0700269035290348,-0.995644399133693,
1.17367754619314)) ;
#47250 = CARTESIAN_POINT('Ctrl Pts',(0.255196528980468,-0.983684703017166,
1.15706829122464)) ;
#47251 = CARTESIAN_POINT('Ctrl Pts',(0.40137680267713,-0.973210034697463,
1.11481385257197)) ;
#47252 = CARTESIAN_POINT('Ctrl Pts',(0.67501512213282,-0.951439899620111,
0.974725872169565)) ;
#47253 = CARTESIAN_POINT('Ctrl Pts',(0.798818187161842,-0.94034255841405,
0.876150002104573)) ;
#47254 = CARTESIAN_POINT('Ctrl Pts',(0.996198613610554,-0.919896337867135,
0.641321507089482)) ;
#47255 = CARTESIAN_POINT('Ctrl Pts',(1.06983935303753,-0.91109670451278,0.509067697275494)) ;
#47256 = CARTESIAN_POINT('Ctrl Pts',(1.16420733489943,-0.890709556561418,
0.221550080315643)) ;
#47257 = CARTESIAN_POINT('Ctrl Pts',(1.18310120566659,-0.879873775266811,
0.0687342954321408)) ;
#47258 = CARTESIAN_POINT('Ctrl Pts',(1.16121537941864,-0.858061178187506,
-0.238886267625975)) ;
#47259 = CARTESIAN_POINT('Ctrl Pts',(1.11932676411979,-0.847298992122945,
-0.390664147393342)) ;
#47260 = CARTESIAN_POINT('Ctrl Pts',(0.98188157937219,-0.82800430468036,-0.66277491868477)) ;
#47261 = CARTESIAN_POINT('Ctrl Pts',(0.890091424208338,-0.818609335264536,
-0.781744819650761)) ;
#47262 = CARTESIAN_POINT('Ctrl Pts',(0.662862137417937,-0.797532518884636,
-0.982660013895455)) ;
#47263 = CARTESIAN_POINT('Ctrl Pts',(0.52823683319041,-0.786483846628287,
-1.06111847054872)) ;
#47264 = CARTESIAN_POINT('Ctrl Pts',(0.235245724512628,-0.764918500588585,
-1.16191020397607)) ;
#47265 = CARTESIAN_POINT('Ctrl Pts',(0.079661845817216,-0.755159707229693,
-1.18279563163626)) ;
#47266 = CARTESIAN_POINT('Ctrl Pts',(-0.225576153538807,-0.735719496716491,
-1.16315722188047)) ;
#47267 = CARTESIAN_POINT('Ctrl Pts',(-0.372417354987327,-0.725341292371487,
-1.12476838448958)) ;
#47268 = CARTESIAN_POINT('Ctrl Pts',(-0.648908395040247,-0.703663698131644,
-0.992231646806144)) ;
#47269 = CARTESIAN_POINT('Ctrl Pts',(-0.774952444899368,-0.692556326854877,
-0.897254370444777)) ;
#47270 = CARTESIAN_POINT('Ctrl Pts',(-0.978796169553678,-0.671901054676124,
-0.667724173774915)) ;
#47271 = CARTESIAN_POINT('Ctrl Pts',(-1.05623767831092,-0.663070027598576,
-0.536897247170042)) ;
#47272 = CARTESIAN_POINT('Ctrl Pts',(-1.15802196864285,-0.642844330631431,
-0.251656554984033)) ;
#47273 = CARTESIAN_POINT('Ctrl Pts',(-1.18083758299913,-0.632075194358561,
-0.0997806572234279)) ;
#47274 = CARTESIAN_POINT('Ctrl Pts',(-1.16715611539121,-0.61025481693953,
0.207949631076429)) ;
#47275 = CARTESIAN_POINT('Ctrl Pts',(-1.12930643333218,-0.599415818249439,
0.36081079052065)) ;
#47276 = CARTESIAN_POINT('Ctrl Pts',(-0.999113353668091,-0.579867007316284,
0.636505436348943)) ;
#47277 = CARTESIAN_POINT('Ctrl Pts',(-0.91051501700737,-0.5707104587482,0.757855711459888)) ;
#47278 = CARTESIAN_POINT('Ctrl Pts',(-0.689007310642716,-0.549783887762853,
0.964443186454003)) ;
#47279 = CARTESIAN_POINT('Ctrl Pts',(-0.556912270785791,-0.538770378599761,
1.04629238738483)) ;
#47280 = CARTESIAN_POINT('Ctrl Pts',(-0.280645631337244,-0.51813092533833,
1.14993623123353)) ;
#47281 = CARTESIAN_POINT('Ctrl Pts',(-0.140822819567578,-0.508647601768867,
1.17524047358083)) ;
#47282 = CARTESIAN_POINT('Ctrl Pts',(1.20840837336544E-13,-0.499999999999992,
1.17524047358083)) ;
#47283 = CARTESIAN_POINT('Origin',(3.46944695195362E-16,1.71875,2.77555756156289E-16)) ;
#47284 = CARTESIAN_POINT('',(-2.44853388629818E-15,-6.93889390390722E-17,
1.17524047358083)) ;
#47285 = CARTESIAN_POINT('',(3.05062464863285E-15,-0.0624999999999969,1.17524047358083)) ;
#47286 = CARTESIAN_POINT('',(5.49963941970804E-16,1.71875,1.17524047358083)) ;
#47287 = CARTESIAN_POINT('Ctrl Pts',(5.48172618408671E-15,-0.0624999999999969,
1.17524047358083)) ;
#47288 = CARTESIAN_POINT('Ctrl Pts',(-0.148863756462329,-0.0716413769988075,
1.17524047358083)) ;
#47289 = CARTESIAN_POINT('Ctrl Pts',(-0.296501321439185,-0.0817101361724437,
1.14695911803628)) ;
#47290 = CARTESIAN_POINT('Ctrl Pts',(-0.577730398749481,-0.102952751434487,
1.03489781920761)) ;
#47291 = CARTESIAN_POINT('Ctrl Pts',(-0.70791218174543,-0.113935392844471,
0.950605408972408)) ;
#47292 = CARTESIAN_POINT('Ctrl Pts',(-0.925193050987279,-0.134749025784293,
0.739882342016849)) ;
#47293 = CARTESIAN_POINT('Ctrl Pts',(-1.0114453570678,-0.14376812017929,0.616745701812903)) ;
#47294 = CARTESIAN_POINT('Ctrl Pts',(-1.13621629707524,-0.163502857584925,
0.338428956197801)) ;
#47295 = CARTESIAN_POINT('Ctrl Pts',(-1.17104173892086,-0.174393915887241,
0.184833605993659)) ;
#47296 = CARTESIAN_POINT('Ctrl Pts',(-1.17862495251038,-0.196209933636515,
-0.122835198382013)) ;
#47297 = CARTESIAN_POINT('Ctrl Pts',(-1.15291451538109,-0.206924918680573,
-0.273947407553108)) ;
#47298 = CARTESIAN_POINT('Ctrl Pts',(-1.04561263009304,-0.227028131315171,
-0.557460717199303)) ;
#47299 = CARTESIAN_POINT('Ctrl Pts',(-0.965292388987877,-0.235921747370174,
-0.687227250187395)) ;
#47300 = CARTESIAN_POINT('Ctrl Pts',(-0.756612097192965,-0.256730841667062,
-0.912718938330612)) ;
#47301 = CARTESIAN_POINT('Ctrl Pts',(-0.628946947889343,-0.267840570816339,
-1.00495489370288)) ;
#47302 = CARTESIAN_POINT('Ctrl Pts',(-0.350441736832899,-0.289438994590288,
-1.13176992081311)) ;
#47303 = CARTESIAN_POINT('Ctrl Pts',(-0.203169603775975,-0.299740292845399,
-1.16724316717551)) ;
#47304 = CARTESIAN_POINT('Ctrl Pts',(0.10316988606121,-0.319043810491533,
-1.18111821169802)) ;
#47305 = CARTESIAN_POINT('Ctrl Pts',(0.259406451010041,-0.329079654765264,
-1.15690367490604)) ;
#47306 = CARTESIAN_POINT('Ctrl Pts',(0.550860524019585,-0.350784890316052,
-1.04950402604207)) ;
#47307 = CARTESIAN_POINT('Ctrl Pts',(0.683499565536527,-0.361806520981249,
-0.968367990394277)) ;
#47308 = CARTESIAN_POINT('Ctrl Pts',(0.906224147383343,-0.38276530379844,
-0.762979645997387)) ;
#47309 = CARTESIAN_POINT('Ctrl Pts',(0.995499624165027,-0.39196753531454,
-0.642139144322849)) ;
#47310 = CARTESIAN_POINT('Ctrl Pts',(1.12724342088431,-0.411462527709364,
-0.367203495188301)) ;
#47311 = CARTESIAN_POINT('Ctrl Pts',(1.16595749631123,-0.422285793008895,
-0.214564221952573)) ;
#47312 = CARTESIAN_POINT('Ctrl Pts',(1.18138899932835,-0.444105823735235,
0.0931611769798911)) ;
#47313 = CARTESIAN_POINT('Ctrl Pts',(1.15940729477125,-0.454889773301367,
0.245245984921959)) ;
#47314 = CARTESIAN_POINT('Ctrl Pts',(1.05920543522115,-0.475150194460935,
0.530976388424197)) ;
#47315 = CARTESIAN_POINT('Ctrl Pts',(0.98258090411365,-0.483969534936611,
0.662108179213888)) ;
#47316 = CARTESIAN_POINT('Ctrl Pts',(0.780120151233503,-0.50458038576238,
0.892780814735941)) ;
#47317 = CARTESIAN_POINT('Ctrl Pts',(0.654548434337712,-0.515686268917954,
0.988534222181722)) ;
#47318 = CARTESIAN_POINT('Ctrl Pts',(0.378652346208475,-0.537384930557364,
1.12269566908047)) ;
#47319 = CARTESIAN_POINT('Ctrl Pts',(0.231944420472717,-0.547784377265534,
1.16191450401602)) ;
#47320 = CARTESIAN_POINT('Ctrl Pts',(0.0545377800954748,-0.559117348409257,
1.1742923822592)) ;
#47321 = CARTESIAN_POINT('Ctrl Pts',(0.0272552647469167,-0.560826317592848,
1.17524047358083)) ;
#47322 = CARTESIAN_POINT('Ctrl Pts',(4.16623745558835E-13,-0.562499999999971,
1.17524047358083)) ;
#47323 = CARTESIAN_POINT('Ctrl Pts',(1.2066736498895E-13,-0.499999999999993,
1.17524047358083)) ;
#47324 = CARTESIAN_POINT('Ctrl Pts',(0.0157279213843709,-0.499034184933935,
1.17524047358083)) ;
#47325 = CARTESIAN_POINT('Ctrl Pts',(0.0314669663668242,-0.498056493301619,
1.17492475250529)) ;
#47326 = CARTESIAN_POINT('Ctrl Pts',(0.197158826179065,-0.487645584755661,
1.16826376594166)) ;
#47327 = CARTESIAN_POINT('Ctrl Pts',(0.344536563790507,-0.477365486927465,
1.13357140642765)) ;
#47328 = CARTESIAN_POINT('Ctrl Pts',(0.623561267562816,-0.455789628905362,
1.00829265153272)) ;
#47329 = CARTESIAN_POINT('Ctrl Pts',(0.751650560225984,-0.444680024415349,
0.916794850119542)) ;
#47330 = CARTESIAN_POINT('Ctrl Pts',(0.961620797812825,-0.423830315427508,
0.692391844939811)) ;
#47331 = CARTESIAN_POINT('Ctrl Pts',(1.04271468875434,-0.414914304009938,
0.562906866567344)) ;
#47332 = CARTESIAN_POINT('Ctrl Pts',(1.15148401473377,-0.394844034949927,
0.279858156387584)) ;
#47333 = CARTESIAN_POINT('Ctrl Pts',(1.17796078895353,-0.384144101172343,
0.128958213506981)) ;
#47334 = CARTESIAN_POINT('Ctrl Pts',(1.1719980207065,-0.362330698347518,-0.178673712888099)) ;
#47335 = CARTESIAN_POINT('Ctrl Pts',(1.13797935938651,-0.351426530807025,
-0.33245394117964)) ;
#47336 = CARTESIAN_POINT('Ctrl Pts',(1.01465442966734,-0.331642805467273,
-0.611461558029465)) ;
#47337 = CARTESIAN_POINT('Ctrl Pts',(0.929022334265141,-0.322654585934169,
-0.735075718348283)) ;
#47338 = CARTESIAN_POINT('Ctrl Pts',(0.712861370794559,-0.301871144438001,
-0.946886946042434)) ;
#47339 = CARTESIAN_POINT('Ctrl Pts',(0.58319249722894,-0.290897365638977,
-1.03181776469222)) ;
#47340 = CARTESIAN_POINT('Ctrl Pts',(0.29630395858214,-0.269163983384795,
-1.14791905051678)) ;
#47341 = CARTESIAN_POINT('Ctrl Pts',(0.141606825355615,-0.25875931516526,
-1.17703349823979)) ;
#47342 = CARTESIAN_POINT('Ctrl Pts',(-0.163814445446772,-0.2398735308139,
-1.17335054150085)) ;
#47343 = CARTESIAN_POINT('Ctrl Pts',(-0.311702081140799,-0.22971536530763,
-1.14298054656693)) ;
#47344 = CARTESIAN_POINT('Ctrl Pts',(-0.593450382682682,-0.208274771929066,
-1.0262344449978)) ;
#47345 = CARTESIAN_POINT('Ctrl Pts',(-0.723811054306731,-0.197171609466349,
-0.938852489697176)) ;
#47346 = CARTESIAN_POINT('Ctrl Pts',(-0.940882920239149,-0.176101524754104,
-0.720533998331314)) ;
#47347 = CARTESIAN_POINT('Ctrl Pts',(-1.02628296898357,-0.167019286382454,
-0.592593192331669)) ;
#47348 = CARTESIAN_POINT('Ctrl Pts',(-1.14310264626327,-0.147132496588164,
-0.312132069261559)) ;
#47349 = CARTESIAN_POINT('Ctrl Pts',(-1.17375434493936,-0.136519917593742,
-0.162464080901736)) ;
#47350 = CARTESIAN_POINT('Ctrl Pts',(-1.17667790497532,-0.114633942569097,
0.146191322931168)) ;
#47351 = CARTESIAN_POINT('Ctrl Pts',(-1.14656204074406,-0.103568168772267,
0.302250665781474)) ;
#47352 = CARTESIAN_POINT('Ctrl Pts',(-1.0297060599707,-0.0834604539426645,
0.585827469369135)) ;
#47353 = CARTESIAN_POINT('Ctrl Pts',(-0.947044314185684,-0.0745879331365558,
0.711759154062011)) ;
#47354 = CARTESIAN_POINT('Ctrl Pts',(-0.73625789154082,-0.053950906669795,
0.928749610689681)) ;
#47355 = CARTESIAN_POINT('Ctrl Pts',(-0.609083798106053,-0.0430235742996687,
1.01669145792555)) ;
#47356 = CARTESIAN_POINT('Ctrl Pts',(-0.325737152011206,-0.0212557872096278,
1.13989789653917)) ;
#47357 = CARTESIAN_POINT('Ctrl Pts',(-0.171855723771338,-0.0106321681509957,
1.17301481473308)) ;
#47358 = CARTESIAN_POINT('Ctrl Pts',(-0.0106387770903632,-0.000654582620188146,
1.17520436830659)) ;
#47359 = CARTESIAN_POINT('Ctrl Pts',(-0.00531867141127997,-0.000326607239120388,
1.17524047358083)) ;
#47360 = CARTESIAN_POINT('Ctrl Pts',(-5.44703171456717E-15,3.46944695195361E-17,
1.17524047358083)) ;
#47361 = CARTESIAN_POINT('Origin',(3.46944695195362E-16,1.71875,2.77555756156289E-16)) ;
#47362 = CARTESIAN_POINT('',(-1.88715537221405E-13,0.499999999999977,1.17524047358083)) ;
#47363 = CARTESIAN_POINT('',(-8.32241523838793E-14,0.437499999999993,1.17524047358083)) ;
#47364 = CARTESIAN_POINT('',(5.49963941970804E-16,1.71875,1.17524047358083)) ;
#47365 = CARTESIAN_POINT('Ctrl Pts',(-1.66998268709729E-13,0.437499999999993,
1.17524047358083)) ;
#47366 = CARTESIAN_POINT('Ctrl Pts',(-0.017816889025783,0.436405906290418,
1.17524047358083)) ;
#47367 = CARTESIAN_POINT('Ctrl Pts',(-0.0356475927526497,0.435296599925478,
1.17483531666615)) ;
#47368 = CARTESIAN_POINT('Ctrl Pts',(-0.203474498162529,0.424719704494279,
1.16719054941927)) ;
#47369 = CARTESIAN_POINT('Ctrl Pts',(-0.35074116224463,0.414417337248731,
1.13167767881478)) ;
#47370 = CARTESIAN_POINT('Ctrl Pts',(-0.629219788395705,0.392817783737344,
1.00478474018186)) ;
#47371 = CARTESIAN_POINT('Ctrl Pts',(-0.756863302708354,0.381708056764137,
0.912511373283748)) ;
#47372 = CARTESIAN_POINT('Ctrl Pts',(-0.965478079711285,0.36090102991899,
0.686964524263308)) ;
#47373 = CARTESIAN_POINT('Ctrl Pts',(-1.04575909549831,0.352008487250049,
0.557183679194484)) ;
#47374 = CARTESIAN_POINT('Ctrl Pts',(-1.15298640618235,0.331903604566664,
0.273646817041186)) ;
#47375 = CARTESIAN_POINT('Ctrl Pts',(-1.17865785708671,0.321187861874008,
0.12252392283852)) ;
#47376 = CARTESIAN_POINT('Ctrl Pts',(-1.17099227410892,0.29937172754926,-0.185146525587731)) ;
#47377 = CARTESIAN_POINT('Ctrl Pts',(-1.13612585809603,0.288481343739001,
-0.338732363507496)) ;
#47378 = CARTESIAN_POINT('Ctrl Pts',(-1.01128147694235,0.268749101102935,
-0.617013925672573)) ;
#47379 = CARTESIAN_POINT('Ctrl Pts',(-0.92499761161151,0.259728374148979,
-0.740126326392309)) ;
#47380 = CARTESIAN_POINT('Ctrl Pts',(-0.707659781494743,0.238913208577674,
-0.950793963271697)) ;
#47381 = CARTESIAN_POINT('Ctrl Pts',(-0.577451976646021,0.227930124001106,
-1.03505380219116)) ;
#47382 = CARTESIAN_POINT('Ctrl Pts',(-0.289830594901794,0.206207888071383,
-1.14957137585777)) ;
#47383 = CARTESIAN_POINT('Ctrl Pts',(-0.134961808647696,0.19587901894077,
-1.17781645643573)) ;
#47384 = CARTESIAN_POINT('Ctrl Pts',(0.170536816874875,0.176927135094982,
-1.17240309477512)) ;
#47385 = CARTESIAN_POINT('Ctrl Pts',(0.31833195220016,0.166743801259716,-1.14116299236951)) ;
#47386 = CARTESIAN_POINT('Ctrl Pts',(0.599552627745338,0.145274570737449,
-1.02269528303885)) ;
#47387 = CARTESIAN_POINT('Ctrl Pts',(0.729466435647479,0.134169329798734,
-0.934480712049055)) ;
#47388 = CARTESIAN_POINT('Ctrl Pts',(0.945113748484863,0.113143004552156,
-0.714929091828199)) ;
#47389 = CARTESIAN_POINT('Ctrl Pts',(1.02964344740617,0.104099930553232,-0.586679065011666)) ;
#47390 = CARTESIAN_POINT('Ctrl Pts',(1.14485192050447,0.0841760461180767,
-0.305694800461991)) ;
#47391 = CARTESIAN_POINT('Ctrl Pts',(1.17467217794547,0.0735453415167243,
-0.155771188739705)) ;
#47392 = CARTESIAN_POINT('Ctrl Pts',(1.17581487774868,0.0516459156569779,
0.153073910682973)) ;
#47393 = CARTESIAN_POINT('Ctrl Pts',(1.14476153163351,0.0405861484727693,
0.30904854296214)) ;
#47394 = CARTESIAN_POINT('Ctrl Pts',(1.02619522438653,0.020527234767995,0.591937109865149)) ;
#47395 = CARTESIAN_POINT('Ctrl Pts',(0.942830977195143,0.0116321861240577,
0.717316136360187)) ;
#47396 = CARTESIAN_POINT('Ctrl Pts',(0.729193137971309,-0.00919364706669305,
0.934693233888779)) ;
#47397 = CARTESIAN_POINT('Ctrl Pts',(0.599257568047615,-0.0202987964095113,
1.02286752841867)) ;
#47398 = CARTESIAN_POINT('Ctrl Pts',(0.318011099999538,-0.0417666563563344,
1.14125190568622)) ;
#47399 = CARTESIAN_POINT('Ctrl Pts',(0.170211367213076,-0.0519487785066309,
1.1724498685463)) ;
#47400 = CARTESIAN_POINT('Ctrl Pts',(0.0136645921220641,-0.0616587775845467,
1.17518091428279)) ;
#47401 = CARTESIAN_POINT('Ctrl Pts',(0.00683113258147283,-0.0620805160386885,
1.17524047358083)) ;
#47402 = CARTESIAN_POINT('Ctrl Pts',(5.55128535529489E-15,-0.0624999999999967,
1.17524047358083)) ;
#47403 = CARTESIAN_POINT('Ctrl Pts',(-5.58580959264532E-15,-1.30104260698261E-17,
1.17524047358083)) ;
#47404 = CARTESIAN_POINT('Ctrl Pts',(0.150387712606244,0.00923495960059556,
1.17524047358083)) ;
#47405 = CARTESIAN_POINT('Ctrl Pts',(0.299504882175791,0.0194152486344145,
1.14637608262904)) ;
#47406 = CARTESIAN_POINT('Ctrl Pts',(0.581649964952125,0.0407716668309997,
1.03269145225507)) ;
#47407 = CARTESIAN_POINT('Ctrl Pts',(0.711464153498591,0.0517479810585996,
0.947940812816467)) ;
#47408 = CARTESIAN_POINT('Ctrl Pts',(0.927941859614262,0.0725399728462657,
0.736437031909328)) ;
#47409 = CARTESIAN_POINT('Ctrl Pts',(1.01374931713132,0.0815366885848531,
0.612958112291061)) ;
#47410 = CARTESIAN_POINT('Ctrl Pts',(1.13748362488098,0.10130657063834,0.33414572572495)) ;
#47411 = CARTESIAN_POINT('Ctrl Pts',(1.17173069626048,0.112207059875292,0.180417372127794)) ;
#47412 = CARTESIAN_POINT('Ctrl Pts',(1.17815196237782,0.134021264674389,-0.127225864418774)) ;
#47413 = CARTESIAN_POINT('Ctrl Pts',(1.15189189723141,0.144725485355728,-0.278186265012975)) ;
#47414 = CARTESIAN_POINT('Ctrl Pts',(1.04353784532397,0.164805092867427,-0.561366674309399)) ;
#47415 = CARTESIAN_POINT('Ctrl Pts',(0.962663238417732,0.173714520435076,
-0.690931317950019)) ;
#47416 = CARTESIAN_POINT('Ctrl Pts',(0.753058194864076,0.19455274892985,-0.915643041587181)) ;
#47417 = CARTESIAN_POINT('Ctrl Pts',(0.625088625188735,0.2056624210965,-1.00735011816981)) ;
#47418 = CARTESIAN_POINT('Ctrl Pts',(0.34621023025533,0.227244729882854,-1.13306423618887)) ;
#47419 = CARTESIAN_POINT('Ctrl Pts',(0.198861988640031,0.237530859218139,
-1.16797780757678)) ;
#47420 = CARTESIAN_POINT('Ctrl Pts',(-0.107685913283433,0.256807842291688,
-1.18074344368933)) ;
#47421 = CARTESIAN_POINT('Ctrl Pts',(-0.264049422991349,0.266900965989962,
-1.15588270733456)) ;
#47422 = CARTESIAN_POINT('Ctrl Pts',(-0.555198262685363,0.288632714640628,
-1.04720655642656)) ;
#47423 = CARTESIAN_POINT('Ctrl Pts',(-0.687447928061904,0.299648562538409,
-0.965559208935909)) ;
#47424 = CARTESIAN_POINT('Ctrl Pts',(-0.909300810834917,0.320584284569134,
-0.759311484724843)) ;
#47425 = CARTESIAN_POINT('Ctrl Pts',(-0.998091138100098,0.329753514657127,
-0.638106010346577)) ;
#47426 = CARTESIAN_POINT('Ctrl Pts',(-1.12872455349813,0.349287072452111,
-0.362626477782252)) ;
#47427 = CARTESIAN_POINT('Ctrl Pts',(-1.16681971741147,0.36012164176838,-0.209827785290715)) ;
#47428 = CARTESIAN_POINT('Ctrl Pts',(-1.18099786356303,0.38194199317296,0.0979021361303076)) ;
#47429 = CARTESIAN_POINT('Ctrl Pts',(-1.15841877755348,0.392715366544137,
0.249837789203979)) ;
#47430 = CARTESIAN_POINT('Ctrl Pts',(-1.05708362777342,0.412950937587882,
0.535217734363541)) ;
#47431 = CARTESIAN_POINT('Ctrl Pts',(-0.979874387076045,0.421778365177155,
0.666131149349083)) ;
#47432 = CARTESIAN_POINT('Ctrl Pts',(-0.776423383293504,0.442421042552534,
0.895986312377557)) ;
#47433 = CARTESIAN_POINT('Ctrl Pts',(-0.650513068327186,0.453528027849362,
0.99118433750606)) ;
#47434 = CARTESIAN_POINT('Ctrl Pts',(-0.374190124089755,0.475211675331599,
1.12418296205339)) ;
#47435 = CARTESIAN_POINT('Ctrl Pts',(-0.227386317306555,0.485595945618796,
1.16280766348317)) ;
#47436 = CARTESIAN_POINT('Ctrl Pts',(-0.0515081845879271,0.496807018632516,
1.17439476386601)) ;
#47437 = CARTESIAN_POINT('Ctrl Pts',(-0.0257415650013721,0.498419270373064,
1.17524047358082)) ;
#47438 = CARTESIAN_POINT('Ctrl Pts',(-3.77981038384781E-13,0.499999999999977,
1.17524047358083)) ;
#47439 = CARTESIAN_POINT('Origin',(3.46944695195362E-16,1.71875,2.77555756156289E-16)) ;
#47440 = CARTESIAN_POINT('',(-2.19540941881722E-13,0.999999999999973,1.17524047358083)) ;
#47441 = CARTESIAN_POINT('',(-2.68861589338229E-13,0.93749999999997,1.17524047358083)) ;
#47442 = CARTESIAN_POINT('',(5.49963941970804E-16,1.71875,1.17524047358083)) ;
#47443 = CARTESIAN_POINT('',(0.94347795579564,1.17524047358083,-0.700742119235159)) ;
#47444 = CARTESIAN_POINT('Ctrl Pts',(-4.39370761995406E-13,0.999999999999973,
1.17524047358083)) ;
#47445 = CARTESIAN_POINT('Ctrl Pts',(0.106843190322386,1.00656099178002,1.17524047358087)) ;
#47446 = CARTESIAN_POINT('Ctrl Pts',(0.213368336153847,1.01361875616957,1.16067774971801)) ;
#47447 = CARTESIAN_POINT('Ctrl Pts',(0.466148916094986,1.03164907154231,1.08994760428343)) ;
#47448 = CARTESIAN_POINT('Ctrl Pts',(0.605855680297113,1.04274604071748,1.01892824263296)) ;
#47449 = CARTESIAN_POINT('Ctrl Pts',(0.845124236320189,1.06412841046368,0.830247305995036)) ;
#47450 = CARTESIAN_POINT('Ctrl Pts',(0.943713350646115,1.07421852266424,0.716165369678224)) ;
#47451 = CARTESIAN_POINT('Ctrl Pts',(1.09610658325736,1.09297021377989,0.451712413511906)) ;
#47452 = CARTESIAN_POINT('Ctrl Pts',(1.14627242176894,1.1035481597673,0.302532850490821)) ;
#47453 = CARTESIAN_POINT('Ctrl Pts',(1.185194327271,1.1252945917279,-0.0041545934619247)) ;
#47454 = CARTESIAN_POINT('Ctrl Pts',(1.17454441508537,1.13624596978566,-0.15860062628145)) ;
#47455 = CARTESIAN_POINT('Ctrl Pts',(1.09609503850357,1.15682667556352,-0.448847967141481)) ;
#47456 = CARTESIAN_POINT('Ctrl Pts',(1.03129237683895,1.16565618612113,-0.582508937325451)) ;
#47457 = CARTESIAN_POINT('Ctrl Pts',(0.943477955795638,1.17524047358083,-0.700742119235157)) ;
#47458 = CARTESIAN_POINT('',(0.190653686692406,1.17524047358083,-1.15967294634871)) ;
#47459 = CARTESIAN_POINT('Origin',(2.81025203108243E-15,1.17524047358083,
-1.11022302462516E-15)) ;
#47460 = CARTESIAN_POINT('Ctrl Pts',(0.190653686690487,1.17524047358096,-1.15967294634902)) ;
#47461 = CARTESIAN_POINT('Ctrl Pts',(0.334721572181544,1.16555387138265,-1.13598775684016)) ;
#47462 = CARTESIAN_POINT('Ctrl Pts',(0.473089930863508,1.15527304834815,-1.08567024027228)) ;
#47463 = CARTESIAN_POINT('Ctrl Pts',(0.724034634321941,1.13459622175091,-0.937113372977569)) ;
#47464 = CARTESIAN_POINT('Ctrl Pts',(0.834519828985816,1.12437695843099,-0.840237138889637)) ;
#47465 = CARTESIAN_POINT('Ctrl Pts',(1.01675905936992,1.10495423704233,-0.608051906254154)) ;
#47466 = CARTESIAN_POINT('Ctrl Pts',(1.08575086392768,1.09611011380817,-0.473999592828079)) ;
#47467 = CARTESIAN_POINT('Ctrl Pts',(1.17083816769886,1.07552627544959,-0.183708073540434)) ;
#47468 = CARTESIAN_POINT('Ctrl Pts',(1.18478330659978,1.06461718036353,-0.0298583526371077)) ;
#47469 = CARTESIAN_POINT('Ctrl Pts',(1.15263710342259,1.04283633695152,0.277314392081248)) ;
#47470 = CARTESIAN_POINT('Ctrl Pts',(1.10574557383279,1.03218111653273,0.427583747574201)) ;
#47471 = CARTESIAN_POINT('Ctrl Pts',(0.959283994206446,1.01321090337417,0.695118495130982)) ;
#47472 = CARTESIAN_POINT('Ctrl Pts',(0.863430595265501,1.00343003623297,0.811138605254806)) ;
#47473 = CARTESIAN_POINT('Ctrl Pts',(0.628978803774639,0.982168112369197,
1.00476515376881)) ;
#47474 = CARTESIAN_POINT('Ctrl Pts',(0.491263975439452,0.971086219817788,
1.0788094017436)) ;
#47475 = CARTESIAN_POINT('Ctrl Pts',(0.231716823142686,0.952338744278339,
1.15804755576006)) ;
#47476 = CARTESIAN_POINT('Ctrl Pts',(0.116090981062413,0.94462887709724,1.17524047358088)) ;
#47477 = CARTESIAN_POINT('Ctrl Pts',(-5.38250000126084E-13,0.93749999999997,
1.17524047358083)) ;
#47478 = CARTESIAN_POINT('Origin',(0.,1.5,0.)) ;
#47479 = CARTESIAN_POINT('',(2.44539079942923E-14,-1.24999999999999,1.5)) ;
#47480 = CARTESIAN_POINT('',(5.94426045891414E-14,-1.3125,1.5)) ;
#47481 = CARTESIAN_POINT('',(-1.83697019872103E-16,1.5,1.5)) ;
#47482 = CARTESIAN_POINT('',(-1.05094390383305,-1.5,-1.07028823734364)) ;
#47483 = CARTESIAN_POINT('Ctrl Pts',(1.19002030452009E-13,-1.3125,1.5)) ;
#47484 = CARTESIAN_POINT('Ctrl Pts',(-0.125690544708079,-1.31854728915183,
1.5)) ;
#47485 = CARTESIAN_POINT('Ctrl Pts',(-0.251130003993841,-1.32502121415508,
1.4842062166389)) ;
#47486 = CARTESIAN_POINT('Ctrl Pts',(-0.565489283533066,-1.34239014330235,
1.40341101133005)) ;
#47487 = CARTESIAN_POINT('Ctrl Pts',(-0.745894934843807,-1.35348619283281,
1.31642498227603)) ;
#47488 = CARTESIAN_POINT('Ctrl Pts',(-1.05645955766431,-1.3749450764572,1.08181887755639)) ;
#47489 = CARTESIAN_POINT('Ctrl Pts',(-1.18544422357363,-1.38512598373554,
0.938714210288529)) ;
#47490 = CARTESIAN_POINT('Ctrl Pts',(-1.38685389066128,-1.40408354370044,
0.605093828083167)) ;
#47491 = CARTESIAN_POINT('Ctrl Pts',(-1.45477162975192,-1.41437991998462,
0.416161440276449)) ;
#47492 = CARTESIAN_POINT('Ctrl Pts',(-1.51252462564358,-1.43607724588768,
0.0256095740214394)) ;
#47493 = CARTESIAN_POINT('Ctrl Pts',(-1.50293685043723,-1.44705355116319,
-0.171963920937831)) ;
#47494 = CARTESIAN_POINT('Ctrl Pts',(-1.42232581449327,-1.46505639030648,
-0.496015025517027)) ;
#47495 = CARTESIAN_POINT('Ctrl Pts',(-1.37068981709763,-1.47220607842093,
-0.62470941157705)) ;
#47496 = CARTESIAN_POINT('Ctrl Pts',(-1.23381696495112,-1.48550538860935,
-0.864096994968711)) ;
#47497 = CARTESIAN_POINT('Ctrl Pts',(-1.1492933800039,-1.49258560548561,-0.973716324451006)) ;
#47498 = CARTESIAN_POINT('Ctrl Pts',(-1.05094390383214,-1.50000000000007,
-1.07028823734453)) ;
#47499 = CARTESIAN_POINT('',(0.,-1.5,-1.5)) ;
#47500 = CARTESIAN_POINT('Origin',(0.,-1.5,0.)) ;
#47501 = CARTESIAN_POINT('Ctrl Pts',(2.18575157973078E-15,-1.5,-1.5)) ;
#47502 = CARTESIAN_POINT('Ctrl Pts',(-0.138596334074203,-1.49333178076779,
-1.5)) ;
#47503 = CARTESIAN_POINT('Ctrl Pts',(-0.276578903789693,-1.48615954753798,
-1.48079242503239)) ;
#47504 = CARTESIAN_POINT('Ctrl Pts',(-0.548119381515871,-1.47095166696557,
-1.40363062815888)) ;
#47505 = CARTESIAN_POINT('Ctrl Pts',(-0.67987312768868,-1.46297740045344,
-1.34476121618135)) ;
#47506 = CARTESIAN_POINT('Ctrl Pts',(-0.9693345679576,-1.44397019985451,-1.16186391599752)) ;
#47507 = CARTESIAN_POINT('Ctrl Pts',(-1.11466773993113,-1.43312791769337,
-1.0232661960797)) ;
#47508 = CARTESIAN_POINT('Ctrl Pts',(-1.33768338804696,-1.41355051431735,
-0.704754107962303)) ;
#47509 = CARTESIAN_POINT('Ctrl Pts',(-1.41608739796283,-1.40443849522844,
-0.52989291411165)) ;
#47510 = CARTESIAN_POINT('Ctrl Pts',(-1.5049026353994,-1.38356148693885,-0.154106764899098)) ;
#47511 = CARTESIAN_POINT('Ctrl Pts',(-1.51213717096723,-1.37256640287649,
0.0438047482233367)) ;
#47512 = CARTESIAN_POINT('Ctrl Pts',(-1.44932925607157,-1.3508053928519,0.435502928665868)) ;
#47513 = CARTESIAN_POINT('Ctrl Pts',(-1.37819971812457,-1.34061157337981,
0.625095293096029)) ;
#47514 = CARTESIAN_POINT('Ctrl Pts',(-1.17058637322926,-1.32139662500094,
0.957236573047296)) ;
#47515 = CARTESIAN_POINT('Ctrl Pts',(-1.03915094756602,-1.31114876375226,
1.09850674283675)) ;
#47516 = CARTESIAN_POINT('Ctrl Pts',(-0.724349226230084,-1.28961552393313,
1.32845080066116)) ;
#47517 = CARTESIAN_POINT('Ctrl Pts',(-0.542233928925934,-1.27851587207399,
1.41260531982395)) ;
#47518 = CARTESIAN_POINT('Ctrl Pts',(-0.234427210984566,-1.26166095877703,
1.48624532412904)) ;
#47519 = CARTESIAN_POINT('Ctrl Pts',(-0.117295539887556,-1.25564338429406,
1.5)) ;
#47520 = CARTESIAN_POINT('Ctrl Pts',(4.81906181626357E-14,-1.24999999999999,
1.5)) ;
#47521 = CARTESIAN_POINT('Origin',(0.,1.5,0.)) ;
#47522 = CARTESIAN_POINT('',(1.25863447800723E-13,-0.749999999999985,1.5)) ;
#47523 = CARTESIAN_POINT('',(1.1883828150139E-13,-0.81249999999999,1.5)) ;
#47524 = CARTESIAN_POINT('',(-1.83697019872103E-16,1.5,1.5)) ;
#47525 = CARTESIAN_POINT('Ctrl Pts',(2.37860260022652E-13,-0.81249999999999,
1.5)) ;
#47526 = CARTESIAN_POINT('Ctrl Pts',(-0.156447465110858,-0.820027082174664,
1.5)) ;
#47527 = CARTESIAN_POINT('Ctrl Pts',(-0.312164809475088,-0.828198750725344,
1.47553028423322)) ;
#47528 = CARTESIAN_POINT('Ctrl Pts',(-0.649100769465223,-0.847436020155903,
1.36657878633297)) ;
#47529 = CARTESIAN_POINT('Ctrl Pts',(-0.822902367070701,-0.858493925193746,
1.26952740245995)) ;
#47530 = CARTESIAN_POINT('Ctrl Pts',(-1.11762648369567,-0.879650906765802,
1.01835321007618)) ;
#47531 = CARTESIAN_POINT('Ctrl Pts',(-1.23751114978123,-0.889238109349478,
0.868714031709184)) ;
#47532 = CARTESIAN_POINT('Ctrl Pts',(-1.41915748444322,-0.90833829037694,
0.524910773214875)) ;
#47533 = CARTESIAN_POINT('Ctrl Pts',(-1.47615258074904,-0.919033448908922,
0.332397919639227)) ;
#47534 = CARTESIAN_POINT('Ctrl Pts',(-1.51142533493793,-0.940813655782774,
-0.0596458040901028)) ;
#47535 = CARTESIAN_POINT('Ctrl Pts',(-1.49090868354231,-0.951681828986031,
-0.255272921748749)) ;
#47536 = CARTESIAN_POINT('Ctrl Pts',(-1.37736667279861,-0.972163237090842,
-0.623938267635399)) ;
#47537 = CARTESIAN_POINT('Ctrl Pts',(-1.28689333739595,-0.980971534163011,
-0.793939874160591)) ;
#47538 = CARTESIAN_POINT('Ctrl Pts',(-1.04114745712756,-1.00124754387222,
-1.0982318733166)) ;
#47539 = CARTESIAN_POINT('Ctrl Pts',(-0.885409852125076,-1.01232423013715,
-1.22724713434068)) ;
#47540 = CARTESIAN_POINT('Ctrl Pts',(-0.539253545854058,-1.03413578891522,
-1.41290294052909)) ;
#47541 = CARTESIAN_POINT('Ctrl Pts',(-0.353564236997969,-1.04466712776859,
-1.47040782188932)) ;
#47542 = CARTESIAN_POINT('Ctrl Pts',(0.0323067062935163,-1.06439721558525,
-1.51234290434375)) ;
#47543 = CARTESIAN_POINT('Ctrl Pts',(0.228921251204819,-1.07364538754622,
-1.49526928635465)) ;
#47544 = CARTESIAN_POINT('Ctrl Pts',(0.606732761779437,-1.09485823271693,
-1.38599559220871)) ;
#47545 = CARTESIAN_POINT('Ctrl Pts',(0.78397190838898,-1.10594048180573,-1.29402183202991)) ;
#47546 = CARTESIAN_POINT('Ctrl Pts',(1.08686896974953,-1.12725901834733,-1.051187616272)) ;
#47547 = CARTESIAN_POINT('Ctrl Pts',(1.21137930856031,-1.13722951519011,-0.904868726577733)) ;
#47548 = CARTESIAN_POINT('Ctrl Pts',(1.4031642124512,-1.15604084125592,-0.566264857393262)) ;
#47549 = CARTESIAN_POINT('Ctrl Pts',(1.46576524891775,-1.16663659132274,-0.37554135619049)) ;
#47550 = CARTESIAN_POINT('Ctrl Pts',(1.51259069068335,-1.18837829937752,0.0158093887954927)) ;
#47551 = CARTESIAN_POINT('Ctrl Pts',(1.49767343362296,-1.1993062118098,0.212511812576511)) ;
#47552 = CARTESIAN_POINT('Ctrl Pts',(1.39459172544617,-1.21995828168816,0.584249070387106)) ;
#47553 = CARTESIAN_POINT('Ctrl Pts',(1.30929591411423,-1.22884778908545,0.756287452464687)) ;
#47554 = CARTESIAN_POINT('Ctrl Pts',(1.07255114321248,-1.24888841128061,1.06769587986244)) ;
#47555 = CARTESIAN_POINT('Ctrl Pts',(0.920126566016231,-1.25993973528819,
1.20153643210929)) ;
#47556 = CARTESIAN_POINT('Ctrl Pts',(0.578370341808044,-1.28182365534903,
1.39741841016814)) ;
#47557 = CARTESIAN_POINT('Ctrl Pts',(0.393835703366298,-1.2924461640788,1.46020535490243)) ;
#47558 = CARTESIAN_POINT('Ctrl Pts',(0.13521340142217,-1.30586770692904,1.49543393057343)) ;
#47559 = CARTESIAN_POINT('Ctrl Pts',(0.0675765704749157,-1.30924872073712,
1.5)) ;
#47560 = CARTESIAN_POINT('Ctrl Pts',(1.19068906198155E-13,-1.3125,1.5)) ;
#47561 = CARTESIAN_POINT('Ctrl Pts',(4.90915130084568E-14,-1.24999999999999,
1.5)) ;
#47562 = CARTESIAN_POINT('Ctrl Pts',(0.07522788002324,-1.24638059693483,1.5)) ;
#47563 = CARTESIAN_POINT('Ctrl Pts',(0.150507881150062,-1.24260150705645,
1.49434155112345)) ;
#47564 = CARTESIAN_POINT('Ctrl Pts',(0.416459553793433,-1.22868401181681,
1.45395353187258)) ;
#47565 = CARTESIAN_POINT('Ctrl Pts',(0.600276122090132,-1.21801338726496,
1.38819068356874)) ;
#47566 = CARTESIAN_POINT('Ctrl Pts',(0.937459127338934,-1.1962224867055,1.18773635996788)) ;
#47567 = CARTESIAN_POINT('Ctrl Pts',(1.08651459968785,-1.18531157658795,1.05311524699077)) ;
#47568 = CARTESIAN_POINT('Ctrl Pts',(1.31823172790811,-1.16548099578163,0.740560177024522)) ;
#47569 = CARTESIAN_POINT('Ctrl Pts',(1.40140246253754,-1.15653696644918,0.567665396084969)) ;
#47570 = CARTESIAN_POINT('Ctrl Pts',(1.50012619162202,-1.13581521641982,0.194673895556624)) ;
#47571 = CARTESIAN_POINT('Ctrl Pts',(1.51270127932233,-1.12486502884897,-0.0024294807186321)) ;
#47572 = CARTESIAN_POINT('Ctrl Pts',(1.46105722910734,-1.10313814923197,-0.393513313824723)) ;
#47573 = CARTESIAN_POINT('Ctrl Pts',(1.3960922028536,-1.09262939091854,-0.583444554325999)) ;
#47574 = CARTESIAN_POINT('Ctrl Pts',(1.20008336997013,-1.07385392283904,-0.919864147901511)) ;
#47575 = CARTESIAN_POINT('Ctrl Pts',(1.07358713734848,-1.06374269118958,-1.0647705854153)) ;
#47576 = CARTESIAN_POINT('Ctrl Pts',(0.767348684105939,-1.0423638998445,-1.30398651359086)) ;
#47577 = CARTESIAN_POINT('Ctrl Pts',(0.588703928541707,-1.03127443753244,
-1.39378536368201)) ;
#47578 = CARTESIAN_POINT('Ctrl Pts',(0.209873430922041,-1.01015376126538,
-1.49797603996222)) ;
#47579 = CARTESIAN_POINT('Ctrl Pts',(0.0137333074789716,-1.00100912536654,
-1.51254172688592)) ;
#47580 = CARTESIAN_POINT('Ctrl Pts',(-0.371192239473193,-0.981198968126641,
-1.46608667070176)) ;
#47581 = CARTESIAN_POINT('Ctrl Pts',(-0.556395397747934,-0.970626859815039,
-1.40627205133812)) ;
#47582 = CARTESIAN_POINT('Ctrl Pts',(-0.900665850508364,-0.948781621036587,
-1.21613737103961)) ;
#47583 = CARTESIAN_POINT('Ctrl Pts',(-1.05497403477983,-0.937714890204883,
-1.08500467628011)) ;
#47584 = CARTESIAN_POINT('Ctrl Pts',(-1.29679747167913,-0.917540931357973,
-0.777592636961856)) ;
#47585 = CARTESIAN_POINT('Ctrl Pts',(-1.38500644009541,-0.908706039897536,
-0.606708718155526)) ;
#47586 = CARTESIAN_POINT('Ctrl Pts',(-1.49400139301044,-0.888149858014107,
-0.236697444253813)) ;
#47587 = CARTESIAN_POINT('Ctrl Pts',(-1.5120883063272,-0.877254631314325,
-0.0405833636577428)) ;
#47588 = CARTESIAN_POINT('Ctrl Pts',(-1.47179007933231,-0.855488831503584,
0.351201032935604)) ;
#47589 = CARTESIAN_POINT('Ctrl Pts',(-1.41234983298357,-0.844835759900771,
0.54295632178624)) ;
#47590 = CARTESIAN_POINT('Ctrl Pts',(-1.22628881776183,-0.825860517668724,
0.884510681963101)) ;
#47591 = CARTESIAN_POINT('Ctrl Pts',(-1.10440403198004,-0.816116121019566,
1.0327035387692)) ;
#47592 = CARTESIAN_POINT('Ctrl Pts',(-0.806135051990802,-0.794888528982598,
1.28027982443691)) ;
#47593 = CARTESIAN_POINT('Ctrl Pts',(-0.630827416060365,-0.783818836307302,
1.37514702836123)) ;
#47594 = CARTESIAN_POINT('Ctrl Pts',(-0.298684002099519,-0.764992300162682,
1.47761306118797)) ;
#47595 = CARTESIAN_POINT('Ctrl Pts',(-0.149642595802423,-0.757199682747379,
1.5)) ;
#47596 = CARTESIAN_POINT('Ctrl Pts',(2.5358187771829E-13,-0.749999999999985,
1.5)) ;
#47597 = CARTESIAN_POINT('Origin',(0.,1.5,0.)) ;
#47598 = CARTESIAN_POINT('',(2.44539079942923E-14,-0.249999999999995,1.5)) ;
#47599 = CARTESIAN_POINT('',(6.9856727510751E-15,-0.3125,1.5)) ;
#47600 = CARTESIAN_POINT('',(-1.83697019872103E-16,1.5,1.5)) ;
#47601 = CARTESIAN_POINT('Ctrl Pts',(1.46410661372443E-14,-0.3125,1.5)) ;
#47602 = CARTESIAN_POINT('Ctrl Pts',(-0.187010746043016,-0.32149755871411,
1.5)) ;
#47603 = CARTESIAN_POINT('Ctrl Pts',(-0.372522155022534,-0.331394385307366,
1.46502942837889)) ;
#47604 = CARTESIAN_POINT('Ctrl Pts',(-0.729433956821984,-0.352448532324359,
1.32526951030474)) ;
#47605 = CARTESIAN_POINT('Ctrl Pts',(-0.896175160711237,-0.363430481795517,
1.21872356619442)) ;
#47606 = CARTESIAN_POINT('Ctrl Pts',(-1.17491701108803,-0.384259579430114,
0.951671098397219)) ;
#47607 = CARTESIAN_POINT('Ctrl Pts',(-1.28587778498005,-0.393312773348132,
0.795370079733538)) ;
#47608 = CARTESIAN_POINT('Ctrl Pts',(-1.44726955852417,-0.412969136442091,
0.441555544042314)) ;
#47609 = CARTESIAN_POINT('Ctrl Pts',(-1.49299246551635,-0.423833555841407,
0.245995994854643)) ;
#47610 = CARTESIAN_POINT('Ctrl Pts',(-1.50535850109774,-0.44563386772807,
-0.146409619105293)) ;
#47611 = CARTESIAN_POINT('Ctrl Pts',(-1.47388303399498,-0.456357986138421,
-0.339443750491626)) ;
#47612 = CARTESIAN_POINT('Ctrl Pts',(-1.33962971691653,-0.476487789999139,
-0.701780219984592)) ;
#47613 = CARTESIAN_POINT('Ctrl Pts',(-1.23855816416065,-0.485348762111955,
-0.867801104486143)) ;
#47614 = CARTESIAN_POINT('Ctrl Pts',(-0.974770975084767,-0.506083106736852,
-1.15734469711718)) ;
#47615 = CARTESIAN_POINT('Ctrl Pts',(-0.812759703657768,-0.517183229195444,
-1.27633735211607)) ;
#47616 = CARTESIAN_POINT('Ctrl Pts',(-0.45858526139189,-0.538796477123096,
-1.44096614876463)) ;
#47617 = CARTESIAN_POINT('Ctrl Pts',(-0.271009539442144,-0.549119454060885,
-1.48770263784166)) ;
#47618 = CARTESIAN_POINT('Ctrl Pts',(0.119102093778023,-0.56846525435471,
-1.50845827905837)) ;
#47619 = CARTESIAN_POINT('Ctrl Pts',(0.318052049351352,-0.578375637986886,
-1.4793593413999)) ;
#47620 = CARTESIAN_POINT('Ctrl Pts',(0.690607371195689,-0.600004849340496,
-1.34599247873446)) ;
#47621 = CARTESIAN_POINT('Ctrl Pts',(0.860852321760142,-0.611028519610325,
-1.24401325313029)) ;
#47622 = CARTESIAN_POINT('Ctrl Pts',(1.14740420182817,-0.632019727786263,
-0.984652174078658)) ;
#47623 = CARTESIAN_POINT('Ctrl Pts',(1.26270901412663,-0.64129791484719,-0.831637532750416)) ;
#47624 = CARTESIAN_POINT('Ctrl Pts',(1.43407232346488,-0.660684006756509,
-0.4826878783827)) ;
#47625 = CARTESIAN_POINT('Ctrl Pts',(1.48535296306111,-0.671469994454859,
-0.288540099812428)) ;
#47626 = CARTESIAN_POINT('Ctrl Pts',(1.50896036510848,-0.693269776161453,
0.103855970906278)) ;
#47627 = CARTESIAN_POINT('Ctrl Pts',(1.48283917680271,-0.704068836163023,
0.29823905093455)) ;
#47628 = CARTESIAN_POINT('Ctrl Pts',(1.35875189168508,-0.724373392606975,
0.663721066925711)) ;
#47629 = CARTESIAN_POINT('Ctrl Pts',(1.26294128670969,-0.733172592590258,
0.831691808807288)) ;
#47630 = CARTESIAN_POINT('Ctrl Pts',(1.0080442938249,-0.753683385620307,1.12858581551606)) ;
#47631 = CARTESIAN_POINT('Ctrl Pts',(0.84906092268456,-0.764776600734295,
1.25257428324593)) ;
#47632 = CARTESIAN_POINT('Ctrl Pts',(0.498700007418968,-0.786496539143091,
1.42764915973622)) ;
#47633 = CARTESIAN_POINT('Ctrl Pts',(0.311980955151472,-0.796926476589065,
1.47972002252289)) ;
#47634 = CARTESIAN_POINT('Ctrl Pts',(0.0803526425168444,-0.808589245183692,
1.49838768597481)) ;
#47635 = CARTESIAN_POINT('Ctrl Pts',(0.0401544197174351,-0.81056806958058,
1.5)) ;
#47636 = CARTESIAN_POINT('Ctrl Pts',(2.37860260022652E-13,-0.81249999999999,
1.5)) ;
#47637 = CARTESIAN_POINT('Ctrl Pts',(2.51910592621317E-13,-0.749999999999984,
1.5)) ;
#47638 = CARTESIAN_POINT('Ctrl Pts',(0.0461416120551636,-0.747780010654926,
1.5)) ;
#47639 = CARTESIAN_POINT('Ctrl Pts',(0.0923346900483627,-0.745498408059054,
1.49787106459072)) ;
#47640 = CARTESIAN_POINT('Ctrl Pts',(0.329943863327776,-0.733454686588535,
1.47584825211639)) ;
#47641 = CARTESIAN_POINT('Ctrl Pts',(0.516238107926601,-0.722980052420667,
1.42143251887597)) ;
#47642 = CARTESIAN_POINT('Ctrl Pts',(0.864824462259465,-0.701218455313852,
1.2417842995603)) ;
#47643 = CARTESIAN_POINT('Ctrl Pts',(1.02242731062005,-0.690131191238374,
1.11561893362118)) ;
#47644 = CARTESIAN_POINT('Ctrl Pts',(1.27338820842905,-0.669720803380355,
0.81552199645074)) ;
#47645 = CARTESIAN_POINT('Ctrl Pts',(1.36689330998072,-0.660926783329383,
0.646682099928811)) ;
#47646 = CARTESIAN_POINT('Ctrl Pts',(1.48645525637395,-0.64054574751106,0.279823455199)) ;
#47647 = CARTESIAN_POINT('Ctrl Pts',(1.51017696617209,-0.629715942961133,
0.0848869733003025)) ;
#47648 = CARTESIAN_POINT('Ctrl Pts',(1.48156266081736,-0.607922189659522,
-0.307400586128696)) ;
#47649 = CARTESIAN_POINT('Ctrl Pts',(1.42782270120019,-0.597174010873431,
-0.500867804278345)) ;
#47650 = CARTESIAN_POINT('Ctrl Pts',(1.25203889624671,-0.577909943419593,
-0.847621018447427)) ;
#47651 = CARTESIAN_POINT('Ctrl Pts',(1.13477837984287,-0.568508627404166,
-0.999183222668732)) ;
#47652 = CARTESIAN_POINT('Ctrl Pts',(0.844728033590153,-0.547445955347855,
-1.25505748023326)) ;
#47653 = CARTESIAN_POINT('Ctrl Pts',(0.672946332215184,-0.536406433221943,
-1.35494564217399)) ;
#47654 = CARTESIAN_POINT('Ctrl Pts',(0.299208731678686,-0.514863106619634,
-1.483172887029)) ;
#47655 = CARTESIAN_POINT('Ctrl Pts',(0.100766701449236,-0.505117175315716,
-1.50968526474447)) ;
#47656 = CARTESIAN_POINT('Ctrl Pts',(-0.288472818487683,-0.485688724200375,
-1.48444364943667)) ;
#47657 = CARTESIAN_POINT('Ctrl Pts',(-0.475702357207199,-0.475319311309763,
-1.43543585911451)) ;
#47658 = CARTESIAN_POINT('Ctrl Pts',(-0.828290876262396,-0.453658618108879,
-1.26635213305172)) ;
#47659 = CARTESIAN_POINT('Ctrl Pts',(-0.989031976371569,-0.44256031447766,
-1.1452249545814)) ;
#47660 = CARTESIAN_POINT('Ctrl Pts',(-1.24904449455747,-0.421920316029762,
-0.85253990255895)) ;
#47661 = CARTESIAN_POINT('Ctrl Pts',(-1.34787241514442,-0.413094081662667,
-0.685693469927933)) ;
#47662 = CARTESIAN_POINT('Ctrl Pts',(-1.4778181443911,-0.392889717508791,
-0.322014915158169)) ;
#47663 = CARTESIAN_POINT('Ctrl Pts',(-1.50703130418987,-0.382132857700582,
-0.1283914386104)) ;
#47664 = CARTESIAN_POINT('Ctrl Pts',(-1.48990386914471,-0.360330572743572,
0.264049690615775)) ;
#47665 = CARTESIAN_POINT('Ctrl Pts',(-1.44182082693689,-0.349498281946545,
0.459030924962268)) ;
#47666 = CARTESIAN_POINT('Ctrl Pts',(-1.27619684671042,-0.32995577793014,
0.810795997257542)) ;
#47667 = CARTESIAN_POINT('Ctrl Pts',(-1.16340334266401,-0.320815927649413,
0.965700303810776)) ;
#47668 = CARTESIAN_POINT('Ctrl Pts',(-0.881360542847993,-0.299917888861523,
1.22951724098448)) ;
#47669 = CARTESIAN_POINT('Ctrl Pts',(-0.713126432759514,-0.288917248829942,
1.33415025588196)) ;
#47670 = CARTESIAN_POINT('Ctrl Pts',(-0.360105689805461,-0.26823254479493,
1.46734973822026)) ;
#47671 = CARTESIAN_POINT('Ctrl Pts',(-0.180705529985591,-0.258694198865097,
1.5)) ;
#47672 = CARTESIAN_POINT('Ctrl Pts',(4.90926743701436E-14,-0.249999999999995,
1.5)) ;
#47673 = CARTESIAN_POINT('Origin',(0.,1.5,0.)) ;
#47674 = CARTESIAN_POINT('',(-3.49720252756921E-15,0.250000000000002,1.5)) ;
#47675 = CARTESIAN_POINT('',(-4.54712573957423E-14,0.187499999999993,1.5)) ;
#47676 = CARTESIAN_POINT('',(-1.83697019872103E-16,1.5,1.5)) ;
#47677 = CARTESIAN_POINT('Ctrl Pts',(-9.07588177716125E-14,0.187499999999994,
1.5)) ;
#47678 = CARTESIAN_POINT('Ctrl Pts',(-0.0237189864434504,0.186358819732662,
1.5)) ;
#47679 = CARTESIAN_POINT('Ctrl Pts',(-0.0474577649910852,0.185201059899418,
1.49943741655724)) ;
#47680 = CARTESIAN_POINT('Ctrl Pts',(-0.262459822908907,0.17457297797897,
1.48922095546663)) ;
#47681 = CARTESIAN_POINT('Ctrl Pts',(-0.450194841475407,0.164273189929587,
1.44359517620589)) ;
#47682 = CARTESIAN_POINT('Ctrl Pts',(-0.805124481113827,0.142684229431146,
1.28114876722784)) ;
#47683 = CARTESIAN_POINT('Ctrl Pts',(-0.967746636206636,0.131583821193572,
1.16320390573225)) ;
#47684 = CARTESIAN_POINT('Ctrl Pts',(-1.23337408545708,0.110803802267297,
0.875203462372997)) ;
#47685 = CARTESIAN_POINT('Ctrl Pts',(-1.33554531695723,0.101921319526277,
0.709583751472954)) ;
#47686 = CARTESIAN_POINT('Ctrl Pts',(-1.47189435169531,0.0818280748851064,
0.347905347931908)) ;
#47687 = CARTESIAN_POINT('Ctrl Pts',(-1.50446685481494,0.0711204066738244,
0.155167320128844)) ;
#47688 = CARTESIAN_POINT('Ctrl Pts',(-1.49441590282142,0.0493222220689783,
-0.23720000275839)) ;
#47689 = CARTESIAN_POINT('Ctrl Pts',(-1.44984377558211,0.0384427620859756,
-0.43303028245246)) ;
#47690 = CARTESIAN_POINT('Ctrl Pts',(-1.29051485664985,0.018731362500822,
-0.787835474985263)) ;
#47691 = CARTESIAN_POINT('Ctrl Pts',(-1.18044177811369,0.00971574318362152,
-0.944818380459478)) ;
#47692 = CARTESIAN_POINT('Ctrl Pts',(-0.901901541919688,-0.0111847314112764,
-1.21478962483548)) ;
#47693 = CARTESIAN_POINT('Ctrl Pts',(-0.733997449933338,-0.0222694381140607,
-1.32302064801658)) ;
#47694 = CARTESIAN_POINT('Ctrl Pts',(-0.372671975906577,-0.0436089300705782,
-1.46540827936792)) ;
#47695 = CARTESIAN_POINT('Ctrl Pts',(-0.183770006155042,-0.0536354113071329,
-1.50082620537561)) ;
#47696 = CARTESIAN_POINT('Ctrl Pts',(0.205428255104891,-0.0724084659494439,
-1.49910740097208)) ;
#47697 = CARTESIAN_POINT('Ctrl Pts',(0.402051497713194,-0.0829904980857595,
-1.45871569021124)) ;
#47698 = CARTESIAN_POINT('Ctrl Pts',(0.765039896519852,-0.104725751684374,
-1.3049609099523)) ;
#47699 = CARTESIAN_POINT('Ctrl Pts',(0.928411042654205,-0.115660845279063,
-1.19426466613892)) ;
#47700 = CARTESIAN_POINT('Ctrl Pts',(1.19983378457874,-0.136334949627821,
-0.920114888926562)) ;
#47701 = CARTESIAN_POINT('Ctrl Pts',(1.30674418549408,-0.145240331171075,
-0.760674038920638)) ;
#47702 = CARTESIAN_POINT('Ctrl Pts',(1.45944177193774,-0.165249915641916,
-0.400501518445528)) ;
#47703 = CARTESIAN_POINT('Ctrl Pts',(1.49989710280014,-0.176297274481281,
-0.20164905933698)) ;
#47704 = CARTESIAN_POINT('Ctrl Pts',(1.50009856498918,-0.19818935744411,0.192408433993937)) ;
#47705 = CARTESIAN_POINT('Ctrl Pts',(1.46287970752877,-0.208823144729875,
0.383816605137735)) ;
#47706 = CARTESIAN_POINT('Ctrl Pts',(1.31759977513551,-0.22875851391926,0.742653250546679)) ;
#47707 = CARTESIAN_POINT('Ctrl Pts',(1.21068115102719,-0.237766756730124,
0.906564507629634)) ;
#47708 = CARTESIAN_POINT('Ctrl Pts',(0.937185311602803,-0.258739597926462,
1.18787810115603)) ;
#47709 = CARTESIAN_POINT('Ctrl Pts',(0.772014362866387,-0.269836739712522,
1.30129073030834)) ;
#47710 = CARTESIAN_POINT('Ctrl Pts',(0.413990985129278,-0.29131324405455,
1.45433020608324)) ;
#47711 = CARTESIAN_POINT('Ctrl Pts',(0.22564585066882,-0.301509802578729,
1.49518297070977)) ;
#47712 = CARTESIAN_POINT('Ctrl Pts',(0.0231149140393018,-0.311384174501881,
1.49986648759641)) ;
#47713 = CARTESIAN_POINT('Ctrl Pts',(0.0115547705911262,-0.311944070840734,
1.5)) ;
#47714 = CARTESIAN_POINT('Ctrl Pts',(1.41550425220223E-14,-0.3125,1.5)) ;
#47715 = CARTESIAN_POINT('Ctrl Pts',(4.90915130084568E-14,-0.249999999999995,
1.5)) ;
#47716 = CARTESIAN_POINT('Ctrl Pts',(0.0191592501217865,-0.249078200148724,
1.5)) ;
#47717 = CARTESIAN_POINT('Ctrl Pts',(0.0383322093844666,-0.248145544213741,
1.49963292591492)) ;
#47718 = CARTESIAN_POINT('Ctrl Pts',(0.248674185200841,-0.23780128807632,
1.49156269404616)) ;
#47719 = CARTESIAN_POINT('Ctrl Pts',(0.436652034139633,-0.227539515533002,
1.44772606754618)) ;
#47720 = CARTESIAN_POINT('Ctrl Pts',(0.792770125914089,-0.205991173594779,
1.28880038621794)) ;
#47721 = CARTESIAN_POINT('Ctrl Pts',(0.956362180861738,-0.194891136528308,
1.17254880270888)) ;
#47722 = CARTESIAN_POINT('Ctrl Pts',(1.22494646823618,-0.174038182575903,
0.887044092269506)) ;
#47723 = CARTESIAN_POINT('Ctrl Pts',(1.32889290290969,-0.165114861284888,
0.722067503127937)) ;
#47724 = CARTESIAN_POINT('Ctrl Pts',(1.46860354017829,-0.145080646468042,
0.361451636424709)) ;
#47725 = CARTESIAN_POINT('Ctrl Pts',(1.50293052915093,-0.134400071955941,
0.16920129520689)) ;
#47726 = CARTESIAN_POINT('Ctrl Pts',(1.49659053880823,-0.112606893140416,
-0.223075923472551)) ;
#47727 = CARTESIAN_POINT('Ctrl Pts',(1.45386747113103,-0.101704118359621,
-0.419325869526868)) ;
#47728 = CARTESIAN_POINT('Ctrl Pts',(1.29785265196493,-0.0819049369369369,
-0.775711135135183)) ;
#47729 = CARTESIAN_POINT('Ctrl Pts',(1.18919831008328,-0.0729433542002783,
-0.933791142129341)) ;
#47730 = CARTESIAN_POINT('Ctrl Pts',(0.9146207727033,-0.0522020884534194,
-1.20489446365697)) ;
#47731 = CARTESIAN_POINT('Ctrl Pts',(0.749787143876792,-0.0412458924799698,
-1.31381729877768)) ;
#47732 = CARTESIAN_POINT('Ctrl Pts',(0.384694175187683,-0.0195251428224716,
-1.4634047151919)) ;
#47733 = CARTESIAN_POINT('Ctrl Pts',(0.187586889710424,-0.00906504495717777,
-1.50143159464614)) ;
#47734 = CARTESIAN_POINT('Ctrl Pts',(-0.209921866159885,0.0101419464948581,
-1.49848526399372)) ;
#47735 = CARTESIAN_POINT('Ctrl Pts',(-0.406427193981676,0.0207347046007646,
-1.45750318392639)) ;
#47736 = CARTESIAN_POINT('Ctrl Pts',(-0.768903774840431,0.0424750264145686,
-1.30267945323063)) ;
#47737 = CARTESIAN_POINT('Ctrl Pts',(-0.931899884490505,0.0534045251144004,
-1.19153504338665)) ;
#47738 = CARTESIAN_POINT('Ctrl Pts',(-1.20251862707306,0.0740614292800871,
-0.916611905055273)) ;
#47739 = CARTESIAN_POINT('Ctrl Pts',(-1.30898495960905,0.0829543119014871,
-0.756822385773172)) ;
#47740 = CARTESIAN_POINT('Ctrl Pts',(-1.46060335034513,0.10298813736439,-0.396213527440928)) ;
#47741 = CARTESIAN_POINT('Ctrl Pts',(-1.50046665242847,0.114038605116938,
-0.197305107895072)) ;
#47742 = CARTESIAN_POINT('Ctrl Pts',(-1.4995431543654,0.13592433948451,0.196638110721231)) ;
#47743 = CARTESIAN_POINT('Ctrl Pts',(-1.46179849759225,0.146549332465405,
0.387887984377344)) ;
#47744 = CARTESIAN_POINT('Ctrl Pts',(-1.31550192893595,0.16646651706018,0.746397307083299)) ;
#47745 = CARTESIAN_POINT('Ctrl Pts',(-1.20803649523317,0.175492594998149,
0.910114007074791)) ;
#47746 = CARTESIAN_POINT('Ctrl Pts',(-0.933642445954468,0.196487186135895,
1.19065485338835)) ;
#47747 = CARTESIAN_POINT('Ctrl Pts',(-0.768187158340748,0.207583488768161,
1.30354478362202)) ;
#47748 = CARTESIAN_POINT('Ctrl Pts',(-0.409824740621127,0.229046263369276,
1.45550275424853)) ;
#47749 = CARTESIAN_POINT('Ctrl Pts',(-0.221417349171984,0.239230615977489,
1.49580827363276)) ;
#47750 = CARTESIAN_POINT('Ctrl Pts',(-0.0203239888607854,0.249019294320898,
1.49989677687175)) ;
#47751 = CARTESIAN_POINT('Ctrl Pts',(-0.0101598874830822,0.249511182185562,
1.5)) ;
#47752 = CARTESIAN_POINT('Ctrl Pts',(-6.81070803526631E-15,0.250000000000002,
1.5)) ;
#47753 = CARTESIAN_POINT('Origin',(0.,1.5,0.)) ;
#47754 = CARTESIAN_POINT('',(-1.13659082146001E-13,0.749999999999992,1.5)) ;
#47755 = CARTESIAN_POINT('',(-1.2415068972871E-13,0.687499999999986,1.5)) ;
#47756 = CARTESIAN_POINT('',(-1.83697019872103E-16,1.5,1.5)) ;
#47757 = CARTESIAN_POINT('Ctrl Pts',(-2.48117682437547E-13,0.687499999999986,
1.5)) ;
#47758 = CARTESIAN_POINT('Ctrl Pts',(-0.0510614672068272,0.685043304013574,
1.49999999999999)) ;
#47759 = CARTESIAN_POINT('Ctrl Pts',(-0.102179477610568,0.682511468087141,
1.49739289784913)) ;
#47760 = CARTESIAN_POINT('Ctrl Pts',(-0.344669170413668,0.670153302582107,
1.47250340791462)) ;
#47761 = CARTESIAN_POINT('Ctrl Pts',(-0.530592504818994,0.659643040161198,
1.41616262226452)) ;
#47762 = CARTESIAN_POINT('Ctrl Pts',(-0.877676886885451,0.637849649816645,
1.23276835411336)) ;
#47763 = CARTESIAN_POINT('Ctrl Pts',(-1.0341236120761,0.626768610768905,1.10482462510261)) ;
#47764 = CARTESIAN_POINT('Ctrl Pts',(-1.28183875596352,0.606441680690317,
0.802110357290677)) ;
#47765 = CARTESIAN_POINT('Ctrl Pts',(-1.37345398630756,0.597641604441125,
0.632548879940103)) ;
#47766 = CARTESIAN_POINT('Ctrl Pts',(-1.48927255276646,0.577197970079465,
0.264563461430231)) ;
#47767 = CARTESIAN_POINT('Ctrl Pts',(-1.51100291455977,0.566343965788529,
0.0691913841933851)) ;
#47768 = CARTESIAN_POINT('Ctrl Pts',(-1.47824767805252,0.544557894761976,
-0.322957894284567)) ;
#47769 = CARTESIAN_POINT('Ctrl Pts',(-1.42248125925354,0.533842322046463,
-0.515838203163837)) ;
#47770 = CARTESIAN_POINT('Ctrl Pts',(-1.24304955486358,0.51467995777457,-0.860760760057962)) ;
#47771 = CARTESIAN_POINT('Ctrl Pts',(-1.12416038075026,0.505166024597211,
-1.01112600981612)) ;
#47772 = CARTESIAN_POINT('Ctrl Pts',(-0.8312063682489,0.48404460150766,-1.26408600710638)) ;
#47773 = CARTESIAN_POINT('Ctrl Pts',(-0.658165242181626,0.472993280290402,
-1.36221754878023)) ;
#47774 = CARTESIAN_POINT('Ctrl Pts',(-0.283470430065135,0.45152259037716,
-1.48617193373867)) ;
#47775 = CARTESIAN_POINT('Ctrl Pts',(-0.0854472376909037,0.441903950874523,
-1.5105432744356)) ;
#47776 = CARTESIAN_POINT('Ctrl Pts',(0.30305399922152,0.422407069963543,-1.48155944277595)) ;
#47777 = CARTESIAN_POINT('Ctrl Pts',(0.489972944982964,0.411999846327852,
-1.43065250284712)) ;
#47778 = CARTESIAN_POINT('Ctrl Pts',(0.841192364010326,0.390301777529644,
-1.25785190447179)) ;
#47779 = CARTESIAN_POINT('Ctrl Pts',(1.00084972049992,0.379206271374095,-1.13494833611413)) ;
#47780 = CARTESIAN_POINT('Ctrl Pts',(1.25769372320449,0.358646139226393,-0.839650441100459)) ;
#47781 = CARTESIAN_POINT('Ctrl Pts',(1.35465031011417,0.349839319344135,-0.672107748194327)) ;
#47782 = CARTESIAN_POINT('Ctrl Pts',(1.48097046872622,0.329572811631444,-0.30731060936592)) ;
#47783 = CARTESIAN_POINT('Ctrl Pts',(1.50827217193254,0.318789518569689,-0.113211334254335)) ;
#47784 = CARTESIAN_POINT('Ctrl Pts',(1.48713507777104,0.296988077347213,0.279214607750242)) ;
#47785 = CARTESIAN_POINT('Ctrl Pts',(1.43707147471412,0.286184087706954,0.473686421274927)) ;
#47786 = CARTESIAN_POINT('Ctrl Pts',(1.26789353267485,0.266738168283495,0.823712970897226)) ;
#47787 = CARTESIAN_POINT('Ctrl Pts',(1.15354857632314,0.257515504479239,0.977446581937966)) ;
#47788 = CARTESIAN_POINT('Ctrl Pts',(0.868718043953079,0.236559724813284,
1.23851369630045)) ;
#47789 = CARTESIAN_POINT('Ctrl Pts',(0.699236785176761,0.225544503037257,
1.34151152910609)) ;
#47790 = CARTESIAN_POINT('Ctrl Pts',(0.349606601167749,0.205174756639845,
1.46924515684965)) ;
#47791 = CARTESIAN_POINT('Ctrl Pts',(0.175384875096167,0.195938208737378,
1.50000000000001)) ;
#47792 = CARTESIAN_POINT('Ctrl Pts',(-9.10382880192628E-14,0.187499999999994,
1.5)) ;
#47793 = CARTESIAN_POINT('Ctrl Pts',(-6.97358837342676E-15,0.250000000000002,
1.5)) ;
#47794 = CARTESIAN_POINT('Ctrl Pts',(0.188419112446916,0.259065318774311,
1.5)) ;
#47795 = CARTESIAN_POINT('Ctrl Pts',(0.375295540662263,0.269042518704381,
1.46450027092331)) ;
#47796 = CARTESIAN_POINT('Ctrl Pts',(0.733064149695413,0.290179090100831,
1.32325710884974)) ;
#47797 = CARTESIAN_POINT('Ctrl Pts',(0.899468751927728,0.301156645101247,
1.21628635451441)) ;
#47798 = CARTESIAN_POINT('Ctrl Pts',(1.17747154217608,0.321970224054261,0.948512469561911)) ;
#47799 = CARTESIAN_POINT('Ctrl Pts',(1.28802255728247,0.331005715020445,0.791897129631915)) ;
#47800 = CARTESIAN_POINT('Ctrl Pts',(1.44846315974962,0.350687492820267,0.437625129235129)) ;
#47801 = CARTESIAN_POINT('Ctrl Pts',(1.49365547206233,0.361558897757654,0.241939840362161)) ;
#47802 = CARTESIAN_POINT('Ctrl Pts',(1.5049535533416,0.383358323322134,-0.150449819798485)) ;
#47803 = CARTESIAN_POINT('Ctrl Pts',(1.4729717817079,0.394074896368886,-0.343348134640027)) ;
#47804 = CARTESIAN_POINT('Ctrl Pts',(1.33775182562377,0.414187860562473,-0.705381490124597)) ;
#47805 = CARTESIAN_POINT('Ctrl Pts',(1.23617371768228,0.423058378322597,-0.871217305620668)) ;
#47806 = CARTESIAN_POINT('Ctrl Pts',(0.971538021496481,0.443813809003432,
-1.16005033884053)) ;
#47807 = CARTESIAN_POINT('Ctrl Pts',(0.80924439776282,0.454914112344198,-1.27856045705693)) ;
#47808 = CARTESIAN_POINT('Ctrl Pts',(0.45472027561449,0.476516256240327,-1.44218384524791)) ;
#47809 = CARTESIAN_POINT('Ctrl Pts',(0.267070329812062,0.486828586095551,
-1.4884084798686)) ;
#47810 = CARTESIAN_POINT('Ctrl Pts',(-0.123236219195116,0.506155635069944,
-1.50815146953946)) ;
#47811 = CARTESIAN_POINT('Ctrl Pts',(-0.322301634956137,0.516104922990632,
-1.47846557944368)) ;
#47812 = CARTESIAN_POINT('Ctrl Pts',(-0.694584723612933,0.537753336345139,
-1.34393592303366)) ;
#47813 = CARTESIAN_POINT('Ctrl Pts',(-0.864478737203401,0.548773170428665,
-1.24148695946718)) ;
#47814 = CARTESIAN_POINT('Ctrl Pts',(-1.15023823130796,0.56974809138546,-0.981339767556789)) ;
#47815 = CARTESIAN_POINT('Ctrl Pts',(-1.26510100725959,0.579000304066912,
-0.827994526795476)) ;
#47816 = CARTESIAN_POINT('Ctrl Pts',(-1.43545918562507,0.598413953974951,
-0.478548828450786)) ;
#47817 = CARTESIAN_POINT('Ctrl Pts',(-1.4861801538254,0.609208278114524,-0.284250993938463)) ;
#47818 = CARTESIAN_POINT('Ctrl Pts',(-1.50865094126074,0.631008931292407,
0.108160763263435)) ;
#47819 = CARTESIAN_POINT('Ctrl Pts',(-1.48198631190391,0.641800785843825,
0.302414145188959)) ;
#47820 = CARTESIAN_POINT('Ctrl Pts',(-1.35687171398149,0.662087858154968,
0.667581446789534)) ;
#47821 = CARTESIAN_POINT('Ctrl Pts',(-1.26053447779002,0.670890154044406,
0.835355305823441)) ;
#47822 = CARTESIAN_POINT('Ctrl Pts',(-1.00474211289518,0.691423661370429,
1.13151619737422)) ;
#47823 = CARTESIAN_POINT('Ctrl Pts',(-0.845448042409291,0.702517983983705,
1.2550063880261)) ;
#47824 = CARTESIAN_POINT('Ctrl Pts',(-0.494690710056344,0.724227968791487,
1.42903632034362)) ;
#47825 = CARTESIAN_POINT('Ctrl Pts',(-0.307878881971955,0.734647510043461,
1.48057222771769)) ;
#47826 = CARTESIAN_POINT('Ctrl Pts',(-0.0776203706639568,0.746223695115845,
1.49849544986286)) ;
#47827 = CARTESIAN_POINT('Ctrl Pts',(-0.0387892381696761,0.748133751908426,
1.49999999999999)) ;
#47828 = CARTESIAN_POINT('Ctrl Pts',(-2.27134467272131E-13,0.749999999999992,
1.5)) ;
#47829 = CARTESIAN_POINT('Origin',(0.,1.5,0.)) ;
#47830 = CARTESIAN_POINT('',(-6.42610964440854E-14,1.25,1.5)) ;
#47831 = CARTESIAN_POINT('',(-1.31145094783846E-14,1.18749999999999,1.5)) ;
#47832 = CARTESIAN_POINT('',(-1.83697019872103E-16,1.5,1.5)) ;
#47833 = CARTESIAN_POINT('',(0.,1.5,-1.5)) ;
#47834 = CARTESIAN_POINT('Ctrl Pts',(-1.28438926161323E-13,1.25,1.5)) ;
#47835 = CARTESIAN_POINT('Ctrl Pts',(0.127128967260225,1.25611649528913,1.50000000000001)) ;
#47836 = CARTESIAN_POINT('Ctrl Pts',(0.253990145120191,1.26266892091996,1.48384268285135)) ;
#47837 = CARTESIAN_POINT('Ctrl Pts',(0.569456085887469,1.28012579796239,1.40179814679003)) ;
#47838 = CARTESIAN_POINT('Ctrl Pts',(0.749564711973221,1.29122093510874,1.31433050078366)) ;
#47839 = CARTESIAN_POINT('Ctrl Pts',(1.05939698210934,1.31266655119982,1.07893355520466)) ;
#47840 = CARTESIAN_POINT('Ctrl Pts',(1.18795943011206,1.32283575506834,0.935518907823889)) ;
#47841 = CARTESIAN_POINT('Ctrl Pts',(1.38845165379318,1.34176259152033,0.601415513490284)) ;
#47842 = CARTESIAN_POINT('Ctrl Pts',(1.45586730411665,1.35209389722695,0.412309849914715)) ;
#47843 = CARTESIAN_POINT('Ctrl Pts',(1.51257980769671,1.37379661020847,0.0216610162474451)) ;
#47844 = CARTESIAN_POINT('Ctrl Pts',(1.50248232461383,1.38476864010628,-0.175835521913221)) ;
#47845 = CARTESIAN_POINT('Ctrl Pts',(1.40835967583881,1.40556303715002,-0.550134668700435)) ;
#47846 = CARTESIAN_POINT('Ctrl Pts',(1.32741330284865,1.41457755125674,-0.723939128419645)) ;
#47847 = CARTESIAN_POINT('Ctrl Pts',(1.09974954059502,1.43429063516671,-1.03928494591313)) ;
#47848 = CARTESIAN_POINT('Ctrl Pts',(0.952416850700394,1.44517055034509,-1.17577418782125)) ;
#47849 = CARTESIAN_POINT('Ctrl Pts',(0.663476955517675,1.46398230579863,-1.35253880535885)) ;
#47850 = CARTESIAN_POINT('Ctrl Pts',(0.53453515321281,1.4717401683217,-1.40848810337764)) ;
#47851 = CARTESIAN_POINT('Ctrl Pts',(0.269540310930297,1.48652483760024,-1.48175166682828)) ;
#47852 = CARTESIAN_POINT('Ctrl Pts',(0.135093550516832,1.49350030852028,-1.5000000000001)) ;
#47853 = CARTESIAN_POINT('Ctrl Pts',(-1.11584352868732E-12,1.50000000000006,
-1.5)) ;
#47854 = CARTESIAN_POINT('',(-1.05094390383289,1.5,-1.07028823734379)) ;
#47855 = CARTESIAN_POINT('Origin',(0.,1.5,0.)) ;
#47856 = CARTESIAN_POINT('Ctrl Pts',(-1.05094390383375,1.50000000000005,-1.07028823734295)) ;
#47857 = CARTESIAN_POINT('Ctrl Pts',(-0.946934342292571,1.49215890157674,
-1.17241793551985)) ;
#47858 = CARTESIAN_POINT('Ctrl Pts',(-0.828604157750759,1.48406532833449,
-1.25883268054643)) ;
#47859 = CARTESIAN_POINT('Ctrl Pts',(-0.571466074106988,1.4679271682902,-1.394430216709)) ;
#47860 = CARTESIAN_POINT('Ctrl Pts',(-0.434119963984296,1.45996699073399,
-1.44310616777797)) ;
#47861 = CARTESIAN_POINT('Ctrl Pts',(-0.103631625899206,1.44224491368682,
-1.50867834860404)) ;
#47862 = CARTESIAN_POINT('Ctrl Pts',(0.0900562705017904,1.43343242685769,
-1.50954940292535)) ;
#47863 = CARTESIAN_POINT('Ctrl Pts',(0.469431154236831,1.41318722380876,-1.43781866690835)) ;
#47864 = CARTESIAN_POINT('Ctrl Pts',(0.651366029083658,1.40241290333334,-1.36506357669648)) ;
#47865 = CARTESIAN_POINT('Ctrl Pts',(0.981346300335995,1.38061091365567,-1.15173454360488)) ;
#47866 = CARTESIAN_POINT('Ctrl Pts',(1.125225928,1.36979706333053,-1.01164275718773)) ;
#47867 = CARTESIAN_POINT('Ctrl Pts',(1.34489832416677,1.35031785689487,-0.690875076685086)) ;
#47868 = CARTESIAN_POINT('Ctrl Pts',(1.42147844966884,1.34112468997402,-0.515244419531858)) ;
#47869 = CARTESIAN_POINT('Ctrl Pts',(1.50645493676708,1.3201887338785,-0.138397209812553)) ;
#47870 = CARTESIAN_POINT('Ctrl Pts',(1.51161612816481,1.30917840593553,0.0597886931608237)) ;
#47871 = CARTESIAN_POINT('Ctrl Pts',(1.44470672617466,1.28748460512355,0.450277107776453)) ;
#47872 = CARTESIAN_POINT('Ctrl Pts',(1.37195785681797,1.2774401639486,0.638454811703191)) ;
#47873 = CARTESIAN_POINT('Ctrl Pts',(1.16156209292362,1.2581578519111,0.968201892290707)) ;
#47874 = CARTESIAN_POINT('Ctrl Pts',(1.02867313929654,1.24787108496626,1.10835508285814)) ;
#47875 = CARTESIAN_POINT('Ctrl Pts',(0.711369794242329,1.22629592738095,1.33547524088418)) ;
#47876 = CARTESIAN_POINT('Ctrl Pts',(0.528252383420287,1.21519553135519,1.41792083851705)) ;
#47877 = CARTESIAN_POINT('Ctrl Pts',(0.224436492138917,1.19864829653047,1.48739673236104)) ;
#47878 = CARTESIAN_POINT('Ctrl Pts',(0.112278148308194,1.19290198492915,1.5)) ;
#47879 = CARTESIAN_POINT('Ctrl Pts',(-2.61943244872498E-14,1.18749999999999,
1.5)) ;
#47880 = CARTESIAN_POINT('Origin',(0.,1.5,0.)) ;
#47881 = CARTESIAN_POINT('',(1.69915517524252E-11,1.1830127018909,-1.1830127018909)) ;
#47882 = CARTESIAN_POINT('',(9.7613887853463E-10,1.35212341201692,-1.35212341201692)) ;
#47883 = CARTESIAN_POINT('',(-1.83697019872103E-16,1.5,-1.5)) ;
#47884 = CARTESIAN_POINT('Ctrl Pts',(0.190653686730815,1.17524047357919,-1.15967294634072)) ;
#47885 = CARTESIAN_POINT('Ctrl Pts',(0.122204175781398,1.17817852967127,-1.17390374658709)) ;
#47886 = CARTESIAN_POINT('Ctrl Pts',(0.0581138399920893,1.18076514130866,
-1.18076514130699)) ;
#47887 = CARTESIAN_POINT('Ctrl Pts',(3.39832483821223E-11,1.1830127018909,
-1.1830127018909)) ;
#47888 = CARTESIAN_POINT('Ctrl Pts',(0.943477955795641,1.17524047358084,-0.700742119235161)) ;
#47889 = CARTESIAN_POINT('Ctrl Pts',(0.87639271171186,1.19709475518657,-0.827718196131212)) ;
#47890 = CARTESIAN_POINT('Ctrl Pts',(0.787836640815196,1.21979792390211,-0.941972631438311)) ;
#47891 = CARTESIAN_POINT('Ctrl Pts',(0.567629405650076,1.26638165677038,-1.14223242554796)) ;
#47892 = CARTESIAN_POINT('Ctrl Pts',(0.43515803729191,1.28984247119423,-1.22380807368022)) ;
#47893 = CARTESIAN_POINT('Ctrl Pts',(0.186827921684265,1.32764663045991,-1.31906224930678)) ;
#47894 = CARTESIAN_POINT('Ctrl Pts',(0.0879972129962622,1.34101066661199,
-1.34101066648493)) ;
#47895 = CARTESIAN_POINT('Ctrl Pts',(1.95227783592045E-9,1.35212341201693,
-1.35212341201692)) ;
#47896 = CARTESIAN_POINT('Origin',(0.,-1.5,0.)) ;
#47897 = CARTESIAN_POINT('',(5.8487450577825E-15,-1.22263611415569,-1.22263611415569)) ;
#47898 = CARTESIAN_POINT('',(1.83697019872103E-16,-1.5,-1.5)) ;
#47899 = CARTESIAN_POINT('Ctrl Pts',(-0.943477955795637,-1.17524047358084,
-0.700742119235167)) ;
#47900 = CARTESIAN_POINT('Ctrl Pts',(-0.856400153191489,-1.18162007517788,
-0.828682984693854)) ;
#47901 = CARTESIAN_POINT('Ctrl Pts',(-0.74531176971572,-1.18842626255131,
-0.938491399735298)) ;
#47902 = CARTESIAN_POINT('Ctrl Pts',(-0.49287562585092,-1.20180300792309,
-1.10604526103621)) ;
#47903 = CARTESIAN_POINT('Ctrl Pts',(-0.355181554475564,-1.20825650987825,
-1.16433423964103)) ;
#47904 = CARTESIAN_POINT('Ctrl Pts',(-0.141096246039747,-1.21720626328448,
-1.21107258328805)) ;
#47905 = CARTESIAN_POINT('Ctrl Pts',(-0.071499869986318,-1.21996046433649,
-1.21996046433649)) ;
#47906 = CARTESIAN_POINT('Ctrl Pts',(1.15477603751927E-14,-1.22263611415569,
-1.22263611415569)) ;
#47907 = CARTESIAN_POINT('Ctrl Pts',(0.,-1.49999999999999,-1.49999999999999)) ;
#47908 = CARTESIAN_POINT('Ctrl Pts',(-0.054521208291996,-1.49379355370233,
-1.49379355370233)) ;
#47909 = CARTESIAN_POINT('Ctrl Pts',(-0.155386697464455,-1.4820996664401,
-1.47945377533922)) ;
#47910 = CARTESIAN_POINT('Ctrl Pts',(-0.360512792586367,-1.45487588361295,
-1.41215042182259)) ;
#47911 = CARTESIAN_POINT('Ctrl Pts',(-0.440541053484735,-1.44346315326101,
-1.37729805085287)) ;
#47912 = CARTESIAN_POINT('Ctrl Pts',(-0.660564421494151,-1.40957426184176,
-1.25580759883132)) ;
#47913 = CARTESIAN_POINT('Ctrl Pts',(-0.789067667032358,-1.38650470000743,
-1.15160047641225)) ;
#47914 = CARTESIAN_POINT('Ctrl Pts',(-1.02696295019047,-1.33537286947486,
-0.87618009528097)) ;
#47915 = CARTESIAN_POINT('Ctrl Pts',(-1.09540172650555,-1.31417335514527,
-0.731932035287483)) ;
#47916 = CARTESIAN_POINT('Ctrl Pts',(-1.18503213710912,-1.28327672009811,
-0.512590967679951)) ;
#47917 = CARTESIAN_POINT('Ctrl Pts',(-1.21503192269102,-1.26261772581496,
-0.371319335995457)) ;
#47918 = CARTESIAN_POINT('Ctrl Pts',(-1.22344776915413,-1.2195157042751,-0.092198866685286)) ;
#47919 = CARTESIAN_POINT('Ctrl Pts',(-1.20421128370105,-1.1975036728211,0.0434683361937809)) ;
#47920 = CARTESIAN_POINT('Ctrl Pts',(-1.16245326511947,-1.17524047358084,
0.172894699616844)) ;
#47921 = CARTESIAN_POINT('Origin',(0.,-1.5,0.)) ;
#47922 = CARTESIAN_POINT('Origin',(0.,-1.5,0.)) ;
#47923 = CARTESIAN_POINT('Ctrl Pts',(1.15477603751927E-14,-1.22263611415569,
-1.22263611415569)) ;
#47924 = CARTESIAN_POINT('Ctrl Pts',(0.00763880650807998,-1.22292197161608,
-1.22292197161608)) ;
#47925 = CARTESIAN_POINT('Ctrl Pts',(0.0152991705677857,-1.22320998165175,
-1.2231384112653)) ;
#47926 = CARTESIAN_POINT('Ctrl Pts',(0.188113702875513,-1.22973789977246,
-1.22642064958551)) ;
#47927 = CARTESIAN_POINT('Ctrl Pts',(0.352214880870685,-1.23655764082388,
-1.19676195776366)) ;
#47928 = CARTESIAN_POINT('Ctrl Pts',(0.65186654613245,-1.25016075841606,-1.07824422992583)) ;
#47929 = CARTESIAN_POINT('Ctrl Pts',(0.785743879428164,-1.25680894903653,
-0.993389073013124)) ;
#47930 = CARTESIAN_POINT('Ctrl Pts',(1.05115350497959,-1.27146311884125,-0.744547013637275)) ;
#47931 = CARTESIAN_POINT('Ctrl Pts',(1.13835376715091,-1.27738305068912,-0.592802361635772)) ;
#47932 = CARTESIAN_POINT('Ctrl Pts',(1.25967765756574,-1.28872257112954,-0.321841073898619)) ;
#47933 = CARTESIAN_POINT('Ctrl Pts',(1.29814354148902,-1.29570591263743,-0.152413792331758)) ;
#47934 = CARTESIAN_POINT('Ctrl Pts',(1.30662190456781,-1.30918043223515,0.18003450505882)) ;
#47935 = CARTESIAN_POINT('Ctrl Pts',(1.28098182378621,-1.31555878519823,0.339873491658122)) ;
#47936 = CARTESIAN_POINT('Ctrl Pts',(1.19729600860591,-1.32477289663106,0.573777581337942)) ;
#47937 = CARTESIAN_POINT('Ctrl Pts',(1.1595090993149,-1.32775228607298,0.652757041424446)) ;
#47938 = CARTESIAN_POINT('Ctrl Pts',(1.0217351705496,-1.33718906902534,0.881033282308611)) ;
#47939 = CARTESIAN_POINT('Ctrl Pts',(0.89957409461852,-1.34406809219364,1.01457191343034)) ;
#47940 = CARTESIAN_POINT('Ctrl Pts',(0.618226364819832,-1.35765968699375,
1.22053654692002)) ;
#47941 = CARTESIAN_POINT('Ctrl Pts',(0.463899970012846,-1.36424162041716,
1.29407692709582)) ;
#47942 = CARTESIAN_POINT('Ctrl Pts',(0.0787412807004137,-1.3788865771125,
1.3954971876506)) ;
#47943 = CARTESIAN_POINT('Ctrl Pts',(-0.112750685838222,-1.38484130930519,
1.38637264346196)) ;
#47944 = CARTESIAN_POINT('Ctrl Pts',(-0.424963139540061,-1.39609957847364,
1.34263453098656)) ;
#47945 = CARTESIAN_POINT('Ctrl Pts',(-0.601276957302403,-1.40306739103552,
1.2811021788905)) ;
#47946 = CARTESIAN_POINT('Ctrl Pts',(-0.920932661732956,-1.41694406395078,
1.09278570715895)) ;
#47947 = CARTESIAN_POINT('Ctrl Pts',(-1.06092241118538,-1.42371641827071,
0.967470185148511)) ;
#47948 = CARTESIAN_POINT('Ctrl Pts',(-1.22864359259982,-1.43307254901287,
0.743570357888767)) ;
#47949 = CARTESIAN_POINT('Ctrl Pts',(-1.27714358218595,-1.43599236885225,
0.662964068257706)) ;
#47950 = CARTESIAN_POINT('Ctrl Pts',(-1.39572498250574,-1.44518361825711,
0.41630053272665)) ;
#47951 = CARTESIAN_POINT('Ctrl Pts',(-1.44314086925414,-1.45167913699272,
0.239798991761196)) ;
#47952 = CARTESIAN_POINT('Ctrl Pts',(-1.47198220396756,-1.46528635709641,
-0.135232180635479)) ;
#47953 = CARTESIAN_POINT('Ctrl Pts',(-1.44783342734718,-1.47227055818032,
-0.330648659022112)) ;
#47954 = CARTESIAN_POINT('Ctrl Pts',(-1.35080505786766,-1.48251153393605,
-0.620873502013194)) ;
#47955 = CARTESIAN_POINT('Ctrl Pts',(-1.30387790518947,-1.48588700190698,
-0.721113686459145)) ;
#47956 = CARTESIAN_POINT('Ctrl Pts',(-1.19033775786212,-1.49278551889176,
-0.90719521171022)) ;
#47957 = CARTESIAN_POINT('Ctrl Pts',(-1.12488215104792,-1.49634374468731,
-0.992562134937736)) ;
#47958 = CARTESIAN_POINT('Ctrl Pts',(-1.05094390383307,-1.5,-1.07028823734362)) ;
#47959 = CARTESIAN_POINT('Origin',(0.,1.5,0.)) ;
#47960 = CARTESIAN_POINT('Ctrl Pts',(1.95227807856166E-9,1.35212341201693,
-1.35212341201692)) ;
#47961 = CARTESIAN_POINT('Ctrl Pts',(-0.088090331159446,1.36324791734227,
-1.36324791746946)) ;
#47962 = CARTESIAN_POINT('Ctrl Pts',(-0.165022923254981,1.37330834159026,
-1.36467558293643)) ;
#47963 = CARTESIAN_POINT('Ctrl Pts',(-0.372223984929874,1.40076164095228,
-1.35821753696589)) ;
#47964 = CARTESIAN_POINT('Ctrl Pts',(-0.517313736874783,1.42078762161895,
-1.33122592552885)) ;
#47965 = CARTESIAN_POINT('Ctrl Pts',(-0.797750176409724,1.46102555179597,
-1.2330414343537)) ;
#47966 = CARTESIAN_POINT('Ctrl Pts',(-0.931055473779404,1.48099102241791,
-1.16136888733187)) ;
#47967 = CARTESIAN_POINT('Ctrl Pts',(-1.05094390383392,1.50000000000013,-1.07028823734296)) ;
#47968 = CARTESIAN_POINT('Origin',(0.,1.5,0.)) ;
#47969 = CARTESIAN_POINT('Ctrl Pts',(3.39832483821223E-11,1.1830127018909,
-1.1830127018909)) ;
#47970 = CARTESIAN_POINT('Ctrl Pts',(-0.0881364884218503,1.1864213924446,
-1.18642139244713)) ;
#47971 = CARTESIAN_POINT('Ctrl Pts',(-0.162469886569823,1.1894852589927,-1.17963706679332)) ;
#47972 = CARTESIAN_POINT('Ctrl Pts',(-0.344721916499354,1.19717151895269,
-1.15365394859358)) ;
#47973 = CARTESIAN_POINT('Ctrl Pts',(-0.468394433977734,1.20277853643706,
-1.11526159830785)) ;
#47974 = CARTESIAN_POINT('Ctrl Pts',(-0.717977954481682,1.21494469994253,
-0.991479164438509)) ;
#47975 = CARTESIAN_POINT('Ctrl Pts',(-0.838726254773585,1.22140244274215,
-0.900448279090885)) ;
#47976 = CARTESIAN_POINT('Ctrl Pts',(-0.993074931050609,1.23066292138297,
-0.731155613055594)) ;
#47977 = CARTESIAN_POINT('Ctrl Pts',(-1.03996298568237,1.23364082281887,-0.668434677590451)) ;
#47978 = CARTESIAN_POINT('Ctrl Pts',(-1.16787199372824,1.24287513018846,-0.456760585322658)) ;
#47979 = CARTESIAN_POINT('Ctrl Pts',(-1.22498602286769,1.24969109010067,-0.298218403352094)) ;
#47980 = CARTESIAN_POINT('Ctrl Pts',(-1.27299648961919,1.26329436412094,0.0239120303898897)) ;
#47981 = CARTESIAN_POINT('Ctrl Pts',(-1.26652670310226,1.26994623938014,0.184012297019625)) ;
#47982 = CARTESIAN_POINT('Ctrl Pts',(-1.18346232080173,1.28455636029785,0.540836393778874)) ;
#47983 = CARTESIAN_POINT('Ctrl Pts',(-1.09549431485504,1.29047203254427,0.69388259441924)) ;
#47984 = CARTESIAN_POINT('Ctrl Pts',(-0.919018352996627,1.30186467240575,
0.938319739625856)) ;
#47985 = CARTESIAN_POINT('Ctrl Pts',(-0.790286241919958,1.30884866284902,
1.05769021139879)) ;
#47986 = CARTESIAN_POINT('Ctrl Pts',(-0.503791478080934,1.3223282587274,1.23329014532573)) ;
#47987 = CARTESIAN_POINT('Ctrl Pts',(-0.35101607093844,1.32871063087591,1.29171656762766)) ;
#47988 = CARTESIAN_POINT('Ctrl Pts',(0.00224632758886806,1.34190441912239,
1.35625398851413)) ;
#47989 = CARTESIAN_POINT('Ctrl Pts',(0.184090354887929,1.34784528749819,1.34460482878569)) ;
#47990 = CARTESIAN_POINT('Ctrl Pts',(0.509771235001103,1.36037444892477,1.27326893451926)) ;
#47991 = CARTESIAN_POINT('Ctrl Pts',(0.671642444484427,1.36717720200835,1.20354849922269)) ;
#47992 = CARTESIAN_POINT('Ctrl Pts',(0.965216569005918,1.3807389647173,1.00366016750726)) ;
#47993 = CARTESIAN_POINT('Ctrl Pts',(1.09284305366252,1.38735662928258,0.873505715555011)) ;
#47994 = CARTESIAN_POINT('Ctrl Pts',(1.24736640638551,1.39674825266539,0.636722907990449)) ;
#47995 = CARTESIAN_POINT('Ctrl Pts',(1.33749441009985,1.40274261027107,0.479517003122467)) ;
#47996 = CARTESIAN_POINT('Ctrl Pts',(1.42759692443734,1.41784814293474,0.0788339234383507)) ;
#47997 = CARTESIAN_POINT('Ctrl Pts',(1.43262059128626,1.42476051709303,-0.107230746119766)) ;
#47998 = CARTESIAN_POINT('Ctrl Pts',(1.38677319302375,1.43471221787533,-0.378874130966391)) ;
#47999 = CARTESIAN_POINT('Ctrl Pts',(1.36300563214594,1.43791909864246,-0.467028878906141)) ;
#48000 = CARTESIAN_POINT('Ctrl Pts',(1.25904594518336,1.44792023136461,-0.743648780311062)) ;
#48001 = CARTESIAN_POINT('Ctrl Pts',(1.15202715535141,1.45375905173618,-0.902957154604828)) ;
#48002 = CARTESIAN_POINT('Ctrl Pts',(0.90829713609045,1.46628394022629,-1.16634790760792)) ;
#48003 = CARTESIAN_POINT('Ctrl Pts',(0.755164312600782,1.47308966663899,-1.2787102515016)) ;
#48004 = CARTESIAN_POINT('Ctrl Pts',(0.4969372415121,1.48321248126175,-1.40087759364243)) ;
#48005 = CARTESIAN_POINT('Ctrl Pts',(0.404922654524661,1.48660505005347,-1.43370843375369)) ;
#48006 = CARTESIAN_POINT('Ctrl Pts',(0.208709632125688,1.49342040871883,-1.48246367972118)) ;
#48007 = CARTESIAN_POINT('Ctrl Pts',(0.104681834995791,1.49680698242307,-1.49680698242307)) ;
#48008 = CARTESIAN_POINT('Ctrl Pts',(2.33493779866478E-14,1.5,-1.5)) ;
#48009 = CARTESIAN_POINT('Origin',(0.,1.5,0.)) ;
#48010 = CARTESIAN_POINT('Ctrl Pts',(-2.6045321936897E-14,1.18749999999999,
1.5)) ;
#48011 = CARTESIAN_POINT('Ctrl Pts',(-0.0798363712549382,1.18365887079706,
1.5)) ;
#48012 = CARTESIAN_POINT('Ctrl Pts',(-0.159716095570403,1.1796386315509,1.49362712814615)) ;
#48013 = CARTESIAN_POINT('Ctrl Pts',(-0.43003397416229,1.165421652833,1.45002019421712)) ;
#48014 = CARTESIAN_POINT('Ctrl Pts',(-0.613395332234769,1.15472324803505,
1.38246880981732)) ;
#48015 = CARTESIAN_POINT('Ctrl Pts',(-0.948787731355424,1.13292657122318,
1.17870512033934)) ;
#48016 = CARTESIAN_POINT('Ctrl Pts',(-1.096542244985,1.12203894221217,1.04266880059696)) ;
#48017 = CARTESIAN_POINT('Ctrl Pts',(-1.32519419631909,1.10229714159564,0.728000775362096)) ;
#48018 = CARTESIAN_POINT('Ctrl Pts',(-1.40668218866386,1.09330106024026,0.554419084324286)) ;
#48019 = CARTESIAN_POINT('Ctrl Pts',(-1.50192885849926,1.07252432270249,0.180437808644521)) ;
#48020 = CARTESIAN_POINT('Ctrl Pts',(-1.51263201628805,1.06155746974118,-0.0169655446590038)) ;
#48021 = CARTESIAN_POINT('Ctrl Pts',(-1.45715689112896,1.03984854017038,-0.407726276933393)) ;
#48022 = CARTESIAN_POINT('Ctrl Pts',(-1.39033878469355,1.02947503072142,-0.597036308852029)) ;
#48023 = CARTESIAN_POINT('Ctrl Pts',(-1.19093892832266,1.01058488791976,-0.931710767455425)) ;
#48024 = CARTESIAN_POINT('Ctrl Pts',(-1.06287946255845,1.00042968985607,-1.07549239665475)) ;
#48025 = CARTESIAN_POINT('Ctrl Pts',(-0.753920534884024,0.97900005206253,
-1.31182679703802)) ;
#48026 = CARTESIAN_POINT('Ctrl Pts',(-0.574166690500253,0.967906112079596,
-1.39986584509514)) ;
#48027 = CARTESIAN_POINT('Ctrl Pts',(-0.194540542660304,0.946860401386108,
-1.49997965412028)) ;
#48028 = CARTESIAN_POINT('Ctrl Pts',(0.0012248453091426,0.937789401646168,
-1.51253995356844)) ;
#48029 = CARTESIAN_POINT('Ctrl Pts',(0.385378877770893,0.917915273631611,
-1.46244564720063)) ;
#48030 = CARTESIAN_POINT('Ctrl Pts',(0.570169026992564,0.907311327584705,
-1.40076951670215)) ;
#48031 = CARTESIAN_POINT('Ctrl Pts',(0.912876418247017,0.885441247393907,
-1.20703324361547)) ;
#48032 = CARTESIAN_POINT('Ctrl Pts',(1.0660107708773,0.874383822393379,-1.07420242273627)) ;
#48033 = CARTESIAN_POINT('Ctrl Pts',(1.30465774113417,0.854293103028418,-0.76428520315489)) ;
#48034 = CARTESIAN_POINT('Ctrl Pts',(1.39104230863307,0.84542671616715,-0.592680891008473)) ;
#48035 = CARTESIAN_POINT('Ctrl Pts',(1.49634230880408,0.824810437592514,-0.221587876665044)) ;
#48036 = CARTESIAN_POINT('Ctrl Pts',(1.51244984009989,0.813894455278159,-0.0251001950066589)) ;
#48037 = CARTESIAN_POINT('Ctrl Pts',(1.46807171896181,0.792143001247831,0.366425977539252)) ;
#48038 = CARTESIAN_POINT('Ctrl Pts',(1.40665379793001,0.781525406973956,0.557542674469026)) ;
#48039 = CARTESIAN_POINT('Ctrl Pts',(1.2170138822344,0.762652401431149,0.897256774239602)) ;
#48040 = CARTESIAN_POINT('Ctrl Pts',(1.09349182081601,0.752769599104504,1.04427782355261)) ;
#48041 = CARTESIAN_POINT('Ctrl Pts',(0.792333292811163,0.731485057323399,
1.28889945603531)) ;
#48042 = CARTESIAN_POINT('Ctrl Pts',(0.615815035989745,0.720407146400333,
1.38196565998746)) ;
#48043 = CARTESIAN_POINT('Ctrl Pts',(0.287670719484251,0.701917111808417,
1.47924427689397)) ;
#48044 = CARTESIAN_POINT('Ctrl Pts',(0.144088320348377,0.694432452545015,
1.50000000000002)) ;
#48045 = CARTESIAN_POINT('Ctrl Pts',(-2.47926679186605E-13,0.687499999999986,
1.5)) ;
#48046 = CARTESIAN_POINT('Ctrl Pts',(-2.2735285876152E-13,0.749999999999992,
1.5)) ;
#48047 = CARTESIAN_POINT('Ctrl Pts',(0.158006103608433,0.75760207220433,1.50000000000002)) ;
#48048 = CARTESIAN_POINT('Ctrl Pts',(0.315250620966226,0.765860831423893,
1.47504016137086)) ;
#48049 = CARTESIAN_POINT('Ctrl Pts',(0.653267439396651,0.78519192030018,1.36458326515879)) ;
#48050 = CARTESIAN_POINT('Ctrl Pts',(0.82672058281258,0.796246860045977,1.26703509143898)) ;
#48051 = CARTESIAN_POINT('Ctrl Pts',(1.12063201557542,0.817387540584502,1.01504012652266)) ;
#48052 = CARTESIAN_POINT('Ctrl Pts',(1.24005937638741,0.826940670742474,0.865067926635356)) ;
#48053 = CARTESIAN_POINT('Ctrl Pts',(1.42068979071896,0.84606941821889,0.520750472059851)) ;
#48054 = CARTESIAN_POINT('Ctrl Pts',(1.47712141321613,0.856773999403544,0.328068010736083)) ;
#48055 = CARTESIAN_POINT('Ctrl Pts',(1.51123898851943,0.878557009171926,-0.0640261650948025)) ;
#48056 = CARTESIAN_POINT('Ctrl Pts',(1.49016513143508,0.889418731933562,-0.259537174804263)) ;
#48057 = CARTESIAN_POINT('Ctrl Pts',(1.37557842161795,0.909882833718419,-0.627891006931695)) ;
#48058 = CARTESIAN_POINT('Ctrl Pts',(1.28458176657173,0.918686934078499,-0.797690513005034)) ;
#48059 = CARTESIAN_POINT('Ctrl Pts',(1.03793264536063,0.938986325811679,-1.10125980581968)) ;
#48060 = CARTESIAN_POINT('Ctrl Pts',(0.88186907475974,0.950065062357037,-1.22978428796118)) ;
#48061 = CARTESIAN_POINT('Ctrl Pts',(0.535285523623325,0.97186839266754,-1.41440385950336)) ;
#48062 = CARTESIAN_POINT('Ctrl Pts',(0.349488035948599,0.982390114957565,
-1.47137517337296)) ;
#48063 = CARTESIAN_POINT('Ctrl Pts',(-0.0365994568080561,1.00210159403079,
-1.51226526638763)) ;
#48064 = CARTESIAN_POINT('Ctrl Pts',(-0.233325040066266,1.01137560495447,
-1.49460904571161)) ;
#48065 = CARTESIAN_POINT('Ctrl Pts',(-0.610896023456313,1.03260960557388,
-1.38415715010836)) ;
#48066 = CARTESIAN_POINT('Ctrl Pts',(-0.787805789672123,1.04368992503295,
-1.2916823530226)) ;
#48067 = CARTESIAN_POINT('Ctrl Pts',(-1.08990680135838,1.06499292132518,-1.04802878776064)) ;
#48068 = CARTESIAN_POINT('Ctrl Pts',(-1.21396431585872,1.07492285292586,-0.901388647334283)) ;
#48069 = CARTESIAN_POINT('Ctrl Pts',(-1.40476782507156,1.09376243663884,-0.562276140500701)) ;
#48070 = CARTESIAN_POINT('Ctrl Pts',(-1.46682776544324,1.10436823503014,-0.371371769457348)) ;
#48071 = CARTESIAN_POINT('Ctrl Pts',(-1.51253331375705,1.12611450906356,0.0200611631441543)) ;
#48072 = CARTESIAN_POINT('Ctrl Pts',(-1.49707111289976,1.13703701072081,0.216666192974721)) ;
#48073 = CARTESIAN_POINT('Ctrl Pts',(-1.39297412284888,1.15767272633219,0.588109073979515)) ;
#48074 = CARTESIAN_POINT('Ctrl Pts',(-1.30718060273184,1.1665512616293,0.759948637254943)) ;
#48075 = CARTESIAN_POINT('Ctrl Pts',(-1.06956567425292,1.18661482367153,1.07067574201322)) ;
#48076 = CARTESIAN_POINT('Ctrl Pts',(-0.916815781785327,1.19766898747329,
1.20405506427194)) ;
#48077 = CARTESIAN_POINT('Ctrl Pts',(-0.574623050279518,1.21954667255649,
1.39895653031842)) ;
#48078 = CARTESIAN_POINT('Ctrl Pts',(-0.389970772161892,1.2301607365114,1.46123570526209)) ;
#48079 = CARTESIAN_POINT('Ctrl Pts',(-0.132606832253855,1.24349796140355,
1.49560838142262)) ;
#48080 = CARTESIAN_POINT('Ctrl Pts',(-0.0662729511061171,1.24681144115324,
1.49999999999999)) ;
#48081 = CARTESIAN_POINT('Ctrl Pts',(-1.28338495868299E-13,1.25,1.5)) ;
#48082 = CARTESIAN_POINT('Origin',(3.46944695195362E-16,1.71875,2.77555756156289E-16)) ;
#48083 = CARTESIAN_POINT('Ctrl Pts',(-5.38273142618428E-13,0.93749999999997,
1.17524047358083)) ;
#48084 = CARTESIAN_POINT('Ctrl Pts',(-0.0372628755316404,0.935211773494173,
1.17524047358081)) ;
#48085 = CARTESIAN_POINT('Ctrl Pts',(-0.0745659590150219,0.932858250931482,
1.1734683901451)) ;
#48086 = CARTESIAN_POINT('Ctrl Pts',(-0.261993141982916,0.920713849671594,
1.15555958845237)) ;
#48087 = CARTESIAN_POINT('Ctrl Pts',(-0.408006918246224,0.910217893515267,
1.11241632793315)) ;
#48088 = CARTESIAN_POINT('Ctrl Pts',(-0.680959750452341,0.888428495475987,
0.970597722086583)) ;
#48089 = CARTESIAN_POINT('Ctrl Pts',(-0.804232669945397,0.877334580368952,
0.871200248783751)) ;
#48090 = CARTESIAN_POINT('Ctrl Pts',(-1.00011814589685,0.856937259941698,
0.63516168914757)) ;
#48091 = CARTESIAN_POINT('Ctrl Pts',(-1.07288678901601,0.848136373379309,
0.50257569992399)) ;
#48092 = CARTESIAN_POINT('Ctrl Pts',(-1.16553188026456,0.827712242222803,
0.214536513049786)) ;
#48093 = CARTESIAN_POINT('Ctrl Pts',(-1.18351018505052,0.816861997968989,
0.0615167587059378)) ;
#48094 = CARTESIAN_POINT('Ctrl Pts',(-1.15971835407239,0.795053447968922,
-0.246046728856358)) ;
#48095 = CARTESIAN_POINT('Ctrl Pts',(-1.11689632394281,0.784310216512354,
-0.397557293954039)) ;
#48096 = CARTESIAN_POINT('Ctrl Pts',(-0.977772301015633,0.765075235042987,
-0.668826038730583)) ;
#48097 = CARTESIAN_POINT('Ctrl Pts',(-0.885233845820656,0.755616003331456,
-0.787246054793336)) ;
#48098 = CARTESIAN_POINT('Ctrl Pts',(-0.656668880959004,0.734504563011645,
-0.986824381689021)) ;
#48099 = CARTESIAN_POINT('Ctrl Pts',(-0.521463213671476,0.723448798493307,
-1.06447766275569)) ;
#48100 = CARTESIAN_POINT('Ctrl Pts',(-0.228029199857764,0.701925845536696,
-1.16330653237555)) ;
#48101 = CARTESIAN_POINT('Ctrl Pts',(-0.072637477112143,0.692242977263605,
-1.18320800497987)) ;
#48102 = CARTESIAN_POINT('Ctrl Pts',(0.232265954968764,0.672762373986269,
-1.16185079863502)) ;
#48103 = CARTESIAN_POINT('Ctrl Pts',(0.378967024087167,0.662361862018095,
-1.12259004120972)) ;
#48104 = CARTESIAN_POINT('Ctrl Pts',(0.654832807433886,0.64066215361674,-0.988346580159853)) ;
#48105 = CARTESIAN_POINT('Ctrl Pts',(0.780380539295739,0.629556355256246,
-0.892554021127282)) ;
#48106 = CARTESIAN_POINT('Ctrl Pts',(0.982771364807177,0.608947755585498,
-0.661823763413569)) ;
#48107 = CARTESIAN_POINT('Ctrl Pts',(1.05935465762482,0.600128932644653,-0.530676535459642)) ;
#48108 = CARTESIAN_POINT('Ctrl Pts',(1.15947644658547,0.579866759244312,-0.244921420306135)) ;
#48109 = CARTESIAN_POINT('Ctrl Pts',(1.18141591408789,0.569082068675803,-0.0928261620922505)) ;
#48110 = CARTESIAN_POINT('Ctrl Pts',(1.16589585188604,0.547262074423877,0.214898722445718)) ;
#48111 = CARTESIAN_POINT('Ctrl Pts',(1.12713807580175,0.536439614695771,0.367526634799766)) ;
#48112 = CARTESIAN_POINT('Ctrl Pts',(0.995315864577872,0.51694735128298,0.642423797412707)) ;
#48113 = CARTESIAN_POINT('Ctrl Pts',(0.906006071567535,0.507742733730941,
0.763238533768287)) ;
#48114 = CARTESIAN_POINT('Ctrl Pts',(0.683219861600841,0.48678232321035,0.968566045760291)) ;
#48115 = CARTESIAN_POINT('Ctrl Pts',(0.550553352182226,0.475760290415287,
1.04966584798988)) ;
#48116 = CARTESIAN_POINT('Ctrl Pts',(0.275839516173969,0.455305018730002,
1.15080424286477)) ;
#48117 = CARTESIAN_POINT('Ctrl Pts',(0.138388810772653,0.445998134950735,
1.17524047358085)) ;
#48118 = CARTESIAN_POINT('Ctrl Pts',(-1.67053870736567E-13,0.437499999999993,
1.17524047358083)) ;
#48119 = CARTESIAN_POINT('Ctrl Pts',(-3.7771868965919E-13,0.499999999999977,
1.17524047358083)) ;
#48120 = CARTESIAN_POINT('Ctrl Pts',(0.129223051317171,0.507935286983878,
1.17524047358087)) ;
#48121 = CARTESIAN_POINT('Ctrl Pts',(0.257722867946538,0.516581478161535,
1.15393619320277)) ;
#48122 = CARTESIAN_POINT('Ctrl Pts',(0.526404828087052,0.536338948242251,
1.06203231537727)) ;
#48123 = CARTESIAN_POINT('Ctrl Pts',(0.661187746072155,0.547389584135236,
0.983791467874058)) ;
#48124 = CARTESIAN_POINT('Ctrl Pts',(0.88877885643814,0.568475796884882,0.783237938588865)) ;
#48125 = CARTESIAN_POINT('Ctrl Pts',(0.980771591358329,0.577887854325915,
0.664417204720868)) ;
#48126 = CARTESIAN_POINT('Ctrl Pts',(1.11867208140571,0.597166381725078,0.392534336674487)) ;
#48127 = CARTESIAN_POINT('Ctrl Pts',(1.16081391242959,0.607923470814767,0.240828338961106)) ;
#48128 = CARTESIAN_POINT('Ctrl Pts',(1.1832164248039,0.629735054227077,-0.0667779284672581)) ;
#48129 = CARTESIAN_POINT('Ctrl Pts',(1.16457058127801,0.640574794194408,-0.219649542059652)) ;
#48130 = CARTESIAN_POINT('Ctrl Pts',(1.07066961934905,0.660971988217725,-0.507308837623868)) ;
#48131 = CARTESIAN_POINT('Ctrl Pts',(0.997265697009338,0.66977164251845,-0.639652621257518)) ;
#48132 = CARTESIAN_POINT('Ctrl Pts',(0.800290746129714,0.690204620729973,
-0.874809910275015)) ;
#48133 = CARTESIAN_POINT('Ctrl Pts',(0.676631046005103,0.701301073419951,
-0.973609034356905)) ;
#48134 = CARTESIAN_POINT('Ctrl Pts',(0.403177716849776,0.723076512512997,
-1.11416703121241)) ;
#48135 = CARTESIAN_POINT('Ctrl Pts',(0.257042102550089,0.733556992879919,
-1.15666275548468)) ;
#48136 = CARTESIAN_POINT('Ctrl Pts',(-0.0465990627160015,0.753185598951027,
-1.18438080504815)) ;
#48137 = CARTESIAN_POINT('Ctrl Pts',(-0.201291410338131,0.762614474487315,
-1.16808644012264)) ;
#48138 = CARTESIAN_POINT('Ctrl Pts',(-0.496304589811692,0.783978003088777,
-1.07648945257075)) ;
#48139 = CARTESIAN_POINT('Ctrl Pts',(-0.633609369050849,0.795056149017342,
-1.00184065511535)) ;
#48140 = CARTESIAN_POINT('Ctrl Pts',(-0.867086037178609,0.816293390128693,
-0.807221339464417)) ;
#48141 = CARTESIAN_POINT('Ctrl Pts',(-0.962388287817152,0.82601667662179,
-0.690806209974619)) ;
#48142 = CARTESIAN_POINT('Ctrl Pts',(-1.1076412594506,0.845030925675896,-0.42265042921707)) ;
#48143 = CARTESIAN_POINT('Ctrl Pts',(-1.15386377952163,0.855701220641653,
-0.272168479111453)) ;
#48144 = CARTESIAN_POINT('Ctrl Pts',(-1.18463152093458,0.877487754511793,
0.0350845174872771)) ;
#48145 = CARTESIAN_POINT('Ctrl Pts',(-1.17001865458337,0.888387649497562,
0.188804490427957)) ;
#48146 = CARTESIAN_POINT('Ctrl Pts',(-1.08368335874431,0.908945399855658,
0.478728093627223)) ;
#48147 = CARTESIAN_POINT('Ctrl Pts',(-1.01407322451917,0.917778187139484,
0.612537166206886)) ;
#48148 = CARTESIAN_POINT('Ctrl Pts',(-0.82364121359487,0.937995371190235,
0.852940518897035)) ;
#48149 = CARTESIAN_POINT('Ctrl Pts',(-0.702338222167855,0.949073319536787,
0.955299652901863)) ;
#48150 = CARTESIAN_POINT('Ctrl Pts',(-0.431965145235364,0.970926219230269,
1.1033776390932)) ;
#48151 = CARTESIAN_POINT('Ctrl Pts',(-0.286601196028543,0.981496568904902,
1.14974475965885)) ;
#48152 = CARTESIAN_POINT('Ctrl Pts',(-0.0910484835269777,0.994315250465939,
1.1725983273716)) ;
#48153 = CARTESIAN_POINT('Ctrl Pts',(-0.0455011814096055,0.997205878294077,
1.17524047358081)) ;
#48154 = CARTESIAN_POINT('Ctrl Pts',(-4.39631847705415E-13,0.999999999999973,
1.17524047358083)) ;
#48155 = CARTESIAN_POINT('Origin',(0.,-1.5,0.)) ;
#48156 = CARTESIAN_POINT('',(1.375,-1.5,2.38156986040721)) ;
#48157 = CARTESIAN_POINT('',(-1.375,-1.5,2.38156986040721)) ;
#48158 = CARTESIAN_POINT('Origin',(0.,-1.5,0.)) ;
#48159 = CARTESIAN_POINT('',(-1.62356638414832E-15,-1.25437990693814,3.17542648054294)) ;
#48160 = CARTESIAN_POINT('Ctrl Pts',(-5.29571615987166E-11,-1.25437990692049,
3.17542648057351)) ;
#48161 = CARTESIAN_POINT('Ctrl Pts',(0.736860279164301,-1.5,2.75000000001228)) ;
#48162 = CARTESIAN_POINT('Ctrl Pts',(1.375,-1.5,2.3815698604072)) ;
#48163 = CARTESIAN_POINT('Ctrl Pts',(-1.375,-1.5,2.3815698604072)) ;
#48164 = CARTESIAN_POINT('Ctrl Pts',(-0.736860279164307,-1.5,2.75000000001228)) ;
#48165 = CARTESIAN_POINT('Ctrl Pts',(5.29522918189065E-11,-1.25437990692049,
3.17542648057351)) ;
#48166 = CARTESIAN_POINT('Origin',(0.,1.5,0.)) ;
#48167 = CARTESIAN_POINT('',(-1.375,1.5,2.3815698604072)) ;
#48168 = CARTESIAN_POINT('',(1.375,1.5,2.3815698604072)) ;
#48169 = CARTESIAN_POINT('Origin',(0.,1.5,0.)) ;
#48170 = CARTESIAN_POINT('',(-1.62356638414832E-15,1.25437990693814,3.17542648054294)) ;
#48171 = CARTESIAN_POINT('Ctrl Pts',(-1.375,1.5,2.38156986040721)) ;
#48172 = CARTESIAN_POINT('Ctrl Pts',(-0.736860279164303,1.5,2.75000000001229)) ;
#48173 = CARTESIAN_POINT('Ctrl Pts',(5.29529270075774E-11,1.25437990692049,
3.17542648057351)) ;
#48174 = CARTESIAN_POINT('Ctrl Pts',(-5.29455164730837E-11,1.25437990692049,
3.17542648057351)) ;
#48175 = CARTESIAN_POINT('Ctrl Pts',(0.736860279164306,1.5,2.75000000001228)) ;
#48176 = CARTESIAN_POINT('Ctrl Pts',(1.375,1.5,2.3815698604072)) ;
#48177 = CARTESIAN_POINT('Ctrl Pts',(-0.00478010547540694,1.68781364799072,
-1.17519533396634)) ;
#48178 = CARTESIAN_POINT('Ctrl Pts',(0.676909706932224,1.64604970885937,-1.17796810638181)) ;
#48179 = CARTESIAN_POINT('Ctrl Pts',(1.01775743268642,1.60418711532683,-0.587602527731244)) ;
#48180 = CARTESIAN_POINT('Ctrl Pts',(1.35700991024855,1.56252044866016,-8.30928921498564E-17)) ;
#48181 = CARTESIAN_POINT('Ctrl Pts',(1.01775743268642,1.52085378199349,0.587602527731244)) ;
#48182 = CARTESIAN_POINT('Ctrl Pts',(0.678504955124277,1.47918711532683,1.17520505546249)) ;
#48183 = CARTESIAN_POINT('Ctrl Pts',(1.43921110951392E-16,1.43752044866016,
1.17520505546249)) ;
#48184 = CARTESIAN_POINT('Ctrl Pts',(-0.678504955124276,1.39585378199349,
1.17520505546249)) ;
#48185 = CARTESIAN_POINT('Ctrl Pts',(-1.01775743268641,1.35418711532683,0.587602527731245)) ;
#48186 = CARTESIAN_POINT('Ctrl Pts',(-1.35700991024855,1.31252044866016,2.49278676449569E-16)) ;
#48187 = CARTESIAN_POINT('Ctrl Pts',(-1.01775743268642,1.27085378199349,-0.587602527731243)) ;
#48188 = CARTESIAN_POINT('Ctrl Pts',(-0.678504955124277,1.22918711532683,
-1.17520505546249)) ;
#48189 = CARTESIAN_POINT('Ctrl Pts',(0.,1.18752044866016,-1.17520505546249)) ;
#48190 = CARTESIAN_POINT('Ctrl Pts',(0.678504955124277,1.14585378199349,-1.17520505546249)) ;
#48191 = CARTESIAN_POINT('Ctrl Pts',(1.01775743268642,1.10418711532683,-0.587602527731244)) ;
#48192 = CARTESIAN_POINT('Ctrl Pts',(1.35700991024855,1.06252044866016,-8.30928921498564E-17)) ;
#48193 = CARTESIAN_POINT('Ctrl Pts',(1.01775743268642,1.02085378199349,0.587602527731244)) ;
#48194 = CARTESIAN_POINT('Ctrl Pts',(0.678504955124277,0.979187115326827,
1.17520505546249)) ;
#48195 = CARTESIAN_POINT('Ctrl Pts',(1.43921110951392E-16,0.937520448660161,
1.17520505546249)) ;
#48196 = CARTESIAN_POINT('Ctrl Pts',(-0.678504955124276,0.895853781993494,
1.17520505546249)) ;
#48197 = CARTESIAN_POINT('Ctrl Pts',(-1.01775743268641,0.854187115326828,
0.587602527731245)) ;
#48198 = CARTESIAN_POINT('Ctrl Pts',(-1.35700991024855,0.812520448660161,
2.49278676449569E-16)) ;
#48199 = CARTESIAN_POINT('Ctrl Pts',(-1.01775743268642,0.770853781993494,
-0.587602527731243)) ;
#48200 = CARTESIAN_POINT('Ctrl Pts',(-0.678504955124277,0.729187115326828,
-1.17520505546249)) ;
#48201 = CARTESIAN_POINT('Ctrl Pts',(0.,0.687520448660161,-1.17520505546249)) ;
#48202 = CARTESIAN_POINT('Ctrl Pts',(0.678504955124277,0.645853781993494,
-1.17520505546249)) ;
#48203 = CARTESIAN_POINT('Ctrl Pts',(1.01775743268642,0.604187115326828,-0.587602527731244)) ;
#48204 = CARTESIAN_POINT('Ctrl Pts',(1.35700991024855,0.562520448660161,-8.30928921498564E-17)) ;
#48205 = CARTESIAN_POINT('Ctrl Pts',(1.01775743268642,0.520853781993494,0.587602527731244)) ;
#48206 = CARTESIAN_POINT('Ctrl Pts',(0.678504955124277,0.479187115326828,
1.17520505546249)) ;
#48207 = CARTESIAN_POINT('Ctrl Pts',(1.43921110951392E-16,0.437520448660161,
1.17520505546249)) ;
#48208 = CARTESIAN_POINT('Ctrl Pts',(-0.678504955124276,0.395853781993494,
1.17520505546249)) ;
#48209 = CARTESIAN_POINT('Ctrl Pts',(-1.01775743268641,0.354187115326828,
0.587602527731245)) ;
#48210 = CARTESIAN_POINT('Ctrl Pts',(-1.35700991024855,0.312520448660161,
2.49278676449569E-16)) ;
#48211 = CARTESIAN_POINT('Ctrl Pts',(-1.01775743268642,0.270853781993494,
-0.587602527731243)) ;
#48212 = CARTESIAN_POINT('Ctrl Pts',(-0.678504955124277,0.229187115326828,
-1.17520505546249)) ;
#48213 = CARTESIAN_POINT('Ctrl Pts',(0.,0.187520448660161,-1.17520505546249)) ;
#48214 = CARTESIAN_POINT('Ctrl Pts',(0.678504955124277,0.145853781993494,
-1.17520505546249)) ;
#48215 = CARTESIAN_POINT('Ctrl Pts',(1.01775743268642,0.104187115326828,-0.587602527731244)) ;
#48216 = CARTESIAN_POINT('Ctrl Pts',(1.35700991024855,0.0625204486601609,
-8.30928921498564E-17)) ;
#48217 = CARTESIAN_POINT('Ctrl Pts',(1.01775743268642,0.0208537819934942,
0.587602527731244)) ;
#48218 = CARTESIAN_POINT('Ctrl Pts',(0.678504955124277,-0.0208128846731724,
1.17520505546249)) ;
#48219 = CARTESIAN_POINT('Ctrl Pts',(1.43921110951392E-16,-0.0624795513398393,
1.17520505546249)) ;
#48220 = CARTESIAN_POINT('Ctrl Pts',(-0.678504955124276,-0.104146218006506,
1.17520505546249)) ;
#48221 = CARTESIAN_POINT('Ctrl Pts',(-1.01775743268641,-0.145812884673173,
0.587602527731245)) ;
#48222 = CARTESIAN_POINT('Ctrl Pts',(-1.35700991024855,-0.187479551339839,
2.49278676449569E-16)) ;
#48223 = CARTESIAN_POINT('Ctrl Pts',(-1.01775743268642,-0.229146218006506,
-0.587602527731243)) ;
#48224 = CARTESIAN_POINT('Ctrl Pts',(-0.678504955124277,-0.270812884673172,
-1.17520505546249)) ;
#48225 = CARTESIAN_POINT('Ctrl Pts',(0.,-0.312479551339839,-1.17520505546249)) ;
#48226 = CARTESIAN_POINT('Ctrl Pts',(0.678504955124277,-0.354146218006506,
-1.17520505546249)) ;
#48227 = CARTESIAN_POINT('Ctrl Pts',(1.01775743268642,-0.395812884673173,
-0.587602527731244)) ;
#48228 = CARTESIAN_POINT('Ctrl Pts',(1.35700991024855,-0.437479551339839,
-8.30928921498564E-17)) ;
#48229 = CARTESIAN_POINT('Ctrl Pts',(1.01775743268642,-0.479146218006506,
0.587602527731244)) ;
#48230 = CARTESIAN_POINT('Ctrl Pts',(0.678504955124277,-0.520812884673173,
1.17520505546249)) ;
#48231 = CARTESIAN_POINT('Ctrl Pts',(1.43921110951392E-16,-0.562479551339839,
1.17520505546249)) ;
#48232 = CARTESIAN_POINT('Ctrl Pts',(-0.678504955124276,-0.604146218006506,
1.17520505546249)) ;
#48233 = CARTESIAN_POINT('Ctrl Pts',(-1.01775743268641,-0.645812884673172,
0.587602527731245)) ;
#48234 = CARTESIAN_POINT('Ctrl Pts',(-1.35700991024855,-0.687479551339839,
2.49278676449569E-16)) ;
#48235 = CARTESIAN_POINT('Ctrl Pts',(-1.01775743268642,-0.729146218006506,
-0.587602527731243)) ;
#48236 = CARTESIAN_POINT('Ctrl Pts',(-0.678504955124277,-0.770812884673173,
-1.17520505546249)) ;
#48237 = CARTESIAN_POINT('Ctrl Pts',(0.,-0.812479551339839,-1.17520505546249)) ;
#48238 = CARTESIAN_POINT('Ctrl Pts',(0.678504955124277,-0.854146218006506,
-1.17520505546249)) ;
#48239 = CARTESIAN_POINT('Ctrl Pts',(1.01775743268642,-0.895812884673173,
-0.587602527731244)) ;
#48240 = CARTESIAN_POINT('Ctrl Pts',(1.35700991024855,-0.937479551339839,
-8.30928921498564E-17)) ;
#48241 = CARTESIAN_POINT('Ctrl Pts',(1.01775743268642,-0.979146218006506,
0.587602527731244)) ;
#48242 = CARTESIAN_POINT('Ctrl Pts',(0.678504955124277,-1.02081288467317,
1.17520505546249)) ;
#48243 = CARTESIAN_POINT('Ctrl Pts',(1.43921110951392E-16,-1.06247955133984,
1.17520505546249)) ;
#48244 = CARTESIAN_POINT('Ctrl Pts',(-0.678504955124276,-1.10414621800651,
1.17520505546249)) ;
#48245 = CARTESIAN_POINT('Ctrl Pts',(-1.01775743268641,-1.14581288467317,
0.587602527731245)) ;
#48246 = CARTESIAN_POINT('Ctrl Pts',(-1.35700991024855,-1.18747955133984,
2.49278676449569E-16)) ;
#48247 = CARTESIAN_POINT('Ctrl Pts',(-1.01775743268642,-1.22914621800651,
-0.587602527731243)) ;
#48248 = CARTESIAN_POINT('Ctrl Pts',(-0.678504955124277,-1.27081288467317,
-1.17520505546249)) ;
#48249 = CARTESIAN_POINT('Ctrl Pts',(0.,-1.31247955133984,-1.17520505546249)) ;
#48250 = CARTESIAN_POINT('Ctrl Pts',(0.678504955124277,-1.35414621800651,
-1.17520505546249)) ;
#48251 = CARTESIAN_POINT('Ctrl Pts',(1.01775743268642,-1.39581288467317,-0.587602527731244)) ;
#48252 = CARTESIAN_POINT('Ctrl Pts',(1.35700991024855,-1.43747955133984,-8.30928921498564E-17)) ;
#48253 = CARTESIAN_POINT('Ctrl Pts',(1.01775743268642,-1.47914621800651,0.587602527731244)) ;
#48254 = CARTESIAN_POINT('Ctrl Pts',(0.678504955124277,-1.52081288467317,
1.17520505546249)) ;
#48255 = CARTESIAN_POINT('Ctrl Pts',(1.43921110951392E-16,-1.56247955133984,
1.17520505546249)) ;
#48256 = CARTESIAN_POINT('Ctrl Pts',(-0.678504955124276,-1.60414621800651,
1.17520505546249)) ;
#48257 = CARTESIAN_POINT('Ctrl Pts',(-1.01775743268641,-1.64581288467317,
0.587602527731245)) ;
#48258 = CARTESIAN_POINT('Ctrl Pts',(-1.35700991024855,-1.68747955133984,
2.49278676449569E-16)) ;
#48259 = CARTESIAN_POINT('Ctrl Pts',(-1.01775743268642,-1.72914621800651,
-0.587602527731243)) ;
#48260 = CARTESIAN_POINT('Ctrl Pts',(-0.678504955124277,-1.77081288467317,
-1.17520505546249)) ;
#48261 = CARTESIAN_POINT('Ctrl Pts',(0.,-1.81247955133984,-1.17520505546249)) ;
#48262 = CARTESIAN_POINT('Ctrl Pts',(-0.00610134161874418,1.5002727506704,
-1.50002300957017)) ;
#48263 = CARTESIAN_POINT('Ctrl Pts',(0.864009672649723,1.45850881153905,-1.50356218497642)) ;
#48264 = CARTESIAN_POINT('Ctrl Pts',(1.2990687786669,1.41664621800651,-0.750017709059173)) ;
#48265 = CARTESIAN_POINT('Ctrl Pts',(1.7320917048892,1.37497955133984,-1.06060028111112E-16)) ;
#48266 = CARTESIAN_POINT('Ctrl Pts',(1.2990687786669,1.33331288467317,0.750017709059172)) ;
#48267 = CARTESIAN_POINT('Ctrl Pts',(0.8660458524446,1.29164621800651,1.50003541811835)) ;
#48268 = CARTESIAN_POINT('Ctrl Pts',(1.83701357340629E-16,1.24997955133984,
1.50003541811835)) ;
#48269 = CARTESIAN_POINT('Ctrl Pts',(-0.866045852444599,1.20831288467317,
1.50003541811835)) ;
#48270 = CARTESIAN_POINT('Ctrl Pts',(-1.2990687786669,1.16664621800651,0.750017709059173)) ;
#48271 = CARTESIAN_POINT('Ctrl Pts',(-1.7320917048892,1.12497955133984,3.18180084333336E-16)) ;
#48272 = CARTESIAN_POINT('Ctrl Pts',(-1.2990687786669,1.08331288467317,-0.750017709059171)) ;
#48273 = CARTESIAN_POINT('Ctrl Pts',(-0.8660458524446,1.04164621800651,-1.50003541811835)) ;
#48274 = CARTESIAN_POINT('Ctrl Pts',(0.,0.99997955133984,-1.50003541811835)) ;
#48275 = CARTESIAN_POINT('Ctrl Pts',(0.866045852444599,0.958312884673173,
-1.50003541811835)) ;
#48276 = CARTESIAN_POINT('Ctrl Pts',(1.2990687786669,0.916646218006506,-0.750017709059173)) ;
#48277 = CARTESIAN_POINT('Ctrl Pts',(1.7320917048892,0.87497955133984,-1.06060028111112E-16)) ;
#48278 = CARTESIAN_POINT('Ctrl Pts',(1.2990687786669,0.833312884673173,0.750017709059172)) ;
#48279 = CARTESIAN_POINT('Ctrl Pts',(0.8660458524446,0.791646218006506,1.50003541811835)) ;
#48280 = CARTESIAN_POINT('Ctrl Pts',(1.83701357340629E-16,0.749979551339839,
1.50003541811835)) ;
#48281 = CARTESIAN_POINT('Ctrl Pts',(-0.866045852444599,0.708312884673173,
1.50003541811835)) ;
#48282 = CARTESIAN_POINT('Ctrl Pts',(-1.2990687786669,0.666646218006506,0.750017709059173)) ;
#48283 = CARTESIAN_POINT('Ctrl Pts',(-1.7320917048892,0.624979551339839,3.18180084333336E-16)) ;
#48284 = CARTESIAN_POINT('Ctrl Pts',(-1.2990687786669,0.583312884673173,-0.750017709059171)) ;
#48285 = CARTESIAN_POINT('Ctrl Pts',(-0.8660458524446,0.541646218006506,-1.50003541811835)) ;
#48286 = CARTESIAN_POINT('Ctrl Pts',(0.,0.499979551339839,-1.50003541811835)) ;
#48287 = CARTESIAN_POINT('Ctrl Pts',(0.866045852444599,0.458312884673173,
-1.50003541811835)) ;
#48288 = CARTESIAN_POINT('Ctrl Pts',(1.2990687786669,0.416646218006506,-0.750017709059173)) ;
#48289 = CARTESIAN_POINT('Ctrl Pts',(1.7320917048892,0.37497955133984,-1.06060028111112E-16)) ;
#48290 = CARTESIAN_POINT('Ctrl Pts',(1.2990687786669,0.333312884673173,0.750017709059172)) ;
#48291 = CARTESIAN_POINT('Ctrl Pts',(0.8660458524446,0.291646218006506,1.50003541811835)) ;
#48292 = CARTESIAN_POINT('Ctrl Pts',(1.83701357340629E-16,0.249979551339839,
1.50003541811835)) ;
#48293 = CARTESIAN_POINT('Ctrl Pts',(-0.866045852444599,0.208312884673173,
1.50003541811835)) ;
#48294 = CARTESIAN_POINT('Ctrl Pts',(-1.2990687786669,0.166646218006506,0.750017709059173)) ;
#48295 = CARTESIAN_POINT('Ctrl Pts',(-1.7320917048892,0.12497955133984,3.18180084333336E-16)) ;
#48296 = CARTESIAN_POINT('Ctrl Pts',(-1.2990687786669,0.0833128846731729,
-0.750017709059171)) ;
#48297 = CARTESIAN_POINT('Ctrl Pts',(-0.8660458524446,0.0416462180065062,
-1.50003541811835)) ;
#48298 = CARTESIAN_POINT('Ctrl Pts',(0.,-2.0448660160613E-5,-1.50003541811835)) ;
#48299 = CARTESIAN_POINT('Ctrl Pts',(0.866045852444599,-0.0416871153268273,
-1.50003541811835)) ;
#48300 = CARTESIAN_POINT('Ctrl Pts',(1.2990687786669,-0.0833537819934939,
-0.750017709059173)) ;
#48301 = CARTESIAN_POINT('Ctrl Pts',(1.7320917048892,-0.125020448660161,-1.06060028111112E-16)) ;
#48302 = CARTESIAN_POINT('Ctrl Pts',(1.2990687786669,-0.166687115326827,0.750017709059172)) ;
#48303 = CARTESIAN_POINT('Ctrl Pts',(0.8660458524446,-0.208353781993494,1.50003541811835)) ;
#48304 = CARTESIAN_POINT('Ctrl Pts',(1.83701357340629E-16,-0.250020448660161,
1.50003541811835)) ;
#48305 = CARTESIAN_POINT('Ctrl Pts',(-0.866045852444599,-0.291687115326827,
1.50003541811835)) ;
#48306 = CARTESIAN_POINT('Ctrl Pts',(-1.2990687786669,-0.333353781993494,
0.750017709059173)) ;
#48307 = CARTESIAN_POINT('Ctrl Pts',(-1.7320917048892,-0.375020448660161,
3.18180084333336E-16)) ;
#48308 = CARTESIAN_POINT('Ctrl Pts',(-1.2990687786669,-0.416687115326827,
-0.750017709059171)) ;
#48309 = CARTESIAN_POINT('Ctrl Pts',(-0.8660458524446,-0.458353781993494,
-1.50003541811835)) ;
#48310 = CARTESIAN_POINT('Ctrl Pts',(0.,-0.500020448660161,-1.50003541811835)) ;
#48311 = CARTESIAN_POINT('Ctrl Pts',(0.866045852444599,-0.541687115326827,
-1.50003541811835)) ;
#48312 = CARTESIAN_POINT('Ctrl Pts',(1.2990687786669,-0.583353781993494,-0.750017709059173)) ;
#48313 = CARTESIAN_POINT('Ctrl Pts',(1.7320917048892,-0.62502044866016,-1.06060028111112E-16)) ;
#48314 = CARTESIAN_POINT('Ctrl Pts',(1.2990687786669,-0.666687115326827,0.750017709059172)) ;
#48315 = CARTESIAN_POINT('Ctrl Pts',(0.8660458524446,-0.708353781993494,1.50003541811835)) ;
#48316 = CARTESIAN_POINT('Ctrl Pts',(1.83701357340629E-16,-0.75002044866016,
1.50003541811835)) ;
#48317 = CARTESIAN_POINT('Ctrl Pts',(-0.866045852444599,-0.791687115326827,
1.50003541811835)) ;
#48318 = CARTESIAN_POINT('Ctrl Pts',(-1.2990687786669,-0.833353781993494,
0.750017709059173)) ;
#48319 = CARTESIAN_POINT('Ctrl Pts',(-1.7320917048892,-0.87502044866016,3.18180084333336E-16)) ;
#48320 = CARTESIAN_POINT('Ctrl Pts',(-1.2990687786669,-0.916687115326827,
-0.750017709059171)) ;
#48321 = CARTESIAN_POINT('Ctrl Pts',(-0.8660458524446,-0.958353781993494,
-1.50003541811835)) ;
#48322 = CARTESIAN_POINT('Ctrl Pts',(0.,-1.00002044866016,-1.50003541811835)) ;
#48323 = CARTESIAN_POINT('Ctrl Pts',(0.866045852444599,-1.04168711532683,
-1.50003541811835)) ;
#48324 = CARTESIAN_POINT('Ctrl Pts',(1.2990687786669,-1.08335378199349,-0.750017709059173)) ;
#48325 = CARTESIAN_POINT('Ctrl Pts',(1.7320917048892,-1.12502044866016,-1.06060028111112E-16)) ;
#48326 = CARTESIAN_POINT('Ctrl Pts',(1.2990687786669,-1.16668711532683,0.750017709059172)) ;
#48327 = CARTESIAN_POINT('Ctrl Pts',(0.8660458524446,-1.20835378199349,1.50003541811835)) ;
#48328 = CARTESIAN_POINT('Ctrl Pts',(1.83701357340629E-16,-1.25002044866016,
1.50003541811835)) ;
#48329 = CARTESIAN_POINT('Ctrl Pts',(-0.866045852444599,-1.29168711532683,
1.50003541811835)) ;
#48330 = CARTESIAN_POINT('Ctrl Pts',(-1.2990687786669,-1.33335378199349,0.750017709059173)) ;
#48331 = CARTESIAN_POINT('Ctrl Pts',(-1.7320917048892,-1.37502044866016,3.18180084333336E-16)) ;
#48332 = CARTESIAN_POINT('Ctrl Pts',(-1.2990687786669,-1.41668711532683,-0.750017709059171)) ;
#48333 = CARTESIAN_POINT('Ctrl Pts',(-0.8660458524446,-1.45835378199349,-1.50003541811835)) ;
#48334 = CARTESIAN_POINT('Ctrl Pts',(0.,-1.50002044866016,-1.50003541811835)) ;
#48335 = CARTESIAN_POINT('Ctrl Pts',(0.866045852444599,-1.54168711532683,
-1.50003541811835)) ;
#48336 = CARTESIAN_POINT('Ctrl Pts',(1.2990687786669,-1.58335378199349,-0.750017709059173)) ;
#48337 = CARTESIAN_POINT('Ctrl Pts',(1.7320917048892,-1.62502044866016,-1.06060028111112E-16)) ;
#48338 = CARTESIAN_POINT('Ctrl Pts',(1.2990687786669,-1.66668711532683,0.750017709059172)) ;
#48339 = CARTESIAN_POINT('Ctrl Pts',(0.8660458524446,-1.70835378199349,1.50003541811835)) ;
#48340 = CARTESIAN_POINT('Ctrl Pts',(1.83701357340629E-16,-1.75002044866016,
1.50003541811835)) ;
#48341 = CARTESIAN_POINT('Ctrl Pts',(-0.866045852444599,-1.79168711532683,
1.50003541811835)) ;
#48342 = CARTESIAN_POINT('Ctrl Pts',(-1.2990687786669,-1.83335378199349,0.750017709059173)) ;
#48343 = CARTESIAN_POINT('Ctrl Pts',(-1.7320917048892,-1.87502044866016,3.18180084333336E-16)) ;
#48344 = CARTESIAN_POINT('Ctrl Pts',(-1.2990687786669,-1.91668711532683,-0.750017709059171)) ;
#48345 = CARTESIAN_POINT('Ctrl Pts',(-0.8660458524446,-1.95835378199349,-1.50003541811835)) ;
#48346 = CARTESIAN_POINT('Ctrl Pts',(0.,-2.00002044866016,-1.50003541811835)) ;
#48347 = CARTESIAN_POINT('Ctrl Pts',(0.,1.93751828185976,-1.50003166510997)) ;
#48348 = CARTESIAN_POINT('Ctrl Pts',(0.866043685644202,1.89585161519309,-1.50003166510997)) ;
#48349 = CARTESIAN_POINT('Ctrl Pts',(1.2990655284663,1.85418494852643,-0.750015832554983)) ;
#48350 = CARTESIAN_POINT('Ctrl Pts',(1.73208737128841,1.81251828185976,-1.06059762754595E-16)) ;
#48351 = CARTESIAN_POINT('Ctrl Pts',(1.2990655284663,1.77085161519309,0.750015832554983)) ;
#48352 = CARTESIAN_POINT('Ctrl Pts',(0.866043685644202,1.72918494852643,1.50003166510997)) ;
#48353 = CARTESIAN_POINT('Ctrl Pts',(1.83700897729659E-16,1.68751828185976,
1.50003166510997)) ;
#48354 = CARTESIAN_POINT('Ctrl Pts',(-0.866043685644201,1.64585161519309,
1.50003166510997)) ;
#48355 = CARTESIAN_POINT('Ctrl Pts',(-1.2990655284663,1.60418494852643,0.750015832554984)) ;
#48356 = CARTESIAN_POINT('Ctrl Pts',(-1.73208737128841,1.56251828185976,3.18179288263784E-16)) ;
#48357 = CARTESIAN_POINT('Ctrl Pts',(-1.2990655284663,1.52085161519309,-0.750015832554982)) ;
#48358 = CARTESIAN_POINT('Ctrl Pts',(-0.866043685644203,1.47918494852643,
-1.50003166510997)) ;
#48359 = CARTESIAN_POINT('Ctrl Pts',(0.,1.43751828185976,-1.50003166510997)) ;
#48360 = CARTESIAN_POINT('Ctrl Pts',(0.866043685644202,1.39585161519309,-1.50003166510997)) ;
#48361 = CARTESIAN_POINT('Ctrl Pts',(1.2990655284663,1.35418494852643,-0.750015832554983)) ;
#48362 = CARTESIAN_POINT('Ctrl Pts',(1.73208737128841,1.31251828185976,-1.06059762754595E-16)) ;
#48363 = CARTESIAN_POINT('Ctrl Pts',(1.2990655284663,1.27085161519309,0.750015832554983)) ;
#48364 = CARTESIAN_POINT('Ctrl Pts',(0.866043685644202,1.22918494852643,1.50003166510997)) ;
#48365 = CARTESIAN_POINT('Ctrl Pts',(1.83700897729659E-16,1.18751828185976,
1.50003166510997)) ;
#48366 = CARTESIAN_POINT('Ctrl Pts',(-0.866043685644201,1.14585161519309,
1.50003166510997)) ;
#48367 = CARTESIAN_POINT('Ctrl Pts',(-1.2990655284663,1.10418494852643,0.750015832554984)) ;
#48368 = CARTESIAN_POINT('Ctrl Pts',(-1.73208737128841,1.06251828185976,3.18179288263784E-16)) ;
#48369 = CARTESIAN_POINT('Ctrl Pts',(-1.2990655284663,1.02085161519309,-0.750015832554982)) ;
#48370 = CARTESIAN_POINT('Ctrl Pts',(-0.866043685644203,0.97918494852643,
-1.50003166510997)) ;
#48371 = CARTESIAN_POINT('Ctrl Pts',(0.,0.937518281859764,-1.50003166510997)) ;
#48372 = CARTESIAN_POINT('Ctrl Pts',(0.866043685644202,0.895851615193097,
-1.50003166510997)) ;
#48373 = CARTESIAN_POINT('Ctrl Pts',(1.2990655284663,0.85418494852643,-0.750015832554983)) ;
#48374 = CARTESIAN_POINT('Ctrl Pts',(1.73208737128841,0.812518281859764,-1.06059762754595E-16)) ;
#48375 = CARTESIAN_POINT('Ctrl Pts',(1.2990655284663,0.770851615193097,0.750015832554983)) ;
#48376 = CARTESIAN_POINT('Ctrl Pts',(0.866043685644202,0.72918494852643,1.50003166510997)) ;
#48377 = CARTESIAN_POINT('Ctrl Pts',(1.83700897729659E-16,0.687518281859763,
1.50003166510997)) ;
#48378 = CARTESIAN_POINT('Ctrl Pts',(-0.866043685644201,0.645851615193097,
1.50003166510997)) ;
#48379 = CARTESIAN_POINT('Ctrl Pts',(-1.2990655284663,0.60418494852643,0.750015832554984)) ;
#48380 = CARTESIAN_POINT('Ctrl Pts',(-1.73208737128841,0.562518281859763,
3.18179288263784E-16)) ;
#48381 = CARTESIAN_POINT('Ctrl Pts',(-1.2990655284663,0.520851615193097,-0.750015832554982)) ;
#48382 = CARTESIAN_POINT('Ctrl Pts',(-0.866043685644203,0.47918494852643,
-1.50003166510997)) ;
#48383 = CARTESIAN_POINT('Ctrl Pts',(0.,0.437518281859763,-1.50003166510997)) ;
#48384 = CARTESIAN_POINT('Ctrl Pts',(0.866043685644202,0.395851615193097,
-1.50003166510997)) ;
#48385 = CARTESIAN_POINT('Ctrl Pts',(1.2990655284663,0.35418494852643,-0.750015832554983)) ;
#48386 = CARTESIAN_POINT('Ctrl Pts',(1.73208737128841,0.312518281859763,-1.06059762754595E-16)) ;
#48387 = CARTESIAN_POINT('Ctrl Pts',(1.2990655284663,0.270851615193097,0.750015832554983)) ;
#48388 = CARTESIAN_POINT('Ctrl Pts',(0.866043685644202,0.22918494852643,1.50003166510997)) ;
#48389 = CARTESIAN_POINT('Ctrl Pts',(1.83700897729659E-16,0.187518281859763,
1.50003166510997)) ;
#48390 = CARTESIAN_POINT('Ctrl Pts',(-0.866043685644201,0.145851615193097,
1.50003166510997)) ;
#48391 = CARTESIAN_POINT('Ctrl Pts',(-1.2990655284663,0.10418494852643,0.750015832554984)) ;
#48392 = CARTESIAN_POINT('Ctrl Pts',(-1.73208737128841,0.0625182818597633,
3.18179288263784E-16)) ;
#48393 = CARTESIAN_POINT('Ctrl Pts',(-1.2990655284663,0.0208516151930967,
-0.750015832554982)) ;
#48394 = CARTESIAN_POINT('Ctrl Pts',(-0.866043685644203,-0.02081505147357,
-1.50003166510997)) ;
#48395 = CARTESIAN_POINT('Ctrl Pts',(0.,-0.0624817181402368,-1.50003166510997)) ;
#48396 = CARTESIAN_POINT('Ctrl Pts',(0.866043685644202,-0.104148384806903,
-1.50003166510997)) ;
#48397 = CARTESIAN_POINT('Ctrl Pts',(1.2990655284663,-0.14581505147357,-0.750015832554983)) ;
#48398 = CARTESIAN_POINT('Ctrl Pts',(1.73208737128841,-0.187481718140236,
-1.06059762754595E-16)) ;
#48399 = CARTESIAN_POINT('Ctrl Pts',(1.2990655284663,-0.229148384806903,0.750015832554983)) ;
#48400 = CARTESIAN_POINT('Ctrl Pts',(0.866043685644202,-0.27081505147357,
1.50003166510997)) ;
#48401 = CARTESIAN_POINT('Ctrl Pts',(1.83700897729659E-16,-0.312481718140236,
1.50003166510997)) ;
#48402 = CARTESIAN_POINT('Ctrl Pts',(-0.866043685644201,-0.354148384806903,
1.50003166510997)) ;
#48403 = CARTESIAN_POINT('Ctrl Pts',(-1.2990655284663,-0.39581505147357,0.750015832554984)) ;
#48404 = CARTESIAN_POINT('Ctrl Pts',(-1.73208737128841,-0.437481718140237,
3.18179288263784E-16)) ;
#48405 = CARTESIAN_POINT('Ctrl Pts',(-1.2990655284663,-0.479148384806903,
-0.750015832554982)) ;
#48406 = CARTESIAN_POINT('Ctrl Pts',(-0.866043685644203,-0.52081505147357,
-1.50003166510997)) ;
#48407 = CARTESIAN_POINT('Ctrl Pts',(0.,-0.562481718140237,-1.50003166510997)) ;
#48408 = CARTESIAN_POINT('Ctrl Pts',(0.866043685644202,-0.604148384806903,
-1.50003166510997)) ;
#48409 = CARTESIAN_POINT('Ctrl Pts',(1.2990655284663,-0.64581505147357,-0.750015832554983)) ;
#48410 = CARTESIAN_POINT('Ctrl Pts',(1.73208737128841,-0.687481718140236,
-1.06059762754595E-16)) ;
#48411 = CARTESIAN_POINT('Ctrl Pts',(1.2990655284663,-0.729148384806903,0.750015832554983)) ;
#48412 = CARTESIAN_POINT('Ctrl Pts',(0.866043685644202,-0.77081505147357,
1.50003166510997)) ;
#48413 = CARTESIAN_POINT('Ctrl Pts',(1.83700897729659E-16,-0.812481718140236,
1.50003166510997)) ;
#48414 = CARTESIAN_POINT('Ctrl Pts',(-0.866043685644201,-0.854148384806903,
1.50003166510997)) ;
#48415 = CARTESIAN_POINT('Ctrl Pts',(-1.2990655284663,-0.89581505147357,0.750015832554984)) ;
#48416 = CARTESIAN_POINT('Ctrl Pts',(-1.73208737128841,-0.937481718140237,
3.18179288263784E-16)) ;
#48417 = CARTESIAN_POINT('Ctrl Pts',(-1.2990655284663,-0.979148384806903,
-0.750015832554982)) ;
#48418 = CARTESIAN_POINT('Ctrl Pts',(-0.866043685644203,-1.02081505147357,
-1.50003166510997)) ;
#48419 = CARTESIAN_POINT('Ctrl Pts',(0.,-1.06248171814024,-1.50003166510997)) ;
#48420 = CARTESIAN_POINT('Ctrl Pts',(0.866043685644202,-1.10414838480691,
-1.50003166510997)) ;
#48421 = CARTESIAN_POINT('Ctrl Pts',(1.2990655284663,-1.14581505147357,-0.750015832554983)) ;
#48422 = CARTESIAN_POINT('Ctrl Pts',(1.73208737128841,-1.18748171814024,-1.06059762754595E-16)) ;
#48423 = CARTESIAN_POINT('Ctrl Pts',(1.2990655284663,-1.22914838480691,0.750015832554983)) ;
#48424 = CARTESIAN_POINT('Ctrl Pts',(0.866043685644202,-1.27081505147357,
1.50003166510997)) ;
#48425 = CARTESIAN_POINT('Ctrl Pts',(1.83700897729659E-16,-1.31248171814024,
1.50003166510997)) ;
#48426 = CARTESIAN_POINT('Ctrl Pts',(-0.866043685644201,-1.35414838480691,
1.50003166510997)) ;
#48427 = CARTESIAN_POINT('Ctrl Pts',(-1.2990655284663,-1.39581505147357,0.750015832554984)) ;
#48428 = CARTESIAN_POINT('Ctrl Pts',(-1.73208737128841,-1.43748171814024,
3.18179288263784E-16)) ;
#48429 = CARTESIAN_POINT('Ctrl Pts',(-1.2990655284663,-1.47914838480691,-0.750015832554982)) ;
#48430 = CARTESIAN_POINT('Ctrl Pts',(-0.866043685644203,-1.52081505147357,
-1.50003166510997)) ;
#48431 = CARTESIAN_POINT('Ctrl Pts',(0.,-1.56248171814024,-1.50003166510997)) ;
#48432 = CARTESIAN_POINT('Ctrl Pts',(0.,1.75,-1.17524047358083)) ;
#48433 = CARTESIAN_POINT('Ctrl Pts',(0.678525403784437,1.70833333333333,-1.17524047358083)) ;
#48434 = CARTESIAN_POINT('Ctrl Pts',(1.01778810567666,1.66666666666667,-0.587620236790417)) ;
#48435 = CARTESIAN_POINT('Ctrl Pts',(1.35705080756887,1.625,-8.30953963884777E-17)) ;
#48436 = CARTESIAN_POINT('Ctrl Pts',(1.01778810567666,1.58333333333333,0.587620236790416)) ;
#48437 = CARTESIAN_POINT('Ctrl Pts',(0.678525403784438,1.54166666666667,1.17524047358083)) ;
#48438 = CARTESIAN_POINT('Ctrl Pts',(1.43925448419919E-16,1.5,1.17524047358083)) ;
#48439 = CARTESIAN_POINT('Ctrl Pts',(-0.678525403784437,1.45833333333333,
1.17524047358083)) ;
#48440 = CARTESIAN_POINT('Ctrl Pts',(-1.01778810567666,1.41666666666667,0.587620236790417)) ;
#48441 = CARTESIAN_POINT('Ctrl Pts',(-1.35705080756887,1.375,2.49286189165433E-16)) ;
#48442 = CARTESIAN_POINT('Ctrl Pts',(-1.01778810567666,1.33333333333333,-0.587620236790416)) ;
#48443 = CARTESIAN_POINT('Ctrl Pts',(-0.678525403784438,1.29166666666667,
-1.17524047358083)) ;
#48444 = CARTESIAN_POINT('Ctrl Pts',(0.,1.25,-1.17524047358083)) ;
#48445 = CARTESIAN_POINT('Ctrl Pts',(0.678525403784437,1.20833333333333,-1.17524047358083)) ;
#48446 = CARTESIAN_POINT('Ctrl Pts',(1.01778810567666,1.16666666666667,-0.587620236790417)) ;
#48447 = CARTESIAN_POINT('Ctrl Pts',(1.35705080756887,1.125,-8.30953963884777E-17)) ;
#48448 = CARTESIAN_POINT('Ctrl Pts',(1.01778810567666,1.08333333333333,0.587620236790416)) ;
#48449 = CARTESIAN_POINT('Ctrl Pts',(0.678525403784438,1.04166666666667,1.17524047358083)) ;
#48450 = CARTESIAN_POINT('Ctrl Pts',(1.43925448419919E-16,1.,1.17524047358083)) ;
#48451 = CARTESIAN_POINT('Ctrl Pts',(-0.678525403784437,0.958333333333334,
1.17524047358083)) ;
#48452 = CARTESIAN_POINT('Ctrl Pts',(-1.01778810567666,0.916666666666667,
0.587620236790417)) ;
#48453 = CARTESIAN_POINT('Ctrl Pts',(-1.35705080756887,0.875,2.49286189165433E-16)) ;
#48454 = CARTESIAN_POINT('Ctrl Pts',(-1.01778810567666,0.833333333333334,
-0.587620236790416)) ;
#48455 = CARTESIAN_POINT('Ctrl Pts',(-0.678525403784438,0.791666666666667,
-1.17524047358083)) ;
#48456 = CARTESIAN_POINT('Ctrl Pts',(0.,0.75,-1.17524047358083)) ;
#48457 = CARTESIAN_POINT('Ctrl Pts',(0.678525403784437,0.708333333333334,
-1.17524047358083)) ;
#48458 = CARTESIAN_POINT('Ctrl Pts',(1.01778810567666,0.666666666666667,-0.587620236790417)) ;
#48459 = CARTESIAN_POINT('Ctrl Pts',(1.35705080756887,0.625,-8.30953963884777E-17)) ;
#48460 = CARTESIAN_POINT('Ctrl Pts',(1.01778810567666,0.583333333333334,0.587620236790416)) ;
#48461 = CARTESIAN_POINT('Ctrl Pts',(0.678525403784438,0.541666666666667,
1.17524047358083)) ;
#48462 = CARTESIAN_POINT('Ctrl Pts',(1.43925448419919E-16,0.5,1.17524047358083)) ;
#48463 = CARTESIAN_POINT('Ctrl Pts',(-0.678525403784437,0.458333333333334,
1.17524047358083)) ;
#48464 = CARTESIAN_POINT('Ctrl Pts',(-1.01778810567666,0.416666666666667,
0.587620236790417)) ;
#48465 = CARTESIAN_POINT('Ctrl Pts',(-1.35705080756887,0.375,2.49286189165433E-16)) ;
#48466 = CARTESIAN_POINT('Ctrl Pts',(-1.01778810567666,0.333333333333334,
-0.587620236790416)) ;
#48467 = CARTESIAN_POINT('Ctrl Pts',(-0.678525403784438,0.291666666666667,
-1.17524047358083)) ;
#48468 = CARTESIAN_POINT('Ctrl Pts',(0.,0.25,-1.17524047358083)) ;
#48469 = CARTESIAN_POINT('Ctrl Pts',(0.678525403784437,0.208333333333334,
-1.17524047358083)) ;
#48470 = CARTESIAN_POINT('Ctrl Pts',(1.01778810567666,0.166666666666667,-0.587620236790417)) ;
#48471 = CARTESIAN_POINT('Ctrl Pts',(1.35705080756887,0.125,-8.30953963884777E-17)) ;
#48472 = CARTESIAN_POINT('Ctrl Pts',(1.01778810567666,0.0833333333333337,
0.587620236790416)) ;
#48473 = CARTESIAN_POINT('Ctrl Pts',(0.678525403784438,0.0416666666666671,
1.17524047358083)) ;
#48474 = CARTESIAN_POINT('Ctrl Pts',(1.43925448419919E-16,2.16840434497101E-16,
1.17524047358083)) ;
#48475 = CARTESIAN_POINT('Ctrl Pts',(-0.678525403784437,-0.0416666666666664,
1.17524047358083)) ;
#48476 = CARTESIAN_POINT('Ctrl Pts',(-1.01778810567666,-0.0833333333333331,
0.587620236790417)) ;
#48477 = CARTESIAN_POINT('Ctrl Pts',(-1.35705080756887,-0.125,2.49286189165433E-16)) ;
#48478 = CARTESIAN_POINT('Ctrl Pts',(-1.01778810567666,-0.166666666666666,
-0.587620236790416)) ;
#48479 = CARTESIAN_POINT('Ctrl Pts',(-0.678525403784438,-0.208333333333333,
-1.17524047358083)) ;
#48480 = CARTESIAN_POINT('Ctrl Pts',(0.,-0.25,-1.17524047358083)) ;
#48481 = CARTESIAN_POINT('Ctrl Pts',(0.678525403784437,-0.291666666666666,
-1.17524047358083)) ;
#48482 = CARTESIAN_POINT('Ctrl Pts',(1.01778810567666,-0.333333333333333,
-0.587620236790417)) ;
#48483 = CARTESIAN_POINT('Ctrl Pts',(1.35705080756887,-0.374999999999999,
-8.30953963884777E-17)) ;
#48484 = CARTESIAN_POINT('Ctrl Pts',(1.01778810567666,-0.416666666666666,
0.587620236790416)) ;
#48485 = CARTESIAN_POINT('Ctrl Pts',(0.678525403784438,-0.458333333333333,
1.17524047358083)) ;
#48486 = CARTESIAN_POINT('Ctrl Pts',(1.43925448419919E-16,-0.5,1.17524047358083)) ;
#48487 = CARTESIAN_POINT('Ctrl Pts',(-0.678525403784437,-0.541666666666666,
1.17524047358083)) ;
#48488 = CARTESIAN_POINT('Ctrl Pts',(-1.01778810567666,-0.583333333333333,
0.587620236790417)) ;
#48489 = CARTESIAN_POINT('Ctrl Pts',(-1.35705080756887,-0.625,2.49286189165433E-16)) ;
#48490 = CARTESIAN_POINT('Ctrl Pts',(-1.01778810567666,-0.666666666666667,
-0.587620236790416)) ;
#48491 = CARTESIAN_POINT('Ctrl Pts',(-0.678525403784438,-0.708333333333333,
-1.17524047358083)) ;
#48492 = CARTESIAN_POINT('Ctrl Pts',(0.,-0.75,-1.17524047358083)) ;
#48493 = CARTESIAN_POINT('Ctrl Pts',(0.678525403784437,-0.791666666666666,
-1.17524047358083)) ;
#48494 = CARTESIAN_POINT('Ctrl Pts',(1.01778810567666,-0.833333333333333,
-0.587620236790417)) ;
#48495 = CARTESIAN_POINT('Ctrl Pts',(1.35705080756887,-0.875,-8.30953963884777E-17)) ;
#48496 = CARTESIAN_POINT('Ctrl Pts',(1.01778810567666,-0.916666666666666,
0.587620236790416)) ;
#48497 = CARTESIAN_POINT('Ctrl Pts',(0.678525403784438,-0.958333333333333,
1.17524047358083)) ;
#48498 = CARTESIAN_POINT('Ctrl Pts',(1.43925448419919E-16,-1.,1.17524047358083)) ;
#48499 = CARTESIAN_POINT('Ctrl Pts',(-0.678525403784437,-1.04166666666667,
1.17524047358083)) ;
#48500 = CARTESIAN_POINT('Ctrl Pts',(-1.01778810567666,-1.08333333333333,
0.587620236790417)) ;
#48501 = CARTESIAN_POINT('Ctrl Pts',(-1.35705080756887,-1.125,2.49286189165433E-16)) ;
#48502 = CARTESIAN_POINT('Ctrl Pts',(-1.01778810567666,-1.16666666666667,
-0.587620236790416)) ;
#48503 = CARTESIAN_POINT('Ctrl Pts',(-0.678525403784438,-1.20833333333333,
-1.17524047358083)) ;
#48504 = CARTESIAN_POINT('Ctrl Pts',(0.,-1.25,-1.17524047358083)) ;
#48505 = CARTESIAN_POINT('Ctrl Pts',(0.678525403784437,-1.29166666666667,
-1.17524047358083)) ;
#48506 = CARTESIAN_POINT('Ctrl Pts',(1.01778810567666,-1.33333333333333,-0.587620236790417)) ;
#48507 = CARTESIAN_POINT('Ctrl Pts',(1.35705080756887,-1.375,-8.30953963884777E-17)) ;
#48508 = CARTESIAN_POINT('Ctrl Pts',(1.01778810567666,-1.41666666666667,0.587620236790416)) ;
#48509 = CARTESIAN_POINT('Ctrl Pts',(0.678525403784438,-1.45833333333333,
1.17524047358083)) ;
#48510 = CARTESIAN_POINT('Ctrl Pts',(1.43925448419919E-16,-1.5,1.17524047358083)) ;
#48511 = CARTESIAN_POINT('Ctrl Pts',(-0.678525403784437,-1.54166666666667,
1.17524047358083)) ;
#48512 = CARTESIAN_POINT('Ctrl Pts',(-1.01778810567666,-1.58333333333333,
0.587620236790417)) ;
#48513 = CARTESIAN_POINT('Ctrl Pts',(-1.35705080756887,-1.625,2.49286189165433E-16)) ;
#48514 = CARTESIAN_POINT('Ctrl Pts',(-1.01778810567666,-1.66666666666667,
-0.587620236790416)) ;
#48515 = CARTESIAN_POINT('Ctrl Pts',(-0.678525403784438,-1.70833333333333,
-1.17524047358083)) ;
#48516 = CARTESIAN_POINT('Ctrl Pts',(0.,-1.75,-1.17524047358083)) ;
#48517 = CARTESIAN_POINT('Origin',(-2.75,1.5,-1.58771324027147)) ;
#48518 = CARTESIAN_POINT('',(2.75,1.5,0.)) ;
#48519 = CARTESIAN_POINT('Origin',(0.,1.5,0.)) ;
#48520 = CARTESIAN_POINT('',(1.375,1.5,-2.38156986040721)) ;
#48521 = CARTESIAN_POINT('Origin',(0.,1.5,0.)) ;
#48522 = CARTESIAN_POINT('',(-1.375,1.5,-2.38156986040721)) ;
#48523 = CARTESIAN_POINT('Origin',(0.,1.5,0.)) ;
#48524 = CARTESIAN_POINT('',(-2.75,1.5,3.7557864968429E-16)) ;
#48525 = CARTESIAN_POINT('Origin',(0.,1.5,0.)) ;
#48526 = CARTESIAN_POINT('Origin',(0.,1.5,0.)) ;
#48527 = CARTESIAN_POINT('Origin',(9.59795089256626E-16,1.5,-3.17542648054295)) ;
#48528 = CARTESIAN_POINT('',(7.2557076685516E-16,1.25437990693814,-3.17542648054295)) ;
#48529 = CARTESIAN_POINT('',(9.59795089256626E-16,-1.25437990693814,-3.17542648054295)) ;
#48530 = CARTESIAN_POINT('',(9.59795089256626E-16,1.5,-3.17542648054295)) ;
#48531 = CARTESIAN_POINT('',(-1.375,-1.5,-2.38156986040721)) ;
#48532 = CARTESIAN_POINT('Ctrl Pts',(5.29535621962484E-11,-1.25437990692049,
-3.17542648057352)) ;
#48533 = CARTESIAN_POINT('Ctrl Pts',(-0.736860279164304,-1.5,-2.75000000001229)) ;
#48534 = CARTESIAN_POINT('Ctrl Pts',(-1.375,-1.5,-2.38156986040721)) ;
#48535 = CARTESIAN_POINT('',(-2.75,-1.25437990693838,-1.58771324027183)) ;
#48536 = CARTESIAN_POINT('Ctrl Pts',(-1.375,-1.5,-2.38156986040721)) ;
#48537 = CARTESIAN_POINT('Ctrl Pts',(-2.01313972081282,-1.5,-2.01313972081534)) ;
#48538 = CARTESIAN_POINT('Ctrl Pts',(-2.74999999999603,-1.25437990693946,
-1.58771324027377)) ;
#48539 = CARTESIAN_POINT('',(-2.75,1.25437990693835,-1.5877132402718)) ;
#48540 = CARTESIAN_POINT('',(-2.75,1.5,-1.58771324027147)) ;
#48541 = CARTESIAN_POINT('Ctrl Pts',(-1.37500000000001,1.5,-2.38156986040721)) ;
#48542 = CARTESIAN_POINT('Ctrl Pts',(-2.01313972083563,1.5,-2.01313972080217)) ;
#48543 = CARTESIAN_POINT('Ctrl Pts',(-2.75000000005277,1.25437990692055,-1.58771324024101)) ;
#48544 = CARTESIAN_POINT('Ctrl Pts',(-3.77979605086846E-12,1.2543799069394,
-3.17542648054076)) ;
#48545 = CARTESIAN_POINT('Ctrl Pts',(-0.736860279187109,1.5,-2.74999999999913)) ;
#48546 = CARTESIAN_POINT('Ctrl Pts',(-1.37500000000001,1.5,-2.38156986040721)) ;
#48547 = CARTESIAN_POINT('Origin',(-2.75,1.5,-1.58771324027147)) ;
#48548 = CARTESIAN_POINT('',(-2.75,-1.5,3.7557864968429E-16)) ;
#48549 = CARTESIAN_POINT('Ctrl Pts',(-2.75,-1.25437990692041,-1.58771324033287)) ;
#48550 = CARTESIAN_POINT('Ctrl Pts',(-2.75,-1.5,-0.736860279210268)) ;
#48551 = CARTESIAN_POINT('Ctrl Pts',(-2.75,-1.5,-4.52014535047054E-15)) ;
#48552 = CARTESIAN_POINT('',(-2.75,-1.25437990693814,1.58771324027147)) ;
#48553 = CARTESIAN_POINT('Ctrl Pts',(-2.75,-1.5,-4.52014535047054E-15)) ;
#48554 = CARTESIAN_POINT('Ctrl Pts',(-2.75,-1.5,0.73686027918383)) ;
#48555 = CARTESIAN_POINT('Ctrl Pts',(-2.75,-1.2543799069394,1.5877132402671)) ;
#48556 = CARTESIAN_POINT('',(-2.75,1.25437990693814,1.58771324027147)) ;
#48557 = CARTESIAN_POINT('',(-2.75,1.5,1.58771324027147)) ;
#48558 = CARTESIAN_POINT('Ctrl Pts',(-2.75,1.5,5.10972952661887E-15)) ;
#48559 = CARTESIAN_POINT('Ctrl Pts',(-2.75,1.5,0.736860279210163)) ;
#48560 = CARTESIAN_POINT('Ctrl Pts',(-2.75,1.25437990692049,1.58771324033261)) ;
#48561 = CARTESIAN_POINT('Ctrl Pts',(-2.75,1.25437990693933,-1.58771324026735)) ;
#48562 = CARTESIAN_POINT('Ctrl Pts',(-2.75,1.5,-0.73686027918393)) ;
#48563 = CARTESIAN_POINT('Ctrl Pts',(-2.75,1.5,5.10972952661887E-15)) ;
#48564 = CARTESIAN_POINT('Origin',(-2.75,1.5,1.58771324027147)) ;
#48565 = CARTESIAN_POINT('Ctrl Pts',(-2.75000000005296,-1.25437990692049,
1.58771324024089)) ;
#48566 = CARTESIAN_POINT('Ctrl Pts',(-2.0131397208357,-1.5,2.01313972080212)) ;
#48567 = CARTESIAN_POINT('Ctrl Pts',(-1.375,-1.5,2.3815698604072)) ;
#48568 = CARTESIAN_POINT('',(-1.61031639274793E-15,1.5,3.17542648054294)) ;
#48569 = CARTESIAN_POINT('Ctrl Pts',(-2.74999999999622,1.2543799069394,1.58771324027365)) ;
#48570 = CARTESIAN_POINT('Ctrl Pts',(-2.01313972081289,1.5,2.01313972081529)) ;
#48571 = CARTESIAN_POINT('Ctrl Pts',(-1.375,1.5,2.38156986040721)) ;
#48572 = CARTESIAN_POINT('Origin',(-1.61031639274793E-15,1.5,3.17542648054294)) ;
#48573 = CARTESIAN_POINT('',(2.75,-1.25437990693814,1.58771324027147)) ;
#48574 = CARTESIAN_POINT('Ctrl Pts',(1.375,-1.5,2.3815698604072)) ;
#48575 = CARTESIAN_POINT('Ctrl Pts',(2.01313972081289,-1.5,2.01313972081528)) ;
#48576 = CARTESIAN_POINT('Ctrl Pts',(2.74999999999622,-1.2543799069394,1.58771324027365)) ;
#48577 = CARTESIAN_POINT('',(2.75,1.25437990693814,1.58771324027147)) ;
#48578 = CARTESIAN_POINT('',(2.75,1.5,1.58771324027147)) ;
#48579 = CARTESIAN_POINT('Ctrl Pts',(1.375,1.5,2.3815698604072)) ;
#48580 = CARTESIAN_POINT('Ctrl Pts',(2.0131397208357,1.5,2.01313972080212)) ;
#48581 = CARTESIAN_POINT('Ctrl Pts',(2.75000000005295,1.25437990692049,1.58771324024089)) ;
#48582 = CARTESIAN_POINT('Origin',(2.75,1.5,1.58771324027147)) ;
#48583 = CARTESIAN_POINT('',(2.75,-1.5,0.)) ;
#48584 = CARTESIAN_POINT('Ctrl Pts',(2.75,-1.25437990692049,1.58771324033261)) ;
#48585 = CARTESIAN_POINT('Ctrl Pts',(2.75,-1.5,0.73686027921016)) ;
#48586 = CARTESIAN_POINT('Ctrl Pts',(2.75,-1.5,7.86112234864441E-16)) ;
#48587 = CARTESIAN_POINT('',(2.75,-1.25437990693814,-1.58771324027148)) ;
#48588 = CARTESIAN_POINT('Ctrl Pts',(2.75,-1.5,7.86112234864441E-16)) ;
#48589 = CARTESIAN_POINT('Ctrl Pts',(2.75,-1.5,-0.736860279183837)) ;
#48590 = CARTESIAN_POINT('Ctrl Pts',(2.75,-1.2543799069394,-1.58771324026712)) ;
#48591 = CARTESIAN_POINT('',(2.75,1.25437990693814,-1.58771324027148)) ;
#48592 = CARTESIAN_POINT('',(2.75,1.5,-1.58771324027148)) ;
#48593 = CARTESIAN_POINT('Ctrl Pts',(2.75,1.5,2.35833670459332E-15)) ;
#48594 = CARTESIAN_POINT('Ctrl Pts',(2.75,1.5,-0.736860279210164)) ;
#48595 = CARTESIAN_POINT('Ctrl Pts',(2.75,1.25437990692049,-1.58771324033262)) ;
#48596 = CARTESIAN_POINT('Ctrl Pts',(2.75,1.2543799069394,1.58771324026711)) ;
#48597 = CARTESIAN_POINT('Ctrl Pts',(2.75,1.5,0.736860279183835)) ;
#48598 = CARTESIAN_POINT('Ctrl Pts',(2.75,1.5,2.35833670459332E-15)) ;
#48599 = CARTESIAN_POINT('Origin',(2.75,1.5,-1.58771324027148)) ;
#48600 = CARTESIAN_POINT('',(1.375,-1.5,-2.38156986040721)) ;
#48601 = CARTESIAN_POINT('Ctrl Pts',(2.75000000005296,-1.25437990692049,-1.5877132402409)) ;
#48602 = CARTESIAN_POINT('Ctrl Pts',(2.0131397208357,-1.5,-2.01313972080213)) ;
#48603 = CARTESIAN_POINT('Ctrl Pts',(1.375,-1.5,-2.38156986040721)) ;
#48604 = CARTESIAN_POINT('Ctrl Pts',(1.375,-1.5,-2.38156986040721)) ;
#48605 = CARTESIAN_POINT('Ctrl Pts',(0.736860279187108,-1.5,-2.74999999999913)) ;
#48606 = CARTESIAN_POINT('Ctrl Pts',(3.78043123953934E-12,-1.2543799069394,
-3.17542648054077)) ;
#48607 = CARTESIAN_POINT('Ctrl Pts',(1.375,1.5,-2.38156986040721)) ;
#48608 = CARTESIAN_POINT('Ctrl Pts',(0.736860279164306,1.5,-2.75000000001229)) ;
#48609 = CARTESIAN_POINT('Ctrl Pts',(-5.29512331711219E-11,1.25437990692049,
-3.17542648057352)) ;
#48610 = CARTESIAN_POINT('Ctrl Pts',(2.74999999999623,1.2543799069394,-1.58771324027366)) ;
#48611 = CARTESIAN_POINT('Ctrl Pts',(2.0131397208129,1.5,-2.01313972081529)) ;
#48612 = CARTESIAN_POINT('Ctrl Pts',(1.375,1.5,-2.38156986040721)) ;
#48613 = CARTESIAN_POINT('Origin',(-2.75,-1.5,-1.58771324027147)) ;
#48614 = CARTESIAN_POINT('Origin',(0.,-1.5,0.)) ;
#48615 = CARTESIAN_POINT('Origin',(0.,-1.5,0.)) ;
#48616 = CARTESIAN_POINT('Origin',(0.,-1.5,0.)) ;
#48617 = CARTESIAN_POINT('Origin',(0.,-1.5,0.)) ;
#48618 = CARTESIAN_POINT('Origin',(0.,-1.5,0.)) ;
#48619 = CARTESIAN_POINT('Origin',(0.,1.5,0.)) ;
#48620 = CARTESIAN_POINT('Origin',(0.,1.5,0.)) ;
#48621 = CARTESIAN_POINT('Origin',(0.,1.5,0.)) ;
#48622 = CARTESIAN_POINT('Origin',(0.,1.5,0.)) ;
#48623 = CARTESIAN_POINT('Origin',(0.,1.5,0.)) ;
#48624 = CARTESIAN_POINT('Origin',(0.,-1.5,0.)) ;
#48625 = CARTESIAN_POINT('Origin',(0.,-1.5,0.)) ;
#48626 = CARTESIAN_POINT('Origin',(0.,-1.5,0.)) ;
#48627 = CARTESIAN_POINT('Origin',(0.,-1.5,0.)) ;
#48628 = CARTESIAN_POINT('Origin',(0.,-1.5,0.)) ;
#48629 = CARTESIAN_POINT('',(7.38852762541953,608.210565160566,-48.0221601717519)) ;
#48630 = CARTESIAN_POINT('',(94.8885276254125,567.710565160551,-48.0221601717558)) ;
#48631 = CARTESIAN_POINT('',(7.38852762540283,513.210565160566,-48.0221601717519)) ;
#48632 = CARTESIAN_POINT('',(184.88852762542,608.210565160535,-48.0221601717599)) ;
#48633 = CARTESIAN_POINT('',(184.888527625403,513.210565160535,-48.0221601717599)) ;
#48634 = CARTESIAN_POINT('',(0.,0.,0.)) ;
#48635 = CARTESIAN_POINT('',(0.,0.,0.)) ;
#48636 = CARTESIAN_POINT('Origin',(1.04083408558609E-16,-6.38378239159465E-15,
-4.1322625)) ;
#48637 = CARTESIAN_POINT('',(7.23560708836202E-13,-1.00995540144768,-0.0444499999998741)) ;
#48638 = CARTESIAN_POINT('',(8.448295215077E-17,-1.00995540144768,2.72004641033163E-14)) ;
#48639 = CARTESIAN_POINT('',(8.448295215077E-17,-1.00995540144768,-4.1322625)) ;
#48640 = CARTESIAN_POINT('',(0.433387415541736,-0.912241887310266,2.49185368278523E-14)) ;
#48641 = CARTESIAN_POINT('Ctrl Pts',(1.44703693472025E-12,-1.00995540144768,
-0.0444499999998741)) ;
#48642 = CARTESIAN_POINT('Ctrl Pts',(0.025506828532912,-1.00995540144768,
-0.0421352325163382)) ;
#48643 = CARTESIAN_POINT('Ctrl Pts',(0.0510333004963693,-1.00898920656169,
-0.0397680585416139)) ;
#48644 = CARTESIAN_POINT('Ctrl Pts',(0.200353389061228,-0.997642142274717,
-0.0256225970302299)) ;
#48645 = CARTESIAN_POINT('Ctrl Pts',(0.321325408922422,-0.965480248872855,
-0.0129591540149241)) ;
#48646 = CARTESIAN_POINT('Ctrl Pts',(0.433387415541733,-0.912241887310264,
2.6701731103973E-14)) ;
#48647 = CARTESIAN_POINT('Origin',(1.04083408558609E-16,-6.38378239159465E-15,
0.)) ;
#48648 = CARTESIAN_POINT('Origin',(1.04083408558609E-16,-6.38378239159465E-15,
-4.1322625)) ;
#48649 = CARTESIAN_POINT('',(6.357143120128E-13,-1.00995540144768,-0.679449999999891)) ;
#48650 = CARTESIAN_POINT('',(2.45193363101085E-13,-1.00995540144768,-0.600074999999959)) ;
#48651 = CARTESIAN_POINT('',(8.448295215077E-17,-1.00995540144768,-4.1322625)) ;
#48652 = CARTESIAN_POINT('Ctrl Pts',(1.27134414107345E-12,-1.00995540144768,
-0.679449999999891)) ;
#48653 = CARTESIAN_POINT('Ctrl Pts',(0.0437634009185802,-1.00995540144768,
-0.675478432257258)) ;
#48654 = CARTESIAN_POINT('Ctrl Pts',(0.0875582439193204,-1.00711177961309,
-0.671355019401001)) ;
#48655 = CARTESIAN_POINT('Ctrl Pts',(0.26557918047378,-0.983801453112301,
-0.653978114529555)) ;
#48656 = CARTESIAN_POINT('Ctrl Pts',(0.395064237667927,-0.939304962798357,
-0.639895833911083)) ;
#48657 = CARTESIAN_POINT('Ctrl Pts',(0.624303148323518,-0.804528605296291,
-0.612030583529934)) ;
#48658 = CARTESIAN_POINT('Ctrl Pts',(0.72291777299032,-0.71724247121487,-0.598507856602888)) ;
#48659 = CARTESIAN_POINT('Ctrl Pts',(0.881958923219596,-0.509301855514422,
-0.57317967053573)) ;
#48660 = CARTESIAN_POINT('Ctrl Pts',(0.940594127778358,-0.390554680687541,
-0.56162626629538)) ;
#48661 = CARTESIAN_POINT('Ctrl Pts',(1.00987101600572,-0.134547391647658,
-0.534799235400863)) ;
#48662 = CARTESIAN_POINT('Ctrl Pts',(1.01878989490851,0.000372688306628111,
-0.520660945952939)) ;
#48663 = CARTESIAN_POINT('Ctrl Pts',(0.984171959584064,0.260795586207613,
-0.49337120293886)) ;
#48664 = CARTESIAN_POINT('Ctrl Pts',(0.942902939882405,0.384163694667602,
-0.48044344580559)) ;
#48665 = CARTESIAN_POINT('Ctrl Pts',(0.813570221399235,0.613266917555062,
-0.456435694848632)) ;
#48666 = CARTESIAN_POINT('Ctrl Pts',(0.724956102393718,0.715905786899936,
-0.443147159257415)) ;
#48667 = CARTESIAN_POINT('Ctrl Pts',(0.514163423924961,0.879282972696947,
-0.415457379020839)) ;
#48668 = CARTESIAN_POINT('Ctrl Pts',(0.394709115734629,0.938997134833771,
-0.401488067118609)) ;
#48669 = CARTESIAN_POINT('Ctrl Pts',(0.143188392677125,1.00798005112781,-0.375047973181057)) ;
#48670 = CARTESIAN_POINT('Ctrl Pts',(0.0140058409597491,1.01799616298282,
-0.363642338709345)) ;
#48671 = CARTESIAN_POINT('Ctrl Pts',(-0.247226330001402,0.988414461209624,
-0.338385350914255)) ;
#48672 = CARTESIAN_POINT('Ctrl Pts',(-0.37639700835342,0.946773140710743,
-0.324481197230098)) ;
#48673 = CARTESIAN_POINT('Ctrl Pts',(-0.607610842133004,0.817251073521645,
-0.296712019629347)) ;
#48674 = CARTESIAN_POINT('Ctrl Pts',(-0.708196666452128,0.731827505295378,
-0.283107993808755)) ;
#48675 = CARTESIAN_POINT('Ctrl Pts',(-0.871156333072791,0.527411858369104,
-0.257608889802603)) ;
#48676 = CARTESIAN_POINT('Ctrl Pts',(-0.931970985059438,0.41050304059754,
-0.246216657040143)) ;
#48677 = CARTESIAN_POINT('Ctrl Pts',(-1.0067530655191,0.156419528956202,-0.219591218982685)) ;
#48678 = CARTESIAN_POINT('Ctrl Pts',(-1.01860033273544,0.0214369986454144,
-0.205446385355298)) ;
#48679 = CARTESIAN_POINT('Ctrl Pts',(-0.989435466647989,-0.240200133406872,
-0.178029402616084)) ;
#48680 = CARTESIAN_POINT('Ctrl Pts',(-0.950651931827455,-0.364659436823405,
-0.164987299047911)) ;
#48681 = CARTESIAN_POINT('Ctrl Pts',(-0.825247524122355,-0.597764147034261,
-0.140560231811127)) ;
#48682 = CARTESIAN_POINT('Ctrl Pts',(-0.737680683582466,-0.703030138026511,
-0.127476546675298)) ;
#48683 = CARTESIAN_POINT('Ctrl Pts',(-0.528466085007257,-0.870794003954716,
-0.0997001382618737)) ;
#48684 = CARTESIAN_POINT('Ctrl Pts',(-0.4098063543708,-0.932536041247264,
-0.0856966843567157)) ;
#48685 = CARTESIAN_POINT('Ctrl Pts',(-0.190611916996757,-0.996422885426864,
-0.0624572387014332)) ;
#48686 = CARTESIAN_POINT('Ctrl Pts',(-0.0955075072374286,-1.00995540144768,
-0.0531173916325512)) ;
#48687 = CARTESIAN_POINT('Ctrl Pts',(1.44703693472025E-12,-1.00995540144768,
-0.0444499999998741)) ;
#48688 = CARTESIAN_POINT('',(-0.348937280953797,-0.94776193575914,-1.56815741427684E-16)) ;
#48689 = CARTESIAN_POINT('Origin',(1.04083408558609E-16,-6.38378239159465E-15,
0.)) ;
#48690 = CARTESIAN_POINT('Ctrl Pts',(-0.348937280953794,-0.947761935759138,
-2.01878444516801E-15)) ;
#48691 = CARTESIAN_POINT('Ctrl Pts',(-0.461713552528522,-0.906241123332891,
-0.0124100325913252)) ;
#48692 = CARTESIAN_POINT('Ctrl Pts',(-0.566180329108771,-0.844921873509237,
-0.0251033112604733)) ;
#48693 = CARTESIAN_POINT('Ctrl Pts',(-0.745859616028041,-0.690852949413873,
-0.0494818165451801)) ;
#48694 = CARTESIAN_POINT('Ctrl Pts',(-0.820397680576272,-0.600383170618035,
-0.0609107840527787)) ;
#48695 = CARTESIAN_POINT('Ctrl Pts',(-0.94161187970814,-0.387303216910876,
-0.0832394549376677)) ;
#48696 = CARTESIAN_POINT('Ctrl Pts',(-0.983280258010021,-0.264116309328272,
-0.0961482240118311)) ;
#48697 = CARTESIAN_POINT('Ctrl Pts',(-1.01877670334187,-0.00390044213731634,
-0.123416272255909)) ;
#48698 = CARTESIAN_POINT('Ctrl Pts',(-1.01033073852162,0.131003656243038,
-0.137552886993011)) ;
#48699 = CARTESIAN_POINT('Ctrl Pts',(-0.941947087402141,0.387317636260553,
-0.164412056067511)) ;
#48700 = CARTESIAN_POINT('Ctrl Pts',(-0.883664649499574,0.506364361030241,
-0.175995964172646)) ;
#48701 = CARTESIAN_POINT('Ctrl Pts',(-0.725256301987552,0.714870181751489,
-0.201296336774658)) ;
#48702 = CARTESIAN_POINT('Ctrl Pts',(-0.626961756250327,0.802451546689399,
-0.214805484889144)) ;
#48703 = CARTESIAN_POINT('Ctrl Pts',(-0.398251277024382,0.937951740403398,
-0.242660705082419)) ;
#48704 = CARTESIAN_POINT('Ctrl Pts',(-0.268963099837451,0.982875339591604,
-0.256747497056347)) ;
#48705 = CARTESIAN_POINT('Ctrl Pts',(-0.00710515020264792,1.01809280298334,
-0.282356560853332)) ;
#48706 = CARTESIAN_POINT('Ctrl Pts',(0.122441064791949,1.0107326518681,-0.293645911973156)) ;
#48707 = CARTESIAN_POINT('Ctrl Pts',(0.375235433236055,0.946911055779092,
-0.319931162722662)) ;
#48708 = CARTESIAN_POINT('Ctrl Pts',(0.495656691472225,0.889806436177891,
-0.333851499086522)) ;
#48709 = CARTESIAN_POINT('Ctrl Pts',(0.709442571371163,0.731236512440977,
-0.361561038277925)) ;
#48710 = CARTESIAN_POINT('Ctrl Pts',(0.800277276817402,0.630566775295668,
-0.375078965173411)) ;
#48711 = CARTESIAN_POINT('Ctrl Pts',(0.934302509181679,0.404472785875835,
-0.399088081314702)) ;
#48712 = CARTESIAN_POINT('Ctrl Pts',(0.978213313024649,0.282309921238749,
-0.411741713495526)) ;
#48713 = CARTESIAN_POINT('Ctrl Pts',(1.01849267055767,0.0230223918801653,
-0.438912481119966)) ;
#48714 = CARTESIAN_POINT('Ctrl Pts',(1.01260644401027,-0.111766631062521,
-0.453037037089784)) ;
#48715 = CARTESIAN_POINT('Ctrl Pts',(0.949079392935516,-0.369721482521146,
-0.480068153256141)) ;
#48716 = CARTESIAN_POINT('Ctrl Pts',(0.892711807051305,-0.490402608322398,
-0.491838609662575)) ;
#48717 = CARTESIAN_POINT('Ctrl Pts',(0.737729733608816,-0.701949266681669,
-0.516987369679715)) ;
#48718 = CARTESIAN_POINT('Ctrl Pts',(0.641175934951445,-0.791102258115751,
-0.530420888894451)) ;
#48719 = CARTESIAN_POINT('Ctrl Pts',(0.415352993918571,-0.93047025311943,
-0.558216716069348)) ;
#48720 = CARTESIAN_POINT('Ctrl Pts',(0.287149755951262,-0.977682389087762,
-0.572324956845148)) ;
#48721 = CARTESIAN_POINT('Ctrl Pts',(0.102530413489681,-1.00605547915662,
-0.590565936714243)) ;
#48722 = CARTESIAN_POINT('Ctrl Pts',(0.0512545503777301,-1.00995540144768,
-0.595423603749283)) ;
#48723 = CARTESIAN_POINT('Ctrl Pts',(4.90302243250019E-13,-1.00995540144768,
-0.600074999999959)) ;
#48724 = CARTESIAN_POINT('Origin',(1.04083408558609E-16,-6.38378239159465E-15,
-4.1322625)) ;
#48725 = CARTESIAN_POINT('',(7.26230717109419E-14,-1.00995540144768,-1.31444999999999)) ;
#48726 = CARTESIAN_POINT('',(-6.18419324832232E-17,-1.00995540144768,-1.235075)) ;
#48727 = CARTESIAN_POINT('',(8.448295215077E-17,-1.00995540144768,-4.1322625)) ;
#48728 = CARTESIAN_POINT('Ctrl Pts',(1.45161660469733E-13,-1.00995540144768,
-1.31444999999999)) ;
#48729 = CARTESIAN_POINT('Ctrl Pts',(0.0565109964714736,-1.00995540144768,
-1.30932157656885)) ;
#48730 = CARTESIAN_POINT('Ctrl Pts',(0.113028660198271,-1.00521499788339,
-1.30394417438287)) ;
#48731 = CARTESIAN_POINT('Ctrl Pts',(0.302193867993356,-0.973108983005214,
-1.28509506637953)) ;
#48732 = CARTESIAN_POINT('Ctrl Pts',(0.429465110701191,-0.924012640872624,
-1.2709726819248)) ;
#48733 = CARTESIAN_POINT('Ctrl Pts',(0.652838291547309,-0.781473970039967,
-1.24323304494836)) ;
#48734 = CARTESIAN_POINT('Ctrl Pts',(0.747925745683043,-0.691040292433543,
-1.22986549618965)) ;
#48735 = CARTESIAN_POINT('Ctrl Pts',(0.900039665300462,-0.476973275113707,
-1.20484496935425)) ;
#48736 = CARTESIAN_POINT('Ctrl Pts',(0.954797052853043,-0.354908264883124,
-1.19289087461317)) ;
#48737 = CARTESIAN_POINT('Ctrl Pts',(1.01423245983247,-0.095605949188269,
-1.16571855752699)) ;
#48738 = CARTESIAN_POINT('Ctrl Pts',(1.01797796810863,0.0390496479844164,
-1.15160798325772)) ;
#48739 = CARTESIAN_POINT('Ctrl Pts',(0.973735166614192,0.297314907494692,
-1.1245443393988)) ;
#48740 = CARTESIAN_POINT('Ctrl Pts',(0.928022939522984,0.418646151519161,
-1.11215059051402)) ;
#48741 = CARTESIAN_POINT('Ctrl Pts',(0.790642705724418,0.642609633844796,
-1.08794863302621)) ;
#48742 = CARTESIAN_POINT('Ctrl Pts',(0.698279070382183,0.741908739075154,
-1.07436376870799)) ;
#48743 = CARTESIAN_POINT('Ctrl Pts',(0.482247866830835,0.897115859201658,
-1.04662665866158)) ;
#48744 = CARTESIAN_POINT('Ctrl Pts',(0.361167799952309,0.952339641367629,
-1.03274508140156)) ;
#48745 = CARTESIAN_POINT('Ctrl Pts',(0.107478375300796,1.01245532598292,-1.006572774929)) ;
#48746 = CARTESIAN_POINT('Ctrl Pts',(-0.0223459833230694,1.01789594597081,
-0.995338127294016)) ;
#48747 = CARTESIAN_POINT('Ctrl Pts',(-0.283626891794233,0.978716836240998,
-0.969573859828927)) ;
#48748 = CARTESIAN_POINT('Ctrl Pts',(-0.412043838067636,0.931947088196774,
-0.955469403772045)) ;
#48749 = CARTESIAN_POINT('Ctrl Pts',(-0.63843240043722,0.793325346866863,
-0.927661345956073)) ;
#48750 = CARTESIAN_POINT('Ctrl Pts',(-0.735326105056216,0.704474795907485,
-0.914212826356226)) ;
#48751 = CARTESIAN_POINT('Ctrl Pts',(-0.890975285096107,0.493517630963721,
-0.889034412357887)) ;
#48752 = CARTESIAN_POINT('Ctrl Pts',(-0.947716387344409,0.373156358605394,
-0.877303094284298)) ;
#48753 = CARTESIAN_POINT('Ctrl Pts',(-1.01219170575329,0.115518356801635,
-0.850305180826787)) ;
#48754 = CARTESIAN_POINT('Ctrl Pts',(-1.01857616319312,-0.0192968522412743,
-0.836177880812757)) ;
#48755 = CARTESIAN_POINT('Ctrl Pts',(-0.979219896892731,-0.278819755610391,
-0.808982448320859)) ;
#48756 = CARTESIAN_POINT('Ctrl Pts',(-0.935726541635327,-0.401177227310065,
-0.796264984497799)) ;
#48757 = CARTESIAN_POINT('Ctrl Pts',(-0.802479205122599,-0.627761205578296,
-0.772300790108584)) ;
#48758 = CARTESIAN_POINT('Ctrl Pts',(-0.712001100701131,-0.728744435673642,
-0.758798799595079)) ;
#48759 = CARTESIAN_POINT('Ctrl Pts',(-0.49874208733636,-0.888087400594881,
-0.731096570478756)) ;
#48760 = CARTESIAN_POINT('Ctrl Pts',(-0.378477339871019,-0.945625968271003,
-0.717167700874882)) ;
#48761 = CARTESIAN_POINT('Ctrl Pts',(-0.168470635591927,-0.999401318650093,
-0.695291842461025)) ;
#48762 = CARTESIAN_POINT('Ctrl Pts',(-0.0843440584127307,-1.00995540144768,
-0.687104298675449)) ;
#48763 = CARTESIAN_POINT('Ctrl Pts',(1.27134414107345E-12,-1.00995540144768,
-0.679449999999891)) ;
#48764 = CARTESIAN_POINT('Ctrl Pts',(4.90302243250019E-13,-1.00995540144768,
-0.600074999999959)) ;
#48765 = CARTESIAN_POINT('Ctrl Pts',(-0.0770781742531291,-1.00995540144768,
-0.60706991319485)) ;
#48766 = CARTESIAN_POINT('Ctrl Pts',(-0.154023911223334,-1.00114029685864,
-0.614514675458974)) ;
#48767 = CARTESIAN_POINT('Ctrl Pts',(-0.357783489255834,-0.953610067886598,
-0.6354963881168)) ;
#48768 = CARTESIAN_POINT('Ctrl Pts',(-0.479017160202537,-0.898838236541642,
-0.649368225096111)) ;
#48769 = CARTESIAN_POINT('Ctrl Pts',(-0.695578689880959,-0.74444211912628,
-0.677110970182544)) ;
#48770 = CARTESIAN_POINT('Ctrl Pts',(-0.788305698603855,-0.645475225111657,
-0.690711404735574)) ;
#48771 = CARTESIAN_POINT('Ctrl Pts',(-0.926488213354373,-0.422025397907093,
-0.7149592569495)) ;
#48772 = CARTESIAN_POINT('Ctrl Pts',(-0.972631542089144,-0.300891171801688,
-0.727294582283833)) ;
#48773 = CARTESIAN_POINT('Ctrl Pts',(-1.01781791392863,-0.0428720573080172,
-0.754332432580429)) ;
#48774 = CARTESIAN_POINT('Ctrl Pts',(-1.01458231554768,0.0917467407720381,
-0.768439150668889)) ;
#48775 = CARTESIAN_POINT('Ctrl Pts',(-0.956125807533879,0.351366681622582,
-0.79564475172873)) ;
#48776 = CARTESIAN_POINT('Ctrl Pts',(-0.901753381462521,0.473763630641837,
-0.80764627858924)) ;
#48777 = CARTESIAN_POINT('Ctrl Pts',(-0.750323191744204,0.688428094908377,
-0.832636059589635)) ;
#48778 = CARTESIAN_POINT('Ctrl Pts',(-0.655586413466596,0.779162370652702,
-0.845987534056174)) ;
#48779 = CARTESIAN_POINT('Ctrl Pts',(-0.432801382336186,0.922447816402019,
-0.873712923231553)) ;
#48780 = CARTESIAN_POINT('Ctrl Pts',(-0.305755405079719,0.971989039570837,
-0.887838174210686)) ;
#48781 = CARTESIAN_POINT('Ctrl Pts',(-0.0453962757393742,1.01717320061781,
-0.913833424377218)) ;
#48782 = CARTESIAN_POINT('Ctrl Pts',(0.0848738524560454,1.01464328987563,
-0.925031755796313)) ;
#48783 = CARTESIAN_POINT('Ctrl Pts',(0.339879357290095,0.960104774255783,
-0.951031281657117)) ;
#48784 = CARTESIAN_POINT('Ctrl Pts',(0.461894575965491,0.907720518449188,
-0.964848947644651)) ;
#48785 = CARTESIAN_POINT('Ctrl Pts',(0.681199070812265,0.757627517530871,
-0.992615157254959)) ;
#48786 = CARTESIAN_POINT('Ctrl Pts',(0.775820085330474,0.660433840697432,
-1.00629456671852)) ;
#48787 = CARTESIAN_POINT('Ctrl Pts',(0.918217069813966,0.439709332307288,
-1.0307820926036)) ;
#48788 = CARTESIAN_POINT('Ctrl Pts',(0.966628035471543,0.319598446430998,
-1.04283424499689)) ;
#48789 = CARTESIAN_POINT('Ctrl Pts',(1.01674514418657,0.0628828651013657,
-1.06973549791536)) ;
#48790 = CARTESIAN_POINT('Ctrl Pts',(1.01617497448599,-0.0715119915840745,
-1.0838187491614)) ;
#48791 = CARTESIAN_POINT('Ctrl Pts',(0.962863906090873,-0.332771271630767,
-1.11119613674899)) ;
#48792 = CARTESIAN_POINT('Ctrl Pts',(0.910514170054564,-0.456917853227476,
-1.12346859379693)) ;
#48793 = CARTESIAN_POINT('Ctrl Pts',(0.762662596351267,-0.674688186803455,
-1.14829634438262)) ;
#48794 = CARTESIAN_POINT('Ctrl Pts',(0.669767552817714,-0.766966274896015,
-1.16156156790488)) ;
#48795 = CARTESIAN_POINT('Ctrl Pts',(0.450085565295974,-0.914103075865332,
-1.18920714506014)) ;
#48796 = CARTESIAN_POINT('Ctrl Pts',(0.324237320273755,-0.965945585652875,
-1.20334427680273)) ;
#48797 = CARTESIAN_POINT('Ctrl Pts',(0.128503467450188,-1.00382548182994,
-1.2230920180285)) ;
#48798 = CARTESIAN_POINT('Ctrl Pts',(0.064265873499002,-1.00995540144768,
-1.2292428145484)) ;
#48799 = CARTESIAN_POINT('Ctrl Pts',(-2.08166817117216E-16,-1.00995540144768,
-1.235075)) ;
#48800 = CARTESIAN_POINT('Origin',(1.04083408558609E-16,-6.38378239159465E-15,
-4.1322625)) ;
#48801 = CARTESIAN_POINT('',(-8.02468796914548E-14,-1.00995540144768,-1.94945000000002)) ;
#48802 = CARTESIAN_POINT('',(-1.98317215169442E-13,-1.00995540144768,-1.87007500000004)) ;
#48803 = CARTESIAN_POINT('',(8.448295215077E-17,-1.00995540144768,-4.1322625)) ;
#48804 = CARTESIAN_POINT('Ctrl Pts',(-1.6057824233506E-13,-1.00995540144768,
-1.94945000000002)) ;
#48805 = CARTESIAN_POINT('Ctrl Pts',(0.0723553003243024,-1.00995540144769,
-1.94288369183485)) ;
#48806 = CARTESIAN_POINT('Ctrl Pts',(0.144623390562603,-1.00218667636261,
-1.93591825530127)) ;
#48807 = CARTESIAN_POINT('Ctrl Pts',(0.344225695278461,-0.958562901762504,
-1.9155184977955)) ;
#48808 = CARTESIAN_POINT('Ctrl Pts',(0.466055957642379,-0.905599570317038,
-1.90168727605979)) ;
#48809 = CARTESIAN_POINT('Ctrl Pts',(0.680797269323851,-0.757160674168711,
-1.87442184630654)) ;
#48810 = CARTESIAN_POINT('Ctrl Pts',(0.772221484095825,-0.663690612493028,
-1.86122764828989)) ;
#48811 = CARTESIAN_POINT('Ctrl Pts',(0.91722818854932,-0.443476524508156,
-1.83653003148946)) ;
#48812 = CARTESIAN_POINT('Ctrl Pts',(0.967959630703487,-0.317925019761586,
-1.82401539644544)) ;
#48813 = CARTESIAN_POINT('Ctrl Pts',(1.01715414359895,-0.0553907798653038,
-1.79650440568037)) ;
#48814 = CARTESIAN_POINT('Ctrl Pts',(1.01561050663032,0.0787883937661297,
-1.78244375588438)) ;
#48815 = CARTESIAN_POINT('Ctrl Pts',(0.961582983560333,0.334449715008675,
-1.75565297899194)) ;
#48816 = CARTESIAN_POINT('Ctrl Pts',(0.911354849604406,0.45375657101305,-1.7437983341723)) ;
#48817 = CARTESIAN_POINT('Ctrl Pts',(0.765589482467509,0.672269616441594,
-1.71912099427007)) ;
#48818 = CARTESIAN_POINT('Ctrl Pts',(0.669473384740545,0.768012341070395,
-1.70538192738671)) ;
#48819 = CARTESIAN_POINT('Ctrl Pts',(0.448029690569759,0.914615154714995,
-1.67760445207281)) ;
#48820 = CARTESIAN_POINT('Ctrl Pts',(0.32542091582782,0.965075466611859,-1.66383372548469)) ;
#48821 = CARTESIAN_POINT('Ctrl Pts',(0.0695471621562103,1.01584437983776,
-1.63795291378274)) ;
#48822 = CARTESIAN_POINT('Ctrl Pts',(-0.061042847696245,1.01639061240754,
-1.62674748023882)) ;
#48823 = CARTESIAN_POINT('Ctrl Pts',(-0.320741465994523,0.967118688915825,
-1.60059799351017)) ;
#48824 = CARTESIAN_POINT('Ctrl Pts',(-0.446819982081549,0.915710520284951,
-1.58646272179053)) ;
#48825 = CARTESIAN_POINT('Ctrl Pts',(-0.667095500822319,0.769299116080178,
-1.55880128834857)) ;
#48826 = CARTESIAN_POINT('Ctrl Pts',(-0.760341749797416,0.677310961433985,
-1.54551938369688)) ;
#48827 = CARTESIAN_POINT('Ctrl Pts',(-0.908874243045885,0.46012886265203,
-1.5206606596471)) ;
#48828 = CARTESIAN_POINT('Ctrl Pts',(-0.961609909749135,0.336316743673208,
-1.50844266713929)) ;
#48829 = CARTESIAN_POINT('Ctrl Pts',(-1.01590285320031,0.0753663643783231,
-1.48109764929416)) ;
#48830 = CARTESIAN_POINT('Ctrl Pts',(-1.01697968853456,-0.0590751536885078,
-1.46700950839704)) ;
#48831 = CARTESIAN_POINT('Ctrl Pts',(-0.967799758829855,-0.316040723953939,
-1.44008205911155)) ;
#48832 = CARTESIAN_POINT('Ctrl Pts',(-0.919821777225401,-0.436345304729499,
-1.42797897963809)) ;
#48833 = CARTESIAN_POINT('Ctrl Pts',(-0.778228666363001,-0.657593182198298,
-1.40353698405195)) ;
#48834 = CARTESIAN_POINT('Ctrl Pts',(-0.683966951987112,-0.755128715282229,
-1.38987226982107)) ;
#48835 = CARTESIAN_POINT('Ctrl Pts',(-0.465180022352401,-0.90604801038786,
-1.36210973598864)) ;
#48836 = CARTESIAN_POINT('Ctrl Pts',(-0.343310564426513,-0.958889388421443,
-1.34828134697613)) ;
#48837 = CARTESIAN_POINT('Ctrl Pts',(-0.143990621346624,-1.00225470563842,
-1.32792075592941)) ;
#48838 = CARTESIAN_POINT('Ctrl Pts',(-0.072037538307033,-1.00995540144768,
-1.32098747097813)) ;
#48839 = CARTESIAN_POINT('Ctrl Pts',(1.45161660469733E-13,-1.00995540144768,
-1.31444999999999)) ;
#48840 = CARTESIAN_POINT('Ctrl Pts',(-2.08166817117216E-16,-1.00995540144768,
-1.235075)) ;
#48841 = CARTESIAN_POINT('Ctrl Pts',(-0.0646876702990289,-1.00995540144768,
-1.24094546388815)) ;
#48842 = CARTESIAN_POINT('Ctrl Pts',(-0.129344610750813,-1.0037448041883,
-1.24713854358703)) ;
#48843 = CARTESIAN_POINT('Ctrl Pts',(-0.322043264294838,-0.966201838386248,
-1.26659318428093)) ;
#48844 = CARTESIAN_POINT('Ctrl Pts',(-0.444785930738073,-0.916190451953308,
-1.28035254018717)) ;
#48845 = CARTESIAN_POINT('Ctrl Pts',(-0.66671972164513,-0.770404905740835,
-1.30813167144754)) ;
#48846 = CARTESIAN_POINT('Ctrl Pts',(-0.763180705005661,-0.675003549261792,
-1.3218841510081)) ;
#48847 = CARTESIAN_POINT('Ctrl Pts',(-0.909728661768419,-0.457008614310503,
-1.34660536519238)) ;
#48848 = CARTESIAN_POINT('Ctrl Pts',(-0.960379737745155,-0.337886824477322,
-1.35841780392719)) ;
#48849 = CARTESIAN_POINT('Ctrl Pts',(-1.01531202255019,-0.0824720101177455,
-1.3851827493373)) ;
#48850 = CARTESIAN_POINT('Ctrl Pts',(-1.01734459520918,0.0516524552068899,
-1.39923766624404)) ;
#48851 = CARTESIAN_POINT('Ctrl Pts',(-0.96910705685852,0.314478405656836,
-1.42677922538887)) ;
#48852 = CARTESIAN_POINT('Ctrl Pts',(-0.918751951194141,0.440357074358718,
-1.43935330491219)) ;
#48853 = CARTESIAN_POINT('Ctrl Pts',(-0.77440432267991,0.661134117077949,
-1.46402060602521)) ;
#48854 = CARTESIAN_POINT('Ctrl Pts',(-0.683321601246241,0.754875873315237,
-1.47719804866716)) ;
#48855 = CARTESIAN_POINT('Ctrl Pts',(-0.466715554991479,0.905690194324463,
-1.50475716526057)) ;
#48856 = CARTESIAN_POINT('Ctrl Pts',(-0.342069221262696,0.959741291666654,
-1.51890094154091)) ;
#48857 = CARTESIAN_POINT('Ctrl Pts',(-0.083356074104296,1.01486601437281,
-1.54526765360729)) ;
#48858 = CARTESIAN_POINT('Ctrl Pts',(0.0476993612733256,1.01716462966343,
-1.55652603176877)) ;
#48859 = CARTESIAN_POINT('Ctrl Pts',(0.30478503753594,0.971753598811276,-1.5822360999986)) ;
#48860 = CARTESIAN_POINT('Ctrl Pts',(0.428184010449668,0.924032903527723,
-1.59593499541964)) ;
#48861 = CARTESIAN_POINT('Ctrl Pts',(0.65256564006348,0.782434360912067,-1.6237168919553)) ;
#48862 = CARTESIAN_POINT('Ctrl Pts',(0.750763187048053,0.688791284702509,
-1.63753484102893)) ;
#48863 = CARTESIAN_POINT('Ctrl Pts',(0.901285507204505,0.473453138348931,
-1.66247752966383)) ;
#48864 = CARTESIAN_POINT('Ctrl Pts',(0.954089680485891,0.355261282001321,
-1.67409713268568)) ;
#48865 = CARTESIAN_POINT('Ctrl Pts',(1.01359551140853,0.101107455485839,-1.70072993904624)) ;
#48866 = CARTESIAN_POINT('Ctrl Pts',(1.01809809795569,-0.0327128628235703,
-1.71475298435508)) ;
#48867 = CARTESIAN_POINT('Ctrl Pts',(0.97472400106394,-0.296993875268589,
-1.74244701960028)) ;
#48868 = CARTESIAN_POINT('Ctrl Pts',(0.926282905700387,-0.424537957414063,
-1.75534102059181)) ;
#48869 = CARTESIAN_POINT('Ctrl Pts',(0.785271774586696,-0.648146462177879,
-1.77985388618761)) ;
#48870 = CARTESIAN_POINT('Ctrl Pts',(0.695921543177911,-0.743238012536047,
-1.7929448263459)) ;
#48871 = CARTESIAN_POINT('Ctrl Pts',(0.482275975299125,-0.897467842237503,
-1.82041423263958)) ;
#48872 = CARTESIAN_POINT('Ctrl Pts',(0.358799392659723,-0.953580438943742,
-1.8345598653314)) ;
#48873 = CARTESIAN_POINT('Ctrl Pts',(0.153004812027378,-1.00125741452764,
-1.85573394509024)) ;
#48874 = CARTESIAN_POINT('Ctrl Pts',(0.0765634856563495,-1.00995540144771,
-1.86312679525529)) ;
#48875 = CARTESIAN_POINT('Ctrl Pts',(-3.96718913291035E-13,-1.00995540144768,
-1.87007500000004)) ;
#48876 = CARTESIAN_POINT('Origin',(1.04083408558609E-16,-6.38378239159465E-15,
-4.1322625)) ;
#48877 = CARTESIAN_POINT('',(-6.5243389008471E-13,-1.00995540144768,-2.58445000000013)) ;
#48878 = CARTESIAN_POINT('',(-7.96237503807855E-13,-1.00995540144768,-2.50507500000015)) ;
#48879 = CARTESIAN_POINT('',(8.448295215077E-17,-1.00995540144768,-4.1322625)) ;
#48880 = CARTESIAN_POINT('Ctrl Pts',(-1.30495226312157E-12,-1.00995540144768,
-2.58445000000013)) ;
#48881 = CARTESIAN_POINT('Ctrl Pts',(0.0846470609818248,-1.00995540144779,
-2.57676820357058)) ;
#48882 = CARTESIAN_POINT('Ctrl Pts',(0.169072699863829,-0.999325393833233,
-2.56854954158348)) ;
#48883 = CARTESIAN_POINT('Ctrl Pts',(0.379335907038639,-0.945283480371864,
-2.54663643871582)) ;
#48884 = CARTESIAN_POINT('Ctrl Pts',(0.499558908636285,-0.88762995657192,
-2.53270533445456)) ;
#48885 = CARTESIAN_POINT('Ctrl Pts',(0.712677793878948,-0.728082385899932,
-2.50500510176141)) ;
#48886 = CARTESIAN_POINT('Ctrl Pts',(0.80306118939936,-0.627016282211641,
-2.49150736399903)) ;
#48887 = CARTESIAN_POINT('Ctrl Pts',(0.936102208690891,-0.400302596724463,
-2.46755509706542)) ;
#48888 = CARTESIAN_POINT('Ctrl Pts',(0.979484856296888,-0.277893397385756,
-2.45482047850282)) ;
#48889 = CARTESIAN_POINT('Ctrl Pts',(1.0185960320577,-0.0183081726476704,
-2.42761851534808)) ;
#48890 = CARTESIAN_POINT('Ctrl Pts',(1.01207931533077,0.11651367972252,-2.41349051917908)) ;
#48891 = CARTESIAN_POINT('Ctrl Pts',(0.947352518855438,0.374067365839076,
-2.38650144117135)) ;
#48892 = CARTESIAN_POINT('Ctrl Pts',(0.890512334711962,0.494343871604385,
-2.37478028355899)) ;
#48893 = CARTESIAN_POINT('Ctrl Pts',(0.734686087275951,0.70514436145921,-2.34959400953578)) ;
#48894 = CARTESIAN_POINT('Ctrl Pts',(0.637702239542249,0.793914347644846,
-2.3361415305633)) ;
#48895 = CARTESIAN_POINT('Ctrl Pts',(0.411163818275492,0.932337458834412,
-2.30833028015519)) ;
#48896 = CARTESIAN_POINT('Ctrl Pts',(0.282690346142352,0.978989524863807,
-2.29422686028141)) ;
#48897 = CARTESIAN_POINT('Ctrl Pts',(0.0213717919190553,1.01791521876209,
-2.26847245416657)) ;
#48898 = CARTESIAN_POINT('Ctrl Pts',(-0.108434393691808,1.01235181018582,
-2.25723504183201)) ;
#48899 = CARTESIAN_POINT('Ctrl Pts',(-0.362067206439329,0.95199970886247,
-2.23105548587441)) ;
#48900 = CARTESIAN_POINT('Ctrl Pts',(-0.483106134822916,0.896655782819292,
-2.21717134702477)) ;
#48901 = CARTESIAN_POINT('Ctrl Pts',(-0.698995761555616,0.741233261904337,
-2.18943579926547)) ;
#48902 = CARTESIAN_POINT('Ctrl Pts',(-0.791262538823597,0.641846029332726,
-2.17585510746734)) ;
#48903 = CARTESIAN_POINT('Ctrl Pts',(-0.928429249625612,0.417746114456447,
-2.15166537899158)) ;
#48904 = CARTESIAN_POINT('Ctrl Pts',(-0.974026766105337,0.296362315267558,
-2.13925583836098)) ;
#48905 = CARTESIAN_POINT('Ctrl Pts',(-1.01801817035029,0.0380316545170728,
-2.11218534109918)) ;
#48906 = CARTESIAN_POINT('Ctrl Pts',(-1.01413682011532,-0.09663341981603,
-2.09807377371727)) ;
#48907 = CARTESIAN_POINT('Ctrl Pts',(-0.954440915256791,-0.35585090227032,
-2.07091034631534)) ;
#48908 = CARTESIAN_POINT('Ctrl Pts',(-0.899581070501349,-0.477827632577549,
-2.05896864865341)) ;
#48909 = CARTESIAN_POINT('Ctrl Pts',(-0.747285042663379,-0.69173530390667,
-2.03393994427587)) ;
#48910 = CARTESIAN_POINT('Ctrl Pts',(-0.652104257507281,-0.78208861345665,
-2.02056813653222)) ;
#48911 = CARTESIAN_POINT('Ctrl Pts',(-0.428574690228414,-0.924427794215891,
-1.99282475964021)) ;
#48912 = CARTESIAN_POINT('Ctrl Pts',(-0.301243647016655,-0.973405364852332,
-1.97870317127512)) ;
#48913 = CARTESIAN_POINT('Ctrl Pts',(-0.112364114618148,-1.00527064570199,
-1.95989260184148)) ;
#48914 = CARTESIAN_POINT('Ctrl Pts',(-0.0561781570330956,-1.00995540144767,
-1.9545482179547)) ;
#48915 = CARTESIAN_POINT('Ctrl Pts',(-1.6057824233506E-13,-1.00995540144768,
-1.94945000000002)) ;
#48916 = CARTESIAN_POINT('Ctrl Pts',(-3.96718913291035E-13,-1.00995540144768,
-1.87007500000004)) ;
#48917 = CARTESIAN_POINT('Ctrl Pts',(-0.0532324031388302,-1.00995540144766,
-1.8749058881563)) ;
#48918 = CARTESIAN_POINT('Ctrl Pts',(-0.106483666306345,-1.00574880487635,
-1.87995889272685)) ;
#48919 = CARTESIAN_POINT('Ctrl Pts',(-0.292825540902382,-0.975986710216376,
-1.8984289708955)) ;
#48920 = CARTESIAN_POINT('Ctrl Pts',(-0.420680856549743,-0.928062759352234,
-1.91254293298895)) ;
#48921 = CARTESIAN_POINT('Ctrl Pts',(-0.645586111849608,-0.787495464559284,
-1.94031831673936)) ;
#48922 = CARTESIAN_POINT('Ctrl Pts',(-0.741589518910646,-0.697857228405682,
-1.95372731184761)) ;
#48923 = CARTESIAN_POINT('Ctrl Pts',(-0.895493231454798,-0.485360289051763,
-1.9788279996725)) ;
#48924 = CARTESIAN_POINT('Ctrl Pts',(-0.951256265240327,-0.364160496663927,
-1.99066458303998)) ;
#48925 = CARTESIAN_POINT('Ctrl Pts',(-1.01324774041705,-0.105696196860988,
-2.01774908435222)) ;
#48926 = CARTESIAN_POINT('Ctrl Pts',(-1.01832881772648,0.0290466284782181,
-2.03186879927028)) ;
#48927 = CARTESIAN_POINT('Ctrl Pts',(-0.976558289733235,0.287951762494217,
-2.05899949564633)) ;
#48928 = CARTESIAN_POINT('Ctrl Pts',(-0.931971481044396,0.409800986068976,
-2.07155263290278)) ;
#48929 = CARTESIAN_POINT('Ctrl Pts',(-0.796686838022514,0.635098512061202,
-2.09563431094332)) ;
#48930 = CARTESIAN_POINT('Ctrl Pts',(-0.705276453944694,0.73525726628461,
-2.10917770821186)) ;
#48931 = CARTESIAN_POINT('Ctrl Pts',(-0.490642543662654,0.892570302392133,
-2.13689835222457)) ;
#48932 = CARTESIAN_POINT('Ctrl Pts',(-0.369970882133026,0.948970636135906,
-2.15080451181635)) ;
#48933 = CARTESIAN_POINT('Ctrl Pts',(-0.116839143478311,1.01140328883631,
-2.17704760545166)) ;
#48934 = CARTESIAN_POINT('Ctrl Pts',(0.0128096373669957,1.0180453032631,-2.18831361520504)) ;
#48935 = CARTESIAN_POINT('Ctrl Pts',(0.274454571680543,0.981345739588494,
-2.21398100239395)) ;
#48936 = CARTESIAN_POINT('Ctrl Pts',(0.403419928429485,0.935729881775167,
-2.22807476905191)) ;
#48937 = CARTESIAN_POINT('Ctrl Pts',(0.631266978248035,0.799057813066932,
-2.25591303270715)) ;
#48938 = CARTESIAN_POINT('Ctrl Pts',(0.729039556487895,0.710999210621054,
-2.26939981668926)) ;
#48939 = CARTESIAN_POINT('Ctrl Pts',(0.886417892194377,0.501575802907125,
-2.29465479181844)) ;
#48940 = CARTESIAN_POINT('Ctrl Pts',(0.94412557286881,0.382039945305987,-2.3062909937258)) ;
#48941 = CARTESIAN_POINT('Ctrl Pts',(1.0110528108713,0.125229171849372,-2.33320222183732)) ;
#48942 = CARTESIAN_POINT('Ctrl Pts',(1.01872908421214,-0.00964540011792789,
-2.34733574249848)) ;
#48943 = CARTESIAN_POINT('Ctrl Pts',(0.981804085738894,-0.269517792034247,
-2.3745677979322)) ;
#48944 = CARTESIAN_POINT('Ctrl Pts',(0.939486941403989,-0.392406817819474,
-2.38744535194132)) ;
#48945 = CARTESIAN_POINT('Ctrl Pts',(0.808252887693214,-0.620249099775226,
-2.41132096876468)) ;
#48946 = CARTESIAN_POINT('Ctrl Pts',(0.718772385618642,-0.722113821672774,
-2.42476428887626)) ;
#48947 = CARTESIAN_POINT('Ctrl Pts',(0.50667115026837,-0.883605021828442,
-2.45247400550182)) ;
#48948 = CARTESIAN_POINT('Ctrl Pts',(0.386817191786182,-0.94226080444667,
-2.46642413217434)) ;
#48949 = CARTESIAN_POINT('Ctrl Pts',(0.174328275065335,-0.99865086313136,
-2.48866225136547)) ;
#48950 = CARTESIAN_POINT('Ctrl Pts',(0.0872926934494732,-1.00995540144781,
-2.49715311005985)) ;
#48951 = CARTESIAN_POINT('Ctrl Pts',(-1.59255949056786E-12,-1.00995540144768,
-2.50507500000015)) ;
#48952 = CARTESIAN_POINT('Origin',(1.04083408558609E-16,-6.38378239159465E-15,
-4.1322625)) ;
#48953 = CARTESIAN_POINT('',(-1.04524481388633E-12,-1.00995540144768,-3.2194500000002)) ;
#48954 = CARTESIAN_POINT('',(-1.02102525789085E-12,-1.00995540144768,-3.14007500000019)) ;
#48955 = CARTESIAN_POINT('',(8.448295215077E-17,-1.00995540144768,-4.1322625)) ;
#48956 = CARTESIAN_POINT('Ctrl Pts',(-2.0905741107248E-12,-1.00995540144768,
-3.2194500000002)) ;
#48957 = CARTESIAN_POINT('Ctrl Pts',(0.0957964344610122,-1.00995540144787,
-3.21075638796364)) ;
#48958 = CARTESIAN_POINT('Ctrl Pts',(0.19120672053905,-0.99634144807684,-3.20138451543131)) ;
#48959 = CARTESIAN_POINT('Ctrl Pts',(0.410677519689301,-0.932154392330389,
-3.17810426009695)) ;
#48960 = CARTESIAN_POINT('Ctrl Pts',(0.529290181800663,-0.870295210259502,
-3.16409893989565)) ;
#48961 = CARTESIAN_POINT('Ctrl Pts',(0.738318065068587,-0.702351931339841,
-3.13633007571004)) ;
#48962 = CARTESIAN_POINT('Ctrl Pts',(0.825761940824997,-0.597043690489556,
-3.12326427147137)) ;
#48963 = CARTESIAN_POINT('Ctrl Pts',(0.950958390039551,-0.363863299157179,
-3.09882927360186)) ;
#48964 = CARTESIAN_POINT('Ctrl Pts',(0.9896403084229,-0.239360706883989,-3.08578263378982)) ;
#48965 = CARTESIAN_POINT('Ctrl Pts',(1.01858275692398,0.0223233789725686,
-3.05836073075649)) ;
#48966 = CARTESIAN_POINT('Ctrl Pts',(1.00661630445378,0.157307122392741,-3.04421577000725)) ;
#48967 = CARTESIAN_POINT('Ctrl Pts',(0.931611065810261,0.411311432915673,
-3.01759863144336)) ;
#48968 = CARTESIAN_POINT('Ctrl Pts',(0.870707847851678,0.528146027334785,
-3.00621194294102)) ;
#48969 = CARTESIAN_POINT('Ctrl Pts',(0.707588663772576,0.732417261249297,
-2.98070592911035)) ;
#48970 = CARTESIAN_POINT('Ctrl Pts',(0.606923010414609,0.817763754257943,
-2.96709869709325)) ;
#48971 = CARTESIAN_POINT('Ctrl Pts',(0.375590136282912,0.947093381198886,
-2.93932879939114)) ;
#48972 = CARTESIAN_POINT('Ctrl Pts',(0.246384826922,0.988624483967684,-2.92542727777577)) ;
#48973 = CARTESIAN_POINT('Ctrl Pts',(-0.0148652763260574,1.01798314072302,
-2.90018034906513)) ;
#48974 = CARTESIAN_POINT('Ctrl Pts',(-0.144033550107956,1.00785891794961,
-2.88876898124755)) ;
#48975 = CARTESIAN_POINT('Ctrl Pts',(-0.395501569538245,0.938665130084104,
-2.86232262158413)) ;
#48976 = CARTESIAN_POINT('Ctrl Pts',(-0.514915155885511,0.878844629487194,
-2.84835143361631)) ;
#48977 = CARTESIAN_POINT('Ctrl Pts',(-0.725575354948663,0.715278209202896,
-2.82066376105321)) ;
#48978 = CARTESIAN_POINT('Ctrl Pts',(-0.814101920087096,0.612561823008408,
-2.80739041821926)) ;
#48979 = CARTESIAN_POINT('Ctrl Pts',(-0.943242638055044,0.383332661133499,
-2.78336947010249)) ;
#48980 = CARTESIAN_POINT('Ctrl Pts',(-0.984405913632964,0.259916848341857,
-2.77043671402726)) ;
#48981 = CARTESIAN_POINT('Ctrl Pts',(-1.01879134190542,-0.00056030937650664,
-2.74314128512119)) ;
#48982 = CARTESIAN_POINT('Ctrl Pts',(-1.00974735449863,-0.135484342474438,
-2.72900258142292)) ;
#48983 = CARTESIAN_POINT('Ctrl Pts',(-0.940234363958862,-0.391410312108166,
-2.70218407199758)) ;
#48984 = CARTESIAN_POINT('Ctrl Pts',(-0.881505880054271,-0.510078366429226,
-2.69063853006172)) ;
#48985 = CARTESIAN_POINT('Ctrl Pts',(-0.722297327848802,-0.717869274875705,
-2.66530299603511)) ;
#48986 = CARTESIAN_POINT('Ctrl Pts',(-0.623598107285679,-0.805077049722201,
-2.65177669759113)) ;
#48987 = CARTESIAN_POINT('Ctrl Pts',(-0.3942196666315,-0.939661430427828,
-2.62390884337232)) ;
#48988 = CARTESIAN_POINT('Ctrl Pts',(-0.264682712776882,-0.984044703498763,
-2.60982778510897)) ;
#48989 = CARTESIAN_POINT('Ctrl Pts',(-0.0869379197352431,-1.00715194062447,
-2.59248658138664)) ;
#48990 = CARTESIAN_POINT('Ctrl Pts',(-0.0434531465249614,-1.00995540144762,
-2.58839341187931)) ;
#48991 = CARTESIAN_POINT('Ctrl Pts',(-1.30495226312157E-12,-1.00995540144768,
-2.58445000000013)) ;
#48992 = CARTESIAN_POINT('Ctrl Pts',(-1.59255949056786E-12,-1.00995540144768,
-2.50507500000015)) ;
#48993 = CARTESIAN_POINT('Ctrl Pts',(-0.0407512997854664,-1.00995540144761,
-2.50877321687317)) ;
#48994 = CARTESIAN_POINT('Ctrl Pts',(-0.0815351550368437,-1.00748961985067,
-2.51260358294113)) ;
#48995 = CARTESIAN_POINT('Ctrl Pts',(-0.256866013574687,-0.986128640680006,
-2.52963422467212)) ;
#48996 = CARTESIAN_POINT('Ctrl Pts',(-0.386850863150314,-0.94273375662927,
-2.54370414317743)) ;
#48997 = CARTESIAN_POINT('Ctrl Pts',(-0.617437752611531,-0.809827169270702,
-2.57159375713428)) ;
#48998 = CARTESIAN_POINT('Ctrl Pts',(-0.716871073866336,-0.723305240324533,
-2.58515074093984)) ;
#48999 = CARTESIAN_POINT('Ctrl Pts',(-0.877535087260389,-0.51681926064045,
-2.61054998755848)) ;
#49000 = CARTESIAN_POINT('Ctrl Pts',(-0.937073888388738,-0.398836931707255,
-2.62203083574432)) ;
#49001 = CARTESIAN_POINT('Ctrl Pts',(-1.00863620516127,-0.143621265000624,
-2.64877491245081)) ;
#49002 = CARTESIAN_POINT('Ctrl Pts',(-1.01876795823122,-0.00866770045745644,
-2.66291671075234)) ;
#49003 = CARTESIAN_POINT('Ctrl Pts',(-0.986405822868516,0.252272244201552,
-2.69026063515088)) ;
#49004 = CARTESIAN_POINT('Ctrl Pts',(-0.946163613771282,0.376098738647618,
-2.70323642660011)) ;
#49005 = CARTESIAN_POINT('Ctrl Pts',(-0.818696660596608,0.606415026005344,
-2.72737129471121)) ;
#49006 = CARTESIAN_POINT('Ctrl Pts',(-0.730933873857989,0.709802076579438,
-2.74051554841513)) ;
#49007 = CARTESIAN_POINT('Ctrl Pts',(-0.521431255058484,0.875008802219531,
-2.76818411342067)) ;
#49008 = CARTESIAN_POINT('Ctrl Pts',(-0.402375462284226,0.93575218806119,
-2.7821711859232)) ;
#49009 = CARTESIAN_POINT('Ctrl Pts',(-0.151367539074259,1.00677805587719,
-2.80867178336935)) ;
#49010 = CARTESIAN_POINT('Ctrl Pts',(-0.0223214203910232,1.0178403111084,
-2.82013618089321)) ;
#49011 = CARTESIAN_POINT('Ctrl Pts',(0.239080785844768,0.990415501805717,
-2.84529558904638)) ;
#49012 = CARTESIAN_POINT('Ctrl Pts',(0.368582276889177,0.949841350688537,
-2.85917384988181)) ;
#49013 = CARTESIAN_POINT('Ctrl Pts',(0.600940525489778,0.822185057368149,
-2.88694912682977)) ;
#49014 = CARTESIAN_POINT('Ctrl Pts',(0.702295931496101,0.737510000342818,
-2.90058377459226)) ;
#49015 = CARTESIAN_POINT('Ctrl Pts',(0.866796281121525,0.534492162085355,
-2.92614945869881)) ;
#49016 = CARTESIAN_POINT('Ctrl Pts',(0.928465926229044,0.418298181480813,
-2.93749148932227)) ;
#49017 = CARTESIAN_POINT('Ctrl Pts',(1.00540024146006,0.164982481451587,-2.96403646831969)) ;
#49018 = CARTESIAN_POINT('Ctrl Pts',(1.01839847450756,0.0299925703233738,
-2.97818207538372)) ;
#49019 = CARTESIAN_POINT('Ctrl Pts',(0.991383041591425,-0.232089948657272,
-3.00564573026626)) ;
#49020 = CARTESIAN_POINT('Ctrl Pts',(0.953582303138476,-0.356963626180555,
-3.01873125614091)) ;
#49021 = CARTESIAN_POINT('Ctrl Pts',(0.830184473602272,-0.590795883260668,
-3.04323456309107)) ;
#49022 = CARTESIAN_POINT('Ctrl Pts',(0.74380025283825,-0.696468175413241,
-3.05614928256783)) ;
#49023 = CARTESIAN_POINT('Ctrl Pts',(0.53638651456345,-0.865955791938646,
-3.08385257730334)) ;
#49024 = CARTESIAN_POINT('Ctrl Pts',(0.418185055368803,-0.928825093038498,
-3.09787350571241)) ;
#49025 = CARTESIAN_POINT('Ctrl Pts',(0.196555780740535,-0.99556386004186,
-3.12148334167159)) ;
#49026 = CARTESIAN_POINT('Ctrl Pts',(0.0984934115873061,-1.00995540144788,
-3.13113663487926)) ;
#49027 = CARTESIAN_POINT('Ctrl Pts',(-2.04213499873386E-12,-1.00995540144768,
-3.14007500000019)) ;
#49028 = CARTESIAN_POINT('Origin',(0.,0.,-3.85445)) ;
#49029 = CARTESIAN_POINT('',(-9.39890130376564E-14,-1.4224,-0.361950000000022)) ;
#49030 = CARTESIAN_POINT('',(-3.86032956577361E-14,-1.4224,-0.282575000000003)) ;
#49031 = CARTESIAN_POINT('',(-1.7419376071072E-16,-1.4224,-3.85445)) ;
#49032 = CARTESIAN_POINT('',(-0.61037374420954,1.28478233657676,4.2165369315862E-15)) ;
#49033 = CARTESIAN_POINT('Ctrl Pts',(-1.8627460685039E-13,-1.42240000000001,
-0.361950000000022)) ;
#49034 = CARTESIAN_POINT('Ctrl Pts',(0.111298535710606,-1.42240000000002,
-0.354778321478478)) ;
#49035 = CARTESIAN_POINT('Ctrl Pts',(0.222425028327351,-1.40934324081798,
-0.347131986267857)) ;
#49036 = CARTESIAN_POINT('Ctrl Pts',(0.514567345684877,-1.33940677840386,
-0.325705580050659)) ;
#49037 = CARTESIAN_POINT('Ctrl Pts',(0.687411639031778,-1.25946111472812,
-0.311593944576295)) ;
#49038 = CARTESIAN_POINT('Ctrl Pts',(0.98610208539558,-1.04103646075053,-0.284221486138232)) ;
#49039 = CARTESIAN_POINT('Ctrl Pts',(1.11078307209736,-0.90683609548697,-0.271194917352188)) ;
#49040 = CARTESIAN_POINT('Ctrl Pts',(1.30756113063591,-0.591354007382843,
-0.246778560086278)) ;
#49041 = CARTESIAN_POINT('Ctrl Pts',(1.3748864251228,-0.411299926504309,-0.233802673102993)) ;
#49042 = CARTESIAN_POINT('Ctrl Pts',(1.43399509839727,-0.0393545326910181,
-0.206128164634742)) ;
#49043 = CARTESIAN_POINT('Ctrl Pts',(1.42682973307147,0.148502360842787,-0.192150717199191)) ;
#49044 = CARTESIAN_POINT('Ctrl Pts',(1.34187381087908,0.505104411187508,-0.165617826548542)) ;
#49045 = CARTESIAN_POINT('Ctrl Pts',(1.26710869380764,0.670945919027301,-0.154053821330338)) ;
#49046 = CARTESIAN_POINT('Ctrl Pts',(1.0547168948564,0.972856235825795,-0.129136272829856)) ;
#49047 = CARTESIAN_POINT('Ctrl Pts',(0.916425588485012,1.10408702592583,-0.11534317911779)) ;
#49048 = CARTESIAN_POINT('Ctrl Pts',(0.600759469129882,1.30237482232973,-0.0876260082340457)) ;
#49049 = CARTESIAN_POINT('Ctrl Pts',(0.427364010981002,1.36911390156539,-0.0739701740617537)) ;
#49050 = CARTESIAN_POINT('Ctrl Pts',(0.104084296066816,1.42588999826873,-0.0510269825442286)) ;
#49051 = CARTESIAN_POINT('Ctrl Pts',(-0.0407736404990986,1.42910084743681,
-0.042071980300692)) ;
#49052 = CARTESIAN_POINT('Ctrl Pts',(-0.331656935595464,1.39121979999024,
-0.0219192387223242)) ;
#49053 = CARTESIAN_POINT('Ctrl Pts',(-0.475640265106083,1.34879144984809,
-0.0110630336517518)) ;
#49054 = CARTESIAN_POINT('Ctrl Pts',(-0.610373744210755,1.28478233657617,
9.84542308790637E-14)) ;
#49055 = CARTESIAN_POINT('',(-1.7419376071072E-16,-1.42240000000001,-6.43033109173613E-17)) ;
#49056 = CARTESIAN_POINT('Origin',(0.,-5.51039363524674E-15,0.)) ;
#49057 = CARTESIAN_POINT('',(-1.7419376071072E-16,-1.42240000000001,0.240832122829321)) ;
#49058 = CARTESIAN_POINT('',(-1.7419376071072E-16,-1.4224,-3.85445)) ;
#49059 = CARTESIAN_POINT('',(2.51958832456576E-16,1.4224,0.240832122829325)) ;
#49060 = CARTESIAN_POINT('Origin',(0.,-5.85469173142172E-15,0.240832122829323)) ;
#49061 = CARTESIAN_POINT('Origin',(0.,-5.85469173142172E-15,0.240832122829323)) ;
#49062 = CARTESIAN_POINT('',(0.491435946297416,1.33480802765296,2.84791806270966E-16)) ;
#49063 = CARTESIAN_POINT('Origin',(0.,-5.51039363524674E-15,0.)) ;
#49064 = CARTESIAN_POINT('Ctrl Pts',(0.491435946296152,1.33480802765341,1.05343251483037E-13)) ;
#49065 = CARTESIAN_POINT('Ctrl Pts',(0.630545413774582,1.28359212890788,-0.010869068609717)) ;
#49066 = CARTESIAN_POINT('Ctrl Pts',(0.760787091978431,1.21094929767397,-0.0219638615839183)) ;
#49067 = CARTESIAN_POINT('Ctrl Pts',(0.991591616538777,1.03004741261812,-0.0435660583179642)) ;
#49068 = CARTESIAN_POINT('Ctrl Pts',(1.09140420456731,0.923638070437862,-0.0539563044444758)) ;
#49069 = CARTESIAN_POINT('Ctrl Pts',(1.27528865898732,0.655250544555112,-0.0757898142532674)) ;
#49070 = CARTESIAN_POINT('Ctrl Pts',(1.34798998887735,0.488534773976204,-0.0874756864601226)) ;
#49071 = CARTESIAN_POINT('Ctrl Pts',(1.4285974262233,0.130728153192531,-0.114098202887478)) ;
#49072 = CARTESIAN_POINT('Ctrl Pts',(1.43341466563187,-0.0574392600133656,
-0.128098754465297)) ;
#49073 = CARTESIAN_POINT('Ctrl Pts',(1.36966067712458,-0.428014838436086,
-0.155671342145558)) ;
#49074 = CARTESIAN_POINT('Ctrl Pts',(1.30050273368294,-0.606469701281969,
-0.168420717677134)) ;
#49075 = CARTESIAN_POINT('Ctrl Pts',(1.10056528640145,-0.919249254739077,
-0.192940113900507)) ;
#49076 = CARTESIAN_POINT('Ctrl Pts',(0.974236166010392,-1.05218422456176,
-0.206025806787986)) ;
#49077 = CARTESIAN_POINT('Ctrl Pts',(0.672712781348542,-1.26740553763213,
-0.233461637702227)) ;
#49078 = CARTESIAN_POINT('Ctrl Pts',(0.498736738258435,-1.34541282634434,
-0.247574086907735)) ;
#49079 = CARTESIAN_POINT('Ctrl Pts',(0.211118407590415,-1.41064129264867,
-0.268533834981004)) ;
#49080 = CARTESIAN_POINT('Ctrl Pts',(0.105619496935363,-1.42240000000001,
-0.275769258371951)) ;
#49081 = CARTESIAN_POINT('Ctrl Pts',(-7.629313847346E-14,-1.4224,-0.282575000000003)) ;
#49082 = CARTESIAN_POINT('Origin',(0.,0.,-3.85445)) ;
#49083 = CARTESIAN_POINT('',(-3.94675305142138E-13,-1.4224,-0.996950000000061)) ;
#49084 = CARTESIAN_POINT('',(-3.54056087750793E-13,-1.4224,-0.917575000000045)) ;
#49085 = CARTESIAN_POINT('',(-1.7419376071072E-16,-1.4224,-3.85445)) ;
#49086 = CARTESIAN_POINT('Ctrl Pts',(-7.89299181569447E-13,-1.4224,-0.996950000000061)) ;
#49087 = CARTESIAN_POINT('Ctrl Pts',(0.138490439042576,-1.42240000000008,
-0.988026172738694)) ;
#49088 = CARTESIAN_POINT('Ctrl Pts',(0.276447863211548,-1.40218515201483,
-0.978384650568776)) ;
#49089 = CARTESIAN_POINT('Ctrl Pts',(0.589172730868239,-1.30815485863121,
-0.954735630741571)) ;
#49090 = CARTESIAN_POINT('Ctrl Pts',(0.756323997591869,-1.21916477894938,
-0.940654359677707)) ;
#49091 = CARTESIAN_POINT('Ctrl Pts',(1.04118398257388,-0.985806550942943,
-0.913617522064665)) ;
#49092 = CARTESIAN_POINT('Ctrl Pts',(1.15779642989958,-0.845761976126516,
-0.901128718461797)) ;
#49093 = CARTESIAN_POINT('Ctrl Pts',(1.33634013558368,-0.522535401145264,
-0.877079122109026)) ;
#49094 = CARTESIAN_POINT('Ctrl Pts',(1.39378321370383,-0.340844339738977,
-0.863560441944868)) ;
#49095 = CARTESIAN_POINT('Ctrl Pts',(1.43408603973681,0.0309190917051568,
-0.83589947234337)) ;
#49096 = CARTESIAN_POINT('Ctrl Pts',(1.4178689094259,0.217297970420088,-0.822031996248509)) ;
#49097 = CARTESIAN_POINT('Ctrl Pts',(1.31608556407904,0.569086032652425,-0.795857289237174)) ;
#49098 = CARTESIAN_POINT('Ctrl Pts',(1.23316536904834,0.731597852345015,-0.784610238875787)) ;
#49099 = CARTESIAN_POINT('Ctrl Pts',(1.00496559334499,1.02446254272169,-0.759010599881342)) ;
#49100 = CARTESIAN_POINT('Ctrl Pts',(0.85897615547451,1.14961402324307,-0.744947630972062)) ;
#49101 = CARTESIAN_POINT('Ctrl Pts',(0.532802075597663,1.33149312522466,-0.717163807294967)) ;
#49102 = CARTESIAN_POINT('Ctrl Pts',(0.357114356937224,1.38897378137191,-0.703704703458175)) ;
#49103 = CARTESIAN_POINT('Ctrl Pts',(-0.00803848792455285,1.43432846886466,
-0.678488261221506)) ;
#49104 = CARTESIAN_POINT('Ctrl Pts',(-0.19404801621122,1.4211685444779,-0.666900428619501)) ;
#49105 = CARTESIAN_POINT('Ctrl Pts',(-0.553888915392507,1.32355145238789,
-0.640081983228383)) ;
#49106 = CARTESIAN_POINT('Ctrl Pts',(-0.723807732144668,1.23882000565941,
-0.625980812450659)) ;
#49107 = CARTESIAN_POINT('Ctrl Pts',(-1.01525839104091,1.01253198536406,-0.598782324005604)) ;
#49108 = CARTESIAN_POINT('Ctrl Pts',(-1.13575754288611,0.87525115937958,-0.585910617188293)) ;
#49109 = CARTESIAN_POINT('Ctrl Pts',(-1.32260332165737,0.556323100980893,
-0.562006062113505)) ;
#49110 = CARTESIAN_POINT('Ctrl Pts',(-1.38468770998822,0.376176269307061,
-0.548689305752013)) ;
#49111 = CARTESIAN_POINT('Ctrl Pts',(-1.43446967338425,0.0049378442003703,
-0.521067399122051)) ;
#49112 = CARTESIAN_POINT('Ctrl Pts',(-1.42285680566885,-0.18224902394239,
-0.507139804766191)) ;
#49113 = CARTESIAN_POINT('Ctrl Pts',(-1.32964842080824,-0.536520346692677,
-0.480780331347271)) ;
#49114 = CARTESIAN_POINT('Ctrl Pts',(-1.25091890948545,-0.700718690590934,
-0.469402991695923)) ;
#49115 = CARTESIAN_POINT('Ctrl Pts',(-1.03128016295316,-0.997669939516361,
-0.444202965013257)) ;
#49116 = CARTESIAN_POINT('Ctrl Pts',(-0.889888612725,-1.12558983710324,-0.430333275789189)) ;
#49117 = CARTESIAN_POINT('Ctrl Pts',(-0.569929244260177,-1.31609920673526,
-0.402628839324504)) ;
#49118 = CARTESIAN_POINT('Ctrl Pts',(-0.395427283560689,-1.37862152606662,
-0.389058579604145)) ;
#49119 = CARTESIAN_POINT('Ctrl Pts',(-0.1429041702682,-1.41702069898609,-0.371358355079311)) ;
#49120 = CARTESIAN_POINT('Ctrl Pts',(-0.071429659967184,-1.4224,-0.366552671139539)) ;
#49121 = CARTESIAN_POINT('Ctrl Pts',(-1.87803832314602E-13,-1.4224,-0.361950000000022)) ;
#49122 = CARTESIAN_POINT('Ctrl Pts',(-7.70323975547614E-14,-1.4224,-0.282575000000003)) ;
#49123 = CARTESIAN_POINT('Ctrl Pts',(-0.0766515080990486,-1.4224,-0.287514148307451)) ;
#49124 = CARTESIAN_POINT('Ctrl Pts',(-0.153336559359331,-1.41620565310975,
-0.292685902468706)) ;
#49125 = CARTESIAN_POINT('Ctrl Pts',(-0.410801712877122,-1.37414531980365,
-0.310840778226794)) ;
#49126 = CARTESIAN_POINT('Ctrl Pts',(-0.584784575647485,-1.30959465944419,
-0.324453048253729)) ;
#49127 = CARTESIAN_POINT('Ctrl Pts',(-0.902704858683785,-1.1153355597406,
-0.352165592252209)) ;
#49128 = CARTESIAN_POINT('Ctrl Pts',(-1.0426166693825,-0.985815050294616,
-0.365999478939528)) ;
#49129 = CARTESIAN_POINT('Ctrl Pts',(-1.25877749321241,-0.686471765330182,
-0.391064390191158)) ;
#49130 = CARTESIAN_POINT('Ctrl Pts',(-1.33560136498211,-0.521489468493963,
-0.402523700260881)) ;
#49131 = CARTESIAN_POINT('Ctrl Pts',(-1.42485964644578,-0.166095250881975,
-0.428966722404629)) ;
#49132 = CARTESIAN_POINT('Ctrl Pts',(-1.43434534633753,0.0214255174811284,
-0.442919160526883)) ;
#49133 = CARTESIAN_POINT('Ctrl Pts',(-1.38021362042203,0.392280885279827,
-0.470512565869048)) ;
#49134 = CARTESIAN_POINT('Ctrl Pts',(-1.31602914390531,0.571717792568198,
-0.48362739773375)) ;
#49135 = CARTESIAN_POINT('Ctrl Pts',(-1.12532984702983,0.888661237299554,
-0.507706427342653)) ;
#49136 = CARTESIAN_POINT('Ctrl Pts',(-1.0030572463384,1.02465806853115,-0.520644641182039)) ;
#49137 = CARTESIAN_POINT('Ctrl Pts',(-0.708527416893833,1.24765681252985,
-0.54791917142539)) ;
#49138 = CARTESIAN_POINT('Ctrl Pts',(-0.537358694150998,1.3303814462102,-0.562026223439437)) ;
#49139 = CARTESIAN_POINT('Ctrl Pts',(-0.176621872539829,1.42336780874833,
-0.588730124694257)) ;
#49140 = CARTESIAN_POINT('Ctrl Pts',(0.00896772525145244,1.43425304753575,
-0.600211886466829)) ;
#49141 = CARTESIAN_POINT('Ctrl Pts',(0.37324274971134,1.38475438273334,-0.62552593092722)) ;
#49142 = CARTESIAN_POINT('Ctrl Pts',(0.548449899820525,1.3251536036109,-0.639032942272491)) ;
#49143 = CARTESIAN_POINT('Ctrl Pts',(0.872818184805203,1.13917930206659,-0.666852758176575)) ;
#49144 = CARTESIAN_POINT('Ctrl Pts',(1.0174569118179,1.01210235889192,-0.680900323917004)) ;
#49145 = CARTESIAN_POINT('Ctrl Pts',(1.24203209642853,0.716392979516036,-0.70637223646316)) ;
#49146 = CARTESIAN_POINT('Ctrl Pts',(1.32287794180158,0.553052690241605,-0.717675246261794)) ;
#49147 = CARTESIAN_POINT('Ctrl Pts',(1.42043614557811,0.200033258872139,-0.743941573000593)) ;
#49148 = CARTESIAN_POINT('Ctrl Pts',(1.43438716284087,0.0132420522884449,
-0.757839728252355)) ;
#49149 = CARTESIAN_POINT('Ctrl Pts',(1.38942345652445,-0.358191594568931,
-0.785476160310195)) ;
#49150 = CARTESIAN_POINT('Ctrl Pts',(1.32972765238025,-0.539134749180973,
-0.798939192647401)) ;
#49151 = CARTESIAN_POINT('Ctrl Pts',(1.14710471396944,-0.860241339444908,
-0.822831052042039)) ;
#49152 = CARTESIAN_POINT('Ctrl Pts',(1.02861183173671,-0.998953723303938,
-0.835541732495152)) ;
#49153 = CARTESIAN_POINT('Ctrl Pts',(0.740439034756506,-1.22891366174676,
-0.862665611370588)) ;
#49154 = CARTESIAN_POINT('Ctrl Pts',(0.571917163271546,-1.31582532470112,
-0.876757877239372)) ;
#49155 = CARTESIAN_POINT('Ctrl Pts',(0.26383719547491,-1.40399825710552,-0.89988968860181)) ;
#49156 = CARTESIAN_POINT('Ctrl Pts',(0.132134173369461,-1.42240000000007,
-0.909060747704911)) ;
#49157 = CARTESIAN_POINT('Ctrl Pts',(-7.07073288808147E-13,-1.4224,-0.917575000000044)) ;
#49158 = CARTESIAN_POINT('Origin',(0.,0.,-3.85445)) ;
#49159 = CARTESIAN_POINT('',(-1.60066293321176E-13,-1.4224,-1.63195000000003)) ;
#49160 = CARTESIAN_POINT('',(-2.51750103553702E-13,-1.4224,-1.55257500000003)) ;
#49161 = CARTESIAN_POINT('',(-1.7419376071072E-16,-1.4224,-3.85445)) ;
#49162 = CARTESIAN_POINT('Ctrl Pts',(-3.2012587025676E-13,-1.4224,-1.63195000000003)) ;
#49163 = CARTESIAN_POINT('Ctrl Pts',(0.164881985030532,-1.42240000000004,
-1.62132559615605)) ;
#49164 = CARTESIAN_POINT('Ctrl Pts',(0.328691648287487,-1.39374152513343,
-1.6097041253823)) ;
#49165 = CARTESIAN_POINT('Ctrl Pts',(0.659540634365683,-1.27397920574445,
-1.58392995972348)) ;
#49166 = CARTESIAN_POINT('Ctrl Pts',(0.82075061318887,-1.17660021785233,-1.56991943658728)) ;
#49167 = CARTESIAN_POINT('Ctrl Pts',(1.09180355217349,-0.929358504128813,
-1.54325577678126)) ;
#49168 = CARTESIAN_POINT('Ctrl Pts',(1.20066148032662,-0.783659607315106,
-1.53150800649667)) ;
#49169 = CARTESIAN_POINT('Ctrl Pts',(1.36192384265765,-0.451701405943932,
-1.50680873556131)) ;
#49170 = CARTESIAN_POINT('Ctrl Pts',(1.40977001143865,-0.267177756656906,
-1.49307929737031)) ;
#49171 = CARTESIAN_POINT('Ctrl Pts',(1.43042550283623,0.105327707786318,-1.46536311698019)) ;
#49172 = CARTESIAN_POINT('Ctrl Pts',(1.40474881606367,0.289672845219077,-1.45164696092121)) ;
#49173 = CARTESIAN_POINT('Ctrl Pts',(1.28519639268473,0.636117224237128,-1.42586984938713)) ;
#49174 = CARTESIAN_POINT('Ctrl Pts',(1.19333408738696,0.795190957391867,-1.41467783900172)) ;
#49175 = CARTESIAN_POINT('Ctrl Pts',(0.949750264870148,1.07567253057638,-1.3885475886414)) ;
#49176 = CARTESIAN_POINT('Ctrl Pts',(0.798252200174296,1.19242237829718,-1.37444222431765)) ;
#49177 = CARTESIAN_POINT('Ctrl Pts',(0.464909851826147,1.35656953071848,-1.34685617386845)) ;
#49178 = CARTESIAN_POINT('Ctrl Pts',(0.287449888658176,1.40492952543529,-1.33362218327198)) ;
#49179 = CARTESIAN_POINT('Ctrl Pts',(-0.0813378461720174,1.43239880238503,
-1.30883690161707)) ;
#49180 = CARTESIAN_POINT('Ctrl Pts',(-0.269258227072101,1.40922494832518,
-1.29660982212353)) ;
#49181 = CARTESIAN_POINT('Ctrl Pts',(-0.62488010447269,1.29140534928586,-1.26931165400671)) ;
#49182 = CARTESIAN_POINT('Ctrl Pts',(-0.789088546257153,1.19814072133656,
-1.25526098465583)) ;
#49183 = CARTESIAN_POINT('Ctrl Pts',(-1.06700509992195,0.957745862977114,
-1.22840977745451)) ;
#49184 = CARTESIAN_POINT('Ctrl Pts',(-1.17970267483513,0.814880028955586,
-1.21633095453539)) ;
#49185 = CARTESIAN_POINT('Ctrl Pts',(-1.34961355640419,0.48724073148818,-1.19195303061668)) ;
#49186 = CARTESIAN_POINT('Ctrl Pts',(-1.40227146194422,0.304066594710712,
-1.17832400258265)) ;
#49187 = CARTESIAN_POINT('Ctrl Pts',(-1.43273619922414,-0.0681992273537915,
-1.15062565272666)) ;
#49188 = CARTESIAN_POINT('Ctrl Pts',(-1.41176366016459,-0.253619377378095,
-1.13682951061175)) ;
#49189 = CARTESIAN_POINT('Ctrl Pts',(-1.30107757466342,-0.602763451894885,
-1.11085152887688)) ;
#49190 = CARTESIAN_POINT('Ctrl Pts',(-1.21372293416922,-0.763544300903012,
-1.09966895414397)) ;
#49191 = CARTESIAN_POINT('Ctrl Pts',(-0.977842841259858,-1.05029117924816,
-1.07380202022439)) ;
#49192 = CARTESIAN_POINT('Ctrl Pts',(-0.829056791780556,-1.1712941195999,
-1.05971318326355)) ;
#49193 = CARTESIAN_POINT('Ctrl Pts',(-0.499201735540026,-1.3443902776224,
-1.03201891709671)) ;
#49194 = CARTESIAN_POINT('Ctrl Pts',(-0.322574355104637,-1.397341407866,-1.018667773973)) ;
#49195 = CARTESIAN_POINT('Ctrl Pts',(-0.0938794309099291,-1.42007914263267,
-1.00308559529349)) ;
#49196 = CARTESIAN_POINT('Ctrl Pts',(-0.0469146980627795,-1.42239999999998,
-0.999973014905758)) ;
#49197 = CARTESIAN_POINT('Ctrl Pts',(-7.89176416523566E-13,-1.4224,-0.996950000000061)) ;
#49198 = CARTESIAN_POINT('Ctrl Pts',(-7.07937981740876E-13,-1.4224,-0.917575000000045)) ;
#49199 = CARTESIAN_POINT('Ctrl Pts',(-0.05257531648526,-1.42239999999998,
-0.920962764857756)) ;
#49200 = CARTESIAN_POINT('Ctrl Pts',(-0.105204870776728,-1.41948537921627,
-0.924462455437981)) ;
#49201 = CARTESIAN_POINT('Ctrl Pts',(-0.339486074083204,-1.39335758485412,
-0.940530712199415)) ;
#49202 = CARTESIAN_POINT('Ctrl Pts',(-0.515668509642552,-1.33819051813931,
-0.953935622783672)) ;
#49203 = CARTESIAN_POINT('Ctrl Pts',(-0.843752765407469,-1.16079183426805,
-0.981675849123684)) ;
#49204 = CARTESIAN_POINT('Ctrl Pts',(-0.99118575839903,-1.0377534239264,-0.995753224306534)) ;
#49205 = CARTESIAN_POINT('Ctrl Pts',(-1.22331892209086,-0.748006330871561,
-1.0214903346745)) ;
#49206 = CARTESIAN_POINT('Ctrl Pts',(-1.30850322480121,-0.586384969788804,
-1.03269516593834)) ;
#49207 = CARTESIAN_POINT('Ctrl Pts',(-1.41485427775941,-0.235945092460195,
-1.05876956157291)) ;
#49208 = CARTESIAN_POINT('Ctrl Pts',(-1.43351483611111,-0.0500429157401591,
-1.07260156876934)) ;
#49209 = CARTESIAN_POINT('Ctrl Pts',(-1.39825729120866,0.322010964809946,
-1.10028414916741)) ;
#49210 = CARTESIAN_POINT('Ctrl Pts',(-1.34326309578732,0.504478797596535,
-1.11386062482118)) ;
#49211 = CARTESIAN_POINT('Ctrl Pts',(-1.16914223240554,0.829978719281117,
-1.13807936899414)) ;
#49212 = CARTESIAN_POINT('Ctrl Pts',(-1.05454617871205,0.971468160551696,
-1.15034808780115)) ;
#49213 = CARTESIAN_POINT('Ctrl Pts',(-0.773254992445382,1.20845733692516,
-1.17729004474716)) ;
#49214 = CARTESIAN_POINT('Ctrl Pts',(-0.607604626552341,1.29965838567566,
-1.19135685645734)) ;
#49215 = CARTESIAN_POINT('Ctrl Pts',(-0.250897438895581,1.4125107507511,-1.21854016514491)) ;
#49216 = CARTESIAN_POINT('Ctrl Pts',(-0.0634571043303167,1.43320730400484,
-1.23058399431525)) ;
#49217 = CARTESIAN_POINT('Ctrl Pts',(0.304465698032599,1.40136852494623,-1.25547609870566)) ;
#49218 = CARTESIAN_POINT('Ctrl Pts',(0.481537650620031,1.35078626936937,-1.26876776068683)) ;
#49219 = CARTESIAN_POINT('Ctrl Pts',(0.813222514640509,1.18230167039937,-1.29640837212861)) ;
#49220 = CARTESIAN_POINT('Ctrl Pts',(0.963423204148111,1.06348716277857,-1.31050694851179)) ;
#49221 = CARTESIAN_POINT('Ctrl Pts',(1.20328783057966,0.779964259574102,-1.33651069193153)) ;
#49222 = CARTESIAN_POINT('Ctrl Pts',(1.29296598630153,0.620069637569694,-1.34768886625226)) ;
#49223 = CARTESIAN_POINT('Ctrl Pts',(1.40824549883862,0.27231592161513,-1.37356339868935)) ;
#49224 = CARTESIAN_POINT('Ctrl Pts',(1.43165952432366,0.0874378248351271,
-1.38731920946167)) ;
#49225 = CARTESIAN_POINT('Ctrl Pts',(1.4062762005124,-0.284984689475835,-1.41502921796695)) ;
#49226 = CARTESIAN_POINT('Ctrl Pts',(1.35610583426426,-0.468874024874967,
-1.42871146018415)) ;
#49227 = CARTESIAN_POINT('Ctrl Pts',(1.19066915502349,-0.798760488338411,
-1.45325658395375)) ;
#49228 = CARTESIAN_POINT('Ctrl Pts',(1.07996781480803,-0.943090859244508,
-1.46515430556019)) ;
#49229 = CARTESIAN_POINT('Ctrl Pts',(0.805613633508822,-1.18705252303244,
-1.49190865991537)) ;
#49230 = CARTESIAN_POINT('Ctrl Pts',(0.642950673153115,-1.28246656113985,
-1.50593970716064)) ;
#49231 = CARTESIAN_POINT('Ctrl Pts',(0.316249096520576,-1.3958894711163,-1.53121078750353)) ;
#49232 = CARTESIAN_POINT('Ctrl Pts',(0.158587883989674,-1.42240000000006,
-1.54235616545629)) ;
#49233 = CARTESIAN_POINT('Ctrl Pts',(-5.03312669319911E-13,-1.4224,-1.55257500000003)) ;
#49234 = CARTESIAN_POINT('Origin',(0.,0.,-3.85445)) ;
#49235 = CARTESIAN_POINT('',(4.08959556090181E-15,-1.4224,-2.26695000000001)) ;
#49236 = CARTESIAN_POINT('',(-1.74193760710719E-16,-1.4224,-2.18757499999999)) ;
#49237 = CARTESIAN_POINT('',(-1.7419376071072E-16,-1.4224,-3.85445)) ;
#49238 = CARTESIAN_POINT('Ctrl Pts',(8.35338488251435E-15,-1.4224,-2.26695000000001)) ;
#49239 = CARTESIAN_POINT('Ctrl Pts',(0.00705824810515262,-1.4224,-2.26649519180319)) ;
#49240 = CARTESIAN_POINT('Ctrl Pts',(0.0141185381379087,-1.42234746325677,
-2.26603829753993)) ;
#49241 = CARTESIAN_POINT('Ctrl Pts',(0.20238837868152,-1.41954371511923,-2.2538025580499)) ;
#49242 = CARTESIAN_POINT('Ctrl Pts',(0.381364936782223,-1.38224015132245,
-2.24088216906958)) ;
#49243 = CARTESIAN_POINT('Ctrl Pts',(0.722111878701266,-1.23983456884393,
-2.21362783133127)) ;
#49244 = CARTESIAN_POINT('Ctrl Pts',(0.879641651811128,-1.13352368170617,
-2.19952215953555)) ;
#49245 = CARTESIAN_POINT('Ctrl Pts',(1.14150362023217,-0.86844369091499,-2.17278710653457)) ;
#49246 = CARTESIAN_POINT('Ctrl Pts',(1.24431409242575,-0.713370649668091,
-2.1612781733384)) ;
#49247 = CARTESIAN_POINT('Ctrl Pts',(1.38467644681224,-0.373504162954386,
-2.13599048831506)) ;
#49248 = CARTESIAN_POINT('Ctrl Pts',(1.42122825231272,-0.192142196309621,
-2.12249629436828)) ;
#49249 = CARTESIAN_POINT('Ctrl Pts',(1.42356155502621,0.181630074663026,-2.09468585753996)) ;
#49250 = CARTESIAN_POINT('Ctrl Pts',(1.38646443566518,0.370488269493329,-2.08063390851984)) ;
#49251 = CARTESIAN_POINT('Ctrl Pts',(1.24381905453741,0.713298253677465,-2.05512721326805)) ;
#49252 = CARTESIAN_POINT('Ctrl Pts',(1.14326175388171,0.86535696644464,-2.04384101479274)) ;
#49253 = CARTESIAN_POINT('Ctrl Pts',(0.887180203460197,1.12718288664927,-2.01759949037251)) ;
#49254 = CARTESIAN_POINT('Ctrl Pts',(0.732792885628689,1.23313983476483,-2.00370947450034)) ;
#49255 = CARTESIAN_POINT('Ctrl Pts',(0.389190744486969,1.38106171658738,-1.97606593849329)) ;
#49256 = CARTESIAN_POINT('Ctrl Pts',(0.202768612285937,1.42046772056397,-1.96258756763748)) ;
#49257 = CARTESIAN_POINT('Ctrl Pts',(-0.166575902046834,1.42411360973044,
-1.93865269585595)) ;
#49258 = CARTESIAN_POINT('Ctrl Pts',(-0.346007778185403,1.39147701313561,
-1.92600409082978)) ;
#49259 = CARTESIAN_POINT('Ctrl Pts',(-0.689597944522936,1.25813706190102,
-1.89890380897293)) ;
#49260 = CARTESIAN_POINT('Ctrl Pts',(-0.849433289927311,1.1562540977711,-1.88481430364497)) ;
#49261 = CARTESIAN_POINT('Ctrl Pts',(-1.1188045432412,0.897749618059628,-1.85784000392214)) ;
#49262 = CARTESIAN_POINT('Ctrl Pts',(-1.22624127259538,0.744307332093111,
-1.84608000982836)) ;
#49263 = CARTESIAN_POINT('Ctrl Pts',(-1.37507900931244,0.407225124304485,
-1.82099948841552)) ;
#49264 = CARTESIAN_POINT('Ctrl Pts',(-1.41598013707408,0.227257966918058,
-1.8076090749195)) ;
#49265 = CARTESIAN_POINT('Ctrl Pts',(-1.42765124254203,-0.14540752582436,
-1.77988098766189)) ;
#49266 = CARTESIAN_POINT('Ctrl Pts',(-1.39547968562878,-0.334652540650194,
-1.76580025739211)) ;
#49267 = CARTESIAN_POINT('Ctrl Pts',(-1.26183834351431,-0.681038000747549,
-1.74002752970629)) ;
#49268 = CARTESIAN_POINT('Ctrl Pts',(-1.16495811008005,-0.836018033780636,
-1.72883052833213)) ;
#49269 = CARTESIAN_POINT('Ctrl Pts',(-0.915543325834338,-1.10419215095865,
-1.7027824183749)) ;
#49270 = CARTESIAN_POINT('Ctrl Pts',(-0.764306362432892,-1.21378811464194,
-1.6889600200146)) ;
#49271 = CARTESIAN_POINT('Ctrl Pts',(-0.431330658955535,-1.36755835010461,
-1.66178364086345)) ;
#49272 = CARTESIAN_POINT('Ctrl Pts',(-0.253175504627166,-1.41145280119291,
-1.64867098348413)) ;
#49273 = CARTESIAN_POINT('Ctrl Pts',(-0.0476886137906572,-1.42180093277766,
-1.635045169987)) ;
#49274 = CARTESIAN_POINT('Ctrl Pts',(-0.0238345165532617,-1.4224,-1.63348581077546)) ;
#49275 = CARTESIAN_POINT('Ctrl Pts',(-3.19958392881641E-13,-1.4224,-1.63195000000003)) ;
#49276 = CARTESIAN_POINT('Ctrl Pts',(-5.03326013346693E-13,-1.4224,-1.55257500000003)) ;
#49277 = CARTESIAN_POINT('Ctrl Pts',(-0.0292793697530499,-1.42239999999999,
-1.55446165759024)) ;
#49278 = CARTESIAN_POINT('Ctrl Pts',(-0.0585860447358915,-1.42149597301951,
-1.5563837065877)) ;
#49279 = CARTESIAN_POINT('Ctrl Pts',(-0.269603865804769,-1.40843387270665,
-1.57046687949346)) ;
#49280 = CARTESIAN_POINT('Ctrl Pts',(-0.44744011881166,-1.36240077891355,
-1.58363855060316)) ;
#49281 = CARTESIAN_POINT('Ctrl Pts',(-0.782456997879084,-1.20280699617351,
-1.6111631056135)) ;
#49282 = CARTESIAN_POINT('Ctrl Pts',(-0.935282858313713,-1.08823109080047,
-1.62527315250176)) ;
#49283 = CARTESIAN_POINT('Ctrl Pts',(-1.18274523279402,-0.810949888412982,
-1.65153426142843)) ;
#49284 = CARTESIAN_POINT('Ctrl Pts',(-1.27689640477158,-0.652732684199964,
-1.66275858004465)) ;
#49285 = CARTESIAN_POINT('Ctrl Pts',(-1.40273768552504,-0.302515682358636,
-1.68881639268165)) ;
#49286 = CARTESIAN_POINT('Ctrl Pts',(-1.43052151306998,-0.113030283103728,
-1.70291500869764)) ;
#49287 = CARTESIAN_POINT('Ctrl Pts',(-1.41056802361381,0.258456000534885,
-1.73055535718265)) ;
#49288 = CARTESIAN_POINT('Ctrl Pts',(-1.36582692532895,0.437092117957235,
-1.74384673496706)) ;
#49289 = CARTESIAN_POINT('Ctrl Pts',(-1.20941761067431,0.771634853533995,
-1.76873830755461)) ;
#49290 = CARTESIAN_POINT('Ctrl Pts',(-1.09776182740402,0.923610562026558,
-1.78078300976017)) ;
#49291 = CARTESIAN_POINT('Ctrl Pts',(-0.821656418115741,1.17608484817488,
-1.80796689678696)) ;
#49292 = CARTESIAN_POINT('Ctrl Pts',(-0.659843409673311,1.27393039077089,
-1.82203363393517)) ;
#49293 = CARTESIAN_POINT('Ctrl Pts',(-0.313952818508723,1.39901801775358,
-1.84897514080793)) ;
#49294 = CARTESIAN_POINT('Ctrl Pts',(-0.134120162014341,1.42750475630256,
-1.86124286862981)) ;
#49295 = CARTESIAN_POINT('Ctrl Pts',(0.23483026846509,1.41552441729608,-1.88546240843901)) ;
#49296 = CARTESIAN_POINT('Ctrl Pts',(0.420346453896695,1.37190502931201,-1.89903915125069)) ;
#49297 = CARTESIAN_POINT('Ctrl Pts',(0.760172461443112,1.21639076140491,-1.92672182158963)) ;
#49298 = CARTESIAN_POINT('Ctrl Pts',(0.911830410768999,1.10727033778187,-1.94055365556386)) ;
#49299 = CARTESIAN_POINT('Ctrl Pts',(1.16212837930198,0.83993220336767,-1.96662757420019)) ;
#49300 = CARTESIAN_POINT('Ctrl Pts',(1.25949542454028,0.685342539624457,-1.97783225151605)) ;
#49301 = CARTESIAN_POINT('Ctrl Pts',(1.39433503064672,0.339427069423941,-2.00357000971548)) ;
#49302 = CARTESIAN_POINT('Ctrl Pts',(1.42716082271295,0.15022630792033,-2.01764744732736)) ;
#49303 = CARTESIAN_POINT('Ctrl Pts',(1.41672756002279,-0.222599408791518,
-2.04538745601127)) ;
#49304 = CARTESIAN_POINT('Ctrl Pts',(1.37640177539242,-0.402757885947333,
-2.05879210460918)) ;
#49305 = CARTESIAN_POINT('Ctrl Pts',(1.22869104674956,-0.740213868060773,
-2.08390043661167)) ;
#49306 = CARTESIAN_POINT('Ctrl Pts',(1.12187530325842,-0.893873509519988,
-2.09562293469196)) ;
#49307 = CARTESIAN_POINT('Ctrl Pts',(0.853504449015797,-1.15326286123838,
-2.12256569163159)) ;
#49308 = CARTESIAN_POINT('Ctrl Pts',(0.693970220958235,-1.255740275215,-2.13665790898719)) ;
#49309 = CARTESIAN_POINT('Ctrl Pts',(0.353622076028277,-1.38916742812599,
-2.1635525307205)) ;
#49310 = CARTESIAN_POINT('Ctrl Pts',(0.177520453174637,-1.4224,-2.17613621859073)) ;
#49311 = CARTESIAN_POINT('Ctrl Pts',(-1.73472347597681E-16,-1.4224,-2.18757499999999)) ;
#49312 = CARTESIAN_POINT('Origin',(0.,0.,-3.85445)) ;
#49313 = CARTESIAN_POINT('',(2.79104006804924E-13,-1.4224,-2.90194999999997)) ;
#49314 = CARTESIAN_POINT('',(1.19211907244443E-13,-1.4224,-2.82257499999998)) ;
#49315 = CARTESIAN_POINT('',(-1.7419376071072E-16,-1.4224,-3.85445)) ;
#49316 = CARTESIAN_POINT('Ctrl Pts',(5.58382207370559E-13,-1.4224,-2.90194999999997)) ;
#49317 = CARTESIAN_POINT('Ctrl Pts',(0.0311347855562209,-1.4224,-2.89994378606897)) ;
#49318 = CARTESIAN_POINT('Ctrl Pts',(0.0622995603867949,-1.42137777228308,
-2.89789761043169)) ;
#49319 = CARTESIAN_POINT('Ctrl Pts',(0.27519485177764,-1.40736126326523,-2.88365795379482)) ;
#49320 = CARTESIAN_POINT('Ctrl Pts',(0.452916575232848,-1.36059958990392,
-2.87046655766408)) ;
#49321 = CARTESIAN_POINT('Ctrl Pts',(0.787415833678526,-1.19957881152357,
-2.84292226863498)) ;
#49322 = CARTESIAN_POINT('Ctrl Pts',(0.939829311069727,-1.08432089525593,
-2.82881342180211)) ;
#49323 = CARTESIAN_POINT('Ctrl Pts',(1.18607923031601,-0.806035459267605,
-2.80259307926183)) ;
#49324 = CARTESIAN_POINT('Ctrl Pts',(1.27951302222529,-0.6475510913556,-2.79138088477348)) ;
#49325 = CARTESIAN_POINT('Ctrl Pts',(1.40211900625454,-0.302048982793983,
-2.76567388264836)) ;
#49326 = CARTESIAN_POINT('Ctrl Pts',(1.4294067606685,-0.118101449897238,-2.75198731026021)) ;
#49327 = CARTESIAN_POINT('Ctrl Pts',(1.41212858153763,0.254426175771634,-2.72426948096937)) ;
#49328 = CARTESIAN_POINT('Ctrl Pts',(1.36594844361767,0.439384554082642,-2.71050769686885)) ;
#49329 = CARTESIAN_POINT('Ctrl Pts',(1.20767557248197,0.772811623871518,-2.68569913512861)) ;
#49330 = CARTESIAN_POINT('Ctrl Pts',(1.10012700707919,0.919492133416788,-2.67404760928657)) ;
#49331 = CARTESIAN_POINT('Ctrl Pts',(0.831425064010638,1.16905521759255,-2.64744907871875)) ;
#49332 = CARTESIAN_POINT('Ctrl Pts',(0.671261647153545,1.26781760859926,-2.63345452639297)) ;
#49333 = CARTESIAN_POINT('Ctrl Pts',(0.318759110331852,1.39915779684059,-2.60585435928681)) ;
#49334 = CARTESIAN_POINT('Ctrl Pts',(0.129508016637823,1.42913284796985,-2.59304551014784)) ;
#49335 = CARTESIAN_POINT('Ctrl Pts',(-0.24154172827379,1.41347133802415,-2.5685537497212)) ;
#49336 = CARTESIAN_POINT('Ctrl Pts',(-0.419906890651167,1.37108939873629,
-2.55548382922917)) ;
#49337 = CARTESIAN_POINT('Ctrl Pts',(-0.757426125987458,1.21866433628123,
-2.52806472481737)) ;
#49338 = CARTESIAN_POINT('Ctrl Pts',(-0.912272533936138,1.10752435050957,
-2.51395230548298)) ;
#49339 = CARTESIAN_POINT('Ctrl Pts',(-1.16578521716074,0.835306996806831,
-2.48748972358525)) ;
#49340 = CARTESIAN_POINT('Ctrl Pts',(-1.26354262584752,0.678416217719143,
-2.47617739715172)) ;
#49341 = CARTESIAN_POINT('Ctrl Pts',(-1.39443401940236,0.335510588952948,
-2.45066358548757)) ;
#49342 = CARTESIAN_POINT('Ctrl Pts',(-1.4260680404596,0.152711926799914,-2.43706249455356)) ;
#49343 = CARTESIAN_POINT('Ctrl Pts',(-1.41794705565271,-0.21972011849095,
-2.409351776898)) ;
#49344 = CARTESIAN_POINT('Ctrl Pts',(-1.37630824974514,-0.4057799169763,-2.39550804189165)) ;
#49345 = CARTESIAN_POINT('Ctrl Pts',(-1.22617739199268,-0.743144079566568,
-2.37040654169892)) ;
#49346 = CARTESIAN_POINT('Ctrl Pts',(-1.12215176235947,-0.892505719027026,
-2.35897076440412)) ;
#49347 = CARTESIAN_POINT('Ctrl Pts',(-0.859797106385966,-1.14827735225385,
-2.33255025744819)) ;
#49348 = CARTESIAN_POINT('Ctrl Pts',(-0.702506433381979,-1.25070748494266,
-2.31860436571127)) ;
#49349 = CARTESIAN_POINT('Ctrl Pts',(-0.361326586308873,-1.38769425018157,
-2.2915237260205)) ;
#49350 = CARTESIAN_POINT('Ctrl Pts',(-0.181419697111433,-1.4224,-2.27864003470577)) ;
#49351 = CARTESIAN_POINT('Ctrl Pts',(8.53483950180589E-15,-1.4224,-2.26695000000001)) ;
#49352 = CARTESIAN_POINT('Ctrl Pts',(-1.74193760710719E-16,-1.4224,-2.18757499999999)) ;
#49353 = CARTESIAN_POINT('Ctrl Pts',(-0.00310549422719388,-1.4224,-2.1877751069116)) ;
#49354 = CARTESIAN_POINT('Ctrl Pts',(-0.00621137440850784,-1.4223898297657,
-2.18797561704965)) ;
#49355 = CARTESIAN_POINT('Ctrl Pts',(-0.198046631073437,-1.42113316446034,
-2.20038354400397)) ;
#49356 = CARTESIAN_POINT('Ctrl Pts',(-0.38459361681943,-1.38234820102978,
-2.21384685578751)) ;
#49357 = CARTESIAN_POINT('Ctrl Pts',(-0.728736496056371,-1.23555032030395,
-2.24148341950132)) ;
#49358 = CARTESIAN_POINT('Ctrl Pts',(-0.883519623551189,-1.13006407827464,
-2.25538142854168)) ;
#49359 = CARTESIAN_POINT('Ctrl Pts',(-1.14044867755491,-0.869051457763149,
-2.28164730636856)) ;
#49360 = CARTESIAN_POINT('Ctrl Pts',(-1.24147395732859,-0.717359988743452,
-2.29295000083755)) ;
#49361 = CARTESIAN_POINT('Ctrl Pts',(-1.38525721567935,-0.375009004575994,
-2.31842254430239)) ;
#49362 = CARTESIAN_POINT('Ctrl Pts',(-1.42297820556566,-0.186208635731148,
-2.33247019079382)) ;
#49363 = CARTESIAN_POINT('Ctrl Pts',(-1.42183065443789,0.187687440960692,
-2.3602898393572)) ;
#49364 = CARTESIAN_POINT('Ctrl Pts',(-1.3858326469319,0.369218569025883,-2.37379661971919)) ;
#49365 = CARTESIAN_POINT('Ctrl Pts',(-1.24654246132111,0.709432919902523,
-2.39911018749276)) ;
#49366 = CARTESIAN_POINT('Ctrl Pts',(-1.14431012112672,0.864711810806592,
-2.41059243085566)) ;
#49367 = CARTESIAN_POINT('Ctrl Pts',(-0.883395687678344,1.13061080258421,
-2.43729689688759)) ;
#49368 = CARTESIAN_POINT('Ctrl Pts',(-0.726164177462196,1.23747476251475,
-2.45140392531674)) ;
#49369 = CARTESIAN_POINT('Ctrl Pts',(-0.385770146025108,1.38102462402414,
-2.47867809267357)) ;
#49370 = CARTESIAN_POINT('Ctrl Pts',(-0.206855967887497,1.4189067249851,-2.49161598507274)) ;
#49371 = CARTESIAN_POINT('Ctrl Pts',(0.162973862078443,1.42556422860031,-2.51569416808132)) ;
#49372 = CARTESIAN_POINT('Ctrl Pts',(0.350460948395063,1.39142050641088,-2.52880995767405)) ;
#49373 = CARTESIAN_POINT('Ctrl Pts',(0.698688059950283,1.25285283966455,-2.55640351111649)) ;
#49374 = CARTESIAN_POINT('Ctrl Pts',(0.856336379803752,1.15086935587789,-2.57035583193125)) ;
#49375 = CARTESIAN_POINT('Ctrl Pts',(1.11947324965008,0.895858284599545,-2.59679844722876)) ;
#49376 = CARTESIAN_POINT('Ctrl Pts',(1.22393218939323,0.746829584895699,-2.60825732255242)) ;
#49377 = CARTESIAN_POINT('Ctrl Pts',(1.37507209273564,0.409948276039682,-2.63332289612801)) ;
#49378 = CARTESIAN_POINT('Ctrl Pts',(1.41727387607924,0.224018429535852,-2.64715696208812)) ;
#49379 = CARTESIAN_POINT('Ctrl Pts',(1.42652621472551,-0.148437749958214,
-2.67486947544333)) ;
#49380 = CARTESIAN_POINT('Ctrl Pts',(1.39542743345201,-0.331383956749282,
-2.688481544401)) ;
#49381 = CARTESIAN_POINT('Ctrl Pts',(1.26556040407222,-0.674613745434463,
-2.71401947510674)) ;
#49382 = CARTESIAN_POINT('Ctrl Pts',(1.16834235645805,-0.831701235349615,
-2.72531580778757)) ;
#49383 = CARTESIAN_POINT('Ctrl Pts',(0.915729788520457,-1.10467757850592,
-2.75174862569883)) ;
#49384 = CARTESIAN_POINT('Ctrl Pts',(0.761180000069932,-1.21633214604863,
-2.76586107560351)) ;
#49385 = CARTESIAN_POINT('Ctrl Pts',(0.424024460116359,-1.36982869321612,
-2.79329660657153)) ;
#49386 = CARTESIAN_POINT('Ctrl Pts',(0.245733458969846,-1.41275541284761,
-2.80638201550567)) ;
#49387 = CARTESIAN_POINT('Ctrl Pts',(0.0427587296775013,-1.4219183587854,
-2.81980186259364)) ;
#49388 = CARTESIAN_POINT('Ctrl Pts',(0.0213712307611172,-1.4224,-2.82119791452758)) ;
#49389 = CARTESIAN_POINT('Ctrl Pts',(2.38598008249596E-13,-1.4224,-2.82257499999998)) ;
#49390 = CARTESIAN_POINT('Origin',(0.,0.,-3.85445)) ;
#49391 = CARTESIAN_POINT('',(1.22356791609788,-0.725329797192901,-3.35280000000001)) ;
#49392 = CARTESIAN_POINT('Ctrl Pts',(2.38351005599213E-13,-1.4224,-2.82257499999998)) ;
#49393 = CARTESIAN_POINT('Ctrl Pts',(-0.167743111464536,-1.4224,-2.83338376457127)) ;
#49394 = CARTESIAN_POINT('Ctrl Pts',(-0.334344174546972,-1.39273727541033,
-2.84522246362053)) ;
#49395 = CARTESIAN_POINT('Ctrl Pts',(-0.667041136862354,-1.27005219390176,
-2.87122443995099)) ;
#49396 = CARTESIAN_POINT('Ctrl Pts',(-0.827583327651127,-1.17178747294409,
-2.88522488459988)) ;
#49397 = CARTESIAN_POINT('Ctrl Pts',(-1.09713364056572,-0.923060689714675,
-2.91184696869191)) ;
#49398 = CARTESIAN_POINT('Ctrl Pts',(-1.20515438702793,-0.776735090525134,
-2.92353221052642)) ;
#49399 = CARTESIAN_POINT('Ctrl Pts',(-1.36450765096001,-0.443837430686508,
-2.94830138164536)) ;
#49400 = CARTESIAN_POINT('Ctrl Pts',(-1.41129001020065,-0.259034280557108,
-2.96205161602999)) ;
#49401 = CARTESIAN_POINT('Ctrl Pts',(-1.42978786909493,0.113488908638944,
-2.98976911522613)) ;
#49402 = CARTESIAN_POINT('Ctrl Pts',(-1.4030814297501,0.297581655368469,-3.00346649221493)) ;
#49403 = CARTESIAN_POINT('Ctrl Pts',(-1.28157828094376,0.643424989524953,
-3.02919888314919)) ;
#49404 = CARTESIAN_POINT('Ctrl Pts',(-1.1887133928311,0.802122054212909,-3.04040275528989)) ;
#49405 = CARTESIAN_POINT('Ctrl Pts',(-0.943427049507034,1.08120312372754,
-3.0665906079147)) ;
#49406 = CARTESIAN_POINT('Ctrl Pts',(-0.791343058130753,1.19700148514056,
-3.08069832969649)) ;
#49407 = CARTESIAN_POINT('Ctrl Pts',(-0.457258970750482,1.35915402133909,
-3.10825797067645)) ;
#49408 = CARTESIAN_POINT('Ctrl Pts',(-0.27963028250354,1.40649395990625,-3.12146488479448)) ;
#49409 = CARTESIAN_POINT('Ctrl Pts',(0.0895500817499499,1.43195430931873,
-3.1462007291939)) ;
#49410 = CARTESIAN_POINT('Ctrl Pts',(0.277693631018515,1.40763447297145,-3.15851789452721)) ;
#49411 = CARTESIAN_POINT('Ctrl Pts',(0.632804233215071,1.28752447428894,-3.18586832622339)) ;
#49412 = CARTESIAN_POINT('Ctrl Pts',(0.796339709168365,1.19331613655909,-3.19991074032015)) ;
#49413 = CARTESIAN_POINT('Ctrl Pts',(1.07269829972026,0.951357858332586,-3.22671972090685)) ;
#49414 = CARTESIAN_POINT('Ctrl Pts',(1.18452190253661,0.807853041441442,-3.23871688679754)) ;
#49415 = CARTESIAN_POINT('Ctrl Pts',(1.35247988444437,0.479229532151915,-3.26316804076252)) ;
#49416 = CARTESIAN_POINT('Ctrl Pts',(1.40405255508825,0.29573873272908,-3.27682063000529)) ;
#49417 = CARTESIAN_POINT('Ctrl Pts',(1.42949530553819,-0.0396614275677127,
-3.30177599907499)) ;
#49418 = CARTESIAN_POINT('Ctrl Pts',(1.41766650813827,-0.187769019916435,
-3.31279590921999)) ;
#49419 = CARTESIAN_POINT('Ctrl Pts',(1.35003538825005,-0.470060262619143,
-3.33379972192108)) ;
#49420 = CARTESIAN_POINT('Ctrl Pts',(1.29618339295294,-0.602833840132126,
-3.34356377781289)) ;
#49421 = CARTESIAN_POINT('Ctrl Pts',(1.22356791609731,-0.725329797193858,
-3.35280000000008)) ;
#49422 = CARTESIAN_POINT('',(1.38082735583561,0.341376000000043,-3.35280000000001)) ;
#49423 = CARTESIAN_POINT('Origin',(0.,-7.17168199644958E-16,-3.35280000000001)) ;
#49424 = CARTESIAN_POINT('Ctrl Pts',(1.380827355836,0.34137599999849,-3.35280000000012)) ;
#49425 = CARTESIAN_POINT('Ctrl Pts',(1.34494946230612,0.486498026315639,-3.34200223018486)) ;
#49426 = CARTESIAN_POINT('Ctrl Pts',(1.28644929427591,0.624961242933701,-3.33201079970659)) ;
#49427 = CARTESIAN_POINT('Ctrl Pts',(1.12759436205324,0.880124714487233,-3.31228206885852)) ;
#49428 = CARTESIAN_POINT('Ctrl Pts',(1.02773415600914,0.994900755466381,-3.30157749328181)) ;
#49429 = CARTESIAN_POINT('Ctrl Pts',(0.767920662584799,1.21186660616474,-3.27676439723266)) ;
#49430 = CARTESIAN_POINT('Ctrl Pts',(0.601792899437461,1.30237154390797,-3.26269272074225)) ;
#49431 = CARTESIAN_POINT('Ctrl Pts',(0.244729405122114,1.413560632934,-3.23554833076054)) ;
#49432 = CARTESIAN_POINT('Ctrl Pts',(0.0574484938757501,1.43343002083784,
-3.22356211797056)) ;
#49433 = CARTESIAN_POINT('Ctrl Pts',(-0.310180545827058,1.40012415083315,
-3.19863436331626)) ;
#49434 = CARTESIAN_POINT('Ctrl Pts',(-0.487115735949317,1.34879474425875,
-3.18532371802188)) ;
#49435 = CARTESIAN_POINT('Ctrl Pts',(-0.818230503166939,1.17885429923585,
-3.15766568063422)) ;
#49436 = CARTESIAN_POINT('Ctrl Pts',(-0.967988546990518,1.05934816381014,
-3.14356989655051)) ;
#49437 = CARTESIAN_POINT('Ctrl Pts',(-1.20659871424787,0.774806463283478,
-3.11760908429534)) ;
#49438 = CARTESIAN_POINT('Ctrl Pts',(-1.2955435602896,0.61463362657052,-3.10643166864363)) ;
#49439 = CARTESIAN_POINT('Ctrl Pts',(-1.40937870005715,0.266440799543008,
-3.08052446425171)) ;
#49440 = CARTESIAN_POINT('Ctrl Pts',(-1.43202599105278,0.0813887985564382,
-3.0667557141783)) ;
#49441 = CARTESIAN_POINT('Ctrl Pts',(-1.40504464208628,-0.290991981533069,
-3.03904881089783)) ;
#49442 = CARTESIAN_POINT('Ctrl Pts',(-1.35409081262042,-0.474660131470722,
-3.02538302593224)) ;
#49443 = CARTESIAN_POINT('Ctrl Pts',(-1.18724577345861,-0.803842203239017,
-3.000890312259)) ;
#49444 = CARTESIAN_POINT('Ctrl Pts',(-1.0759183915845,-0.947711345213575,
-2.98893787104943)) ;
#49445 = CARTESIAN_POINT('Ctrl Pts',(-0.8004455509441,-1.19055603339596,-2.96215298844984)) ;
#49446 = CARTESIAN_POINT('Ctrl Pts',(-0.637294720828622,-1.28529834410964,
-2.94811549448515)) ;
#49447 = CARTESIAN_POINT('Ctrl Pts',(-0.31202552629567,-1.39659904097479,
-2.92301566308883)) ;
#49448 = CARTESIAN_POINT('Ctrl Pts',(-0.156452602692893,-1.4224,-2.91203124467417)) ;
#49449 = CARTESIAN_POINT('Ctrl Pts',(5.58382207370559E-13,-1.4224,-2.90194999999997)) ;
#49450 = CARTESIAN_POINT('Origin',(1.04083408558609E-16,-6.38378239159465E-15,
-4.1322625)) ;
#49451 = CARTESIAN_POINT('',(0.105153794786494,-1.00446632216085,-3.76524459855233)) ;
#49452 = CARTESIAN_POINT('Ctrl Pts',(-2.04213499873386E-12,-1.00995540144768,
-3.14007500000019)) ;
#49453 = CARTESIAN_POINT('Ctrl Pts',(-0.0294481807784787,-1.00995540144762,
-3.14274744872219)) ;
#49454 = CARTESIAN_POINT('Ctrl Pts',(-0.0589227263234698,-1.00866757816801,
-3.14548976563933)) ;
#49455 = CARTESIAN_POINT('Ctrl Pts',(-0.22224974390044,-0.994325948900357,
-3.16106326886646)) ;
#49456 = CARTESIAN_POINT('Ctrl Pts',(-0.352403824776246,-0.955958878606333,
-3.17488511269584)) ;
#49457 = CARTESIAN_POINT('Ctrl Pts',(-0.58707145263758,-0.83217887860383,
-3.20266686928213)) ;
#49458 = CARTESIAN_POINT('Ctrl Pts',(-0.689994926562969,-0.749067644977869,
-3.21636188399988)) ;
#49459 = CARTESIAN_POINT('Ctrl Pts',(-0.85765553496316,-0.548938105493903,
-3.24206303184746)) ;
#49460 = CARTESIAN_POINT('Ctrl Pts',(-0.921076654143625,-0.434195982679694,
-3.25332555705325)) ;
#49461 = CARTESIAN_POINT('Ctrl Pts',(-1.00240386668299,-0.182474912493191,
-3.2797034346208)) ;
#49462 = CARTESIAN_POINT('Ctrl Pts',(-1.01776124772871,-0.0475000472824059,
-3.29384746502155)) ;
#49463 = CARTESIAN_POINT('Ctrl Pts',(-0.995162373102043,0.215439381887664,
-3.32140091561347)) ;
#49464 = CARTESIAN_POINT('Ctrl Pts',(-0.959386467255263,0.341136886974746,
-3.33457277046565)) ;
#49465 = CARTESIAN_POINT('Ctrl Pts',(-0.840090695756902,0.576437934152737,
-3.35922999208551)) ;
#49466 = CARTESIAN_POINT('Ctrl Pts',(-0.756097394197089,0.68293213094862,
-3.37182408423458)) ;
#49467 = CARTESIAN_POINT('Ctrl Pts',(-0.552359595968076,0.855892906106022,
-3.39937576045609)) ;
#49468 = CARTESIAN_POINT('Ctrl Pts',(-0.435123051699683,0.921045071508901,
-3.41342873276919)) ;
#49469 = CARTESIAN_POINT('Ctrl Pts',(-0.186382082707184,1.0008786337726,-3.44018508171057)) ;
#49470 = CARTESIAN_POINT('Ctrl Pts',(-0.0578768782872739,1.01642197753821,
-3.4519838049772)) ;
#49471 = CARTESIAN_POINT('Ctrl Pts',(0.204166864423636,0.998193749791793,
-3.47671957776183)) ;
#49472 = CARTESIAN_POINT('Ctrl Pts',(0.334976010765058,0.962200820461377,
-3.49047647612628)) ;
#49473 = CARTESIAN_POINT('Ctrl Pts',(0.572042398711904,0.842616738883757,
-3.51825607696624)) ;
#49474 = CARTESIAN_POINT('Ctrl Pts',(0.676617624943253,0.76121127136032,-3.53201161597671)) ;
#49475 = CARTESIAN_POINT('Ctrl Pts',(0.847640811743635,0.564186360355263,
-3.55785525364576)) ;
#49476 = CARTESIAN_POINT('Ctrl Pts',(0.912923698230532,0.450967386047363,
-3.56906807992056)) ;
#49477 = CARTESIAN_POINT('Ctrl Pts',(0.99889282399385,0.200971487538376,-3.59526517656557)) ;
#49478 = CARTESIAN_POINT('Ctrl Pts',(1.0167565119974,0.0660569363633425,-3.60940288665213)) ;
#49479 = CARTESIAN_POINT('Ctrl Pts',(0.998865597141553,-0.197710566395658,
-3.63704311116301)) ;
#49480 = CARTESIAN_POINT('Ctrl Pts',(0.965256077089535,-0.324245770666553,
-3.65030274860126)) ;
#49481 = CARTESIAN_POINT('Ctrl Pts',(0.85030427513232,-0.561075523321808,
-3.67512016342977)) ;
#49482 = CARTESIAN_POINT('Ctrl Pts',(0.768804038865719,-0.668429348081556,
-3.68741107080029)) ;
#49483 = CARTESIAN_POINT('Ctrl Pts',(0.589722281275919,-0.826643482906197,
-3.71195253829972)) ;
#49484 = CARTESIAN_POINT('Ctrl Pts',(0.500332228866758,-0.883615481910104,
-3.72304981634036)) ;
#49485 = CARTESIAN_POINT('Ctrl Pts',(0.308892965347628,-0.967113466557388,
-3.7447979819066)) ;
#49486 = CARTESIAN_POINT('Ctrl Pts',(0.208180352251547,-0.993680860028146,
-3.7553297415333)) ;
#49487 = CARTESIAN_POINT('Ctrl Pts',(0.105153794786493,-1.00446632216085,
-3.76524459855233)) ;
#49488 = CARTESIAN_POINT('',(0.774268453261688,-0.648473804557356,-3.76524459855233)) ;
#49489 = CARTESIAN_POINT('Origin',(-1.52655665885959E-15,-8.32667268468867E-16,
-3.76524459855233)) ;
#49490 = CARTESIAN_POINT('Ctrl Pts',(0.774268453261685,-0.648473804557355,
-3.76524459855232)) ;
#49491 = CARTESIAN_POINT('Ctrl Pts',(0.840370767588072,-0.569548586127837,
-3.7551104634612)) ;
#49492 = CARTESIAN_POINT('Ctrl Pts',(0.893970558333253,-0.481062795668105,
-3.74611062123658)) ;
#49493 = CARTESIAN_POINT('Ctrl Pts',(0.974045968545029,-0.287421080478679,
-3.72581888542181)) ;
#49494 = CARTESIAN_POINT('Ctrl Pts',(0.998915511899947,-0.183104863629178,
-3.71488757802538)) ;
#49495 = CARTESIAN_POINT('Ctrl Pts',(1.01727115688353,0.0573323294145966,
-3.68969213913704)) ;
#49496 = CARTESIAN_POINT('Ctrl Pts',(1.00058656044149,0.19228093719233,-3.67555086025547)) ;
#49497 = CARTESIAN_POINT('Ctrl Pts',(0.916798193787988,0.44309246430084,-3.64926829380326)) ;
#49498 = CARTESIAN_POINT('Ctrl Pts',(0.852391509108282,0.557025563477903,
-3.63803657400815)) ;
#49499 = CARTESIAN_POINT('Ctrl Pts',(0.682951053349339,0.755515849489765,
-3.61225979219456)) ;
#49500 = CARTESIAN_POINT('Ctrl Pts',(0.579151050689367,0.837729557186524,
-3.59853225762935)) ;
#49501 = CARTESIAN_POINT('Ctrl Pts',(0.343206047134314,0.959297696220488,
-3.57075046862974)) ;
#49502 = CARTESIAN_POINT('Ctrl Pts',(0.212700111861635,0.996411341438793,
-3.55696236697253)) ;
#49503 = CARTESIAN_POINT('Ctrl Pts',(-0.0491996360435293,1.01688069028333,
-3.53212223818676)) ;
#49504 = CARTESIAN_POINT('Ctrl Pts',(-0.177830599393395,1.00243281614573,
-3.52041756793102)) ;
#49505 = CARTESIAN_POINT('Ctrl Pts',(-0.427136245527989,0.924760364510814,
-3.49372320554004)) ;
#49506 = CARTESIAN_POINT('Ctrl Pts',(-0.544834254403358,0.860685319992209,
-3.47968479070716)) ;
#49507 = CARTESIAN_POINT('Ctrl Pts',(-0.750311381920156,0.689360432784342,
-3.45206098123404)) ;
#49508 = CARTESIAN_POINT('Ctrl Pts',(-0.835432159454808,0.583253987341258,
-3.43931924702003)) ;
#49509 = CARTESIAN_POINT('Ctrl Pts',(-0.956669977026895,0.348645229828716,
-3.41473457050743)) ;
#49510 = CARTESIAN_POINT('Ctrl Pts',(-0.993407093942808,0.223333825066968,
-3.40160317514917)) ;
#49511 = CARTESIAN_POINT('Ctrl Pts',(-1.0181005821026,-0.0392089297094878,
-3.37409129210891)) ;
#49512 = CARTESIAN_POINT('Ctrl Pts',(-1.00386109065737,-0.174195975373168,
-3.35994598531722)) ;
#49513 = CARTESIAN_POINT('Ctrl Pts',(-0.924612462163221,-0.426676173258984,
-3.33348855867777)) ;
#49514 = CARTESIAN_POINT('Ctrl Pts',(-0.862021228541091,-0.542104042455757,
-3.32219229353536)) ;
#49515 = CARTESIAN_POINT('Ctrl Pts',(-0.695858586016805,-0.743606186778871,
-3.29655516972656)) ;
#49516 = CARTESIAN_POINT('Ctrl Pts',(-0.59367656343571,-0.827463437935267,
-3.28288835475294)) ;
#49517 = CARTESIAN_POINT('Ctrl Pts',(-0.360097102063987,-0.95308900066841,
-3.25510865189117)) ;
#49518 = CARTESIAN_POINT('Ctrl Pts',(-0.230247952113534,-0.992505220312161,
-3.24125951058011)) ;
#49519 = CARTESIAN_POINT('Ctrl Pts',(-0.0643298621211295,-1.0084204317768,
-3.22536841729334)) ;
#49520 = CARTESIAN_POINT('Ctrl Pts',(-0.0321504521144425,-1.00995540144761,
-3.22236768226083)) ;
#49521 = CARTESIAN_POINT('Ctrl Pts',(-2.0905741107248E-12,-1.00995540144768,
-3.2194500000002)) ;
#49522 = CARTESIAN_POINT('Origin',(0.,-1.99494625052956E-16,1.6393)) ;
#49523 = CARTESIAN_POINT('',(-2.55525626680218,-5.21339033092948E-16,1.7018)) ;
#49524 = CARTESIAN_POINT('Origin',(0.,-2.08410392278897E-16,1.7018)) ;
#49525 = CARTESIAN_POINT('',(-2.60242561556611,-5.12350575476211E-16,1.59829631068809)) ;
#49526 = CARTESIAN_POINT('Origin',(-2.55525626680218,-5.12423265867006E-16,
1.6393)) ;
#49527 = CARTESIAN_POINT('',(-3.18705220012211E-16,2.60242561556611,1.59829631068809)) ;
#49528 = CARTESIAN_POINT('Origin',(-3.18705220012211E-16,-2.77555756156289E-16,
1.59829631068809)) ;
#49529 = CARTESIAN_POINT('Origin',(-3.18705220012211E-16,-2.77555756156289E-16,
1.59829631068809)) ;
#49530 = CARTESIAN_POINT('Origin',(0.,2.40741243048404E-32,0.240832122829324)) ;
#49531 = CARTESIAN_POINT('',(-1.7419376071072E-16,1.4224,0.240832122829324)) ;
#49532 = CARTESIAN_POINT('Origin',(0.,-2.08410392278897E-16,1.7018)) ;
#49533 = CARTESIAN_POINT('',(1.75503707368249,-0.355600000000007,1.7018)) ;
#49534 = CARTESIAN_POINT('',(1.75503707368249,0.355600000000001,1.7018)) ;
#49535 = CARTESIAN_POINT('Origin',(0.,-1.33894542197505E-16,1.7018)) ;
#49536 = CARTESIAN_POINT('',(1.05531853684124,-0.355600000000004,1.7018)) ;
#49537 = CARTESIAN_POINT('',(-1.13137151332636E-15,-0.355600000000001,1.7018)) ;
#49538 = CARTESIAN_POINT('',(0.56054281451887,-0.560542814518875,1.7018)) ;
#49539 = CARTESIAN_POINT('',(0.280271407259434,-0.676635032551125,1.7018)) ;
#49540 = CARTESIAN_POINT('',(0.355599999999997,-1.05531853684125,1.7018)) ;
#49541 = CARTESIAN_POINT('',(0.676635032551123,-0.280271407259438,1.7018)) ;
#49542 = CARTESIAN_POINT('',(0.355599999999995,-1.75503707368249,1.7018)) ;
#49543 = CARTESIAN_POINT('',(0.355600000000001,-1.18647113870949E-15,1.7018)) ;
#49544 = CARTESIAN_POINT('',(-0.3556,-1.75503707368249,1.7018)) ;
#49545 = CARTESIAN_POINT('Origin',(-1.33894542197505E-16,4.67490295455533E-31,
1.7018)) ;
#49546 = CARTESIAN_POINT('',(-0.355600000000001,-1.05531853684125,1.7018)) ;
#49547 = CARTESIAN_POINT('',(-0.355600000000001,-1.10199250766261E-16,1.7018)) ;
#49548 = CARTESIAN_POINT('',(-0.560542814518873,-0.560542814518872,1.7018)) ;
#49549 = CARTESIAN_POINT('',(-0.676635032551124,-0.280271407259437,1.7018)) ;
#49550 = CARTESIAN_POINT('',(-1.05531853684125,-0.355600000000001,1.7018)) ;
#49551 = CARTESIAN_POINT('',(-0.280271407259436,-0.676635032551124,1.7018)) ;
#49552 = CARTESIAN_POINT('',(-1.75503707368249,-0.355600000000001,1.7018)) ;
#49553 = CARTESIAN_POINT('',(5.50996253831303E-17,-0.355600000000001,1.7018)) ;
#49554 = CARTESIAN_POINT('',(-1.75503707368249,0.355600000000019,1.7018)) ;
#49555 = CARTESIAN_POINT('Origin',(0.,1.33894542197505E-16,1.7018)) ;
#49556 = CARTESIAN_POINT('',(-1.05531853684124,0.355600000000012,1.7018)) ;
#49557 = CARTESIAN_POINT('',(3.6145130415116E-15,0.355600000000001,1.7018)) ;
#49558 = CARTESIAN_POINT('',(-0.560542814518866,0.560542814518879,1.7018)) ;
#49559 = CARTESIAN_POINT('',(-0.28027140725943,0.676635032551127,1.7018)) ;
#49560 = CARTESIAN_POINT('',(-0.35559999999999,1.05531853684125,1.7018)) ;
#49561 = CARTESIAN_POINT('',(-0.676635032551121,0.280271407259443,1.7018)) ;
#49562 = CARTESIAN_POINT('',(-0.355599999999983,1.75503707368249,1.7018)) ;
#49563 = CARTESIAN_POINT('',(-0.355600000000001,3.66961266689473E-15,1.7018)) ;
#49564 = CARTESIAN_POINT('',(0.3556,1.75503707368249,1.7018)) ;
#49565 = CARTESIAN_POINT('Origin',(0.,-1.33894542197505E-16,1.7018)) ;
#49566 = CARTESIAN_POINT('',(0.355600000000001,1.05531853684125,1.7018)) ;
#49567 = CARTESIAN_POINT('',(0.355600000000001,1.10199250766261E-16,1.7018)) ;
#49568 = CARTESIAN_POINT('',(0.560542814518873,0.560542814518872,1.7018)) ;
#49569 = CARTESIAN_POINT('',(0.676635032551124,0.280271407259437,1.7018)) ;
#49570 = CARTESIAN_POINT('',(1.05531853684125,0.355600000000001,1.7018)) ;
#49571 = CARTESIAN_POINT('',(0.280271407259436,0.676635032551124,1.7018)) ;
#49572 = CARTESIAN_POINT('',(-5.50996253831303E-17,0.355600000000001,1.7018)) ;
#49573 = CARTESIAN_POINT('Origin',(0.,1.88183760310947E-30,-3.85445)) ;
#49574 = CARTESIAN_POINT('',(5.12045573059185E-15,1.15468837738307,-3.62051162261693)) ;
#49575 = CARTESIAN_POINT('Ctrl Pts',(1.03838891449855E-14,1.15468837738307,
-3.62051162261693)) ;
#49576 = CARTESIAN_POINT('Ctrl Pts',(-0.0254296726502328,1.1559680560723,
-3.6192319439277)) ;
#49577 = CARTESIAN_POINT('Ctrl Pts',(-0.0508514616237012,1.15642735309998,
-3.61793251315105)) ;
#49578 = CARTESIAN_POINT('Ctrl Pts',(-0.233510489525033,1.15388205746895,
-3.60845534611773)) ;
#49579 = CARTESIAN_POINT('Ctrl Pts',(-0.388772346045262,1.12045269968389,
-3.59965551646851)) ;
#49580 = CARTESIAN_POINT('Ctrl Pts',(-0.668629325046152,0.998730134850622,
-3.58242290709769)) ;
#49581 = CARTESIAN_POINT('Ctrl Pts',(-0.792053279372469,0.914879512409016,
-3.57414824333137)) ;
#49582 = CARTESIAN_POINT('Ctrl Pts',(-1.03279540943537,0.675197560377038,
-3.55623042073669)) ;
#49583 = CARTESIAN_POINT('Ctrl Pts',(-1.11355473457586,0.529659861818994,
-3.54881034220498)) ;
#49584 = CARTESIAN_POINT('Ctrl Pts',(-1.22297818921426,0.264095836621968,
-3.53409227811305)) ;
#49585 = CARTESIAN_POINT('Ctrl Pts',(-1.2550263520995,0.107380842554988,-3.52557676781509)) ;
#49586 = CARTESIAN_POINT('Ctrl Pts',(-1.25910520773258,-0.217034008792059,
-3.50831229920614)) ;
#49587 = CARTESIAN_POINT('Ctrl Pts',(-1.22823973733675,-0.381711211853662,
-3.49973959429333)) ;
#49588 = CARTESIAN_POINT('Ctrl Pts',(-1.13475227202362,-0.613697014078021,
-3.4878698745816)) ;
#49589 = CARTESIAN_POINT('Ctrl Pts',(-1.09529703778593,-0.688397717616974,
-3.48416949380928)) ;
#49590 = CARTESIAN_POINT('Ctrl Pts',(-0.960513035812505,-0.89515457262902,
-3.47251753328569)) ;
#49591 = CARTESIAN_POINT('Ctrl Pts',(-0.845988378373653,-1.01478305680017,
-3.46424837249028)) ;
#49592 = CARTESIAN_POINT('Ctrl Pts',(-0.56869741157037,-1.2132712153186,-3.4469467685559)) ;
#49593 = CARTESIAN_POINT('Ctrl Pts',(-0.405690771199438,-1.28628105760199,
-3.43807887608712)) ;
#49594 = CARTESIAN_POINT('Ctrl Pts',(-0.00488190160641552,-1.37632292771543,
-3.41885139468694)) ;
#49595 = CARTESIAN_POINT('Ctrl Pts',(0.185605942854219,-1.35631716810315,
-3.4111058346593)) ;
#49596 = CARTESIAN_POINT('Ctrl Pts',(0.473218634669871,-1.30588042490048,
-3.39746749290741)) ;
#49597 = CARTESIAN_POINT('Ctrl Pts',(0.639723227604972,-1.24247603160398,
-3.38887866863048)) ;
#49598 = CARTESIAN_POINT('Ctrl Pts',(0.873435804281771,-1.09786424296003,
-3.37571354842859)) ;
#49599 = CARTESIAN_POINT('Ctrl Pts',(0.951273721808984,-1.03743011170928,
-3.37108278809331)) ;
#49600 = CARTESIAN_POINT('Ctrl Pts',(1.09831291486203,-0.89591089855239,-3.36177284448109)) ;
#49601 = CARTESIAN_POINT('Ctrl Pts',(1.16590959394519,-0.814068072356269,
-3.35714783320766)) ;
#49602 = CARTESIAN_POINT('Ctrl Pts',(1.22356791609788,-0.7253297971929,-3.3528)) ;
#49603 = CARTESIAN_POINT('',(-1.12759354031493E-16,0.92075,-3.85445)) ;
#49604 = CARTESIAN_POINT('',(-1.12759354031493E-16,0.92075,-3.85445)) ;
#49605 = CARTESIAN_POINT('Origin',(0.,1.88183760310947E-30,-3.85445)) ;
#49606 = CARTESIAN_POINT('Ctrl Pts',(0.774268453261687,-0.648473804557357,
-3.76524459855232)) ;
#49607 = CARTESIAN_POINT('Ctrl Pts',(0.859102969586174,-0.55913383481557,
-3.75757093331012)) ;
#49608 = CARTESIAN_POINT('Ctrl Pts',(0.916121144663882,-0.465482527176917,
-3.75163840738811)) ;
#49609 = CARTESIAN_POINT('Ctrl Pts',(0.998843870248869,-0.290638199560699,
-3.73995486333014)) ;
#49610 = CARTESIAN_POINT('Ctrl Pts',(1.02887334963585,-0.192294498521731,
-3.73350006306968)) ;
#49611 = CARTESIAN_POINT('Ctrl Pts',(1.06402398082417,0.0390726262195363,
-3.71860738004544)) ;
#49612 = CARTESIAN_POINT('Ctrl Pts',(1.0591688619149,0.171888637195841,-3.71026675792788)) ;
#49613 = CARTESIAN_POINT('Ctrl Pts',(0.99249334900811,0.464810257053766,-3.69226247684784)) ;
#49614 = CARTESIAN_POINT('Ctrl Pts',(0.921867648435038,0.593606465432917,
-3.68488414547832)) ;
#49615 = CARTESIAN_POINT('Ctrl Pts',(0.768670465162765,0.807762346300646,
-3.66988824166624)) ;
#49616 = CARTESIAN_POINT('Ctrl Pts',(0.660201212740624,0.909449744418889,
-3.66103765914579)) ;
#49617 = CARTESIAN_POINT('Ctrl Pts',(0.418335514202568,1.05987871318753,-3.64405552581747)) ;
#49618 = CARTESIAN_POINT('Ctrl Pts',(0.289099677970515,1.11038390089825,-3.63605666514225)) ;
#49619 = CARTESIAN_POINT('Ctrl Pts',(0.10284383143768,1.14596277031152,-3.62580411226576)) ;
#49620 = CARTESIAN_POINT('Ctrl Pts',(0.0514158133764808,1.15210101727144,
-3.62309898272856)) ;
#49621 = CARTESIAN_POINT('Ctrl Pts',(1.0399667238481E-14,1.15468837738307,
-3.62051162261693)) ;
#49622 = CARTESIAN_POINT('Ctrl Pts',(0.105153794786499,-1.00446632216084,
-3.76524459855233)) ;
#49623 = CARTESIAN_POINT('Ctrl Pts',(0.195392726897351,-1.01520050247604,
-3.74517332734323)) ;
#49624 = CARTESIAN_POINT('Ctrl Pts',(0.286522180585977,-1.01456179720496,
-3.72467512354645)) ;
#49625 = CARTESIAN_POINT('Ctrl Pts',(0.46774836542941,-0.990396472641326,
-3.68358102451341)) ;
#49626 = CARTESIAN_POINT('Ctrl Pts',(0.557102511311268,-0.966654412138457,
-3.66314099600361)) ;
#49627 = CARTESIAN_POINT('Ctrl Pts',(0.766470858342022,-0.881427413527447,
-3.61446326325569)) ;
#49628 = CARTESIAN_POINT('Ctrl Pts',(0.880404660110909,-0.80843917966244,
-3.58726411136041)) ;
#49629 = CARTESIAN_POINT('Ctrl Pts',(1.00638639259649,-0.690563563660173,
-3.55523972623751)) ;
#49630 = CARTESIAN_POINT('Ctrl Pts',(1.06917436077557,-0.62930339582118,-3.54012168635209)) ;
#49631 = CARTESIAN_POINT('Ctrl Pts',(1.22604009876658,-0.407710720418697,
-3.49187907348018)) ;
#49632 = CARTESIAN_POINT('Ctrl Pts',(1.29218005609473,-0.26941590119793,-3.46374626079454)) ;
#49633 = CARTESIAN_POINT('Ctrl Pts',(1.37633487012138,0.0277330507548143,
-3.40722015539582)) ;
#49634 = CARTESIAN_POINT('Ctrl Pts',(1.39229240585019,0.184820732040757,-3.37924330459697)) ;
#49635 = CARTESIAN_POINT('Ctrl Pts',(1.38082735583561,0.341376000000042,-3.35280000000001)) ;
#49636 = CARTESIAN_POINT('Origin',(0.,-5.62590548091936E-17,0.635211073789819)) ;
#49637 = CARTESIAN_POINT('',(0.,-5.7099106829244E-18,-0.479172560746747)) ;
#49638 = CARTESIAN_POINT('',(-2.19297502323318E-16,1.79070000000001,1.58079214606392)) ;
#49639 = CARTESIAN_POINT('',(-1.18633851772253E-16,0.968718914342085,0.635211073789819)) ;
#49640 = CARTESIAN_POINT('',(-0.345013184582974,1.75714893861161,1.58079214606391)) ;
#49641 = CARTESIAN_POINT('Origin',(0.,-1.91148346547618E-16,1.58079214606391)) ;
#49642 = CARTESIAN_POINT('',(-0.272892694210214,1.03886703084701,0.756451169002388)) ;
#49643 = CARTESIAN_POINT('Ctrl Pts',(-0.272892694210214,1.03886703084701,
0.756451169002387)) ;
#49644 = CARTESIAN_POINT('Ctrl Pts',(-0.299689250637345,1.3071111559911,1.06273721049842)) ;
#49645 = CARTESIAN_POINT('Ctrl Pts',(-0.345013184582945,1.75714893861133,
1.58079214606358)) ;
#49646 = CARTESIAN_POINT('',(-0.465177703148305,0.465177703148315,0.277609509066653)) ;
#49647 = CARTESIAN_POINT('Ctrl Pts',(-0.272892694210214,1.03886703084701,
0.756451169002388)) ;
#49648 = CARTESIAN_POINT('Ctrl Pts',(-0.388126284358586,0.67608985904451,
0.386496290406958)) ;
#49649 = CARTESIAN_POINT('Ctrl Pts',(-0.465177703148304,0.465177703148316,
0.277609509066654)) ;
#49650 = CARTESIAN_POINT('',(-1.03886703084701,0.272892694210236,0.756451169002387)) ;
#49651 = CARTESIAN_POINT('Ctrl Pts',(-0.465177703148307,0.465177703148314,
0.277609509066655)) ;
#49652 = CARTESIAN_POINT('Ctrl Pts',(-0.676089859053593,0.38812628435528,
0.386496290411651)) ;
#49653 = CARTESIAN_POINT('Ctrl Pts',(-1.03886703088336,0.272892694198688,
0.756451169039463)) ;
#49654 = CARTESIAN_POINT('',(-1.75714893861161,0.34501318458301,1.58079214606391)) ;
#49655 = CARTESIAN_POINT('Ctrl Pts',(-1.03886703084701,0.272892694210236,
0.756451169002386)) ;
#49656 = CARTESIAN_POINT('Ctrl Pts',(-1.30711115599117,0.29968925063738,1.06273721049851)) ;
#49657 = CARTESIAN_POINT('Ctrl Pts',(-1.75714893861161,0.34501318458301,1.58079214606391)) ;
#49658 = CARTESIAN_POINT('',(-1.75714893861161,-0.345013184582992,1.58079214606391)) ;
#49659 = CARTESIAN_POINT('Origin',(0.,1.91148346547618E-16,1.58079214606391)) ;
#49660 = CARTESIAN_POINT('',(-1.03886703084701,-0.272892694210225,0.756451169002387)) ;
#49661 = CARTESIAN_POINT('Ctrl Pts',(-1.03886703084701,-0.272892694210225,
0.756451169002387)) ;
#49662 = CARTESIAN_POINT('Ctrl Pts',(-1.3071111559911,-0.299689250637359,
1.06273721049842)) ;
#49663 = CARTESIAN_POINT('Ctrl Pts',(-1.75714893861132,-0.345013184582963,
1.58079214606358)) ;
#49664 = CARTESIAN_POINT('',(-0.46517770314831,-0.465177703148309,0.277609509066653)) ;
#49665 = CARTESIAN_POINT('Ctrl Pts',(-1.03886703084701,-0.272892694210225,
0.756451169002387)) ;
#49666 = CARTESIAN_POINT('Ctrl Pts',(-0.676089859044505,-0.388126284358593,
0.386496290406956)) ;
#49667 = CARTESIAN_POINT('Ctrl Pts',(-0.46517770314831,-0.465177703148309,
0.277609509066652)) ;
#49668 = CARTESIAN_POINT('',(-0.272892694210225,-1.03886703084701,0.756451169002387)) ;
#49669 = CARTESIAN_POINT('Ctrl Pts',(-0.465177703148309,-0.465177703148311,
0.277609509066654)) ;
#49670 = CARTESIAN_POINT('Ctrl Pts',(-0.388126284355273,-0.676089859053595,
0.386496290411649)) ;
#49671 = CARTESIAN_POINT('Ctrl Pts',(-0.272892694198678,-1.03886703088336,
0.756451169039458)) ;
#49672 = CARTESIAN_POINT('',(-0.345013184582991,-1.75714893861161,1.58079214606391)) ;
#49673 = CARTESIAN_POINT('Ctrl Pts',(-0.272892694210235,-1.038867030847,0.756451169002379)) ;
#49674 = CARTESIAN_POINT('Ctrl Pts',(-0.299689250637379,-1.30711115599116,
1.0627372104985)) ;
#49675 = CARTESIAN_POINT('Ctrl Pts',(-0.345013184583009,-1.75714893861159,
1.58079214606389)) ;
#49676 = CARTESIAN_POINT('',(0.345013184582986,-1.75714893861161,1.58079214606391)) ;
#49677 = CARTESIAN_POINT('Origin',(-1.91148346547618E-16,6.6739088492173E-31,
1.58079214606391)) ;
#49678 = CARTESIAN_POINT('',(0.272892694210221,-1.03886703084701,0.756451169002387)) ;
#49679 = CARTESIAN_POINT('Ctrl Pts',(0.272892694210226,-1.03886703084701,
0.756451169002393)) ;
#49680 = CARTESIAN_POINT('Ctrl Pts',(0.299689250637368,-1.30711115599118,
1.06273721049852)) ;
#49681 = CARTESIAN_POINT('Ctrl Pts',(0.345013184582994,-1.75714893861162,
1.58079214606392)) ;
#49682 = CARTESIAN_POINT('',(0.465177703148308,-0.465177703148311,0.277609509066653)) ;
#49683 = CARTESIAN_POINT('Ctrl Pts',(0.272892694198675,-1.03886703088336,
0.756451169039455)) ;
#49684 = CARTESIAN_POINT('Ctrl Pts',(0.388126284355271,-0.676089859053595,
0.386496290411648)) ;
#49685 = CARTESIAN_POINT('Ctrl Pts',(0.465177703148307,-0.465177703148311,
0.277609509066652)) ;
#49686 = CARTESIAN_POINT('',(1.03886703084701,-0.272892694210228,0.756451169002387)) ;
#49687 = CARTESIAN_POINT('Ctrl Pts',(0.465177703148308,-0.465177703148311,
0.277609509066653)) ;
#49688 = CARTESIAN_POINT('Ctrl Pts',(0.676089859044505,-0.388126284358596,
0.386496290406957)) ;
#49689 = CARTESIAN_POINT('Ctrl Pts',(1.03886703084701,-0.272892694210229,
0.756451169002387)) ;
#49690 = CARTESIAN_POINT('',(1.75714893861161,-0.345013184582997,1.58079214606391)) ;
#49691 = CARTESIAN_POINT('Ctrl Pts',(1.03886703084701,-0.272892694210228,
0.756451169002387)) ;
#49692 = CARTESIAN_POINT('Ctrl Pts',(1.30711115599109,-0.299689250637364,
1.06273721049842)) ;
#49693 = CARTESIAN_POINT('Ctrl Pts',(1.75714893861132,-0.345013184582969,
1.58079214606358)) ;
#49694 = CARTESIAN_POINT('',(1.75714893861161,0.345013184582992,1.58079214606391)) ;
#49695 = CARTESIAN_POINT('Origin',(0.,-1.91148346547618E-16,1.58079214606391)) ;
#49696 = CARTESIAN_POINT('',(1.03886703084701,0.272892694210225,0.756451169002387)) ;
#49697 = CARTESIAN_POINT('Ctrl Pts',(1.03886703084701,0.272892694210225,0.756451169002387)) ;
#49698 = CARTESIAN_POINT('Ctrl Pts',(1.30711115599118,0.299689250637367,1.06273721049851)) ;
#49699 = CARTESIAN_POINT('Ctrl Pts',(1.75714893861161,0.345013184582992,1.5807921460639)) ;
#49700 = CARTESIAN_POINT('',(0.46517770314831,0.46517770314831,0.277609509066653)) ;
#49701 = CARTESIAN_POINT('Ctrl Pts',(1.03886703088336,0.272892694198679,0.756451169039457)) ;
#49702 = CARTESIAN_POINT('Ctrl Pts',(0.676089859053591,0.388126284355274,
0.386496290411646)) ;
#49703 = CARTESIAN_POINT('Ctrl Pts',(0.465177703148306,0.465177703148311,
0.277609509066652)) ;
#49704 = CARTESIAN_POINT('',(0.272892694210225,1.03886703084701,0.756451169002387)) ;
#49705 = CARTESIAN_POINT('Ctrl Pts',(0.46517770314831,0.465177703148308,0.277609509066653)) ;
#49706 = CARTESIAN_POINT('Ctrl Pts',(0.388126284358594,0.676089859044504,
0.386496290406956)) ;
#49707 = CARTESIAN_POINT('Ctrl Pts',(0.272892694210225,1.03886703084701,0.756451169002387)) ;
#49708 = CARTESIAN_POINT('',(0.345013184582991,1.75714893861161,1.58079214606391)) ;
#49709 = CARTESIAN_POINT('Ctrl Pts',(0.272892694210225,1.03886703084701,0.756451169002387)) ;
#49710 = CARTESIAN_POINT('Ctrl Pts',(0.299689250637359,1.30711115599109,1.06273721049842)) ;
#49711 = CARTESIAN_POINT('Ctrl Pts',(0.345013184582963,1.75714893861132,1.58079214606358)) ;
#49712 = CARTESIAN_POINT('Origin',(0.,-1.91148346547618E-16,1.58079214606391)) ;
#49713 = CARTESIAN_POINT('Origin',(0.,-1.33894542197505E-16,-5.05771666666667)) ;
#49714 = CARTESIAN_POINT('Origin',(0.,-1.33894542197505E-16,-2.36272659886193)) ;
#49715 = CARTESIAN_POINT('Origin',(0.,-1.33894542197505E-16,-2.36272659886194)) ;
#49716 = CARTESIAN_POINT('Origin',(0.,1.33894542197505E-16,-5.05771666666667)) ;
#49717 = CARTESIAN_POINT('Origin',(0.,1.33894542197505E-16,-2.36272659886194)) ;
#49718 = CARTESIAN_POINT('Origin',(0.,1.33894542197505E-16,-2.36272659886193)) ;
#49719 = CARTESIAN_POINT('Origin',(-1.33894542197505E-16,4.67490295455533E-31,
-5.05771666666667)) ;
#49720 = CARTESIAN_POINT('Origin',(-1.33894542197505E-16,4.67490295455533E-31,
-2.36272659886193)) ;
#49721 = CARTESIAN_POINT('Origin',(-1.33894542197505E-16,4.67490295455533E-31,
-2.36272659886193)) ;
#49722 = CARTESIAN_POINT('Origin',(0.280271407259434,-0.676635032551125,1.7018)) ;
#49723 = CARTESIAN_POINT('',(0.559813216252793,-0.559813216252798,1.69090411891923)) ;
#49724 = CARTESIAN_POINT('',(1.05500145698799,-0.354005931931581,1.68357971860376)) ;
#49725 = CARTESIAN_POINT('Origin',(0.676635032551123,-0.280271407259438,1.7018)) ;
#49726 = CARTESIAN_POINT('',(0.354005931931574,-1.05500145698799,1.68357971860376)) ;
#49727 = CARTESIAN_POINT('Origin',(0.355600000000001,-1.18647113870949E-15,
1.7018)) ;
#49728 = CARTESIAN_POINT('Origin',(-0.355600000000001,-1.10199250766261E-16,
1.7018)) ;
#49729 = CARTESIAN_POINT('',(-0.354005931931577,-1.05500145698799,1.68357971860376)) ;
#49730 = CARTESIAN_POINT('Origin',(-0.676635032551124,-0.280271407259437,
1.7018)) ;
#49731 = CARTESIAN_POINT('',(-0.559813216252796,-0.559813216252795,1.69090411891923)) ;
#49732 = CARTESIAN_POINT('Origin',(-0.280271407259436,-0.676635032551124,
1.7018)) ;
#49733 = CARTESIAN_POINT('',(-1.05500145698799,-0.354005931931578,1.68357971860376)) ;
#49734 = CARTESIAN_POINT('Origin',(5.50996253831303E-17,-0.355600000000001,
1.7018)) ;
#49735 = CARTESIAN_POINT('Origin',(3.6145130415116E-15,0.355600000000001,
1.7018)) ;
#49736 = CARTESIAN_POINT('',(-1.05500145698799,0.354005931931589,1.68357971860376)) ;
#49737 = CARTESIAN_POINT('Origin',(-0.28027140725943,0.676635032551127,1.7018)) ;
#49738 = CARTESIAN_POINT('',(-0.559813216252789,0.559813216252801,1.69090411891923)) ;
#49739 = CARTESIAN_POINT('Origin',(-0.676635032551121,0.280271407259443,1.7018)) ;
#49740 = CARTESIAN_POINT('',(-0.354005931931567,1.055001456988,1.68357971860376)) ;
#49741 = CARTESIAN_POINT('Origin',(-0.355600000000001,3.66961266689473E-15,
1.7018)) ;
#49742 = CARTESIAN_POINT('Origin',(0.,-1.33894542197505E-16,-2.36272659886193)) ;
#49743 = CARTESIAN_POINT('Origin',(0.,-1.33894542197505E-16,-5.05771666666667)) ;
#49744 = CARTESIAN_POINT('Origin',(0.,-1.33894542197505E-16,-2.36272659886194)) ;
#49745 = CARTESIAN_POINT('Origin',(0.355600000000001,1.10199250766261E-16,
1.7018)) ;
#49746 = CARTESIAN_POINT('',(0.354005931931577,1.05500145698799,1.68357971860376)) ;
#49747 = CARTESIAN_POINT('Origin',(0.676635032551124,0.280271407259437,1.7018)) ;
#49748 = CARTESIAN_POINT('',(0.559813216252796,0.559813216252795,1.69090411891923)) ;
#49749 = CARTESIAN_POINT('Origin',(0.280271407259436,0.676635032551124,1.7018)) ;
#49750 = CARTESIAN_POINT('',(1.05500145698799,0.354005931931578,1.68357971860376)) ;
#49751 = CARTESIAN_POINT('Origin',(-5.50996253831303E-17,0.355600000000001,
1.7018)) ;
#49752 = CARTESIAN_POINT('Origin',(-1.13137151332636E-15,-0.355600000000001,
1.7018)) ;
#49753 = CARTESIAN_POINT('Origin',(0.,0.,0.)) ;
#49754 = CARTESIAN_POINT('Ctrl Pts',(0.491435946297415,1.33480802765296,1.64178456984939E-16)) ;
#49755 = CARTESIAN_POINT('Ctrl Pts',(0.631063497904959,1.26227785840513,1.57620625117627E-16)) ;
#49756 = CARTESIAN_POINT('Ctrl Pts',(0.757237166432859,1.16646160759251,4.82074980013067E-17)) ;
#49757 = CARTESIAN_POINT('Ctrl Pts',(0.973454042431244,0.93461893256702,2.5493608898663E-17)) ;
#49758 = CARTESIAN_POINT('Ctrl Pts',(1.06120306904122,0.799873965737815,1.19234218146397E-16)) ;
#49759 = CARTESIAN_POINT('Ctrl Pts',(1.15674989147546,0.576768217997932,9.6322737338553E-17)) ;
#49760 = CARTESIAN_POINT('Ctrl Pts',(1.21968871378171,0.413792942784443,1.81740200073975E-18)) ;
#49761 = CARTESIAN_POINT('Ctrl Pts',(1.22263774786217,0.0317209092632606,
-3.26382690937545E-17)) ;
#49762 = CARTESIAN_POINT('Ctrl Pts',(1.19297461938357,-0.123873174315643,
8.71909996142948E-10)) ;
#49763 = CARTESIAN_POINT('Ctrl Pts',(1.10615071765841,-0.338117862197598,
8.71909977118802E-10)) ;
#49764 = CARTESIAN_POINT('Ctrl Pts',(1.07193711691856,-0.404128908965352,
-4.7408330026157E-17)) ;
#49765 = CARTESIAN_POINT('Ctrl Pts',(0.975954116420733,-0.553514539862139,
-6.15088024485444E-17)) ;
#49766 = CARTESIAN_POINT('Ctrl Pts',(0.923582668623707,-0.610351469100532,
6.3909699607946E-17)) ;
#49767 = CARTESIAN_POINT('Ctrl Pts',(0.835080540402359,-0.703023782935501,
5.64767333076593E-17)) ;
#49768 = CARTESIAN_POINT('Ctrl Pts',(0.759258426489408,-0.762791943082818,
1.79114405874878E-16)) ;
#49769 = CARTESIAN_POINT('Ctrl Pts',(0.599973513232069,-0.855169615486292,
1.71874893413169E-16)) ;
#49770 = CARTESIAN_POINT('Ctrl Pts',(0.518382068332362,-0.889218776095626,
-1.05380833470058E-16)) ;
#49771 = CARTESIAN_POINT('Ctrl Pts',(0.433387415541747,-0.912241887310308,
-1.07462473344528E-16)) ;
#49772 = CARTESIAN_POINT('Ctrl Pts',(-0.348937280953795,-0.947761935759142,
-1.09130430082023E-16)) ;
#49773 = CARTESIAN_POINT('Ctrl Pts',(-0.447327671712729,-0.930286436395833,
-1.07550378803908E-16)) ;
#49774 = CARTESIAN_POINT('Ctrl Pts',(-0.542596325781123,-0.898520691472632,
-3.93871915511075E-18)) ;
#49775 = CARTESIAN_POINT('Ctrl Pts',(-0.728576337247976,-0.804661253243085,
4.27229455739307E-18)) ;
#49776 = CARTESIAN_POINT('Ctrl Pts',(-0.816997845188147,-0.740844670056653,
-1.84590828456541E-16)) ;
#49777 = CARTESIAN_POINT('Ctrl Pts',(-0.923212579592666,-0.635422833885916,
-1.75901819604059E-16)) ;
#49778 = CARTESIAN_POINT('Ctrl Pts',(-0.976887238434203,-0.578692663218018,
-8.04035336178024E-18)) ;
#49779 = CARTESIAN_POINT('Ctrl Pts',(-1.12225033728478,-0.360679713470414,
1.23482497677119E-17)) ;
#49780 = CARTESIAN_POINT('Ctrl Pts',(-1.18348749295032,-0.212768435947515,
3.01208314832676E-16)) ;
#49781 = CARTESIAN_POINT('Ctrl Pts',(-1.24366589458071,0.089532641158921,
3.29749778961003E-16)) ;
#49782 = CARTESIAN_POINT('Ctrl Pts',(-1.24543419386366,0.240302910086207,
-4.39954125660478E-13)) ;
#49783 = CARTESIAN_POINT('Ctrl Pts',(-1.18298227166626,0.599699993322773,
-4.39919613627758E-13)) ;
#49784 = CARTESIAN_POINT('Ctrl Pts',(-1.09722247554694,0.7592012229505,-1.08314018284233E-16)) ;
#49785 = CARTESIAN_POINT('Ctrl Pts',(-0.980276797203946,0.943575674806962,
-9.10890065762937E-17)) ;
#49786 = CARTESIAN_POINT('Ctrl Pts',(-0.916929923265699,1.02290966726172,
-4.78134042320515E-16)) ;
#49787 = CARTESIAN_POINT('Ctrl Pts',(-0.774264939856819,1.16639610296708,
-4.65847090734852E-16)) ;
#49788 = CARTESIAN_POINT('Ctrl Pts',(-0.695420302659111,1.23011726595772,
9.13016138116806E-17)) ;
#49789 = CARTESIAN_POINT('Ctrl Pts',(-0.610373744209535,1.28478233657676,
9.62441686940418E-17)) ;
#49790 = CARTESIAN_POINT('Origin',(0.,0.92075,-3.85445)) ;
#49791 = CARTESIAN_POINT('Ctrl Pts',(0.,1.00995540144767,-4.17195000000001)) ;
#49792 = CARTESIAN_POINT('Ctrl Pts',(-0.583098022895331,1.00995540144767,
-4.11903333333334)) ;
#49793 = CARTESIAN_POINT('Ctrl Pts',(-0.874647034342996,0.504977700723831,
-4.06611666666667)) ;
#49794 = CARTESIAN_POINT('Ctrl Pts',(-1.16619604579066,-5.43898472251395E-15,
-4.01320000000001)) ;
#49795 = CARTESIAN_POINT('Ctrl Pts',(-0.874647034342996,-0.504977700723842,
-3.96028333333334)) ;
#49796 = CARTESIAN_POINT('Ctrl Pts',(-0.583098022895331,-1.00995540144768,
-3.90736666666667)) ;
#49797 = CARTESIAN_POINT('Ctrl Pts',(-1.23683864966447E-16,-1.00995540144768,
-3.85445000000001)) ;
#49798 = CARTESIAN_POINT('Ctrl Pts',(0.58309802289533,-1.00995540144768,-3.80153333333334)) ;
#49799 = CARTESIAN_POINT('Ctrl Pts',(0.874647034342996,-0.504977700723843,
-3.74861666666667)) ;
#49800 = CARTESIAN_POINT('Ctrl Pts',(1.16619604579066,-5.72462037344511E-15,
-3.69570000000001)) ;
#49801 = CARTESIAN_POINT('Ctrl Pts',(0.874647034342997,0.504977700723831,
-3.64278333333334)) ;
#49802 = CARTESIAN_POINT('Ctrl Pts',(0.583098022895331,1.00995540144767,-3.58986666666667)) ;
#49803 = CARTESIAN_POINT('Ctrl Pts',(0.,1.00995540144767,-3.53695000000001)) ;
#49804 = CARTESIAN_POINT('Ctrl Pts',(-0.583098022895331,1.00995540144767,
-3.48403333333334)) ;
#49805 = CARTESIAN_POINT('Ctrl Pts',(-0.874647034342996,0.504977700723831,
-3.43111666666667)) ;
#49806 = CARTESIAN_POINT('Ctrl Pts',(-1.16619604579066,-5.43898472251395E-15,
-3.37820000000001)) ;
#49807 = CARTESIAN_POINT('Ctrl Pts',(-0.874647034342996,-0.504977700723842,
-3.32528333333334)) ;
#49808 = CARTESIAN_POINT('Ctrl Pts',(-0.583098022895331,-1.00995540144768,
-3.27236666666667)) ;
#49809 = CARTESIAN_POINT('Ctrl Pts',(-1.23683864966447E-16,-1.00995540144768,
-3.21945000000001)) ;
#49810 = CARTESIAN_POINT('Ctrl Pts',(0.58309802289533,-1.00995540144768,-3.16653333333334)) ;
#49811 = CARTESIAN_POINT('Ctrl Pts',(0.874647034342996,-0.504977700723843,
-3.11361666666667)) ;
#49812 = CARTESIAN_POINT('Ctrl Pts',(1.16619604579066,-5.72462037344511E-15,
-3.06070000000001)) ;
#49813 = CARTESIAN_POINT('Ctrl Pts',(0.874647034342997,0.504977700723831,
-3.00778333333334)) ;
#49814 = CARTESIAN_POINT('Ctrl Pts',(0.583098022895331,1.00995540144767,-2.95486666666667)) ;
#49815 = CARTESIAN_POINT('Ctrl Pts',(0.,1.00995540144767,-2.90195000000001)) ;
#49816 = CARTESIAN_POINT('Ctrl Pts',(-0.583098022895331,1.00995540144767,
-2.84903333333334)) ;
#49817 = CARTESIAN_POINT('Ctrl Pts',(-0.874647034342996,0.504977700723831,
-2.79611666666667)) ;
#49818 = CARTESIAN_POINT('Ctrl Pts',(-1.16619604579066,-5.43898472251395E-15,
-2.74320000000001)) ;
#49819 = CARTESIAN_POINT('Ctrl Pts',(-0.874647034342996,-0.504977700723842,
-2.69028333333334)) ;
#49820 = CARTESIAN_POINT('Ctrl Pts',(-0.583098022895331,-1.00995540144768,
-2.63736666666667)) ;
#49821 = CARTESIAN_POINT('Ctrl Pts',(-1.23683864966447E-16,-1.00995540144768,
-2.58445000000001)) ;
#49822 = CARTESIAN_POINT('Ctrl Pts',(0.58309802289533,-1.00995540144768,-2.53153333333334)) ;
#49823 = CARTESIAN_POINT('Ctrl Pts',(0.874647034342996,-0.504977700723843,
-2.47861666666667)) ;
#49824 = CARTESIAN_POINT('Ctrl Pts',(1.16619604579066,-5.72462037344511E-15,
-2.42570000000001)) ;
#49825 = CARTESIAN_POINT('Ctrl Pts',(0.874647034342997,0.504977700723831,
-2.37278333333334)) ;
#49826 = CARTESIAN_POINT('Ctrl Pts',(0.583098022895331,1.00995540144767,-2.31986666666667)) ;
#49827 = CARTESIAN_POINT('Ctrl Pts',(0.,1.00995540144767,-2.26695000000001)) ;
#49828 = CARTESIAN_POINT('Ctrl Pts',(-0.583098022895331,1.00995540144767,
-2.21403333333334)) ;
#49829 = CARTESIAN_POINT('Ctrl Pts',(-0.874647034342996,0.504977700723831,
-2.16111666666667)) ;
#49830 = CARTESIAN_POINT('Ctrl Pts',(-1.16619604579066,-5.43898472251395E-15,
-2.10820000000001)) ;
#49831 = CARTESIAN_POINT('Ctrl Pts',(-0.874647034342996,-0.504977700723842,
-2.05528333333334)) ;
#49832 = CARTESIAN_POINT('Ctrl Pts',(-0.583098022895331,-1.00995540144768,
-2.00236666666667)) ;
#49833 = CARTESIAN_POINT('Ctrl Pts',(-1.23683864966447E-16,-1.00995540144768,
-1.94945000000001)) ;
#49834 = CARTESIAN_POINT('Ctrl Pts',(0.58309802289533,-1.00995540144768,-1.89653333333334)) ;
#49835 = CARTESIAN_POINT('Ctrl Pts',(0.874647034342996,-0.504977700723843,
-1.84361666666667)) ;
#49836 = CARTESIAN_POINT('Ctrl Pts',(1.16619604579066,-5.72462037344511E-15,
-1.79070000000001)) ;
#49837 = CARTESIAN_POINT('Ctrl Pts',(0.874647034342997,0.504977700723831,
-1.73778333333334)) ;
#49838 = CARTESIAN_POINT('Ctrl Pts',(0.583098022895331,1.00995540144767,-1.68486666666667)) ;
#49839 = CARTESIAN_POINT('Ctrl Pts',(0.,1.00995540144767,-1.63195000000001)) ;
#49840 = CARTESIAN_POINT('Ctrl Pts',(-0.583098022895331,1.00995540144767,
-1.57903333333334)) ;
#49841 = CARTESIAN_POINT('Ctrl Pts',(-0.874647034342996,0.504977700723831,
-1.52611666666667)) ;
#49842 = CARTESIAN_POINT('Ctrl Pts',(-1.16619604579066,-5.43898472251395E-15,
-1.47320000000001)) ;
#49843 = CARTESIAN_POINT('Ctrl Pts',(-0.874647034342996,-0.504977700723842,
-1.42028333333334)) ;
#49844 = CARTESIAN_POINT('Ctrl Pts',(-0.583098022895331,-1.00995540144768,
-1.36736666666667)) ;
#49845 = CARTESIAN_POINT('Ctrl Pts',(-1.23683864966447E-16,-1.00995540144768,
-1.31445000000001)) ;
#49846 = CARTESIAN_POINT('Ctrl Pts',(0.58309802289533,-1.00995540144768,-1.26153333333334)) ;
#49847 = CARTESIAN_POINT('Ctrl Pts',(0.874647034342996,-0.504977700723843,
-1.20861666666667)) ;
#49848 = CARTESIAN_POINT('Ctrl Pts',(1.16619604579066,-5.72462037344511E-15,
-1.15570000000001)) ;
#49849 = CARTESIAN_POINT('Ctrl Pts',(0.874647034342997,0.504977700723831,
-1.10278333333334)) ;
#49850 = CARTESIAN_POINT('Ctrl Pts',(0.583098022895331,1.00995540144767,-1.04986666666667)) ;
#49851 = CARTESIAN_POINT('Ctrl Pts',(0.,1.00995540144767,-0.996950000000008)) ;
#49852 = CARTESIAN_POINT('Ctrl Pts',(-0.583098022895331,1.00995540144767,
-0.944033333333341)) ;
#49853 = CARTESIAN_POINT('Ctrl Pts',(-0.874647034342996,0.504977700723831,
-0.891116666666674)) ;
#49854 = CARTESIAN_POINT('Ctrl Pts',(-1.16619604579066,-5.43898472251395E-15,
-0.838200000000008)) ;
#49855 = CARTESIAN_POINT('Ctrl Pts',(-0.874647034342996,-0.504977700723842,
-0.785283333333341)) ;
#49856 = CARTESIAN_POINT('Ctrl Pts',(-0.583098022895331,-1.00995540144768,
-0.732366666666674)) ;
#49857 = CARTESIAN_POINT('Ctrl Pts',(-1.23683864966447E-16,-1.00995540144768,
-0.679450000000008)) ;
#49858 = CARTESIAN_POINT('Ctrl Pts',(0.58309802289533,-1.00995540144768,-0.626533333333341)) ;
#49859 = CARTESIAN_POINT('Ctrl Pts',(0.874647034342996,-0.504977700723843,
-0.573616666666674)) ;
#49860 = CARTESIAN_POINT('Ctrl Pts',(1.16619604579066,-5.72462037344511E-15,
-0.520700000000008)) ;
#49861 = CARTESIAN_POINT('Ctrl Pts',(0.874647034342997,0.504977700723831,
-0.467783333333341)) ;
#49862 = CARTESIAN_POINT('Ctrl Pts',(0.583098022895331,1.00995540144767,-0.414866666666674)) ;
#49863 = CARTESIAN_POINT('Ctrl Pts',(0.,1.00995540144767,-0.361950000000008)) ;
#49864 = CARTESIAN_POINT('Ctrl Pts',(-0.583098022895331,1.00995540144767,
-0.309033333333341)) ;
#49865 = CARTESIAN_POINT('Ctrl Pts',(-0.874647034342996,0.504977700723831,
-0.256116666666674)) ;
#49866 = CARTESIAN_POINT('Ctrl Pts',(-1.16619604579066,-5.43898472251395E-15,
-0.203200000000008)) ;
#49867 = CARTESIAN_POINT('Ctrl Pts',(-0.874647034342996,-0.504977700723842,
-0.150283333333341)) ;
#49868 = CARTESIAN_POINT('Ctrl Pts',(-0.583098022895331,-1.00995540144768,
-0.0973666666666739)) ;
#49869 = CARTESIAN_POINT('Ctrl Pts',(-1.23683864966447E-16,-1.00995540144768,
-0.0444500000000075)) ;
#49870 = CARTESIAN_POINT('Ctrl Pts',(0.58309802289533,-1.00995540144768,0.00846666666665889)) ;
#49871 = CARTESIAN_POINT('Ctrl Pts',(0.874647034342996,-0.504977700723843,
0.0613833333333261)) ;
#49872 = CARTESIAN_POINT('Ctrl Pts',(1.16619604579066,-5.72462037344511E-15,
0.114299999999993)) ;
#49873 = CARTESIAN_POINT('Ctrl Pts',(0.874647034342997,0.504977700723831,
0.167216666666659)) ;
#49874 = CARTESIAN_POINT('Ctrl Pts',(0.583098022895331,1.00995540144767,0.220133333333326)) ;
#49875 = CARTESIAN_POINT('Ctrl Pts',(0.,1.00995540144767,0.273049999999993)) ;
#49876 = CARTESIAN_POINT('Ctrl Pts',(-0.583098022895331,1.00995540144767,
0.325966666666659)) ;
#49877 = CARTESIAN_POINT('Ctrl Pts',(-0.874647034342996,0.504977700723831,
0.378883333333326)) ;
#49878 = CARTESIAN_POINT('Ctrl Pts',(-1.16619604579066,-5.43898472251395E-15,
0.431799999999993)) ;
#49879 = CARTESIAN_POINT('Ctrl Pts',(-0.874647034342996,-0.504977700723842,
0.484716666666659)) ;
#49880 = CARTESIAN_POINT('Ctrl Pts',(-0.583098022895331,-1.00995540144768,
0.537633333333326)) ;
#49881 = CARTESIAN_POINT('Ctrl Pts',(-1.23683864966447E-16,-1.00995540144768,
0.590549999999993)) ;
#49882 = CARTESIAN_POINT('Ctrl Pts',(0.58309802289533,-1.00995540144768,0.643466666666659)) ;
#49883 = CARTESIAN_POINT('Ctrl Pts',(0.874647034342996,-0.504977700723843,
0.696383333333326)) ;
#49884 = CARTESIAN_POINT('Ctrl Pts',(1.16619604579066,-5.72462037344511E-15,
0.749299999999993)) ;
#49885 = CARTESIAN_POINT('Ctrl Pts',(0.874647034342997,0.504977700723831,
0.802216666666659)) ;
#49886 = CARTESIAN_POINT('Ctrl Pts',(0.583098022895331,1.00995540144767,0.855133333333326)) ;
#49887 = CARTESIAN_POINT('Ctrl Pts',(0.,1.00995540144767,0.908049999999993)) ;
#49888 = CARTESIAN_POINT('Ctrl Pts',(-0.583098022895331,1.00995540144767,
0.960966666666659)) ;
#49889 = CARTESIAN_POINT('Ctrl Pts',(-0.874647034342996,0.504977700723831,
1.01388333333333)) ;
#49890 = CARTESIAN_POINT('Ctrl Pts',(-1.16619604579066,-5.43898472251395E-15,
1.06679999999999)) ;
#49891 = CARTESIAN_POINT('Ctrl Pts',(-0.874647034342996,-0.504977700723842,
1.11971666666666)) ;
#49892 = CARTESIAN_POINT('Ctrl Pts',(-0.583098022895331,-1.00995540144768,
1.17263333333333)) ;
#49893 = CARTESIAN_POINT('Ctrl Pts',(-1.23683864966447E-16,-1.00995540144768,
1.22554999999999)) ;
#49894 = CARTESIAN_POINT('Ctrl Pts',(0.58309802289533,-1.00995540144768,1.27846666666666)) ;
#49895 = CARTESIAN_POINT('Ctrl Pts',(0.874647034342996,-0.504977700723843,
1.33138333333333)) ;
#49896 = CARTESIAN_POINT('Ctrl Pts',(1.00995540144771,-0.2706167342093,1.35594204380104)) ;
#49897 = CARTESIAN_POINT('Ctrl Pts',(1.00995540144767,1.23844880459077E-13,
1.38430000000001)) ;
#49898 = CARTESIAN_POINT('Ctrl Pts',(0.,1.4567703832127,-4.42991875000001)) ;
#49899 = CARTESIAN_POINT('Ctrl Pts',(-0.841066772895328,1.4567703832127,-4.37700208333334)) ;
#49900 = CARTESIAN_POINT('Ctrl Pts',(-1.26160015934299,0.728385191606346,
-4.32408541666667)) ;
#49901 = CARTESIAN_POINT('Ctrl Pts',(-1.68213354579066,-5.40739266211719E-15,
-4.27116875)) ;
#49902 = CARTESIAN_POINT('Ctrl Pts',(-1.26160015934299,-0.728385191606357,
-4.21825208333334)) ;
#49903 = CARTESIAN_POINT('Ctrl Pts',(-0.841066772895329,-1.45677038321271,
-4.16533541666667)) ;
#49904 = CARTESIAN_POINT('Ctrl Pts',(-1.7840291868941E-16,-1.45677038321271,
-4.11241875)) ;
#49905 = CARTESIAN_POINT('Ctrl Pts',(0.841066772895328,-1.45677038321271,
-4.05950208333334)) ;
#49906 = CARTESIAN_POINT('Ctrl Pts',(1.26160015934299,-0.728385191606358,
-4.00658541666667)) ;
#49907 = CARTESIAN_POINT('Ctrl Pts',(1.68213354579066,-5.81939655463538E-15,
-3.95366875000001)) ;
#49908 = CARTESIAN_POINT('Ctrl Pts',(1.26160015934299,0.728385191606345,-3.90075208333334)) ;
#49909 = CARTESIAN_POINT('Ctrl Pts',(0.841066772895329,1.4567703832127,-3.84783541666667)) ;
#49910 = CARTESIAN_POINT('Ctrl Pts',(0.,1.4567703832127,-3.79491875)) ;
#49911 = CARTESIAN_POINT('Ctrl Pts',(-0.841066772895328,1.4567703832127,-3.74200208333334)) ;
#49912 = CARTESIAN_POINT('Ctrl Pts',(-1.26160015934299,0.728385191606346,
-3.68908541666667)) ;
#49913 = CARTESIAN_POINT('Ctrl Pts',(-1.68213354579066,-5.40739266211719E-15,
-3.63616875)) ;
#49914 = CARTESIAN_POINT('Ctrl Pts',(-1.26160015934299,-0.728385191606357,
-3.58325208333334)) ;
#49915 = CARTESIAN_POINT('Ctrl Pts',(-0.841066772895329,-1.45677038321271,
-3.53033541666667)) ;
#49916 = CARTESIAN_POINT('Ctrl Pts',(-1.7840291868941E-16,-1.45677038321271,
-3.47741875)) ;
#49917 = CARTESIAN_POINT('Ctrl Pts',(0.841066772895328,-1.45677038321271,
-3.42450208333334)) ;
#49918 = CARTESIAN_POINT('Ctrl Pts',(1.26160015934299,-0.728385191606358,
-3.37158541666667)) ;
#49919 = CARTESIAN_POINT('Ctrl Pts',(1.68213354579066,-5.81939655463538E-15,
-3.31866875)) ;
#49920 = CARTESIAN_POINT('Ctrl Pts',(1.26160015934299,0.728385191606345,-3.26575208333334)) ;
#49921 = CARTESIAN_POINT('Ctrl Pts',(0.841066772895329,1.4567703832127,-3.21283541666667)) ;
#49922 = CARTESIAN_POINT('Ctrl Pts',(0.,1.4567703832127,-3.15991875)) ;
#49923 = CARTESIAN_POINT('Ctrl Pts',(-0.841066772895328,1.4567703832127,-3.10700208333334)) ;
#49924 = CARTESIAN_POINT('Ctrl Pts',(-1.26160015934299,0.728385191606346,
-3.05408541666667)) ;
#49925 = CARTESIAN_POINT('Ctrl Pts',(-1.68213354579066,-5.40739266211719E-15,
-3.00116875)) ;
#49926 = CARTESIAN_POINT('Ctrl Pts',(-1.26160015934299,-0.728385191606357,
-2.94825208333334)) ;
#49927 = CARTESIAN_POINT('Ctrl Pts',(-0.841066772895329,-1.45677038321271,
-2.89533541666667)) ;
#49928 = CARTESIAN_POINT('Ctrl Pts',(-1.7840291868941E-16,-1.45677038321271,
-2.84241875)) ;
#49929 = CARTESIAN_POINT('Ctrl Pts',(0.841066772895328,-1.45677038321271,
-2.78950208333334)) ;
#49930 = CARTESIAN_POINT('Ctrl Pts',(1.26160015934299,-0.728385191606358,
-2.73658541666667)) ;
#49931 = CARTESIAN_POINT('Ctrl Pts',(1.68213354579066,-5.81939655463538E-15,
-2.68366875)) ;
#49932 = CARTESIAN_POINT('Ctrl Pts',(1.26160015934299,0.728385191606345,-2.63075208333334)) ;
#49933 = CARTESIAN_POINT('Ctrl Pts',(0.841066772895329,1.4567703832127,-2.57783541666667)) ;
#49934 = CARTESIAN_POINT('Ctrl Pts',(0.,1.4567703832127,-2.52491875)) ;
#49935 = CARTESIAN_POINT('Ctrl Pts',(-0.841066772895328,1.4567703832127,-2.47200208333334)) ;
#49936 = CARTESIAN_POINT('Ctrl Pts',(-1.26160015934299,0.728385191606346,
-2.41908541666667)) ;
#49937 = CARTESIAN_POINT('Ctrl Pts',(-1.68213354579066,-5.40739266211719E-15,
-2.36616875)) ;
#49938 = CARTESIAN_POINT('Ctrl Pts',(-1.26160015934299,-0.728385191606357,
-2.31325208333334)) ;
#49939 = CARTESIAN_POINT('Ctrl Pts',(-0.841066772895329,-1.45677038321271,
-2.26033541666667)) ;
#49940 = CARTESIAN_POINT('Ctrl Pts',(-1.7840291868941E-16,-1.45677038321271,
-2.20741875)) ;
#49941 = CARTESIAN_POINT('Ctrl Pts',(0.841066772895328,-1.45677038321271,
-2.15450208333334)) ;
#49942 = CARTESIAN_POINT('Ctrl Pts',(1.26160015934299,-0.728385191606358,
-2.10158541666667)) ;
#49943 = CARTESIAN_POINT('Ctrl Pts',(1.68213354579066,-5.81939655463538E-15,
-2.04866875)) ;
#49944 = CARTESIAN_POINT('Ctrl Pts',(1.26160015934299,0.728385191606345,-1.99575208333334)) ;
#49945 = CARTESIAN_POINT('Ctrl Pts',(0.841066772895329,1.4567703832127,-1.94283541666667)) ;
#49946 = CARTESIAN_POINT('Ctrl Pts',(0.,1.4567703832127,-1.88991875)) ;
#49947 = CARTESIAN_POINT('Ctrl Pts',(-0.841066772895328,1.4567703832127,-1.83700208333334)) ;
#49948 = CARTESIAN_POINT('Ctrl Pts',(-1.26160015934299,0.728385191606346,
-1.78408541666667)) ;
#49949 = CARTESIAN_POINT('Ctrl Pts',(-1.68213354579066,-5.40739266211719E-15,
-1.73116875)) ;
#49950 = CARTESIAN_POINT('Ctrl Pts',(-1.26160015934299,-0.728385191606357,
-1.67825208333334)) ;
#49951 = CARTESIAN_POINT('Ctrl Pts',(-0.841066772895329,-1.45677038321271,
-1.62533541666667)) ;
#49952 = CARTESIAN_POINT('Ctrl Pts',(-1.7840291868941E-16,-1.45677038321271,
-1.57241875)) ;
#49953 = CARTESIAN_POINT('Ctrl Pts',(0.841066772895328,-1.45677038321271,
-1.51950208333334)) ;
#49954 = CARTESIAN_POINT('Ctrl Pts',(1.26160015934299,-0.728385191606358,
-1.46658541666667)) ;
#49955 = CARTESIAN_POINT('Ctrl Pts',(1.68213354579066,-5.81939655463538E-15,
-1.41366875)) ;
#49956 = CARTESIAN_POINT('Ctrl Pts',(1.26160015934299,0.728385191606345,-1.36075208333334)) ;
#49957 = CARTESIAN_POINT('Ctrl Pts',(0.841066772895329,1.4567703832127,-1.30783541666667)) ;
#49958 = CARTESIAN_POINT('Ctrl Pts',(0.,1.4567703832127,-1.25491875)) ;
#49959 = CARTESIAN_POINT('Ctrl Pts',(-0.841066772895328,1.4567703832127,-1.20200208333334)) ;
#49960 = CARTESIAN_POINT('Ctrl Pts',(-1.26160015934299,0.728385191606346,
-1.14908541666667)) ;
#49961 = CARTESIAN_POINT('Ctrl Pts',(-1.68213354579066,-5.40739266211719E-15,
-1.09616875)) ;
#49962 = CARTESIAN_POINT('Ctrl Pts',(-1.26160015934299,-0.728385191606357,
-1.04325208333334)) ;
#49963 = CARTESIAN_POINT('Ctrl Pts',(-0.841066772895329,-1.45677038321271,
-0.990335416666671)) ;
#49964 = CARTESIAN_POINT('Ctrl Pts',(-1.7840291868941E-16,-1.45677038321271,
-0.937418750000005)) ;
#49965 = CARTESIAN_POINT('Ctrl Pts',(0.841066772895328,-1.45677038321271,
-0.884502083333338)) ;
#49966 = CARTESIAN_POINT('Ctrl Pts',(1.26160015934299,-0.728385191606358,
-0.831585416666671)) ;
#49967 = CARTESIAN_POINT('Ctrl Pts',(1.68213354579066,-5.81939655463538E-15,
-0.778668750000004)) ;
#49968 = CARTESIAN_POINT('Ctrl Pts',(1.26160015934299,0.728385191606345,-0.725752083333338)) ;
#49969 = CARTESIAN_POINT('Ctrl Pts',(0.841066772895329,1.4567703832127,-0.672835416666671)) ;
#49970 = CARTESIAN_POINT('Ctrl Pts',(0.,1.4567703832127,-0.619918750000005)) ;
#49971 = CARTESIAN_POINT('Ctrl Pts',(-0.841066772895328,1.4567703832127,-0.567002083333338)) ;
#49972 = CARTESIAN_POINT('Ctrl Pts',(-1.26160015934299,0.728385191606346,
-0.514085416666671)) ;
#49973 = CARTESIAN_POINT('Ctrl Pts',(-1.68213354579066,-5.40739266211719E-15,
-0.461168750000004)) ;
#49974 = CARTESIAN_POINT('Ctrl Pts',(-1.26160015934299,-0.728385191606357,
-0.408252083333338)) ;
#49975 = CARTESIAN_POINT('Ctrl Pts',(-0.841066772895329,-1.45677038321271,
-0.355335416666671)) ;
#49976 = CARTESIAN_POINT('Ctrl Pts',(-1.7840291868941E-16,-1.45677038321271,
-0.302418750000004)) ;
#49977 = CARTESIAN_POINT('Ctrl Pts',(0.841066772895328,-1.45677038321271,
-0.249502083333338)) ;
#49978 = CARTESIAN_POINT('Ctrl Pts',(1.26160015934299,-0.728385191606358,
-0.196585416666671)) ;
#49979 = CARTESIAN_POINT('Ctrl Pts',(1.68213354579066,-5.81939655463538E-15,
-0.143668750000004)) ;
#49980 = CARTESIAN_POINT('Ctrl Pts',(1.26160015934299,0.728385191606345,-0.090752083333338)) ;
#49981 = CARTESIAN_POINT('Ctrl Pts',(0.841066772895329,1.4567703832127,-0.0378354166666707)) ;
#49982 = CARTESIAN_POINT('Ctrl Pts',(0.,1.4567703832127,0.0150812499999957)) ;
#49983 = CARTESIAN_POINT('Ctrl Pts',(-0.841066772895328,1.4567703832127,0.0679979166666621)) ;
#49984 = CARTESIAN_POINT('Ctrl Pts',(-1.26160015934299,0.728385191606346,
0.120914583333329)) ;
#49985 = CARTESIAN_POINT('Ctrl Pts',(-1.68213354579066,-5.40739266211719E-15,
0.173831249999996)) ;
#49986 = CARTESIAN_POINT('Ctrl Pts',(-1.26160015934299,-0.728385191606357,
0.226747916666662)) ;
#49987 = CARTESIAN_POINT('Ctrl Pts',(-0.841066772895329,-1.45677038321271,
0.279664583333329)) ;
#49988 = CARTESIAN_POINT('Ctrl Pts',(-1.7840291868941E-16,-1.45677038321271,
0.332581249999996)) ;
#49989 = CARTESIAN_POINT('Ctrl Pts',(0.841066772895328,-1.45677038321271,
0.385497916666662)) ;
#49990 = CARTESIAN_POINT('Ctrl Pts',(1.26160015934299,-0.728385191606358,
0.438414583333329)) ;
#49991 = CARTESIAN_POINT('Ctrl Pts',(1.68213354579066,-5.81939655463538E-15,
0.491331249999996)) ;
#49992 = CARTESIAN_POINT('Ctrl Pts',(1.26160015934299,0.728385191606345,0.544247916666662)) ;
#49993 = CARTESIAN_POINT('Ctrl Pts',(0.841066772895329,1.4567703832127,0.597164583333328)) ;
#49994 = CARTESIAN_POINT('Ctrl Pts',(0.,1.4567703832127,0.650081249999996)) ;
#49995 = CARTESIAN_POINT('Ctrl Pts',(-0.841066772895328,1.4567703832127,0.702997916666662)) ;
#49996 = CARTESIAN_POINT('Ctrl Pts',(-1.26160015934299,0.728385191606346,
0.755914583333329)) ;
#49997 = CARTESIAN_POINT('Ctrl Pts',(-1.68213354579066,-5.40739266211719E-15,
0.808831249999996)) ;
#49998 = CARTESIAN_POINT('Ctrl Pts',(-1.26160015934299,-0.728385191606357,
0.861747916666662)) ;
#49999 = CARTESIAN_POINT('Ctrl Pts',(-0.841066772895329,-1.45677038321271,
0.914664583333328)) ;
#50000 = CARTESIAN_POINT('Ctrl Pts',(-1.7840291868941E-16,-1.45677038321271,
0.967581249999996)) ;
#50001 = CARTESIAN_POINT('Ctrl Pts',(0.841066772895328,-1.45677038321271,
1.02049791666666)) ;
#50002 = CARTESIAN_POINT('Ctrl Pts',(1.26160015934299,-0.728385191606358,
1.07341458333333)) ;
#50003 = CARTESIAN_POINT('Ctrl Pts',(1.45677038321275,-0.39034044773934,1.09797329380104)) ;
#50004 = CARTESIAN_POINT('Ctrl Pts',(1.4567703832127,1.81104617588996E-13,
1.12633125000001)) ;
#50005 = CARTESIAN_POINT('Ctrl Pts',(0.,1.4567703832127,-3.83460625)) ;
#50006 = CARTESIAN_POINT('Ctrl Pts',(-0.841066772895328,1.4567703832127,-3.78168958333334)) ;
#50007 = CARTESIAN_POINT('Ctrl Pts',(-1.26160015934299,0.728385191606346,
-3.72877291666667)) ;
#50008 = CARTESIAN_POINT('Ctrl Pts',(-1.68213354579066,-5.40739266211719E-15,
-3.67585625)) ;
#50009 = CARTESIAN_POINT('Ctrl Pts',(-1.26160015934299,-0.728385191606357,
-3.62293958333334)) ;
#50010 = CARTESIAN_POINT('Ctrl Pts',(-0.841066772895329,-1.45677038321271,
-3.57002291666667)) ;
#50011 = CARTESIAN_POINT('Ctrl Pts',(-1.7840291868941E-16,-1.45677038321271,
-3.51710625)) ;
#50012 = CARTESIAN_POINT('Ctrl Pts',(0.841066772895328,-1.45677038321271,
-3.46418958333334)) ;
#50013 = CARTESIAN_POINT('Ctrl Pts',(1.26160015934299,-0.728385191606358,
-3.41127291666667)) ;
#50014 = CARTESIAN_POINT('Ctrl Pts',(1.68213354579066,-5.81939655463538E-15,
-3.35835625)) ;
#50015 = CARTESIAN_POINT('Ctrl Pts',(1.26160015934299,0.728385191606345,-3.30543958333334)) ;
#50016 = CARTESIAN_POINT('Ctrl Pts',(0.841066772895329,1.4567703832127,-3.25252291666667)) ;
#50017 = CARTESIAN_POINT('Ctrl Pts',(0.,1.4567703832127,-3.19960625)) ;
#50018 = CARTESIAN_POINT('Ctrl Pts',(-0.841066772895328,1.4567703832127,-3.14668958333334)) ;
#50019 = CARTESIAN_POINT('Ctrl Pts',(-1.26160015934299,0.728385191606346,
-3.09377291666667)) ;
#50020 = CARTESIAN_POINT('Ctrl Pts',(-1.68213354579066,-5.40739266211719E-15,
-3.04085625)) ;
#50021 = CARTESIAN_POINT('Ctrl Pts',(-1.26160015934299,-0.728385191606357,
-2.98793958333334)) ;
#50022 = CARTESIAN_POINT('Ctrl Pts',(-0.841066772895329,-1.45677038321271,
-2.93502291666667)) ;
#50023 = CARTESIAN_POINT('Ctrl Pts',(-1.7840291868941E-16,-1.45677038321271,
-2.88210625)) ;
#50024 = CARTESIAN_POINT('Ctrl Pts',(0.841066772895328,-1.45677038321271,
-2.82918958333334)) ;
#50025 = CARTESIAN_POINT('Ctrl Pts',(1.26160015934299,-0.728385191606358,
-2.77627291666667)) ;
#50026 = CARTESIAN_POINT('Ctrl Pts',(1.68213354579066,-5.81939655463538E-15,
-2.72335625)) ;
#50027 = CARTESIAN_POINT('Ctrl Pts',(1.26160015934299,0.728385191606345,-2.67043958333334)) ;
#50028 = CARTESIAN_POINT('Ctrl Pts',(0.841066772895329,1.4567703832127,-2.61752291666667)) ;
#50029 = CARTESIAN_POINT('Ctrl Pts',(0.,1.4567703832127,-2.56460625)) ;
#50030 = CARTESIAN_POINT('Ctrl Pts',(-0.841066772895328,1.4567703832127,-2.51168958333334)) ;
#50031 = CARTESIAN_POINT('Ctrl Pts',(-1.26160015934299,0.728385191606346,
-2.45877291666667)) ;
#50032 = CARTESIAN_POINT('Ctrl Pts',(-1.68213354579066,-5.40739266211719E-15,
-2.40585625)) ;
#50033 = CARTESIAN_POINT('Ctrl Pts',(-1.26160015934299,-0.728385191606357,
-2.35293958333334)) ;
#50034 = CARTESIAN_POINT('Ctrl Pts',(-0.841066772895329,-1.45677038321271,
-2.30002291666667)) ;
#50035 = CARTESIAN_POINT('Ctrl Pts',(-1.7840291868941E-16,-1.45677038321271,
-2.24710625)) ;
#50036 = CARTESIAN_POINT('Ctrl Pts',(0.841066772895328,-1.45677038321271,
-2.19418958333334)) ;
#50037 = CARTESIAN_POINT('Ctrl Pts',(1.26160015934299,-0.728385191606358,
-2.14127291666667)) ;
#50038 = CARTESIAN_POINT('Ctrl Pts',(1.68213354579066,-5.81939655463538E-15,
-2.08835625)) ;
#50039 = CARTESIAN_POINT('Ctrl Pts',(1.26160015934299,0.728385191606345,-2.03543958333334)) ;
#50040 = CARTESIAN_POINT('Ctrl Pts',(0.841066772895329,1.4567703832127,-1.98252291666667)) ;
#50041 = CARTESIAN_POINT('Ctrl Pts',(0.,1.4567703832127,-1.92960625)) ;
#50042 = CARTESIAN_POINT('Ctrl Pts',(-0.841066772895328,1.4567703832127,-1.87668958333334)) ;
#50043 = CARTESIAN_POINT('Ctrl Pts',(-1.26160015934299,0.728385191606346,
-1.82377291666667)) ;
#50044 = CARTESIAN_POINT('Ctrl Pts',(-1.68213354579066,-5.40739266211719E-15,
-1.77085625)) ;
#50045 = CARTESIAN_POINT('Ctrl Pts',(-1.26160015934299,-0.728385191606357,
-1.71793958333334)) ;
#50046 = CARTESIAN_POINT('Ctrl Pts',(-0.841066772895329,-1.45677038321271,
-1.66502291666667)) ;
#50047 = CARTESIAN_POINT('Ctrl Pts',(-1.7840291868941E-16,-1.45677038321271,
-1.61210625)) ;
#50048 = CARTESIAN_POINT('Ctrl Pts',(0.841066772895328,-1.45677038321271,
-1.55918958333334)) ;
#50049 = CARTESIAN_POINT('Ctrl Pts',(1.26160015934299,-0.728385191606358,
-1.50627291666667)) ;
#50050 = CARTESIAN_POINT('Ctrl Pts',(1.68213354579066,-5.81939655463538E-15,
-1.45335625)) ;
#50051 = CARTESIAN_POINT('Ctrl Pts',(1.26160015934299,0.728385191606345,-1.40043958333334)) ;
#50052 = CARTESIAN_POINT('Ctrl Pts',(0.841066772895329,1.4567703832127,-1.34752291666667)) ;
#50053 = CARTESIAN_POINT('Ctrl Pts',(0.,1.4567703832127,-1.29460625)) ;
#50054 = CARTESIAN_POINT('Ctrl Pts',(-0.841066772895328,1.4567703832127,-1.24168958333334)) ;
#50055 = CARTESIAN_POINT('Ctrl Pts',(-1.26160015934299,0.728385191606346,
-1.18877291666667)) ;
#50056 = CARTESIAN_POINT('Ctrl Pts',(-1.68213354579066,-5.40739266211719E-15,
-1.13585625)) ;
#50057 = CARTESIAN_POINT('Ctrl Pts',(-1.26160015934299,-0.728385191606357,
-1.08293958333334)) ;
#50058 = CARTESIAN_POINT('Ctrl Pts',(-0.841066772895329,-1.45677038321271,
-1.03002291666667)) ;
#50059 = CARTESIAN_POINT('Ctrl Pts',(-1.7840291868941E-16,-1.45677038321271,
-0.977106250000004)) ;
#50060 = CARTESIAN_POINT('Ctrl Pts',(0.841066772895328,-1.45677038321271,
-0.924189583333337)) ;
#50061 = CARTESIAN_POINT('Ctrl Pts',(1.26160015934299,-0.728385191606358,
-0.871272916666671)) ;
#50062 = CARTESIAN_POINT('Ctrl Pts',(1.68213354579066,-5.81939655463538E-15,
-0.818356250000004)) ;
#50063 = CARTESIAN_POINT('Ctrl Pts',(1.26160015934299,0.728385191606345,-0.765439583333338)) ;
#50064 = CARTESIAN_POINT('Ctrl Pts',(0.841066772895329,1.4567703832127,-0.712522916666671)) ;
#50065 = CARTESIAN_POINT('Ctrl Pts',(0.,1.4567703832127,-0.659606250000004)) ;
#50066 = CARTESIAN_POINT('Ctrl Pts',(-0.841066772895328,1.4567703832127,-0.606689583333337)) ;
#50067 = CARTESIAN_POINT('Ctrl Pts',(-1.26160015934299,0.728385191606346,
-0.553772916666671)) ;
#50068 = CARTESIAN_POINT('Ctrl Pts',(-1.68213354579066,-5.40739266211719E-15,
-0.500856250000004)) ;
#50069 = CARTESIAN_POINT('Ctrl Pts',(-1.26160015934299,-0.728385191606357,
-0.447939583333337)) ;
#50070 = CARTESIAN_POINT('Ctrl Pts',(-0.841066772895329,-1.45677038321271,
-0.395022916666671)) ;
#50071 = CARTESIAN_POINT('Ctrl Pts',(-1.7840291868941E-16,-1.45677038321271,
-0.342106250000004)) ;
#50072 = CARTESIAN_POINT('Ctrl Pts',(0.841066772895328,-1.45677038321271,
-0.289189583333337)) ;
#50073 = CARTESIAN_POINT('Ctrl Pts',(1.26160015934299,-0.728385191606358,
-0.236272916666671)) ;
#50074 = CARTESIAN_POINT('Ctrl Pts',(1.68213354579066,-5.81939655463538E-15,
-0.183356250000004)) ;
#50075 = CARTESIAN_POINT('Ctrl Pts',(1.26160015934299,0.728385191606345,-0.130439583333337)) ;
#50076 = CARTESIAN_POINT('Ctrl Pts',(0.841066772895329,1.4567703832127,-0.077522916666671)) ;
#50077 = CARTESIAN_POINT('Ctrl Pts',(0.,1.4567703832127,-0.0246062500000041)) ;
#50078 = CARTESIAN_POINT('Ctrl Pts',(-0.841066772895328,1.4567703832127,0.0283104166666627)) ;
#50079 = CARTESIAN_POINT('Ctrl Pts',(-1.26160015934299,0.728385191606346,
0.0812270833333295)) ;
#50080 = CARTESIAN_POINT('Ctrl Pts',(-1.68213354579066,-5.40739266211719E-15,
0.134143749999996)) ;
#50081 = CARTESIAN_POINT('Ctrl Pts',(-1.26160015934299,-0.728385191606357,
0.187060416666662)) ;
#50082 = CARTESIAN_POINT('Ctrl Pts',(-0.841066772895329,-1.45677038321271,
0.23997708333333)) ;
#50083 = CARTESIAN_POINT('Ctrl Pts',(-1.7840291868941E-16,-1.45677038321271,
0.292893749999996)) ;
#50084 = CARTESIAN_POINT('Ctrl Pts',(0.841066772895328,-1.45677038321271,
0.345810416666662)) ;
#50085 = CARTESIAN_POINT('Ctrl Pts',(1.26160015934299,-0.728385191606358,
0.39872708333333)) ;
#50086 = CARTESIAN_POINT('Ctrl Pts',(1.68213354579066,-5.81939655463538E-15,
0.451643749999996)) ;
#50087 = CARTESIAN_POINT('Ctrl Pts',(1.26160015934299,0.728385191606345,0.504560416666662)) ;
#50088 = CARTESIAN_POINT('Ctrl Pts',(0.841066772895329,1.4567703832127,0.55747708333333)) ;
#50089 = CARTESIAN_POINT('Ctrl Pts',(0.,1.4567703832127,0.610393749999996)) ;
#50090 = CARTESIAN_POINT('Ctrl Pts',(-0.841066772895328,1.4567703832127,0.663310416666662)) ;
#50091 = CARTESIAN_POINT('Ctrl Pts',(-1.26160015934299,0.728385191606346,
0.71622708333333)) ;
#50092 = CARTESIAN_POINT('Ctrl Pts',(-1.68213354579066,-5.40739266211719E-15,
0.769143749999996)) ;
#50093 = CARTESIAN_POINT('Ctrl Pts',(-1.26160015934299,-0.728385191606357,
0.822060416666662)) ;
#50094 = CARTESIAN_POINT('Ctrl Pts',(-0.841066772895329,-1.45677038321271,
0.87497708333333)) ;
#50095 = CARTESIAN_POINT('Ctrl Pts',(-1.7840291868941E-16,-1.45677038321271,
0.927893749999996)) ;
#50096 = CARTESIAN_POINT('Ctrl Pts',(0.841066772895328,-1.45677038321271,
0.980810416666662)) ;
#50097 = CARTESIAN_POINT('Ctrl Pts',(1.26160015934299,-0.728385191606358,
1.03372708333333)) ;
#50098 = CARTESIAN_POINT('Ctrl Pts',(1.68213354579066,-5.81939655463538E-15,
1.08664375)) ;
#50099 = CARTESIAN_POINT('Ctrl Pts',(1.26160015934299,0.728385191606345,1.13956041666666)) ;
#50100 = CARTESIAN_POINT('Ctrl Pts',(0.841066772895329,1.4567703832127,1.19247708333333)) ;
#50101 = CARTESIAN_POINT('Ctrl Pts',(0.,1.4567703832127,1.24539375)) ;
#50102 = CARTESIAN_POINT('Ctrl Pts',(-0.841066772895328,1.4567703832127,1.29831041666666)) ;
#50103 = CARTESIAN_POINT('Ctrl Pts',(-1.26160015934299,0.728385191606346,
1.35122708333333)) ;
#50104 = CARTESIAN_POINT('Ctrl Pts',(-1.68213354579066,-5.40739266211719E-15,
1.40414375)) ;
#50105 = CARTESIAN_POINT('Ctrl Pts',(-1.26160015934299,-0.728385191606357,
1.45706041666666)) ;
#50106 = CARTESIAN_POINT('Ctrl Pts',(-0.841066772895329,-1.45677038321271,
1.50997708333333)) ;
#50107 = CARTESIAN_POINT('Ctrl Pts',(-1.7840291868941E-16,-1.45677038321271,
1.56289375)) ;
#50108 = CARTESIAN_POINT('Ctrl Pts',(0.841066772895328,-1.45677038321271,
1.61581041666666)) ;
#50109 = CARTESIAN_POINT('Ctrl Pts',(1.26160015934299,-0.728385191606358,
1.66872708333333)) ;
#50110 = CARTESIAN_POINT('Ctrl Pts',(1.45677038321276,-0.390340447739336,
1.69328579380104)) ;
#50111 = CARTESIAN_POINT('Ctrl Pts',(1.4567703832127,1.90517177117201E-13,
1.72164375000001)) ;
#50112 = CARTESIAN_POINT('Ctrl Pts',(0.,1.00995540144767,-4.092575)) ;
#50113 = CARTESIAN_POINT('Ctrl Pts',(-0.583098022895331,1.00995540144767,
-4.03965833333334)) ;
#50114 = CARTESIAN_POINT('Ctrl Pts',(-0.874647034342996,0.504977700723831,
-3.98674166666667)) ;
#50115 = CARTESIAN_POINT('Ctrl Pts',(-1.16619604579066,-5.43898472251395E-15,
-3.933825)) ;
#50116 = CARTESIAN_POINT('Ctrl Pts',(-0.874647034342996,-0.504977700723842,
-3.88090833333333)) ;
#50117 = CARTESIAN_POINT('Ctrl Pts',(-0.583098022895331,-1.00995540144768,
-3.82799166666667)) ;
#50118 = CARTESIAN_POINT('Ctrl Pts',(-1.23683864966447E-16,-1.00995540144768,
-3.775075)) ;
#50119 = CARTESIAN_POINT('Ctrl Pts',(0.58309802289533,-1.00995540144768,-3.72215833333333)) ;
#50120 = CARTESIAN_POINT('Ctrl Pts',(0.874647034342996,-0.504977700723843,
-3.66924166666667)) ;
#50121 = CARTESIAN_POINT('Ctrl Pts',(1.16619604579066,-5.72462037344511E-15,
-3.616325)) ;
#50122 = CARTESIAN_POINT('Ctrl Pts',(0.874647034342997,0.504977700723831,
-3.56340833333334)) ;
#50123 = CARTESIAN_POINT('Ctrl Pts',(0.583098022895331,1.00995540144767,-3.51049166666667)) ;
#50124 = CARTESIAN_POINT('Ctrl Pts',(0.,1.00995540144767,-3.457575)) ;
#50125 = CARTESIAN_POINT('Ctrl Pts',(-0.583098022895331,1.00995540144767,
-3.40465833333333)) ;
#50126 = CARTESIAN_POINT('Ctrl Pts',(-0.874647034342996,0.504977700723831,
-3.35174166666667)) ;
#50127 = CARTESIAN_POINT('Ctrl Pts',(-1.16619604579066,-5.43898472251395E-15,
-3.298825)) ;
#50128 = CARTESIAN_POINT('Ctrl Pts',(-0.874647034342996,-0.504977700723842,
-3.24590833333334)) ;
#50129 = CARTESIAN_POINT('Ctrl Pts',(-0.583098022895331,-1.00995540144768,
-3.19299166666667)) ;
#50130 = CARTESIAN_POINT('Ctrl Pts',(-1.23683864966447E-16,-1.00995540144768,
-3.140075)) ;
#50131 = CARTESIAN_POINT('Ctrl Pts',(0.58309802289533,-1.00995540144768,-3.08715833333333)) ;
#50132 = CARTESIAN_POINT('Ctrl Pts',(0.874647034342996,-0.504977700723843,
-3.03424166666667)) ;
#50133 = CARTESIAN_POINT('Ctrl Pts',(1.16619604579066,-5.72462037344511E-15,
-2.981325)) ;
#50134 = CARTESIAN_POINT('Ctrl Pts',(0.874647034342997,0.504977700723831,
-2.92840833333333)) ;
#50135 = CARTESIAN_POINT('Ctrl Pts',(0.583098022895331,1.00995540144767,-2.87549166666667)) ;
#50136 = CARTESIAN_POINT('Ctrl Pts',(0.,1.00995540144767,-2.822575)) ;
#50137 = CARTESIAN_POINT('Ctrl Pts',(-0.583098022895331,1.00995540144767,
-2.76965833333333)) ;
#50138 = CARTESIAN_POINT('Ctrl Pts',(-0.874647034342996,0.504977700723831,
-2.71674166666667)) ;
#50139 = CARTESIAN_POINT('Ctrl Pts',(-1.16619604579066,-5.43898472251395E-15,
-2.663825)) ;
#50140 = CARTESIAN_POINT('Ctrl Pts',(-0.874647034342996,-0.504977700723842,
-2.61090833333333)) ;
#50141 = CARTESIAN_POINT('Ctrl Pts',(-0.583098022895331,-1.00995540144768,
-2.55799166666667)) ;
#50142 = CARTESIAN_POINT('Ctrl Pts',(-1.23683864966447E-16,-1.00995540144768,
-2.505075)) ;
#50143 = CARTESIAN_POINT('Ctrl Pts',(0.58309802289533,-1.00995540144768,-2.45215833333333)) ;
#50144 = CARTESIAN_POINT('Ctrl Pts',(0.874647034342996,-0.504977700723843,
-2.39924166666667)) ;
#50145 = CARTESIAN_POINT('Ctrl Pts',(1.16619604579066,-5.72462037344511E-15,
-2.346325)) ;
#50146 = CARTESIAN_POINT('Ctrl Pts',(0.874647034342997,0.504977700723831,
-2.29340833333333)) ;
#50147 = CARTESIAN_POINT('Ctrl Pts',(0.583098022895331,1.00995540144767,-2.24049166666667)) ;
#50148 = CARTESIAN_POINT('Ctrl Pts',(0.,1.00995540144767,-2.187575)) ;
#50149 = CARTESIAN_POINT('Ctrl Pts',(-0.583098022895331,1.00995540144767,
-2.13465833333333)) ;
#50150 = CARTESIAN_POINT('Ctrl Pts',(-0.874647034342996,0.504977700723831,
-2.08174166666667)) ;
#50151 = CARTESIAN_POINT('Ctrl Pts',(-1.16619604579066,-5.43898472251395E-15,
-2.028825)) ;
#50152 = CARTESIAN_POINT('Ctrl Pts',(-0.874647034342996,-0.504977700723842,
-1.97590833333333)) ;
#50153 = CARTESIAN_POINT('Ctrl Pts',(-0.583098022895331,-1.00995540144768,
-1.92299166666667)) ;
#50154 = CARTESIAN_POINT('Ctrl Pts',(-1.23683864966447E-16,-1.00995540144768,
-1.870075)) ;
#50155 = CARTESIAN_POINT('Ctrl Pts',(0.58309802289533,-1.00995540144768,-1.81715833333333)) ;
#50156 = CARTESIAN_POINT('Ctrl Pts',(0.874647034342996,-0.504977700723843,
-1.76424166666667)) ;
#50157 = CARTESIAN_POINT('Ctrl Pts',(1.16619604579066,-5.72462037344511E-15,
-1.711325)) ;
#50158 = CARTESIAN_POINT('Ctrl Pts',(0.874647034342997,0.504977700723831,
-1.65840833333333)) ;
#50159 = CARTESIAN_POINT('Ctrl Pts',(0.583098022895331,1.00995540144767,-1.60549166666667)) ;
#50160 = CARTESIAN_POINT('Ctrl Pts',(0.,1.00995540144767,-1.552575)) ;
#50161 = CARTESIAN_POINT('Ctrl Pts',(-0.583098022895331,1.00995540144767,
-1.49965833333333)) ;
#50162 = CARTESIAN_POINT('Ctrl Pts',(-0.874647034342996,0.504977700723831,
-1.44674166666667)) ;
#50163 = CARTESIAN_POINT('Ctrl Pts',(-1.16619604579066,-5.43898472251395E-15,
-1.393825)) ;
#50164 = CARTESIAN_POINT('Ctrl Pts',(-0.874647034342996,-0.504977700723842,
-1.34090833333333)) ;
#50165 = CARTESIAN_POINT('Ctrl Pts',(-0.583098022895331,-1.00995540144768,
-1.28799166666667)) ;
#50166 = CARTESIAN_POINT('Ctrl Pts',(-1.23683864966447E-16,-1.00995540144768,
-1.235075)) ;
#50167 = CARTESIAN_POINT('Ctrl Pts',(0.58309802289533,-1.00995540144768,-1.18215833333333)) ;
#50168 = CARTESIAN_POINT('Ctrl Pts',(0.874647034342996,-0.504977700723843,
-1.12924166666667)) ;
#50169 = CARTESIAN_POINT('Ctrl Pts',(1.16619604579066,-5.72462037344511E-15,
-1.076325)) ;
#50170 = CARTESIAN_POINT('Ctrl Pts',(0.874647034342997,0.504977700723831,
-1.02340833333333)) ;
#50171 = CARTESIAN_POINT('Ctrl Pts',(0.583098022895331,1.00995540144767,-0.970491666666667)) ;
#50172 = CARTESIAN_POINT('Ctrl Pts',(0.,1.00995540144767,-0.917575000000001)) ;
#50173 = CARTESIAN_POINT('Ctrl Pts',(-0.583098022895331,1.00995540144767,
-0.864658333333334)) ;
#50174 = CARTESIAN_POINT('Ctrl Pts',(-0.874647034342996,0.504977700723831,
-0.811741666666668)) ;
#50175 = CARTESIAN_POINT('Ctrl Pts',(-1.16619604579066,-5.43898472251395E-15,
-0.758825000000001)) ;
#50176 = CARTESIAN_POINT('Ctrl Pts',(-0.874647034342996,-0.504977700723842,
-0.705908333333334)) ;
#50177 = CARTESIAN_POINT('Ctrl Pts',(-0.583098022895331,-1.00995540144768,
-0.652991666666667)) ;
#50178 = CARTESIAN_POINT('Ctrl Pts',(-1.23683864966447E-16,-1.00995540144768,
-0.600075000000001)) ;
#50179 = CARTESIAN_POINT('Ctrl Pts',(0.58309802289533,-1.00995540144768,-0.547158333333334)) ;
#50180 = CARTESIAN_POINT('Ctrl Pts',(0.874647034342996,-0.504977700723843,
-0.494241666666667)) ;
#50181 = CARTESIAN_POINT('Ctrl Pts',(1.16619604579066,-5.72462037344511E-15,
-0.441325000000001)) ;
#50182 = CARTESIAN_POINT('Ctrl Pts',(0.874647034342997,0.504977700723831,
-0.388408333333334)) ;
#50183 = CARTESIAN_POINT('Ctrl Pts',(0.583098022895331,1.00995540144767,-0.335491666666668)) ;
#50184 = CARTESIAN_POINT('Ctrl Pts',(0.,1.00995540144767,-0.282575000000001)) ;
#50185 = CARTESIAN_POINT('Ctrl Pts',(-0.583098022895331,1.00995540144767,
-0.229658333333334)) ;
#50186 = CARTESIAN_POINT('Ctrl Pts',(-0.874647034342996,0.504977700723831,
-0.176741666666667)) ;
#50187 = CARTESIAN_POINT('Ctrl Pts',(-1.16619604579066,-5.43898472251395E-15,
-0.123825000000001)) ;
#50188 = CARTESIAN_POINT('Ctrl Pts',(-0.874647034342996,-0.504977700723842,
-0.0709083333333346)) ;
#50189 = CARTESIAN_POINT('Ctrl Pts',(-0.583098022895331,-1.00995540144768,
-0.0179916666666674)) ;
#50190 = CARTESIAN_POINT('Ctrl Pts',(-1.23683864966447E-16,-1.00995540144768,
0.034924999999999)) ;
#50191 = CARTESIAN_POINT('Ctrl Pts',(0.58309802289533,-1.00995540144768,0.0878416666666654)) ;
#50192 = CARTESIAN_POINT('Ctrl Pts',(0.874647034342996,-0.504977700723843,
0.140758333333333)) ;
#50193 = CARTESIAN_POINT('Ctrl Pts',(1.16619604579066,-5.72462037344511E-15,
0.193674999999999)) ;
#50194 = CARTESIAN_POINT('Ctrl Pts',(0.874647034342997,0.504977700723831,
0.246591666666665)) ;
#50195 = CARTESIAN_POINT('Ctrl Pts',(0.583098022895331,1.00995540144767,0.299508333333333)) ;
#50196 = CARTESIAN_POINT('Ctrl Pts',(0.,1.00995540144767,0.352424999999999)) ;
#50197 = CARTESIAN_POINT('Ctrl Pts',(-0.583098022895331,1.00995540144767,
0.405341666666665)) ;
#50198 = CARTESIAN_POINT('Ctrl Pts',(-0.874647034342996,0.504977700723831,
0.458258333333333)) ;
#50199 = CARTESIAN_POINT('Ctrl Pts',(-1.16619604579066,-5.43898472251395E-15,
0.511174999999999)) ;
#50200 = CARTESIAN_POINT('Ctrl Pts',(-0.874647034342996,-0.504977700723842,
0.564091666666666)) ;
#50201 = CARTESIAN_POINT('Ctrl Pts',(-0.583098022895331,-1.00995540144768,
0.617008333333333)) ;
#50202 = CARTESIAN_POINT('Ctrl Pts',(-1.23683864966447E-16,-1.00995540144768,
0.669924999999999)) ;
#50203 = CARTESIAN_POINT('Ctrl Pts',(0.58309802289533,-1.00995540144768,0.722841666666665)) ;
#50204 = CARTESIAN_POINT('Ctrl Pts',(0.874647034342996,-0.504977700723843,
0.775758333333332)) ;
#50205 = CARTESIAN_POINT('Ctrl Pts',(1.16619604579066,-5.72462037344511E-15,
0.828674999999999)) ;
#50206 = CARTESIAN_POINT('Ctrl Pts',(0.874647034342997,0.504977700723831,
0.881591666666666)) ;
#50207 = CARTESIAN_POINT('Ctrl Pts',(0.583098022895331,1.00995540144767,0.934508333333332)) ;
#50208 = CARTESIAN_POINT('Ctrl Pts',(0.,1.00995540144767,0.987424999999999)) ;
#50209 = CARTESIAN_POINT('Ctrl Pts',(-0.583098022895331,1.00995540144767,
1.04034166666667)) ;
#50210 = CARTESIAN_POINT('Ctrl Pts',(-0.874647034342996,0.504977700723831,
1.09325833333333)) ;
#50211 = CARTESIAN_POINT('Ctrl Pts',(-1.16619604579066,-5.43898472251395E-15,
1.146175)) ;
#50212 = CARTESIAN_POINT('Ctrl Pts',(-0.874647034342996,-0.504977700723842,
1.19909166666667)) ;
#50213 = CARTESIAN_POINT('Ctrl Pts',(-0.583098022895331,-1.00995540144768,
1.25200833333333)) ;
#50214 = CARTESIAN_POINT('Ctrl Pts',(-1.23683864966447E-16,-1.00995540144768,
1.304925)) ;
#50215 = CARTESIAN_POINT('Ctrl Pts',(0.58309802289533,-1.00995540144768,1.35784166666667)) ;
#50216 = CARTESIAN_POINT('Ctrl Pts',(0.874647034342996,-0.504977700723843,
1.41075833333333)) ;
#50217 = CARTESIAN_POINT('Ctrl Pts',(1.00995540144771,-0.270616734209297,
1.43531704380105)) ;
#50218 = CARTESIAN_POINT('Ctrl Pts',(1.00995540144767,1.30352329021787E-13,
1.46367500000001)) ;
#50219 = CARTESIAN_POINT('',(6.48852762540244,505.412365160566,-24.0221601717538)) ;
#50220 = CARTESIAN_POINT('',(187.388264603403,505.412365160535,-24.0203292412001)) ;
#50221 = CARTESIAN_POINT('',(6.48826460342228,617.008765160563,-24.0203292411918)) ;
#50222 = CARTESIAN_POINT('',(111.188527625421,613.758765160548,-29.5221601717566)) ;
#50223 = CARTESIAN_POINT('',(187.388264603422,617.008765160534,-24.0203292412001)) ;
#50224 = CARTESIAN_POINT('',(119.388527625403,508.662365160546,-29.522160171757)) ;
#50225 = CARTESIAN_POINT('Origin',(179.888527625416,585.710565160536,-51.0680854522974)) ;
#50226 = CARTESIAN_POINT('',(178.636459939217,587.33977480686,-47.7297342831525)) ;
#50227 = CARTESIAN_POINT('',(178.636459895391,587.339774773179,-47.671523035887)) ;
#50228 = CARTESIAN_POINT('',(178.636459914529,587.339774787887,-51.0680854522974)) ;
#50229 = CARTESIAN_POINT('',(178.005900115752,584.887332980433,-47.5221601717597)) ;
#50230 = CARTESIAN_POINT('Ctrl Pts',(178.636459895391,587.339774773179,-47.6715230358871)) ;
#50231 = CARTESIAN_POINT('Ctrl Pts',(178.622051948503,587.328702087864,-47.6704668912743)) ;
#50232 = CARTESIAN_POINT('Ctrl Pts',(178.607789560242,587.317437260344,-47.6694051968374)) ;
#50233 = CARTESIAN_POINT('Ctrl Pts',(178.487045236967,587.219440421823,-47.6602809317652)) ;
#50234 = CARTESIAN_POINT('Ctrl Pts',(178.389364918817,587.12243134586,-47.6519504773091)) ;
#50235 = CARTESIAN_POINT('Ctrl Pts',(178.270018935768,586.97744097979,-47.6409601002178)) ;
#50236 = CARTESIAN_POINT('Ctrl Pts',(178.239388517243,586.937302978343,-47.6380533492227)) ;
#50237 = CARTESIAN_POINT('Ctrl Pts',(178.193017158957,586.87165754715,-47.6335619409714)) ;
#50238 = CARTESIAN_POINT('Ctrl Pts',(178.176303322685,586.846865984155,-47.6319234492914)) ;
#50239 = CARTESIAN_POINT('Ctrl Pts',(178.13743793732,586.786410828827,-47.6280712936817)) ;
#50240 = CARTESIAN_POINT('Ctrl Pts',(178.11582742136,586.750417784659,-47.6258889309011)) ;
#50241 = CARTESIAN_POINT('Ctrl Pts',(178.041476930324,586.61752088359,-47.6181384242265)) ;
#50242 = CARTESIAN_POINT('Ctrl Pts',(177.99545548892,586.517067886397,-47.6128483931015)) ;
#50243 = CARTESIAN_POINT('Ctrl Pts',(177.913341108927,586.291485316647,-47.601291085922)) ;
#50244 = CARTESIAN_POINT('Ctrl Pts',(177.880612878398,586.165652951717,-47.5950305003944)) ;
#50245 = CARTESIAN_POINT('Ctrl Pts',(177.850497749422,585.97884066761,-47.5853775866719)) ;
#50246 = CARTESIAN_POINT('Ctrl Pts',(177.843585084823,585.919722142574,-47.5822759537453)) ;
#50247 = CARTESIAN_POINT('Ctrl Pts',(177.835183898614,585.804812341749,-47.576118591322)) ;
#50248 = CARTESIAN_POINT('Ctrl Pts',(177.833383449117,585.749095971256,-47.5730751020488)) ;
#50249 = CARTESIAN_POINT('Ctrl Pts',(177.834968265367,585.559629255589,-47.5625121835925)) ;
#50250 = CARTESIAN_POINT('Ctrl Pts',(177.849141441219,585.426323248145,-47.5546957485577)) ;
#50251 = CARTESIAN_POINT('Ctrl Pts',(177.896728318326,585.1956967431,-47.5408154361288)) ;
#50252 = CARTESIAN_POINT('Ctrl Pts',(177.924657234882,585.097736004592,-47.5348091115553)) ;
#50253 = CARTESIAN_POINT('Ctrl Pts',(177.967607229132,584.980780886296,-47.527743521705)) ;
#50254 = CARTESIAN_POINT('Ctrl Pts',(177.975846412108,584.95945204961,-47.5264597113805)) ;
#50255 = CARTESIAN_POINT('Ctrl Pts',(177.991364576761,584.921192414976,-47.5241702591099)) ;
#50256 = CARTESIAN_POINT('Ctrl Pts',(177.998518536886,584.904213714415,-47.5231591248557)) ;
#50257 = CARTESIAN_POINT('Ctrl Pts',(178.005900115752,584.887332980433,-47.5221601717597)) ;
#50258 = CARTESIAN_POINT('',(178.665796911972,584.056482856676,-47.523444591023)) ;
#50259 = CARTESIAN_POINT('Origin',(179.888527625416,585.710565160536,-47.5221601717598)) ;
#50260 = CARTESIAN_POINT('Ctrl Pts',(178.666885451598,584.058418689533,-47.5247290102857)) ;
#50261 = CARTESIAN_POINT('Ctrl Pts',(178.653511313722,584.068307891946,-47.525627662434)) ;
#50262 = CARTESIAN_POINT('Ctrl Pts',(178.640257270952,584.078359478669,-47.5265153396178)) ;
#50263 = CARTESIAN_POINT('Ctrl Pts',(178.609645663288,584.102165685899,-47.5285624606179)) ;
#50264 = CARTESIAN_POINT('Ctrl Pts',(178.592385307971,584.116042314304,-47.5297143830976)) ;
#50265 = CARTESIAN_POINT('Ctrl Pts',(178.481292589341,584.20835253247,-47.5371376308387)) ;
#50266 = CARTESIAN_POINT('Ctrl Pts',(178.394389987336,584.294757521546,-47.542999568097)) ;
#50267 = CARTESIAN_POINT('Ctrl Pts',(178.239218126975,584.479347585433,-47.5546974006364)) ;
#50268 = CARTESIAN_POINT('Ctrl Pts',(178.170792702272,584.576765419694,-47.5605112595867)) ;
#50269 = CARTESIAN_POINT('Ctrl Pts',(178.084524128559,584.725481636807,-47.5693820913402)) ;
#50270 = CARTESIAN_POINT('Ctrl Pts',(178.0596681154,584.772433838276,-47.5721793006139)) ;
#50271 = CARTESIAN_POINT('Ctrl Pts',(178.013698342065,584.868056265502,-47.5778991786517)) ;
#50272 = CARTESIAN_POINT('Ctrl Pts',(177.992594836705,584.916685944811,-47.5808193878186)) ;
#50273 = CARTESIAN_POINT('Ctrl Pts',(177.933181634483,585.06952069295,-47.5900474878534)) ;
#50274 = CARTESIAN_POINT('Ctrl Pts',(177.901420110829,585.176042772451,-47.596561393858)) ;
#50275 = CARTESIAN_POINT('Ctrl Pts',(177.85864488408,585.377895156172,-47.6088857426835)) ;
#50276 = CARTESIAN_POINT('Ctrl Pts',(177.845393105198,585.472458198085,-47.6146479075646)) ;
#50277 = CARTESIAN_POINT('Ctrl Pts',(177.835876382909,585.60890486476,-47.6227188470256)) ;
#50278 = CARTESIAN_POINT('Ctrl Pts',(177.834244503055,585.650289489834,-47.6251338894464)) ;
#50279 = CARTESIAN_POINT('Ctrl Pts',(177.833548232647,585.726111104898,-47.629466674811)) ;
#50280 = CARTESIAN_POINT('Ctrl Pts',(177.834096847837,585.760529887158,-47.6313988241779)) ;
#50281 = CARTESIAN_POINT('Ctrl Pts',(177.836784129112,585.825931992355,-47.6349835616902)) ;
#50282 = CARTESIAN_POINT('Ctrl Pts',(177.838760818321,585.856910608852,-47.6366427024279)) ;
#50283 = CARTESIAN_POINT('Ctrl Pts',(177.847662721803,585.959709543268,-47.6420513037143)) ;
#50284 = CARTESIAN_POINT('Ctrl Pts',(177.857668629265,586.031214532293,-47.6456573976396)) ;
#50285 = CARTESIAN_POINT('Ctrl Pts',(177.903134627704,586.265476184802,-47.6573654666969)) ;
#50286 = CARTESIAN_POINT('Ctrl Pts',(177.954593475042,586.424435928558,-47.6651906308011)) ;
#50287 = CARTESIAN_POINT('Ctrl Pts',(178.049939653255,586.629910935619,-47.6766599426331)) ;
#50288 = CARTESIAN_POINT('Ctrl Pts',(178.077584741966,586.683235374413,-47.6797657868005)) ;
#50289 = CARTESIAN_POINT('Ctrl Pts',(178.132378598873,586.778470706083,-47.6856030880404)) ;
#50290 = CARTESIAN_POINT('Ctrl Pts',(178.158796050686,586.820749708351,-47.6883063300768)) ;
#50291 = CARTESIAN_POINT('Ctrl Pts',(178.22743122292,586.922189413675,-47.6950902412122)) ;
#50292 = CARTESIAN_POINT('Ctrl Pts',(178.271297572279,586.980147673663,-47.699231731675)) ;
#50293 = CARTESIAN_POINT('Ctrl Pts',(178.413054389223,587.148146249744,-47.7120490358254)) ;
#50294 = CARTESIAN_POINT('Ctrl Pts',(178.519774316991,587.250100468531,-47.7210107004045)) ;
#50295 = CARTESIAN_POINT('Ctrl Pts',(178.636459939217,587.33977480686,-47.7297342831524)) ;
#50296 = CARTESIAN_POINT('Origin',(179.888527625416,585.710565160536,-51.0680854522974)) ;
#50297 = CARTESIAN_POINT('',(178.636459914536,587.339774787892,-48.4293959864655)) ;
#50298 = CARTESIAN_POINT('',(178.636459914529,587.339774787887,-48.3712343220044)) ;
#50299 = CARTESIAN_POINT('',(178.636459914529,587.339774787887,-51.0680854522974)) ;
#50300 = CARTESIAN_POINT('',(181.94327755488,585.71002676683,-47.9194602314969)) ;
#50301 = CARTESIAN_POINT('Ctrl Pts',(178.636459914529,587.339774787887,-48.3712343220044)) ;
#50302 = CARTESIAN_POINT('Ctrl Pts',(178.616732770872,587.324614234459,-48.3699812011576)) ;
#50303 = CARTESIAN_POINT('Ctrl Pts',(178.597273587933,587.309089704676,-48.3687167206434)) ;
#50304 = CARTESIAN_POINT('Ctrl Pts',(178.535957355158,587.258319596,-48.3646324682209)) ;
#50305 = CARTESIAN_POINT('Ctrl Pts',(178.49523514045,587.221765161574,-48.3617663414953)) ;
#50306 = CARTESIAN_POINT('Ctrl Pts',(178.418883875532,587.147516231435,-48.3560489276152)) ;
#50307 = CARTESIAN_POINT('Ctrl Pts',(178.383127531142,587.110011835591,-48.3532070584353)) ;
#50308 = CARTESIAN_POINT('Ctrl Pts',(178.285318242291,586.999330403391,-48.3449298370018)) ;
#50309 = CARTESIAN_POINT('Ctrl Pts',(178.226925342831,586.923112147398,-48.3393511592422)) ;
#50310 = CARTESIAN_POINT('Ctrl Pts',(178.098656363484,586.728936491659,-48.3255182844141)) ;
#50311 = CARTESIAN_POINT('Ctrl Pts',(178.034833883732,586.607525688292,-48.3171593759884)) ;
#50312 = CARTESIAN_POINT('Ctrl Pts',(177.966076214654,586.437443706439,-48.3064290896158)) ;
#50313 = CARTESIAN_POINT('Ctrl Pts',(177.950075089051,586.393627581319,-48.303749038531)) ;
#50314 = CARTESIAN_POINT('Ctrl Pts',(177.926513557381,586.321587738282,-48.2995201732169)) ;
#50315 = CARTESIAN_POINT('Ctrl Pts',(177.918040449193,586.293684649819,-48.2979262294828)) ;
#50316 = CARTESIAN_POINT('Ctrl Pts',(177.898407146047,586.223704463639,-48.2940379135337)) ;
#50317 = CARTESIAN_POINT('Ctrl Pts',(177.887984843604,586.181437314423,-48.2917817422532)) ;
#50318 = CARTESIAN_POINT('Ctrl Pts',(177.866532065166,586.080779991881,-48.2865581034063)) ;
#50319 = CARTESIAN_POINT('Ctrl Pts',(177.856675638199,586.022179185615,-48.283633345089)) ;
#50320 = CARTESIAN_POINT('Ctrl Pts',(177.828623120527,585.795779535687,-48.2725167961253)) ;
#50321 = CARTESIAN_POINT('Ctrl Pts',(177.82857950266,585.626422692747,-48.2645227019426)) ;
#50322 = CARTESIAN_POINT('Ctrl Pts',(177.85586501095,585.405265518843,-48.2530683432249)) ;
#50323 = CARTESIAN_POINT('Ctrl Pts',(177.864608379056,585.351851706924,-48.2502282743187)) ;
#50324 = CARTESIAN_POINT('Ctrl Pts',(177.885916441807,585.247666537071,-48.2445106014221)) ;
#50325 = CARTESIAN_POINT('Ctrl Pts',(177.898331449846,585.196906556028,-48.2416398273973)) ;
#50326 = CARTESIAN_POINT('Ctrl Pts',(177.940788212944,585.048138059375,-48.2329551796179)) ;
#50327 = CARTESIAN_POINT('Ctrl Pts',(177.97623875876,584.951852304478,-48.2269703149639)) ;
#50328 = CARTESIAN_POINT('Ctrl Pts',(178.074597442009,584.735978691476,-48.2128257421043)) ;
#50329 = CARTESIAN_POINT('Ctrl Pts',(178.14240753163,584.619131848229,-48.204600120584)) ;
#50330 = CARTESIAN_POINT('Ctrl Pts',(178.24625653502,584.474933400225,-48.1942621728566)) ;
#50331 = CARTESIAN_POINT('Ctrl Pts',(178.272429697812,584.440892678788,-48.1918088082005)) ;
#50332 = CARTESIAN_POINT('Ctrl Pts',(178.318180262506,584.385098984106,-48.1877999845216)) ;
#50333 = CARTESIAN_POINT('Ctrl Pts',(178.337186839399,584.362902980642,-48.18621087511)) ;
#50334 = CARTESIAN_POINT('Ctrl Pts',(178.388377929359,584.305640700901,-48.1821201130052)) ;
#50335 = CARTESIAN_POINT('Ctrl Pts',(178.421317200854,584.271275027624,-48.1796696874536)) ;
#50336 = CARTESIAN_POINT('Ctrl Pts',(178.504763121472,584.190060672954,-48.1737998996133)) ;
#50337 = CARTESIAN_POINT('Ctrl Pts',(178.556488879704,584.144547337068,-48.1704397252974)) ;
#50338 = CARTESIAN_POINT('Ctrl Pts',(178.729431106123,584.007156360584,-48.1597264770878)) ;
#50339 = CARTESIAN_POINT('Ctrl Pts',(178.858572523721,583.926105746112,-48.1524478137044)) ;
#50340 = CARTESIAN_POINT('Ctrl Pts',(179.044017713304,583.836610388659,-48.141857130019)) ;
#50341 = CARTESIAN_POINT('Ctrl Pts',(179.093466176679,583.815102140579,-48.1390260709258)) ;
#50342 = CARTESIAN_POINT('Ctrl Pts',(179.192436484254,583.776608278394,-48.133313773514)) ;
#50343 = CARTESIAN_POINT('Ctrl Pts',(179.241874965903,583.759521407952,-48.1304387269888)) ;
#50344 = CARTESIAN_POINT('Ctrl Pts',(179.391229339971,583.714202241957,-48.1216725489935)) ;
#50345 = CARTESIAN_POINT('Ctrl Pts',(179.492678663355,583.691637391317,-48.1156042010222)) ;
#50346 = CARTESIAN_POINT('Ctrl Pts',(179.728553311563,583.657638598557,-48.101381247454)) ;
#50347 = CARTESIAN_POINT('Ctrl Pts',(179.863282043351,583.651569615006,-48.0931669054093)) ;
#50348 = CARTESIAN_POINT('Ctrl Pts',(180.039958209376,583.660964602471,-48.0828789164744)) ;
#50349 = CARTESIAN_POINT('Ctrl Pts',(180.082202386195,583.664524036193,-48.0804580024299)) ;
#50350 = CARTESIAN_POINT('Ctrl Pts',(180.153271647572,583.672733423954,-48.0764846107144)) ;
#50351 = CARTESIAN_POINT('Ctrl Pts',(180.182157092363,583.6766945972,-48.0748998497865)) ;
#50352 = CARTESIAN_POINT('Ctrl Pts',(180.258192238367,583.688775492105,-48.0708011130373)) ;
#50353 = CARTESIAN_POINT('Ctrl Pts',(180.305158046741,583.697928790143,-48.0683394527122)) ;
#50354 = CARTESIAN_POINT('Ctrl Pts',(180.419476518232,583.724382584651,-48.0624282559596)) ;
#50355 = CARTESIAN_POINT('Ctrl Pts',(180.486353181931,583.743477588543,-48.0590392477585)) ;
#50356 = CARTESIAN_POINT('Ctrl Pts',(180.694272382868,583.814430075535,-48.0483888442308)) ;
#50357 = CARTESIAN_POINT('Ctrl Pts',(180.830650194738,583.878365781271,-48.0411953677898)) ;
#50358 = CARTESIAN_POINT('Ctrl Pts',(181.004812856034,583.984643594465,-48.0307080167695)) ;
#50359 = CARTESIAN_POINT('Ctrl Pts',(181.04966096301,584.014491273626,-48.0278813501209)) ;
#50360 = CARTESIAN_POINT('Ctrl Pts',(181.135276784856,584.076459447805,-48.0221990740497)) ;
#50361 = CARTESIAN_POINT('Ctrl Pts',(181.176102652813,584.108430709867,-48.0193506201744)) ;
#50362 = CARTESIAN_POINT('Ctrl Pts',(181.291326405921,584.205914651208,-48.0108786437663)) ;
#50363 = CARTESIAN_POINT('Ctrl Pts',(181.362240599236,584.275300928053,-48.0050970984169)) ;
#50364 = CARTESIAN_POINT('Ctrl Pts',(181.518388855748,584.451904723304,-47.9910442369297)) ;
#50365 = CARTESIAN_POINT('Ctrl Pts',(181.598469878208,584.563058691308,-47.9826831206871)) ;
#50366 = CARTESIAN_POINT('Ctrl Pts',(181.689454312248,584.720270284086,-47.9720696293225)) ;
#50367 = CARTESIAN_POINT('Ctrl Pts',(181.710702755804,584.759934171019,-47.9694875488808)) ;
#50368 = CARTESIAN_POINT('Ctrl Pts',(181.743589097101,584.826483883817,-47.965349145489)) ;
#50369 = CARTESIAN_POINT('Ctrl Pts',(181.755982737469,584.852972977259,-47.9637529047783)) ;
#50370 = CARTESIAN_POINT('Ctrl Pts',(181.786209978292,584.921343895791,-47.959757070883)) ;
#50371 = CARTESIAN_POINT('Ctrl Pts',(181.803224687991,584.963568325523,-47.9574015053188)) ;
#50372 = CARTESIAN_POINT('Ctrl Pts',(181.840670292856,585.066205485159,-47.9518637578263)) ;
#50373 = CARTESIAN_POINT('Ctrl Pts',(181.859719488281,585.127072365383,-47.9487308504889)) ;
#50374 = CARTESIAN_POINT('Ctrl Pts',(181.908742796499,585.313774658712,-47.9393219140778)) ;
#50375 = CARTESIAN_POINT('Ctrl Pts',(181.929700552961,585.441634024675,-47.933129186118)) ;
#50376 = CARTESIAN_POINT('Ctrl Pts',(181.94167411048,585.617020177267,-47.924269032645)) ;
#50377 = CARTESIAN_POINT('Ctrl Pts',(181.943265368409,585.663517772867,-47.9218881440502)) ;
#50378 = CARTESIAN_POINT('Ctrl Pts',(181.94327755488,585.71002676683,-47.9194602314969)) ;
#50379 = CARTESIAN_POINT('Ctrl Pts',(181.943277555182,585.710027921507,-47.9194601712192)) ;
#50380 = CARTESIAN_POINT('Ctrl Pts',(181.943288990901,585.753765513704,-47.9171769336477)) ;
#50381 = CARTESIAN_POINT('Ctrl Pts',(181.941903931433,585.797490452821,-47.9148533307488)) ;
#50382 = CARTESIAN_POINT('Ctrl Pts',(181.935789748451,585.893512517472,-47.9096434456928)) ;
#50383 = CARTESIAN_POINT('Ctrl Pts',(181.93044953608,585.945737714692,-47.906739351913)) ;
#50384 = CARTESIAN_POINT('Ctrl Pts',(181.899647721926,586.163995586748,-47.8942856313623)) ;
#50385 = CARTESIAN_POINT('Ctrl Pts',(181.855881423971,586.326767122333,-47.8841510595223)) ;
#50386 = CARTESIAN_POINT('Ctrl Pts',(181.75964674558,586.564209951801,-47.8687596087727)) ;
#50387 = CARTESIAN_POINT('Ctrl Pts',(181.721231234971,586.643836981885,-47.8634994713564)) ;
#50388 = CARTESIAN_POINT('Ctrl Pts',(181.661916626856,586.748897381278,-47.8566364834576)) ;
#50389 = CARTESIAN_POINT('Ctrl Pts',(181.645362047115,586.77666813238,-47.8548307418738)) ;
#50390 = CARTESIAN_POINT('Ctrl Pts',(181.610228564451,586.832562699905,-47.8512317357504)) ;
#50391 = CARTESIAN_POINT('Ctrl Pts',(181.591599632597,586.860642824386,-47.8494417739713)) ;
#50392 = CARTESIAN_POINT('Ctrl Pts',(181.499143100928,586.992829358914,-47.8410397257878)) ;
#50393 = CARTESIAN_POINT('Ctrl Pts',(181.416407412661,587.090374540805,-47.8349004729119)) ;
#50394 = CARTESIAN_POINT('Ctrl Pts',(181.238320119738,587.264529957423,-47.8227993555768)) ;
#50395 = CARTESIAN_POINT('Ctrl Pts',(181.144140809479,587.341570526276,-47.816862729015)) ;
#50396 = CARTESIAN_POINT('Ctrl Pts',(180.999202436521,587.440101645439,-47.8078192845947)) ;
#50397 = CARTESIAN_POINT('Ctrl Pts',(180.953518174105,587.468600829704,-47.8049837135906)) ;
#50398 = CARTESIAN_POINT('Ctrl Pts',(180.860202423943,587.521840987488,-47.7991886966417)) ;
#50399 = CARTESIAN_POINT('Ctrl Pts',(180.81261595788,587.546574972235,-47.7962320466396)) ;
#50400 = CARTESIAN_POINT('Ctrl Pts',(180.661739375481,587.617643700048,-47.7868355248201)) ;
#50401 = CARTESIAN_POINT('Ctrl Pts',(180.555562932533,587.657322204198,-47.7801787748269)) ;
#50402 = CARTESIAN_POINT('Ctrl Pts',(180.355034759728,587.713921164562,-47.7677030782489)) ;
#50403 = CARTESIAN_POINT('Ctrl Pts',(180.261708858907,587.733385049441,-47.7619375674298)) ;
#50404 = CARTESIAN_POINT('Ctrl Pts',(180.111160795272,587.754006052561,-47.7529542111146)) ;
#50405 = CARTESIAN_POINT('Ctrl Pts',(180.054653005402,587.759374472618,-47.7496539479627)) ;
#50406 = CARTESIAN_POINT('Ctrl Pts',(179.968584681763,587.763966155414,-47.7448051540227)) ;
#50407 = CARTESIAN_POINT('Ctrl Pts',(179.939144838034,587.764902772479,-47.7431783160048)) ;
#50408 = CARTESIAN_POINT('Ctrl Pts',(179.875210140234,587.765561347818,-47.7397285817788)) ;
#50409 = CARTESIAN_POINT('Ctrl Pts',(179.840722482333,587.765048471467,-47.7379186989338)) ;
#50410 = CARTESIAN_POINT('Ctrl Pts',(179.693339667233,587.759142986261,-47.7303405527453)) ;
#50411 = CARTESIAN_POINT('Ctrl Pts',(179.580971023856,587.745309284466,-47.7249485680904)) ;
#50412 = CARTESIAN_POINT('Ctrl Pts',(179.33415706429,587.693998335569,-47.7129334424596)) ;
#50413 = CARTESIAN_POINT('Ctrl Pts',(179.201250395347,587.651951304077,-47.7063258665227)) ;
#50414 = CARTESIAN_POINT('Ctrl Pts',(179.022503689492,587.574727072608,-47.6964391260437)) ;
#50415 = CARTESIAN_POINT('Ctrl Pts',(178.972318281831,587.550580578585,-47.6935484885674)) ;
#50416 = CARTESIAN_POINT('Ctrl Pts',(178.879111969972,587.500975565246,-47.6879243501719)) ;
#50417 = CARTESIAN_POINT('Ctrl Pts',(178.835918336567,587.475927004888,-47.685207514099)) ;
#50418 = CARTESIAN_POINT('Ctrl Pts',(178.739586813696,587.415270144877,-47.678880404289)) ;
#50419 = CARTESIAN_POINT('Ctrl Pts',(178.687123423991,587.378710321286,-47.675236820593)) ;
#50420 = CARTESIAN_POINT('Ctrl Pts',(178.636459895391,587.339774773179,-47.6715230358871)) ;
#50421 = CARTESIAN_POINT('Ctrl Pts',(178.636459939217,587.33977480686,-47.7297342831524)) ;
#50422 = CARTESIAN_POINT('Ctrl Pts',(178.685121246926,587.377171621376,-47.7333722715894)) ;
#50423 = CARTESIAN_POINT('Ctrl Pts',(178.735429412256,587.412367062688,-47.7369561190645)) ;
#50424 = CARTESIAN_POINT('Ctrl Pts',(178.809385083481,587.459317969666,-47.7418993910626)) ;
#50425 = CARTESIAN_POINT('Ctrl Pts',(178.831788584265,587.472946435851,-47.743356368714)) ;
#50426 = CARTESIAN_POINT('Ctrl Pts',(178.882639345079,587.502561434873,-47.7465626887374)) ;
#50427 = CARTESIAN_POINT('Ctrl Pts',(178.91121922827,587.518306956344,-47.7482956410734)) ;
#50428 = CARTESIAN_POINT('Ctrl Pts',(179.062994969881,587.597272621547,-47.757204387362)) ;
#50429 = CARTESIAN_POINT('Ctrl Pts',(179.191986039724,587.648607440626,-47.7637955950988)) ;
#50430 = CARTESIAN_POINT('Ctrl Pts',(179.403531539794,587.708918365324,-47.7744335276501)) ;
#50431 = CARTESIAN_POINT('Ctrl Pts',(179.483146674648,587.726576573746,-47.7783973377741)) ;
#50432 = CARTESIAN_POINT('Ctrl Pts',(179.627946151611,587.749766461961,-47.7857484251801)) ;
#50433 = CARTESIAN_POINT('Ctrl Pts',(179.692744623988,587.757004154329,-47.7890872707027)) ;
#50434 = CARTESIAN_POINT('Ctrl Pts',(179.806922777768,587.764284630978,-47.7951226952449)) ;
#50435 = CARTESIAN_POINT('Ctrl Pts',(179.856165259636,587.76565034262,-47.7977745711824)) ;
#50436 = CARTESIAN_POINT('Ctrl Pts',(179.969551834077,587.764718888585,-47.8040120431308)) ;
#50437 = CARTESIAN_POINT('Ctrl Pts',(180.033631541949,587.761188487531,-47.8076345366458)) ;
#50438 = CARTESIAN_POINT('Ctrl Pts',(180.244234576702,587.739664676921,-47.8198607373283)) ;
#50439 = CARTESIAN_POINT('Ctrl Pts',(180.388978726142,587.70889252268,-47.8288161444471)) ;
#50440 = CARTESIAN_POINT('Ctrl Pts',(180.602059547016,587.638972966298,-47.8422324087778)) ;
#50441 = CARTESIAN_POINT('Ctrl Pts',(180.673570674285,587.610984552505,-47.8467682387898)) ;
#50442 = CARTESIAN_POINT('Ctrl Pts',(180.77191781701,587.565991261117,-47.8529028490711)) ;
#50443 = CARTESIAN_POINT('Ctrl Pts',(180.800181215274,587.552268814845,-47.8546528564018)) ;
#50444 = CARTESIAN_POINT('Ctrl Pts',(180.857994067106,587.522542170704,-47.8581884581791)) ;
#50445 = CARTESIAN_POINT('Ctrl Pts',(180.887487456895,587.506450850997,-47.8599687544073)) ;
#50446 = CARTESIAN_POINT('Ctrl Pts',(181.027472061702,587.42556016813,-47.8683679266912)) ;
#50447 = CARTESIAN_POINT('Ctrl Pts',(181.132146775073,587.351242068804,-47.8745059408282)) ;
#50448 = CARTESIAN_POINT('Ctrl Pts',(181.322303135832,587.187511707329,-47.8866473468647)) ;
#50449 = CARTESIAN_POINT('Ctrl Pts',(181.408000507189,587.099191091871,-47.8926264083878)) ;
#50450 = CARTESIAN_POINT('Ctrl Pts',(181.518932709314,586.962217579984,-47.9016958987071)) ;
#50451 = CARTESIAN_POINT('Ctrl Pts',(181.550936707775,586.91938684467,-47.9045039576313)) ;
#50452 = CARTESIAN_POINT('Ctrl Pts',(181.610732168192,586.832490746178,-47.910178771066)) ;
#50453 = CARTESIAN_POINT('Ctrl Pts',(181.638590046267,586.788519857356,-47.9130399002851)) ;
#50454 = CARTESIAN_POINT('Ctrl Pts',(181.755704513453,586.587139645176,-47.9261227425133)) ;
#50455 = CARTESIAN_POINT('Ctrl Pts',(181.825592849092,586.419429188602,-47.9370595229622)) ;
#50456 = CARTESIAN_POINT('Ctrl Pts',(181.887379883498,586.189951930345,-47.9512949238449)) ;
#50457 = CARTESIAN_POINT('Ctrl Pts',(181.89986481163,586.134529058559,-47.9546712369496)) ;
#50458 = CARTESIAN_POINT('Ctrl Pts',(181.917608862202,586.037081332327,-47.9604290658585)) ;
#50459 = CARTESIAN_POINT('Ctrl Pts',(181.923895539515,585.995278086389,-47.9628425815576)) ;
#50460 = CARTESIAN_POINT('Ctrl Pts',(181.932320421659,585.924463173431,-47.9668031182439)) ;
#50461 = CARTESIAN_POINT('Ctrl Pts',(181.935139833815,585.89555156452,-47.9683822080552)) ;
#50462 = CARTESIAN_POINT('Ctrl Pts',(181.940953881478,585.819202681555,-47.972459522156)) ;
#50463 = CARTESIAN_POINT('Ctrl Pts',(181.942917584158,585.771706060209,-47.974906408834)) ;
#50464 = CARTESIAN_POINT('Ctrl Pts',(181.944140632089,585.587138683429,-47.9842104124131)) ;
#50465 = CARTESIAN_POINT('Ctrl Pts',(181.931336410573,585.450342006926,-47.9906895499841)) ;
#50466 = CARTESIAN_POINT('Ctrl Pts',(181.886883181918,585.223254546101,-48.0019933683402)) ;
#50467 = CARTESIAN_POINT('Ctrl Pts',(181.862408409543,585.132042235162,-48.0066859319288)) ;
#50468 = CARTESIAN_POINT('Ctrl Pts',(181.815029468638,584.99415895087,-48.0142488882546)) ;
#50469 = CARTESIAN_POINT('Ctrl Pts',(181.796479679247,584.946127110689,-48.0169744114881)) ;
#50470 = CARTESIAN_POINT('Ctrl Pts',(181.754646973934,584.848846994174,-48.0227102638407)) ;
#50471 = CARTESIAN_POINT('Ctrl Pts',(181.731170387928,584.799726827208,-48.0257257385062)) ;
#50472 = CARTESIAN_POINT('Ctrl Pts',(181.627255775538,584.602808025621,-48.0383298795153)) ;
#50473 = CARTESIAN_POINT('Ctrl Pts',(181.530770202985,584.464241040989,-48.048497541916)) ;
#50474 = CARTESIAN_POINT('Ctrl Pts',(181.379537424341,584.295540354759,-48.0620831337559)) ;
#50475 = CARTESIAN_POINT('Ctrl Pts',(181.338733810148,584.253750790581,-48.0655596198017)) ;
#50476 = CARTESIAN_POINT('Ctrl Pts',(181.264880107449,584.184295057971,-48.0714613126554)) ;
#50477 = CARTESIAN_POINT('Ctrl Pts',(181.232636586987,584.15582459596,-48.0739205583258)) ;
#50478 = CARTESIAN_POINT('Ctrl Pts',(181.177209693695,584.109897904425,-48.0779225835602)) ;
#50479 = CARTESIAN_POINT('Ctrl Pts',(181.154511533064,584.091886053223,-48.0794998337636)) ;
#50480 = CARTESIAN_POINT('Ctrl Pts',(181.094518301859,584.046313554621,-48.0835163547645)) ;
#50481 = CARTESIAN_POINT('Ctrl Pts',(181.056659362174,584.019525305305,-48.0859079033304)) ;
#50482 = CARTESIAN_POINT('Ctrl Pts',(180.903781206245,583.918938415685,-48.0951494693389)) ;
#50483 = CARTESIAN_POINT('Ctrl Pts',(180.782425708051,583.855405453882,-48.101611621751)) ;
#50484 = CARTESIAN_POINT('Ctrl Pts',(180.5665410488,583.768524288893,-48.1129684175069)) ;
#50485 = CARTESIAN_POINT('Ctrl Pts',(180.475029262308,583.738957122749,-48.1177399653916)) ;
#50486 = CARTESIAN_POINT('Ctrl Pts',(180.331724867342,583.703519135387,-48.1253929051634)) ;
#50487 = CARTESIAN_POINT('Ctrl Pts',(180.281213082619,583.693028287582,-48.1281221150801)) ;
#50488 = CARTESIAN_POINT('Ctrl Pts',(180.176939632221,583.675435836514,-48.1338470225872)) ;
#50489 = CARTESIAN_POINT('Ctrl Pts',(180.123184838433,583.668539682639,-48.1368470084502)) ;
#50490 = CARTESIAN_POINT('Ctrl Pts',(179.904729169015,583.649253826554,-48.149253612751)) ;
#50491 = CARTESIAN_POINT('Ctrl Pts',(179.739103961346,583.654616901791,-48.1592159016528)) ;
#50492 = CARTESIAN_POINT('Ctrl Pts',(179.489951376294,583.692966635994,-48.1743445615698)) ;
#50493 = CARTESIAN_POINT('Ctrl Pts',(179.404882292459,583.711651318651,-48.1795206036668)) ;
#50494 = CARTESIAN_POINT('Ctrl Pts',(179.290413414615,583.744532051245,-48.1862917883039)) ;
#50495 = CARTESIAN_POINT('Ctrl Pts',(179.259787857356,583.754110862513,-48.1880833580417)) ;
#50496 = CARTESIAN_POINT('Ctrl Pts',(179.198265249755,583.774947490261,-48.1916236081324)) ;
#50497 = CARTESIAN_POINT('Ctrl Pts',(179.167389063839,583.786237391059,-48.1933700956937)) ;
#50498 = CARTESIAN_POINT('Ctrl Pts',(179.009776680321,583.848195386809,-48.2021918055425)) ;
#50499 = CARTESIAN_POINT('Ctrl Pts',(178.888034361432,583.91066348513,-48.2087065889619)) ;
#50500 = CARTESIAN_POINT('Ctrl Pts',(178.673245011278,584.049451579728,-48.2210947512499)) ;
#50501 = CARTESIAN_POINT('Ctrl Pts',(178.5789406374,584.122740061617,-48.2269230229882)) ;
#50502 = CARTESIAN_POINT('Ctrl Pts',(178.452847466274,584.239646283619,-48.235795173972)) ;
#50503 = CARTESIAN_POINT('Ctrl Pts',(178.415564827687,584.27698231178,-48.238573663469)) ;
#50504 = CARTESIAN_POINT('Ctrl Pts',(178.343961353214,584.35443322779,-48.2442612720391)) ;
#50505 = CARTESIAN_POINT('Ctrl Pts',(178.309667660239,584.39451832682,-48.2471682239792)) ;
#50506 = CARTESIAN_POINT('Ctrl Pts',(178.175010798644,584.564763085197,-48.2593901721941)) ;
#50507 = CARTESIAN_POINT('Ctrl Pts',(178.08890997158,584.705397593426,-48.2692667916853)) ;
#50508 = CARTESIAN_POINT('Ctrl Pts',(177.993744151752,584.913122014472,-48.2829923187101)) ;
#50509 = CARTESIAN_POINT('Ctrl Pts',(177.969751377576,584.972717998752,-48.2868315469812)) ;
#50510 = CARTESIAN_POINT('Ctrl Pts',(177.93356250256,585.076382845395,-48.2932464649048)) ;
#50511 = CARTESIAN_POINT('Ctrl Pts',(177.919972544042,585.119915217059,-48.2958636277839)) ;
#50512 = CARTESIAN_POINT('Ctrl Pts',(177.900136405436,585.191781470052,-48.3000202988913)) ;
#50513 = CARTESIAN_POINT('Ctrl Pts',(177.893022713931,585.219854914262,-48.3016021401449)) ;
#50514 = CARTESIAN_POINT('Ctrl Pts',(177.876673238317,585.290628304369,-48.3054861972944)) ;
#50515 = CARTESIAN_POINT('Ctrl Pts',(177.868201324395,585.333487955035,-48.3077492958369)) ;
#50516 = CARTESIAN_POINT('Ctrl Pts',(177.839106260069,585.510111076727,-48.3168306450971)) ;
#50517 = CARTESIAN_POINT('Ctrl Pts',(177.830353564614,585.645489593599,-48.3232400091894)) ;
#50518 = CARTESIAN_POINT('Ctrl Pts',(177.838418384486,585.881447432622,-48.3347357433026)) ;
#50519 = CARTESIAN_POINT('Ctrl Pts',(177.849261112119,585.981744041669,-48.3397224335615)) ;
#50520 = CARTESIAN_POINT('Ctrl Pts',(177.876765189013,586.131875156197,-48.3476239015105)) ;
#50521 = CARTESIAN_POINT('Ctrl Pts',(177.888045446498,586.182540388175,-48.3503660802006)) ;
#50522 = CARTESIAN_POINT('Ctrl Pts',(177.914883102183,586.284682946268,-48.3560766796963)) ;
#50523 = CARTESIAN_POINT('Ctrl Pts',(177.930567397288,586.336084872031,-48.359047485209)) ;
#50524 = CARTESIAN_POINT('Ctrl Pts',(178.004139143522,586.547176825693,-48.371675885257)) ;
#50525 = CARTESIAN_POINT('Ctrl Pts',(178.079691484335,586.699975624319,-48.3819321091802)) ;
#50526 = CARTESIAN_POINT('Ctrl Pts',(178.219609065619,586.912159829085,-48.397173639217)) ;
#50527 = CARTESIAN_POINT('Ctrl Pts',(178.270364970187,586.979687263092,-48.4021860179028)) ;
#50528 = CARTESIAN_POINT('Ctrl Pts',(178.345864689751,587.068213582013,-48.4087972105741)) ;
#50529 = CARTESIAN_POINT('Ctrl Pts',(178.367161054818,587.09203621,-48.4105802503613)) ;
#50530 = CARTESIAN_POINT('Ctrl Pts',(178.411603574376,587.139475723884,-48.4141213908943)) ;
#50531 = CARTESIAN_POINT('Ctrl Pts',(178.434781280395,587.163049892017,-48.4158765831591)) ;
#50532 = CARTESIAN_POINT('Ctrl Pts',(178.51484535328,587.240645969364,-48.4216807330674)) ;
#50533 = CARTESIAN_POINT('Ctrl Pts',(178.574255931544,587.291970259067,-48.4255669620015)) ;
#50534 = CARTESIAN_POINT('Ctrl Pts',(178.636459914542,587.339774787898,-48.4293959864656)) ;
#50535 = CARTESIAN_POINT('Origin',(179.888527625416,585.710565160536,-51.0680854522974)) ;
#50536 = CARTESIAN_POINT('',(178.63687932657,587.339321169053,-49.1271827457828)) ;
#50537 = CARTESIAN_POINT('',(178.636459914524,587.339774787883,-49.0681958067691)) ;
#50538 = CARTESIAN_POINT('',(178.636459914529,587.339774787887,-51.0680854522974)) ;
#50539 = CARTESIAN_POINT('',(181.943277589855,585.710182877802,-49.3762357656828)) ;
#50540 = CARTESIAN_POINT('Ctrl Pts',(181.942731046524,585.710143815257,-49.375289272883)) ;
#50541 = CARTESIAN_POINT('Ctrl Pts',(181.942609902982,585.781072616081,-49.3712166166913)) ;
#50542 = CARTESIAN_POINT('Ctrl Pts',(181.938842933789,585.852042270409,-49.3671991813958)) ;
#50543 = CARTESIAN_POINT('Ctrl Pts',(181.931456861355,585.922655946303,-49.3632663178078)) ;
#50544 = CARTESIAN_POINT('Ctrl Pts',(181.924072660175,585.993251732304,-49.3593344506064)) ;
#50545 = CARTESIAN_POINT('Ctrl Pts',(181.913071204659,586.063491698852,-49.3554871423331)) ;
#50546 = CARTESIAN_POINT('Ctrl Pts',(181.898513657117,586.132983525398,-49.3517291276852)) ;
#50547 = CARTESIAN_POINT('Ctrl Pts',(181.88395481418,586.202481535636,-49.3479707786323)) ;
#50548 = CARTESIAN_POINT('Ctrl Pts',(181.865839152381,586.271231202506,-49.3443016663953)) ;
#50549 = CARTESIAN_POINT('Ctrl Pts',(181.844262927951,586.338844996212,-49.3407022466588)) ;
#50550 = CARTESIAN_POINT('Ctrl Pts',(181.822661713033,586.406537103051,-49.3370986579233)) ;
#50551 = CARTESIAN_POINT('Ctrl Pts',(181.797591708343,586.473090572644,-49.333564737381)) ;
#50552 = CARTESIAN_POINT('Ctrl Pts',(181.769186915986,586.538122925371,-49.3300584437495)) ;
#50553 = CARTESIAN_POINT('Ctrl Pts',(181.740764472904,586.603195689168,-49.3265499713089)) ;
#50554 = CARTESIAN_POINT('Ctrl Pts',(181.709002781512,586.666745209728,-49.3230688143823)) ;
#50555 = CARTESIAN_POINT('Ctrl Pts',(181.674077437369,586.728397382294,-49.3195543533391)) ;
#50556 = CARTESIAN_POINT('Ctrl Pts',(181.641178847481,586.786471814792,-49.3162438401467)) ;
#50557 = CARTESIAN_POINT('Ctrl Pts',(181.605472728773,586.842862902337,-49.3129032840571)) ;
#50558 = CARTESIAN_POINT('Ctrl Pts',(181.567145026093,586.897267996673,-49.3094721752712)) ;
#50559 = CARTESIAN_POINT('Ctrl Pts',(181.564706940191,586.900728790934,-49.3092539170043)) ;
#50560 = CARTESIAN_POINT('Ctrl Pts',(181.562258245026,586.904181566495,-49.309035292322)) ;
#50561 = CARTESIAN_POINT('Ctrl Pts',(181.5597989878,586.907626252577,-49.308816285649)) ;
#50562 = CARTESIAN_POINT('Ctrl Pts',(181.533601879691,586.944320589691,-49.3064833285961)) ;
#50563 = CARTESIAN_POINT('Ctrl Pts',(181.506207383144,586.980095008409,-49.3041067928128)) ;
#50564 = CARTESIAN_POINT('Ctrl Pts',(181.477684382118,587.014860414755,-49.3016672162806)) ;
#50565 = CARTESIAN_POINT('Ctrl Pts',(181.477662093227,587.014887581684,-49.3016653099084)) ;
#50566 = CARTESIAN_POINT('Ctrl Pts',(181.477639803647,587.014914747998,-49.3016634034977)) ;
#50567 = CARTESIAN_POINT('Ctrl Pts',(181.477617513378,587.014941913696,-49.3016614970486)) ;
#50568 = CARTESIAN_POINT('Ctrl Pts',(181.436792415083,587.064696463765,-49.298169795156)) ;
#50569 = CARTESIAN_POINT('Ctrl Pts',(181.393498463665,587.112564995586,-49.2945396579515)) ;
#50570 = CARTESIAN_POINT('Ctrl Pts',(181.347956768597,587.15831772393,-49.2908361813299)) ;
#50571 = CARTESIAN_POINT('Ctrl Pts',(181.343340057968,587.162955827692,-49.290460747788)) ;
#50572 = CARTESIAN_POINT('Ctrl Pts',(181.338700291656,587.16757217983,-49.2900845605706)) ;
#50573 = CARTESIAN_POINT('Ctrl Pts',(181.33403772939,587.17216653593,-49.2897076874925)) ;
#50574 = CARTESIAN_POINT('Ctrl Pts',(181.283458903455,587.222005470876,-49.2856194208424)) ;
#50575 = CARTESIAN_POINT('Ctrl Pts',(181.230191784817,587.269257599862,-49.2814510605544)) ;
#50576 = CARTESIAN_POINT('Ctrl Pts',(181.174555896109,587.313659051509,-49.2772769797148)) ;
#50577 = CARTESIAN_POINT('Ctrl Pts',(181.118988717447,587.358005667584,-49.2731080538443)) ;
#50578 = CARTESIAN_POINT('Ctrl Pts',(181.061058803437,587.399508975766,-49.2689337751207)) ;
#50579 = CARTESIAN_POINT('Ctrl Pts',(181.00110188632,587.437942358132,-49.2648088811621)) ;
#50580 = CARTESIAN_POINT('Ctrl Pts',(180.941185011684,587.476350072602,-49.2606867420313)) ;
#50581 = CARTESIAN_POINT('Ctrl Pts',(180.879243905101,587.511692123099,-49.2566140905518)) ;
#50582 = CARTESIAN_POINT('Ctrl Pts',(180.815629223576,587.543774893854,-49.2526223602738)) ;
#50583 = CARTESIAN_POINT('Ctrl Pts',(180.752035650566,587.575847018959,-49.2486319545248)) ;
#50584 = CARTESIAN_POINT('Ctrl Pts',(180.686769631124,587.604662042031,-49.2447224565592)) ;
#50585 = CARTESIAN_POINT('Ctrl Pts',(180.620196491689,587.63005777694,-49.2409005518772)) ;
#50586 = CARTESIAN_POINT('Ctrl Pts',(180.553623072081,587.655453618726,-49.2370786311107)) ;
#50587 = CARTESIAN_POINT('Ctrl Pts',(180.485742520518,587.677430034423,-49.2333442395844)) ;
#50588 = CARTESIAN_POINT('Ctrl Pts',(180.416935074601,587.695856798957,-49.2296795293261)) ;
#50589 = CARTESIAN_POINT('Ctrl Pts',(180.348058708124,587.714302020548,-49.226011148333)) ;
#50590 = CARTESIAN_POINT('Ctrl Pts',(180.278253579484,587.729190236431,-49.2224124098555)) ;
#50591 = CARTESIAN_POINT('Ctrl Pts',(180.207916107238,587.740425467912,-49.2188426223026)) ;
#50592 = CARTESIAN_POINT('Ctrl Pts',(180.137540745288,587.751666751639,-49.2152709117605)) ;
#50593 = CARTESIAN_POINT('Ctrl Pts',(180.06663248392,587.759250723212,-49.2117278455962)) ;
#50594 = CARTESIAN_POINT('Ctrl Pts',(179.995603422909,587.763120605311,-49.2081536905138)) ;
#50595 = CARTESIAN_POINT('Ctrl Pts',(179.92834605237,587.766784994091,-49.204769325448)) ;
#50596 = CARTESIAN_POINT('Ctrl Pts',(179.860980032854,587.767118982164,-49.2013565946411)) ;
#50597 = CARTESIAN_POINT('Ctrl Pts',(179.793868461632,587.764113188371,-49.1978542829438)) ;
#50598 = CARTESIAN_POINT('Ctrl Pts',(179.789983017362,587.76393916705,-49.197651515572)) ;
#50599 = CARTESIAN_POINT('Ctrl Pts',(179.78609841312,587.763753958018,-49.1974484479372)) ;
#50600 = CARTESIAN_POINT('Ctrl Pts',(179.782214714566,587.763557561845,-49.19724506816)) ;
#50601 = CARTESIAN_POINT('Ctrl Pts',(179.739246410607,587.761384681962,-49.1949949233658)) ;
#50602 = CARTESIAN_POINT('Ctrl Pts',(179.696391016001,587.757842438412,-49.1927063515351)) ;
#50603 = CARTESIAN_POINT('Ctrl Pts',(179.653745543434,587.752938395067,-49.1903625908485)) ;
#50604 = CARTESIAN_POINT('Ctrl Pts',(179.653711814989,587.752934516443,-49.1903607371604)) ;
#50605 = CARTESIAN_POINT('Ctrl Pts',(179.653678086674,587.752930636967,-49.1903588834378)) ;
#50606 = CARTESIAN_POINT('Ctrl Pts',(179.65364435849,587.75292675664,-49.1903570296806)) ;
#50607 = CARTESIAN_POINT('Ctrl Pts',(179.589350160997,587.745529900698,-49.1868233135333)) ;
#50608 = CARTESIAN_POINT('Ctrl Pts',(179.525312509616,587.735005549323,-49.1831554356994)) ;
#50609 = CARTESIAN_POINT('Ctrl Pts',(179.46184773535,587.721416836011,-49.1794183432615)) ;
#50610 = CARTESIAN_POINT('Ctrl Pts',(179.455646154714,587.72008898915,-49.1790531661949)) ;
#50611 = CARTESIAN_POINT('Ctrl Pts',(179.449450072789,587.718731911477,-49.1786873282263)) ;
#50612 = CARTESIAN_POINT('Ctrl Pts',(179.443259802766,587.717345681468,-49.1783208899553)) ;
#50613 = CARTESIAN_POINT('Ctrl Pts',(179.374193897246,587.701879275243,-49.1742324752477)) ;
#50614 = CARTESIAN_POINT('Ctrl Pts',(179.305847650325,587.682780044733,-49.1700700719711)) ;
#50615 = CARTESIAN_POINT('Ctrl Pts',(179.238608498183,587.660172786892,-49.1659052769008)) ;
#50616 = CARTESIAN_POINT('Ctrl Pts',(179.235036122816,587.658971676996,-49.165684003865)) ;
#50617 = CARTESIAN_POINT('Ctrl Pts',(179.231466882203,587.657760672292,-49.1654627240778)) ;
#50618 = CARTESIAN_POINT('Ctrl Pts',(179.227900837645,587.656539794077,-49.1652414482766)) ;
#50619 = CARTESIAN_POINT('Ctrl Pts',(179.160499471941,587.633464126422,-49.1610591418145)) ;
#50620 = CARTESIAN_POINT('Ctrl Pts',(179.094235691661,587.606858873681,-49.156878466474)) ;
#50621 = CARTESIAN_POINT('Ctrl Pts',(179.029481540879,587.576886091707,-49.1527518854787)) ;
#50622 = CARTESIAN_POINT('Ctrl Pts',(178.964770398448,587.546933217028,-49.1486280452721)) ;
#50623 = CARTESIAN_POINT('Ctrl Pts',(178.901566786388,587.513617417541,-49.1445583855618)) ;
#50624 = CARTESIAN_POINT('Ctrl Pts',(178.840223204897,587.477131031072,-49.1405719754824)) ;
#50625 = CARTESIAN_POINT('Ctrl Pts',(178.77889638879,587.44065461644,-49.1365866549009)) ;
#50626 = CARTESIAN_POINT('Ctrl Pts',(178.719428589935,587.401009363747,-49.1326845707494)) ;
#50627 = CARTESIAN_POINT('Ctrl Pts',(178.662153901579,587.358416989177,-49.1288700914329)) ;
#50628 = CARTESIAN_POINT('Ctrl Pts',(178.653680728366,587.35211590614,-49.1283057803054)) ;
#50629 = CARTESIAN_POINT('Ctrl Pts',(178.645255520909,587.345750375093,-49.1277433423199)) ;
#50630 = CARTESIAN_POINT('Ctrl Pts',(178.63687932657,587.339321169054,-49.1271827457828)) ;
#50631 = CARTESIAN_POINT('',(180.418697842604,583.725390834864,-49.5221601717598)) ;
#50632 = CARTESIAN_POINT('Ctrl Pts',(180.418697842604,583.725390834864,-49.5221601717598)) ;
#50633 = CARTESIAN_POINT('Ctrl Pts',(180.488833687662,583.744121651461,-49.5182241312826)) ;
#50634 = CARTESIAN_POINT('Ctrl Pts',(180.558043092019,583.766591466879,-49.5142880908053)) ;
#50635 = CARTESIAN_POINT('Ctrl Pts',(180.625912157186,583.792685702696,-49.5103520503281)) ;
#50636 = CARTESIAN_POINT('Ctrl Pts',(180.693726478774,583.818758890751,-49.5064191846838)) ;
#50637 = CARTESIAN_POINT('Ctrl Pts',(180.760202181966,583.848450521621,-49.5024863190395)) ;
#50638 = CARTESIAN_POINT('Ctrl Pts',(180.824941915912,583.881596642749,-49.4985534533952)) ;
#50639 = CARTESIAN_POINT('Ctrl Pts',(180.889661927391,583.914732666164,-49.4946217858685)) ;
#50640 = CARTESIAN_POINT('Ctrl Pts',(180.952646607951,583.951320884749,-49.4906901183417)) ;
#50641 = CARTESIAN_POINT('Ctrl Pts',(181.01352096904,583.991150277705,-49.486758450815)) ;
#50642 = CARTESIAN_POINT('Ctrl Pts',(181.074388214353,584.030975014891,-49.482827242872)) ;
#50643 = CARTESIAN_POINT('Ctrl Pts',(181.133145244721,584.074039921525,-49.478896034929)) ;
#50644 = CARTESIAN_POINT('Ctrl Pts',(181.189445268872,584.120090122239,-49.474964826986)) ;
#50645 = CARTESIAN_POINT('Ctrl Pts',(181.245754646727,584.166147973749,-49.4710329659108)) ;
#50646 = CARTESIAN_POINT('Ctrl Pts',(181.299605850614,584.215191813014,-49.4671011048356)) ;
#50647 = CARTESIAN_POINT('Ctrl Pts',(181.350685554016,584.266926786727,-49.4631692437604)) ;
#50648 = CARTESIAN_POINT('Ctrl Pts',(181.401788202959,584.318685000336,-49.4592356164518)) ;
#50649 = CARTESIAN_POINT('Ctrl Pts',(181.450116553871,584.373136422868,-49.4553019891431)) ;
#50650 = CARTESIAN_POINT('Ctrl Pts',(181.495395471567,584.429950742568,-49.4513683618344)) ;
#50651 = CARTESIAN_POINT('Ctrl Pts',(181.540741306735,584.48684902785,-49.4474289210388)) ;
#50652 = CARTESIAN_POINT('Ctrl Pts',(181.583028425668,584.546116819582,-49.4434894802433)) ;
#50653 = CARTESIAN_POINT('Ctrl Pts',(181.622023487452,584.60739261791,-49.4395500394477)) ;
#50654 = CARTESIAN_POINT('Ctrl Pts',(181.661050939679,584.668719313714,-49.4356073264369)) ;
#50655 = CARTESIAN_POINT('Ctrl Pts',(181.69678066254,584.732056936852,-49.4316646134261)) ;
#50656 = CARTESIAN_POINT('Ctrl Pts',(181.729025270704,584.797019332353,-49.4277219004154)) ;
#50657 = CARTESIAN_POINT('Ctrl Pts',(181.761331269842,584.862105410695,-49.4237716808165)) ;
#50658 = CARTESIAN_POINT('Ctrl Pts',(181.790138722435,584.928822015519,-49.4198214612176)) ;
#50659 = CARTESIAN_POINT('Ctrl Pts',(181.815308509274,584.996763375656,-49.4158712416187)) ;
#50660 = CARTESIAN_POINT('Ctrl Pts',(181.825786450384,585.025046712936,-49.4142268030466)) ;
#50661 = CARTESIAN_POINT('Ctrl Pts',(181.835634593048,585.053542127974,-49.4125823644746)) ;
#50662 = CARTESIAN_POINT('Ctrl Pts',(181.844845492613,585.082219742008,-49.4109379259025)) ;
#50663 = CARTESIAN_POINT('Ctrl Pts',(181.870333237588,585.161574392204,-49.4063875526567)) ;
#50664 = CARTESIAN_POINT('Ctrl Pts',(181.891016257104,585.242567282731,-49.4018371794109)) ;
#50665 = CARTESIAN_POINT('Ctrl Pts',(181.906713128642,585.324657351507,-49.3972868061651)) ;
#50666 = CARTESIAN_POINT('Ctrl Pts',(181.922242415703,585.40587100225,-49.3927850140597)) ;
#50667 = CARTESIAN_POINT('Ctrl Pts',(181.932891369071,585.488158412433,-49.3882832219544)) ;
#50668 = CARTESIAN_POINT('Ctrl Pts',(181.938530559059,585.570974564301,-49.3837814298491)) ;
#50669 = CARTESIAN_POINT('Ctrl Pts',(181.941681262365,585.617245238656,-49.3812662084604)) ;
#50670 = CARTESIAN_POINT('Ctrl Pts',(181.943268938184,585.663680597079,-49.3787509870716)) ;
#50671 = CARTESIAN_POINT('Ctrl Pts',(181.943277589855,585.710182877802,-49.3762357656828)) ;
#50672 = CARTESIAN_POINT('',(179.355546343215,583.723963875141,-49.5209457596381)) ;
#50673 = CARTESIAN_POINT('Origin',(179.888527625416,585.710565160536,-49.5221601717598)) ;
#50674 = CARTESIAN_POINT('Ctrl Pts',(179.356176202651,583.725974642273,-49.5197218953676)) ;
#50675 = CARTESIAN_POINT('Ctrl Pts',(179.386889376523,583.717736065268,-49.5180018393397)) ;
#50676 = CARTESIAN_POINT('Ctrl Pts',(179.417791541479,583.710211061965,-49.5163222483587)) ;
#50677 = CARTESIAN_POINT('Ctrl Pts',(179.62291895486,583.665277731807,-49.5054338937319)) ;
#50678 = CARTESIAN_POINT('Ctrl Pts',(179.8012184922,583.649948421268,-49.4971434324973)) ;
#50679 = CARTESIAN_POINT('Ctrl Pts',(180.046299752696,583.660783124538,-49.485062778235)) ;
#50680 = CARTESIAN_POINT('Ctrl Pts',(180.113133550294,583.667026643641,-49.4817057318923)) ;
#50681 = CARTESIAN_POINT('Ctrl Pts',(180.232949061191,583.684168734103,-49.4754789283973)) ;
#50682 = CARTESIAN_POINT('Ctrl Pts',(180.286033818234,583.693910325479,-49.4726452771753)) ;
#50683 = CARTESIAN_POINT('Ctrl Pts',(180.38961266037,583.717166744821,-49.466936066763)) ;
#50684 = CARTESIAN_POINT('Ctrl Pts',(180.44009631471,583.730541237049,-49.4640669709128)) ;
#50685 = CARTESIAN_POINT('Ctrl Pts',(180.658536214026,583.797414324731,-49.4512467161314)) ;
#50686 = CARTESIAN_POINT('Ctrl Pts',(180.819699315335,583.87046782969,-49.4406323481091)) ;
#50687 = CARTESIAN_POINT('Ctrl Pts',(181.039578895036,584.00649269093,-49.4251737513292)) ;
#50688 = CARTESIAN_POINT('Ctrl Pts',(181.106963343656,584.054002869783,-49.4202967402071)) ;
#50689 = CARTESIAN_POINT('Ctrl Pts',(181.196194163741,584.125314438653,-49.4138177849933)) ;
#50690 = CARTESIAN_POINT('Ctrl Pts',(181.220606829301,584.145772222574,-49.4120432686528)) ;
#50691 = CARTESIAN_POINT('Ctrl Pts',(181.269515556757,584.188732282953,-49.4085018593836)) ;
#50692 = CARTESIAN_POINT('Ctrl Pts',(181.293960615279,584.211278207407,-49.4067387469068)) ;
#50693 = CARTESIAN_POINT('Ctrl Pts',(181.413096631273,584.326634341954,-49.398117883182)) ;
#50694 = CARTESIAN_POINT('Ctrl Pts',(181.499205055676,584.427872260819,-49.3917808198691)) ;
#50695 = CARTESIAN_POINT('Ctrl Pts',(181.622908773339,584.605593193042,-49.3813051619974)) ;
#50696 = CARTESIAN_POINT('Ctrl Pts',(181.666587291408,584.677345034425,-49.3772266321849)) ;
#50697 = CARTESIAN_POINT('Ctrl Pts',(181.736732034291,584.810263369691,-49.3696979435945)) ;
#50698 = CARTESIAN_POINT('Ctrl Pts',(181.764844856385,584.870425085859,-49.3663001305553)) ;
#50699 = CARTESIAN_POINT('Ctrl Pts',(181.808774185936,584.977690174157,-49.3601887408044)) ;
#50700 = CARTESIAN_POINT('Ctrl Pts',(181.825886519072,585.024203356173,-49.3575224584785)) ;
#50701 = CARTESIAN_POINT('Ctrl Pts',(181.861229729117,585.13216457032,-49.3512781347795)) ;
#50702 = CARTESIAN_POINT('Ctrl Pts',(181.878299808622,585.193935477701,-49.3476646133698)) ;
#50703 = CARTESIAN_POINT('Ctrl Pts',(181.924877811513,585.399452434824,-49.3355110738389)) ;
#50704 = CARTESIAN_POINT('Ctrl Pts',(181.941885161974,585.545557198841,-49.3266292723503)) ;
#50705 = CARTESIAN_POINT('Ctrl Pts',(181.94387725099,585.768487613464,-49.3133195289235)) ;
#50706 = CARTESIAN_POINT('Ctrl Pts',(181.940310231736,585.844755901183,-49.308818262318)) ;
#50707 = CARTESIAN_POINT('Ctrl Pts',(181.929291183026,585.951961391816,-49.3027124523943)) ;
#50708 = CARTESIAN_POINT('Ctrl Pts',(181.925354210697,585.983192785691,-49.3009608130156)) ;
#50709 = CARTESIAN_POINT('Ctrl Pts',(181.915760062096,586.047378507676,-49.2974340859969)) ;
#50710 = CARTESIAN_POINT('Ctrl Pts',(181.91001315652,586.080309818826,-49.2956641350769)) ;
#50711 = CARTESIAN_POINT('Ctrl Pts',(181.881733465697,586.221871392507,-49.2881706885986)) ;
#50712 = CARTESIAN_POINT('Ctrl Pts',(181.851225742185,586.328727459923,-49.2828025136458)) ;
#50713 = CARTESIAN_POINT('Ctrl Pts',(181.765035255342,586.558361766762,-49.2709509441333)) ;
#50714 = CARTESIAN_POINT('Ctrl Pts',(181.705618529938,586.679181361807,-49.2644842935094)) ;
#50715 = CARTESIAN_POINT('Ctrl Pts',(181.606007583798,586.839836828763,-49.2548131821556)) ;
#50716 = CARTESIAN_POINT('Ctrl Pts',(181.575327955583,586.885169698002,-49.2519542820075)) ;
#50717 = CARTESIAN_POINT('Ctrl Pts',(181.513046335847,586.969718204178,-49.2463318399926)) ;
#50718 = CARTESIAN_POINT('Ctrl Pts',(181.48174035064,587.009102801363,-49.2435812871606)) ;
#50719 = CARTESIAN_POINT('Ctrl Pts',(181.39353869084,587.112069056182,-49.2360100209409)) ;
#50720 = CARTESIAN_POINT('Ctrl Pts',(181.334081765618,587.173316644171,-49.231084553678)) ;
#50721 = CARTESIAN_POINT('Ctrl Pts',(181.163438823021,587.328507198668,-49.2174600850716)) ;
#50722 = CARTESIAN_POINT('Ctrl Pts',(181.045809206581,587.414628392046,-49.2085624441057)) ;
#50723 = CARTESIAN_POINT('Ctrl Pts',(180.876825266669,587.512721294467,-49.1970823189271)) ;
#50724 = CARTESIAN_POINT('Ctrl Pts',(180.832664925807,587.536244346927,-49.1941935835968)) ;
#50725 = CARTESIAN_POINT('Ctrl Pts',(180.761658948036,587.570800943084,-49.1897713126811)) ;
#50726 = CARTESIAN_POINT('Ctrl Pts',(180.735365521296,587.582916992102,-49.1881814058169)) ;
#50727 = CARTESIAN_POINT('Ctrl Pts',(180.672443125917,587.610314680613,-49.1844939719287)) ;
#50728 = CARTESIAN_POINT('Ctrl Pts',(180.635612223257,587.625098206874,-49.1824234557031)) ;
#50729 = CARTESIAN_POINT('Ctrl Pts',(180.494983306995,587.676868124178,-49.1747640503639)) ;
#50730 = CARTESIAN_POINT('Ctrl Pts',(180.388690515493,587.706555339862,-49.1694648879953)) ;
#50731 = CARTESIAN_POINT('Ctrl Pts',(180.154806656935,587.75200939133,-49.1579392175482)) ;
#50732 = CARTESIAN_POINT('Ctrl Pts',(180.027088591908,587.764633356966,-49.1517160110635)) ;
#50733 = CARTESIAN_POINT('Ctrl Pts',(179.846249286691,587.765558270212,-49.1423985175278)) ;
#50734 = CARTESIAN_POINT('Ctrl Pts',(179.793474814603,587.763793941935,-49.1396220272722)) ;
#50735 = CARTESIAN_POINT('Ctrl Pts',(179.689026453531,587.756266594903,-49.1339834551273)) ;
#50736 = CARTESIAN_POINT('Ctrl Pts',(179.637387179636,587.750570762241,-49.1311255514424)) ;
#50737 = CARTESIAN_POINT('Ctrl Pts',(179.480864991807,587.72727330979,-49.1222322948421)) ;
#50738 = CARTESIAN_POINT('Ctrl Pts',(179.377094388892,587.703485526091,-49.1160073953665)) ;
#50739 = CARTESIAN_POINT('Ctrl Pts',(179.133131826722,587.627246389328,-49.1007412704924)) ;
#50740 = CARTESIAN_POINT('Ctrl Pts',(178.995899259555,587.567311496861,-49.0916085268589)) ;
#50741 = CARTESIAN_POINT('Ctrl Pts',(178.837263816686,587.476341986995,-49.0811645232351)) ;
#50742 = CARTESIAN_POINT('Ctrl Pts',(178.80856788964,587.458938879881,-49.0792820225989)) ;
#50743 = CARTESIAN_POINT('Ctrl Pts',(178.758045081827,587.42657967757,-49.0759979476098)) ;
#50744 = CARTESIAN_POINT('Ctrl Pts',(178.736057726286,587.411891056373,-49.0745802295068)) ;
#50745 = CARTESIAN_POINT('Ctrl Pts',(178.687948631364,587.378391106045,-49.0714902426275)) ;
#50746 = CARTESIAN_POINT('Ctrl Pts',(178.661980295812,587.359387515948,-49.0698303506149)) ;
#50747 = CARTESIAN_POINT('Ctrl Pts',(178.636459914524,587.339774787883,-49.0681958067691)) ;
#50748 = CARTESIAN_POINT('Origin',(29.8885276254155,585.710565160562,-51.0680854522906)) ;
#50749 = CARTESIAN_POINT('',(27.873599051246,585.307997894761,-47.6045419700025)) ;
#50750 = CARTESIAN_POINT('',(27.8735991218939,585.307997541154,-47.5475669749031)) ;
#50751 = CARTESIAN_POINT('',(27.8735990520584,585.307997890694,-51.0680854522905)) ;
#50752 = CARTESIAN_POINT('',(28.0059001157518,584.887332980459,-47.5221601717529)) ;
#50753 = CARTESIAN_POINT('Ctrl Pts',(27.8735991218939,585.307997541154,-47.5475669749032)) ;
#50754 = CARTESIAN_POINT('Ctrl Pts',(27.895951833801,585.196117911047,-47.5408462881297)) ;
#50755 = CARTESIAN_POINT('Ctrl Pts',(27.9276066114201,585.086179402263,-47.5340931280632)) ;
#50756 = CARTESIAN_POINT('Ctrl Pts',(27.9800846809023,584.948370365598,-47.525792691713)) ;
#50757 = CARTESIAN_POINT('Ctrl Pts',(27.9926238383014,584.917694141937,-47.5239568576251)) ;
#50758 = CARTESIAN_POINT('Ctrl Pts',(28.0059001157519,584.887332980459,-47.522160171753)) ;
#50759 = CARTESIAN_POINT('',(28.665910763353,584.056452215556,-47.5234195439953)) ;
#50760 = CARTESIAN_POINT('Origin',(29.8885276254157,585.710565160562,-47.522160171753)) ;
#50761 = CARTESIAN_POINT('Ctrl Pts',(28.6669780822516,584.058350199942,-47.5246789162374)) ;
#50762 = CARTESIAN_POINT('Ctrl Pts',(28.6536409221051,584.068210903466,-47.5255745090143)) ;
#50763 = CARTESIAN_POINT('Ctrl Pts',(28.6404231746705,584.078233088099,-47.5264591946414)) ;
#50764 = CARTESIAN_POINT('Ctrl Pts',(28.6099181024573,584.101950363772,-47.5284978961042)) ;
#50765 = CARTESIAN_POINT('Ctrl Pts',(28.5927268286653,584.115766037774,-47.5296444808809)) ;
#50766 = CARTESIAN_POINT('Ctrl Pts',(28.4803476990676,584.209096065911,-47.5371487358809)) ;
#50767 = CARTESIAN_POINT('Ctrl Pts',(28.3922965013326,584.29681904309,-47.5430847582806)) ;
#50768 = CARTESIAN_POINT('Ctrl Pts',(28.23723308194,584.482131450054,-47.5548023003805)) ;
#50769 = CARTESIAN_POINT('Ctrl Pts',(28.1696609137121,584.578612473591,-47.5605572957726)) ;
#50770 = CARTESIAN_POINT('Ctrl Pts',(28.0841276347631,584.726212641845,-47.569358114201)) ;
#50771 = CARTESIAN_POINT('Ctrl Pts',(28.0593291575392,584.773099697532,-47.5721505613178)) ;
#50772 = CARTESIAN_POINT('Ctrl Pts',(28.0134598379404,584.868592012861,-47.577861074877)) ;
#50773 = CARTESIAN_POINT('Ctrl Pts',(27.9923997258961,584.917157164115,-47.5807767116811)) ;
#50774 = CARTESIAN_POINT('Ctrl Pts',(27.9332548385845,585.069396801963,-47.5899668624736)) ;
#50775 = CARTESIAN_POINT('Ctrl Pts',(27.9016364340812,585.175358181933,-47.5964448569719)) ;
#50776 = CARTESIAN_POINT('Ctrl Pts',(27.8769385539296,585.291545532497,-47.6035380539106)) ;
#50777 = CARTESIAN_POINT('Ctrl Pts',(27.8752435130242,585.299767039094,-47.6040398358064)) ;
#50778 = CARTESIAN_POINT('Ctrl Pts',(27.8735990504334,585.307997898828,-47.6045419700025)) ;
#50779 = CARTESIAN_POINT('Origin',(29.8885276254155,585.710565160562,-51.0680854522906)) ;
#50780 = CARTESIAN_POINT('',(27.873599051992,585.307997891027,-48.3063633758768)) ;
#50781 = CARTESIAN_POINT('',(27.8735990526509,585.307997887729,-48.2478302996211)) ;
#50782 = CARTESIAN_POINT('',(27.8735990520584,585.307997890694,-51.0680854522905)) ;
#50783 = CARTESIAN_POINT('',(31.94327712373,585.709998440692,-47.9195214922471)) ;
#50784 = CARTESIAN_POINT('Ctrl Pts',(27.8735990532433,585.307997884764,-48.2478302996211)) ;
#50785 = CARTESIAN_POINT('Ctrl Pts',(27.8791763621533,585.280082354232,-48.2463036433711)) ;
#50786 = CARTESIAN_POINT('Ctrl Pts',(27.8853334487669,585.252284467362,-48.244758529309)) ;
#50787 = CARTESIAN_POINT('Ctrl Pts',(27.9070920087431,585.16289103314,-48.2397045223047)) ;
#50788 = CARTESIAN_POINT('Ctrl Pts',(27.9249711401828,585.101895516817,-48.2361228016622)) ;
#50789 = CARTESIAN_POINT('Ctrl Pts',(27.9708782613911,584.968521068649,-48.2279904734401)) ;
#50790 = CARTESIAN_POINT('Ctrl Pts',(28.0002381666779,584.896704121209,-48.223405743598)) ;
#50791 = CARTESIAN_POINT('Ctrl Pts',(28.0943565480803,584.699175320679,-48.2103129966963)) ;
#50792 = CARTESIAN_POINT('Ctrl Pts',(28.16812458387,584.578233238202,-48.2016933275169)) ;
#50793 = CARTESIAN_POINT('Ctrl Pts',(28.2746238613887,584.438361233323,-48.1916354411103)) ;
#50794 = CARTESIAN_POINT('Ctrl Pts',(28.2962166765566,584.411436855179,-48.1896964566119)) ;
#50795 = CARTESIAN_POINT('Ctrl Pts',(28.3386926405478,584.361124179889,-48.1860883893746)) ;
#50796 = CARTESIAN_POINT('Ctrl Pts',(28.3594518786549,584.337646045659,-48.1844129498431)) ;
#50797 = CARTESIAN_POINT('Ctrl Pts',(28.4307882733337,584.260592521698,-48.1789081355011)) ;
#50798 = CARTESIAN_POINT('Ctrl Pts',(28.4837116193195,584.209259542846,-48.1752287016001)) ;
#50799 = CARTESIAN_POINT('Ctrl Pts',(28.6502667192815,584.064247376582,-48.1643964993453)) ;
#50800 = CARTESIAN_POINT('Ctrl Pts',(28.7713071806064,583.979822089249,-48.1574409409065)) ;
#50801 = CARTESIAN_POINT('Ctrl Pts',(28.9586369416767,583.877064778857,-48.14673438553)) ;
#50802 = CARTESIAN_POINT('Ctrl Pts',(29.0184584731459,583.84793292598,-48.1433289198448)) ;
#50803 = CARTESIAN_POINT('Ctrl Pts',(29.1253764569807,583.802141862425,-48.1371938378907)) ;
#50804 = CARTESIAN_POINT('Ctrl Pts',(29.1718642480738,583.784202735805,-48.1345115149232)) ;
#50805 = CARTESIAN_POINT('Ctrl Pts',(29.2801842777808,583.74686703889,-48.128208125788)) ;
#50806 = CARTESIAN_POINT('Ctrl Pts',(29.3423712526496,583.728671157219,-48.1245498503397)) ;
#50807 = CARTESIAN_POINT('Ctrl Pts',(29.4832857838523,583.694575836378,-48.1161735945466)) ;
#50808 = CARTESIAN_POINT('Ctrl Pts',(29.5622947888377,583.680293189844,-48.1114170702281)) ;
#50809 = CARTESIAN_POINT('Ctrl Pts',(29.7821550571299,583.653714991094,-48.098143462204)) ;
#50810 = CARTESIAN_POINT('Ctrl Pts',(29.9237589071104,583.651266642562,-48.0895336769122)) ;
#50811 = CARTESIAN_POINT('Ctrl Pts',(30.0969004817843,583.666149365845,-48.0796441104913)) ;
#50812 = CARTESIAN_POINT('Ctrl Pts',(30.1292337505538,583.669703568193,-48.0778263956943)) ;
#50813 = CARTESIAN_POINT('Ctrl Pts',(30.1939115380498,583.678371884333,-48.0742674485293)) ;
#50814 = CARTESIAN_POINT('Ctrl Pts',(30.226245537593,583.683494433374,-48.0725272163753)) ;
#50815 = CARTESIAN_POINT('Ctrl Pts',(30.3592048794961,583.707828772456,-48.0654823232685)) ;
#50816 = CARTESIAN_POINT('Ctrl Pts',(30.4584549829245,583.73378062531,-48.0604835032138)) ;
#50817 = CARTESIAN_POINT('Ctrl Pts',(30.6960009096934,583.815283694953,-48.0483141553702)) ;
#50818 = CARTESIAN_POINT('Ctrl Pts',(30.8309737141318,583.878654430109,-48.0411895723705)) ;
#50819 = CARTESIAN_POINT('Ctrl Pts',(31.0040371455349,583.984137549062,-48.0307774336922)) ;
#50820 = CARTESIAN_POINT('Ctrl Pts',(31.0490198906013,584.01404791213,-48.0279445342932)) ;
#50821 = CARTESIAN_POINT('Ctrl Pts',(31.1346951689422,584.076018931988,-48.0222621277005)) ;
#50822 = CARTESIAN_POINT('Ctrl Pts',(31.1754568321568,584.107915029271,-48.0194203834038)) ;
#50823 = CARTESIAN_POINT('Ctrl Pts',(31.2896151106487,584.204409594192,-48.0110342415765)) ;
#50824 = CARTESIAN_POINT('Ctrl Pts',(31.3596551015355,584.272743679219,-48.0053376464281)) ;
#50825 = CARTESIAN_POINT('Ctrl Pts',(31.5154689791388,584.448110285689,-47.9913658277476)) ;
#50826 = CARTESIAN_POINT('Ctrl Pts',(31.5959248378698,584.559250743006,-47.982993681087)) ;
#50827 = CARTESIAN_POINT('Ctrl Pts',(31.6877042577938,584.717061875886,-47.9723182844464)) ;
#50828 = CARTESIAN_POINT('Ctrl Pts',(31.709353350906,584.757318266474,-47.9696931626625)) ;
#50829 = CARTESIAN_POINT('Ctrl Pts',(31.7426187720382,584.824451387697,-47.9655136988059)) ;
#50830 = CARTESIAN_POINT('Ctrl Pts',(31.7550332301088,584.850909049513,-47.9639172304712)) ;
#50831 = CARTESIAN_POINT('Ctrl Pts',(31.7850205938924,584.918533387881,-47.959960490056)) ;
#50832 = CARTESIAN_POINT('Ctrl Pts',(31.8018202341635,584.960024105956,-47.9576418861994)) ;
#50833 = CARTESIAN_POINT('Ctrl Pts',(31.8386354329746,585.060240318765,-47.9522248476218)) ;
#50834 = CARTESIAN_POINT('Ctrl Pts',(31.8573734922608,585.119388711621,-47.9491728441143)) ;
#50835 = CARTESIAN_POINT('Ctrl Pts',(31.9078613298227,585.308017126589,-47.9396497905559)) ;
#50836 = CARTESIAN_POINT('Ctrl Pts',(31.9297102836829,585.439777701415,-47.9332804013813)) ;
#50837 = CARTESIAN_POINT('Ctrl Pts',(31.9417213650514,585.618420883782,-47.9242558801685)) ;
#50838 = CARTESIAN_POINT('Ctrl Pts',(31.94326489026,585.664203639874,-47.9219118724121)) ;
#50839 = CARTESIAN_POINT('Ctrl Pts',(31.9432775469358,585.709997258212,-47.9195222884686)) ;
#50840 = CARTESIAN_POINT('Ctrl Pts',(31.9432775472728,585.709998478805,-47.9195222247762)) ;
#50841 = CARTESIAN_POINT('Ctrl Pts',(31.9432895684224,585.753586358521,-47.9172477390332)) ;
#50842 = CARTESIAN_POINT('Ctrl Pts',(31.9419146380902,585.797161735405,-47.9149331527379)) ;
#50843 = CARTESIAN_POINT('Ctrl Pts',(31.9358506616059,585.892746243631,-47.909749736901)) ;
#50844 = CARTESIAN_POINT('Ctrl Pts',(31.930563087351,585.944684850245,-47.9068634703778)) ;
#50845 = CARTESIAN_POINT('Ctrl Pts',(31.9003772973783,586.159596891199,-47.8946101911145)) ;
#50846 = CARTESIAN_POINT('Ctrl Pts',(31.8578935033976,586.319457659665,-47.8846822993874)) ;
#50847 = CARTESIAN_POINT('Ctrl Pts',(31.7628877887553,586.557400188683,-47.8692846858374)) ;
#50848 = CARTESIAN_POINT('Ctrl Pts',(31.7233554077588,586.639954947482,-47.863830861321)) ;
#50849 = CARTESIAN_POINT('Ctrl Pts',(31.6625049858158,586.747896583627,-47.8567799774564)) ;
#50850 = CARTESIAN_POINT('Ctrl Pts',(31.6458876683006,586.775806074372,-47.8549651672118)) ;
#50851 = CARTESIAN_POINT('Ctrl Pts',(31.6107687354862,586.831729338061,-47.8513642082803)) ;
#50852 = CARTESIAN_POINT('Ctrl Pts',(31.5922286585981,586.859706854857,-47.8495807371591)) ;
#50853 = CARTESIAN_POINT('Ctrl Pts',(31.4990396814934,586.993114972238,-47.8411013358479)) ;
#50854 = CARTESIAN_POINT('Ctrl Pts',(31.4152399003025,587.091810923917,-47.8348922752838)) ;
#50855 = CARTESIAN_POINT('Ctrl Pts',(31.2365275719078,587.266000864805,-47.8227667067565)) ;
#50856 = CARTESIAN_POINT('Ctrl Pts',(31.1431270040543,587.342270131788,-47.8168790170872)) ;
#50857 = CARTESIAN_POINT('Ctrl Pts',(30.9991790775615,587.440112871951,-47.8078961187918)) ;
#50858 = CARTESIAN_POINT('Ctrl Pts',(30.9535984076406,587.468548511161,-47.805066468503)) ;
#50859 = CARTESIAN_POINT('Ctrl Pts',(30.8604330062125,587.521715931628,-47.7992796666911)) ;
#50860 = CARTESIAN_POINT('Ctrl Pts',(30.8128901665524,587.546435612866,-47.7963251109806)) ;
#50861 = CARTESIAN_POINT('Ctrl Pts',(30.6623647751032,587.617370489837,-47.786948339349)) ;
#50862 = CARTESIAN_POINT('Ctrl Pts',(30.5565148256575,587.656976667338,-47.7803105145352)) ;
#50863 = CARTESIAN_POINT('Ctrl Pts',(30.3558578954533,587.713753215226,-47.7678217929438)) ;
#50864 = CARTESIAN_POINT('Ctrl Pts',(30.2620448222929,587.733346711718,-47.7620232198825)) ;
#50865 = CARTESIAN_POINT('Ctrl Pts',(30.110847350709,587.754044411417,-47.7529976444087)) ;
#50866 = CARTESIAN_POINT('Ctrl Pts',(30.0541867181453,587.759416452001,-47.7496872861673)) ;
#50867 = CARTESIAN_POINT('Ctrl Pts',(29.9679728019198,587.763989806308,-47.7448290838786)) ;
#50868 = CARTESIAN_POINT('Ctrl Pts',(29.9385405751248,587.764917459924,-47.7432022773115)) ;
#50869 = CARTESIAN_POINT('Ctrl Pts',(29.8746247144214,587.765557282675,-47.7397526626701)) ;
#50870 = CARTESIAN_POINT('Ctrl Pts',(29.8401484109236,587.765034845209,-47.7379427791917)) ;
#50871 = CARTESIAN_POINT('Ctrl Pts',(29.6929166270205,587.759095008949,-47.7303693937815)) ;
#50872 = CARTESIAN_POINT('Ctrl Pts',(29.5806884191535,587.745258862525,-47.7249803758292)) ;
#50873 = CARTESIAN_POINT('Ctrl Pts',(29.3345856097655,587.694077198643,-47.7129907238908)) ;
#50874 = CARTESIAN_POINT('Ctrl Pts',(29.2022252623547,587.652254408195,-47.7064054927449)) ;
#50875 = CARTESIAN_POINT('Ctrl Pts',(29.0240310954337,587.575433414706,-47.6965489186305)) ;
#50876 = CARTESIAN_POINT('Ctrl Pts',(28.9739003634705,587.551364997342,-47.6936617107901)) ;
#50877 = CARTESIAN_POINT('Ctrl Pts',(28.8807610553989,587.501903095422,-47.6880428240056)) ;
#50878 = CARTESIAN_POINT('Ctrl Pts',(28.8375816763748,587.47691649689,-47.6853276874536)) ;
#50879 = CARTESIAN_POINT('Ctrl Pts',(28.725968023883,587.406786937141,-47.6779993969809)) ;
#50880 = CARTESIAN_POINT('Ctrl Pts',(28.6592572347831,587.359081152255,-47.6732925638568)) ;
#50881 = CARTESIAN_POINT('Ctrl Pts',(28.4895986556163,587.221720134921,-47.6604797202275)) ;
#50882 = CARTESIAN_POINT('Ctrl Pts',(28.3924300419724,587.125584971483,-47.6522051418259)) ;
#50883 = CARTESIAN_POINT('Ctrl Pts',(28.2722415573568,586.980344142012,-47.6411528064696)) ;
#50884 = CARTESIAN_POINT('Ctrl Pts',(28.2405213517831,586.938895515114,-47.63814304934)) ;
#50885 = CARTESIAN_POINT('Ctrl Pts',(28.1931909144416,586.871909861343,-47.6335563983695)) ;
#50886 = CARTESIAN_POINT('Ctrl Pts',(28.1765029272481,586.847165294975,-47.6319196288005)) ;
#50887 = CARTESIAN_POINT('Ctrl Pts',(28.1379146701452,586.787167736202,-47.6280933869951)) ;
#50888 = CARTESIAN_POINT('Ctrl Pts',(28.116532481735,586.751599510589,-47.6259339184782)) ;
#50889 = CARTESIAN_POINT('Ctrl Pts',(28.0428274433261,586.620135298275,-47.6182551168412)) ;
#50890 = CARTESIAN_POINT('Ctrl Pts',(27.9970912172832,586.520749762445,-47.6130114496642)) ;
#50891 = CARTESIAN_POINT('Ctrl Pts',(27.9138997018933,586.293962202881,-47.6013822923232)) ;
#50892 = CARTESIAN_POINT('Ctrl Pts',(27.8804391956897,586.165630924532,-47.5950040210229)) ;
#50893 = CARTESIAN_POINT('Ctrl Pts',(27.8501584134073,585.976245863917,-47.5852178133009)) ;
#50894 = CARTESIAN_POINT('Ctrl Pts',(27.843322911764,585.917137363842,-47.5821164177999)) ;
#50895 = CARTESIAN_POINT('Ctrl Pts',(27.8350567191064,585.802089177468,-47.5759510157502)) ;
#50896 = CARTESIAN_POINT('Ctrl Pts',(27.8333276045775,585.746223199151,-47.5728988394472)) ;
#50897 = CARTESIAN_POINT('Ctrl Pts',(27.8344573756436,585.631340513076,-47.5664927294243)) ;
#50898 = CARTESIAN_POINT('Ctrl Pts',(27.8375803875382,585.572377758809,-47.5631343847387)) ;
#50899 = CARTESIAN_POINT('Ctrl Pts',(27.849888613493,585.444546476883,-47.5557168352009)) ;
#50900 = CARTESIAN_POINT('Ctrl Pts',(27.8600298425148,585.375914399032,-47.5516467875374)) ;
#50901 = CARTESIAN_POINT('Ctrl Pts',(27.8735991218939,585.307997541154,-47.5475669749032)) ;
#50902 = CARTESIAN_POINT('',(28.6364422247127,587.339761192919,-47.7296814414421)) ;
#50903 = CARTESIAN_POINT('Ctrl Pts',(27.8735990504334,585.307997898828,-47.6045419700025)) ;
#50904 = CARTESIAN_POINT('Ctrl Pts',(27.8564936227868,585.393613939248,-47.6097650867871)) ;
#50905 = CARTESIAN_POINT('Ctrl Pts',(27.8448606829014,585.480241673589,-47.6150312344685)) ;
#50906 = CARTESIAN_POINT('Ctrl Pts',(27.8358843342787,585.608720025698,-47.622630874679)) ;
#50907 = CARTESIAN_POINT('Ctrl Pts',(27.8342469626353,585.650164533989,-47.6250494566789)) ;
#50908 = CARTESIAN_POINT('Ctrl Pts',(27.8335474492433,585.726077930594,-47.6293875477471)) ;
#50909 = CARTESIAN_POINT('Ctrl Pts',(27.8340962817061,585.760528524501,-47.6313215203702)) ;
#50910 = CARTESIAN_POINT('Ctrl Pts',(27.8367863735249,585.825975415845,-47.6349087658605)) ;
#50911 = CARTESIAN_POINT('Ctrl Pts',(27.8387646497125,585.856967034994,-47.636568643584)) ;
#50912 = CARTESIAN_POINT('Ctrl Pts',(27.8476753019987,585.95982645283,-47.6419806542633)) ;
#50913 = CARTESIAN_POINT('Ctrl Pts',(27.8576927934502,586.031378326314,-47.6455893746302)) ;
#50914 = CARTESIAN_POINT('Ctrl Pts',(27.9032444872837,586.26595130639,-47.6573146546028)) ;
#50915 = CARTESIAN_POINT('Ctrl Pts',(27.9548368867758,586.425158873018,-47.6651545488101)) ;
#50916 = CARTESIAN_POINT('Ctrl Pts',(28.0502896792992,586.630593307613,-47.6766305303463)) ;
#50917 = CARTESIAN_POINT('Ctrl Pts',(28.0778286365599,586.683672968718,-47.6797241666656)) ;
#50918 = CARTESIAN_POINT('Ctrl Pts',(28.1324953542873,586.778662171874,-47.6855489862616)) ;
#50919 = CARTESIAN_POINT('Ctrl Pts',(28.1589114778527,586.820929036927,-47.6882526683113)) ;
#50920 = CARTESIAN_POINT('Ctrl Pts',(28.2277374707619,586.922629200175,-47.6950570249377)) ;
#50921 = CARTESIAN_POINT('Ctrl Pts',(28.2718254573564,586.980838934933,-47.6992196674799)) ;
#50922 = CARTESIAN_POINT('Ctrl Pts',(28.4136315333929,587.148696520203,-47.7120397130181)) ;
#50923 = CARTESIAN_POINT('Ctrl Pts',(28.5200895330464,587.250341602668,-47.7209796683478)) ;
#50924 = CARTESIAN_POINT('Ctrl Pts',(28.6364501397495,587.339767275828,-47.7296820333927)) ;
#50925 = CARTESIAN_POINT('Ctrl Pts',(28.6364422247126,587.339761192919,-47.7296814414422)) ;
#50926 = CARTESIAN_POINT('Ctrl Pts',(28.6824239637675,587.375099521165,-47.733120337256)) ;
#50927 = CARTESIAN_POINT('Ctrl Pts',(28.7298764916139,587.408472467074,-47.7365108495857)) ;
#50928 = CARTESIAN_POINT('Ctrl Pts',(28.8011066382216,587.454188607936,-47.7413072153448)) ;
#50929 = CARTESIAN_POINT('Ctrl Pts',(28.8238032681358,587.468140002077,-47.7427942145078)) ;
#50930 = CARTESIAN_POINT('Ctrl Pts',(28.8736065695272,587.497434626283,-47.7459576724762)) ;
#50931 = CARTESIAN_POINT('Ctrl Pts',(28.9008028245355,587.512610394951,-47.7476214770647)) ;
#50932 = CARTESIAN_POINT('Ctrl Pts',(28.9755781080381,587.552134138423,-47.7520520266294)) ;
#50933 = CARTESIAN_POINT('Ctrl Pts',(29.0237816085301,587.575255016306,-47.7547547867105)) ;
#50934 = CARTESIAN_POINT('Ctrl Pts',(29.1963957008045,587.649914106246,-47.7640861401261)) ;
#50935 = CARTESIAN_POINT('Ctrl Pts',(29.3249122544347,587.691085679759,-47.7704390440422)) ;
#50936 = CARTESIAN_POINT('Ctrl Pts',(29.521901707099,587.733447543895,-47.780329622509)) ;
#50937 = CARTESIAN_POINT('Ctrl Pts',(29.5879097366807,587.744304487177,-47.7836642756877)) ;
#50938 = CARTESIAN_POINT('Ctrl Pts',(29.7081549116701,587.758100000751,-47.7898716357544)) ;
#50939 = CARTESIAN_POINT('Ctrl Pts',(29.7622030695182,587.762143729498,-47.7927092136559)) ;
#50940 = CARTESIAN_POINT('Ctrl Pts',(29.8674117401597,587.765841961987,-47.7983577551711)) ;
#50941 = CARTESIAN_POINT('Ctrl Pts',(29.9185241183404,587.765731371519,-47.8011589785321)) ;
#50942 = CARTESIAN_POINT('Ctrl Pts',(30.0617085907539,587.760079130019,-47.8091822413788)) ;
#50943 = CARTESIAN_POINT('Ctrl Pts',(30.1534808935024,587.750245395855,-47.8145343646433)) ;
#50944 = CARTESIAN_POINT('Ctrl Pts',(30.359317180954,587.714061767701,-47.8269363661386)) ;
#50945 = CARTESIAN_POINT('Ctrl Pts',(30.4724214579021,587.684066653035,-47.8340407963561)) ;
#50946 = CARTESIAN_POINT('Ctrl Pts',(30.6247391686622,587.629423422938,-47.8436530868642)) ;
#50947 = CARTESIAN_POINT('Ctrl Pts',(30.666607235695,587.612831446989,-47.8462980778568)) ;
#50948 = CARTESIAN_POINT('Ctrl Pts',(30.7412348310008,587.580380508186,-47.8509781550086)) ;
#50949 = CARTESIAN_POINT('Ctrl Pts',(30.7741830627879,587.565001414862,-47.8530317237531)) ;
#50950 = CARTESIAN_POINT('Ctrl Pts',(30.8335104181901,587.53536725649,-47.8566827033609)) ;
#50951 = CARTESIAN_POINT('Ctrl Pts',(30.8600163426123,587.521395047013,-47.858294053187)) ;
#50952 = CARTESIAN_POINT('Ctrl Pts',(30.9386460594716,587.47772299346,-47.8630368487413)) ;
#50953 = CARTESIAN_POINT('Ctrl Pts',(30.989787787867,587.446313630178,-47.8660737633124)) ;
#50954 = CARTESIAN_POINT('Ctrl Pts',(31.1511088600168,587.337231335096,-47.8757313328263)) ;
#50955 = CARTESIAN_POINT('Ctrl Pts',(31.2550393687273,587.250955542727,-47.882098111838)) ;
#50956 = CARTESIAN_POINT('Ctrl Pts',(31.3969579715102,587.107396990695,-47.8920286314581)) ;
#50957 = CARTESIAN_POINT('Ctrl Pts',(31.4417690113181,587.057391616715,-47.8953846192265)) ;
#50958 = CARTESIAN_POINT('Ctrl Pts',(31.5178336423956,586.963654900244,-47.9015933280279)) ;
#50959 = CARTESIAN_POINT('Ctrl Pts',(31.5499715471862,586.920720269273,-47.9044087387962)) ;
#50960 = CARTESIAN_POINT('Ctrl Pts',(31.6098659187617,586.833814757294,-47.9100849141257)) ;
#50961 = CARTESIAN_POINT('Ctrl Pts',(31.6377054130344,586.789949960652,-47.9129394017441)) ;
#50962 = CARTESIAN_POINT('Ctrl Pts',(31.7563361671869,586.586368562414,-47.926166304809)) ;
#50963 = CARTESIAN_POINT('Ctrl Pts',(31.8271070476719,586.41599171671,-47.9372812364368)) ;
#50964 = CARTESIAN_POINT('Ctrl Pts',(31.8946776028362,586.161847301536,-47.9530245803131)) ;
#50965 = CARTESIAN_POINT('Ctrl Pts',(31.9106083177976,586.084042191839,-47.9577222140946)) ;
#50966 = CARTESIAN_POINT('Ctrl Pts',(31.9265403086592,585.974198569042,-47.9640213406026)) ;
#50967 = CARTESIAN_POINT('Ctrl Pts',(31.9303579035701,585.942788656879,-47.9657847128987)) ;
#50968 = CARTESIAN_POINT('Ctrl Pts',(31.9367236079293,585.877940180081,-47.9693303378259)) ;
#50969 = CARTESIAN_POINT('Ctrl Pts',(31.9391817100796,585.844502811593,-47.9711079582763)) ;
#50970 = CARTESIAN_POINT('Ctrl Pts',(31.9471323072716,585.682069113005,-47.9795619645583)) ;
#50971 = CARTESIAN_POINT('Ctrl Pts',(31.9412774670893,585.552797949443,-47.9857492176068)) ;
#50972 = CARTESIAN_POINT('Ctrl Pts',(31.9063792546025,585.304199292865,-47.9979042033426)) ;
#50973 = CARTESIAN_POINT('Ctrl Pts',(31.8787237778798,585.185232675492,-48.0038451310871)) ;
#50974 = CARTESIAN_POINT('Ctrl Pts',(31.824026800936,585.018689038426,-48.0128699415235)) ;
#50975 = CARTESIAN_POINT('Ctrl Pts',(31.805392504124,584.968623134488,-48.0156770104237)) ;
#50976 = CARTESIAN_POINT('Ctrl Pts',(31.7647433622415,584.871200380387,-48.0213587486375)) ;
#50977 = CARTESIAN_POINT('Ctrl Pts',(31.7428317519569,584.823844107924,-48.0242282133877)) ;
#50978 = CARTESIAN_POINT('Ctrl Pts',(31.6377074933674,584.617624340005,-48.0372337905549)) ;
#50979 = CARTESIAN_POINT('Ctrl Pts',(31.5357205058415,584.469241835868,-48.0480686431251)) ;
#50980 = CARTESIAN_POINT('Ctrl Pts',(31.3606108890533,584.274676360172,-48.0637589076327)) ;
#50981 = CARTESIAN_POINT('Ctrl Pts',(31.3017641100319,584.216720889008,-48.0686546326443)) ;
#50982 = CARTESIAN_POINT('Ctrl Pts',(31.2156033532213,584.141526958755,-48.0751505388989)) ;
#50983 = CARTESIAN_POINT('Ctrl Pts',(31.1911346901922,584.121154563864,-48.0769265792578)) ;
#50984 = CARTESIAN_POINT('Ctrl Pts',(31.1402183921068,584.080728232137,-48.080467117722)) ;
#50985 = CARTESIAN_POINT('Ctrl Pts',(31.1137388779886,584.060730060345,-48.0822281910013)) ;
#50986 = CARTESIAN_POINT('Ctrl Pts',(30.978719694028,583.963803844077,-48.0908771326382)) ;
#50987 = CARTESIAN_POINT('Ctrl Pts',(30.8633639178683,583.896895993447,-48.0972385578789)) ;
#50988 = CARTESIAN_POINT('Ctrl Pts',(30.6336529125506,583.791955335237,-48.109468931987)) ;
#50989 = CARTESIAN_POINT('Ctrl Pts',(30.5208503590398,583.751881955797,-48.1153012344371)) ;
#50990 = CARTESIAN_POINT('Ctrl Pts',(30.3536895456436,583.708452298691,-48.124196677322)) ;
#50991 = CARTESIAN_POINT('Ctrl Pts',(30.3016679832874,583.697074192168,-48.1269959652828)) ;
#50992 = CARTESIAN_POINT('Ctrl Pts',(30.1978439860137,583.678558937028,-48.1326742082429)) ;
#50993 = CARTESIAN_POINT('Ctrl Pts',(30.146094564906,583.671353434077,-48.1355485533053)) ;
#50994 = CARTESIAN_POINT('Ctrl Pts',(29.9183362257767,583.648448531857,-48.1484152304664)) ;
#50995 = CARTESIAN_POINT('Ctrl Pts',(29.7410198324542,583.653520172812,-48.1590814486319)) ;
#50996 = CARTESIAN_POINT('Ctrl Pts',(29.4833452460618,583.694398698308,-48.1747279541632)) ;
#50997 = CARTESIAN_POINT('Ctrl Pts',(29.4009942358834,583.712712929357,-48.1797337826392)) ;
#50998 = CARTESIAN_POINT('Ctrl Pts',(29.2893122274845,583.744869873336,-48.1863379078977)) ;
#50999 = CARTESIAN_POINT('Ctrl Pts',(29.2588368531494,583.754419225053,-48.1881200510754)) ;
#51000 = CARTESIAN_POINT('Ctrl Pts',(29.1973095361061,583.775285748045,-48.1916594170515)) ;
#51001 = CARTESIAN_POINT('Ctrl Pts',(29.1662834416572,583.786649239736,-48.1934137471815)) ;
#51002 = CARTESIAN_POINT('Ctrl Pts',(29.0102494313651,583.848104778917,-48.2021442611999)) ;
#51003 = CARTESIAN_POINT('Ctrl Pts',(28.8900962194717,583.909655925334,-48.2085781117679)) ;
#51004 = CARTESIAN_POINT('Ctrl Pts',(28.675545236477,584.047684154462,-48.2209340870237)) ;
#51005 = CARTESIAN_POINT('Ctrl Pts',(28.5801994991868,584.121611589251,-48.2268168573551)) ;
#51006 = CARTESIAN_POINT('Ctrl Pts',(28.4531719460388,584.239328606531,-48.2357514893828)) ;
#51007 = CARTESIAN_POINT('Ctrl Pts',(28.4158607922054,584.276677212472,-48.2385311079599)) ;
#51008 = CARTESIAN_POINT('Ctrl Pts',(28.3442567741649,584.354098782591,-48.2442168507004)) ;
#51009 = CARTESIAN_POINT('Ctrl Pts',(28.3099865598374,584.394137846638,-48.2471206136923)) ;
#51010 = CARTESIAN_POINT('Ctrl Pts',(28.1749867453748,584.56472294007,-48.2593677038929)) ;
#51011 = CARTESIAN_POINT('Ctrl Pts',(28.0886231978602,584.705824474986,-48.2692774453331)) ;
#51012 = CARTESIAN_POINT('Ctrl Pts',(27.9934242252772,584.913898527553,-48.2830221519237)) ;
#51013 = CARTESIAN_POINT('Ctrl Pts',(27.9695268578066,584.973319331029,-48.2868490426797)) ;
#51014 = CARTESIAN_POINT('Ctrl Pts',(27.9334539723609,585.076723707667,-48.2932466069319)) ;
#51015 = CARTESIAN_POINT('Ctrl Pts',(27.9198964153185,585.120175665592,-48.2958584953778)) ;
#51016 = CARTESIAN_POINT('Ctrl Pts',(27.9000910882341,585.191955481162,-48.3000097033398)) ;
#51017 = CARTESIAN_POINT('Ctrl Pts',(27.8929810953536,585.220024496866,-48.3015911007769)) ;
#51018 = CARTESIAN_POINT('Ctrl Pts',(27.881880517771,585.268094598002,-48.3042289210213)) ;
#51019 = CARTESIAN_POINT('Ctrl Pts',(27.8775912202124,585.28801630178,-48.3053027255326)) ;
#51020 = CARTESIAN_POINT('Ctrl Pts',(27.8735990519255,585.30799789136,-48.3063633758768)) ;
#51021 = CARTESIAN_POINT('Origin',(29.8885276254155,585.710565160562,-51.0680854522906)) ;
#51022 = CARTESIAN_POINT('',(27.87359904473,585.307997927374,-49.0033678628587)) ;
#51023 = CARTESIAN_POINT('',(27.8735990520585,585.307997890694,-48.9453612460011)) ;
#51024 = CARTESIAN_POINT('',(27.8735990520584,585.307997890694,-51.0680854522905)) ;
#51025 = CARTESIAN_POINT('',(28.6368801712448,587.339287485482,-49.1271361537871)) ;
#51026 = CARTESIAN_POINT('Ctrl Pts',(27.873599044712,585.307997927464,-49.0033678610064)) ;
#51027 = CARTESIAN_POINT('Ctrl Pts',(27.8698044451442,585.326990648413,-49.0043292920081)) ;
#51028 = CARTESIAN_POINT('Ctrl Pts',(27.8662773002645,585.346042440035,-49.0052965367617)) ;
#51029 = CARTESIAN_POINT('Ctrl Pts',(27.8522738852341,585.428157689329,-49.0094833265671)) ;
#51030 = CARTESIAN_POINT('Ctrl Pts',(27.8444753952256,585.491629795012,-49.0127661281195)) ;
#51031 = CARTESIAN_POINT('Ctrl Pts',(27.8359270169899,585.604476743004,-49.0187470486518)) ;
#51032 = CARTESIAN_POINT('Ctrl Pts',(27.8339739363669,585.653709544196,-49.0214042849436)) ;
#51033 = CARTESIAN_POINT('Ctrl Pts',(27.8335495298772,585.768407778413,-49.0277249220421)) ;
#51034 = CARTESIAN_POINT('Ctrl Pts',(27.8364342456864,585.833821556768,-49.0314290385932)) ;
#51035 = CARTESIAN_POINT('Ctrl Pts',(27.8499665688143,585.980774838618,-49.0399727484017)) ;
#51036 = CARTESIAN_POINT('Ctrl Pts',(27.8623957923818,586.062036905603,-49.0448547447766)) ;
#51037 = CARTESIAN_POINT('Ctrl Pts',(27.9082682901971,586.275467394998,-49.0579623338322)) ;
#51038 = CARTESIAN_POINT('Ctrl Pts',(27.9500484921029,586.405434989352,-49.0662576607064)) ;
#51039 = CARTESIAN_POINT('Ctrl Pts',(28.0174950170872,586.560456219298,-49.0759010162996)) ;
#51040 = CARTESIAN_POINT('Ctrl Pts',(28.03132982233,586.590277867984,-49.0777424831793)) ;
#51041 = CARTESIAN_POINT('Ctrl Pts',(28.0601800189521,586.64874837403,-49.0813066865867)) ;
#51042 = CARTESIAN_POINT('Ctrl Pts',(28.0751680862041,586.677400285444,-49.0830304273165)) ;
#51043 = CARTESIAN_POINT('Ctrl Pts',(28.1336480025451,586.78304487914,-49.0893437095975)) ;
#51044 = CARTESIAN_POINT('Ctrl Pts',(28.1814216529146,586.857564431637,-49.0937131246284)) ;
#51045 = CARTESIAN_POINT('Ctrl Pts',(28.3174912346045,587.042384919887,-49.104909569831)) ;
#51046 = CARTESIAN_POINT('Ctrl Pts',(28.4126026257719,587.147069027542,-49.1116446440223)) ;
#51047 = CARTESIAN_POINT('Ctrl Pts',(28.5560453762575,587.275538057089,-49.1213964028017)) ;
#51048 = CARTESIAN_POINT('Ctrl Pts',(28.5956789397844,587.308435868694,-49.1240512373501)) ;
#51049 = CARTESIAN_POINT('Ctrl Pts',(28.6365041795376,587.339808805163,-49.1267657875976)) ;
#51050 = CARTESIAN_POINT('',(31.9432775542228,585.710024266058,-49.3762357692215)) ;
#51051 = CARTESIAN_POINT('Ctrl Pts',(31.9427342614473,585.709985596129,-49.3752948960846)) ;
#51052 = CARTESIAN_POINT('Ctrl Pts',(31.9426172492493,585.780898218238,-49.3712207238047)) ;
#51053 = CARTESIAN_POINT('Ctrl Pts',(31.9388560335549,585.851852550851,-49.3672016667734)) ;
#51054 = CARTESIAN_POINT('Ctrl Pts',(31.9314771415032,585.922451909701,-49.3632671281545)) ;
#51055 = CARTESIAN_POINT('Ctrl Pts',(31.9241001716764,585.993032877193,-49.3593336144954)) ;
#51056 = CARTESIAN_POINT('Ctrl Pts',(31.9131074252591,586.063259034058,-49.3554846054318)) ;
#51057 = CARTESIAN_POINT('Ctrl Pts',(31.8985598759689,586.132738183609,-49.3517248952043)) ;
#51058 = CARTESIAN_POINT('Ctrl Pts',(31.8840111309949,586.202223043751,-49.347964875961)) ;
#51059 = CARTESIAN_POINT('Ctrl Pts',(31.8659069048801,586.27096070311,-49.3442940977577)) ;
#51060 = CARTESIAN_POINT('Ctrl Pts',(31.8443432717175,586.338563738127,-49.3406930811079)) ;
#51061 = CARTESIAN_POINT('Ctrl Pts',(31.8227548532057,586.406244476415,-49.3370879254312)) ;
#51062 = CARTESIAN_POINT('Ctrl Pts',(31.7976988646946,586.472787848852,-49.3335525062726)) ;
#51063 = CARTESIAN_POINT('Ctrl Pts',(31.7693091276861,586.537811473414,-49.3300448494271)) ;
#51064 = CARTESIAN_POINT('Ctrl Pts',(31.7409018983242,586.602875162322,-49.3265350313368)) ;
#51065 = CARTESIAN_POINT('Ctrl Pts',(31.709156496649,586.666416994456,-49.3230526645967)) ;
#51066 = CARTESIAN_POINT('Ctrl Pts',(31.6742483334829,586.728062954153,-49.3195371923347)) ;
#51067 = CARTESIAN_POINT('Ctrl Pts',(31.64135561025,586.786149754111,-49.316224687589)) ;
#51068 = CARTESIAN_POINT('Ctrl Pts',(31.605654388214,586.842553459408,-49.3128822981287)) ;
#51069 = CARTESIAN_POINT('Ctrl Pts',(31.5673306236686,586.896971209509,-49.3094494968086)) ;
#51070 = CARTESIAN_POINT('Ctrl Pts',(31.5649058173613,586.900414308203,-49.3092322979402)) ;
#51071 = CARTESIAN_POINT('Ctrl Pts',(31.5624705110518,586.903849473833,-49.3090147371263)) ;
#51072 = CARTESIAN_POINT('Ctrl Pts',(31.5600247511938,586.907276636694,-49.3087967990357)) ;
#51073 = CARTESIAN_POINT('Ctrl Pts',(31.5337788156842,586.944054203026,-49.3064580620361)) ;
#51074 = CARTESIAN_POINT('Ctrl Pts',(31.5063302027123,586.979908205151,-49.3040756442879)) ;
#51075 = CARTESIAN_POINT('Ctrl Pts',(31.4777482332981,587.014748947238,-49.3016299549295)) ;
#51076 = CARTESIAN_POINT('Ctrl Pts',(31.4777263603074,587.014775609894,-49.3016280833111)) ;
#51077 = CARTESIAN_POINT('Ctrl Pts',(31.477704486653,587.014802271958,-49.3016262116556)) ;
#51078 = CARTESIAN_POINT('Ctrl Pts',(31.4776826123349,587.014828933428,-49.3016243399631)) ;
#51079 = CARTESIAN_POINT('Ctrl Pts',(31.436861728681,587.064583389718,-49.2981314702291)) ;
#51080 = CARTESIAN_POINT('Ctrl Pts',(31.3935720803975,587.112452150401,-49.2945002447966)) ;
#51081 = CARTESIAN_POINT('Ctrl Pts',(31.3480347240497,587.158205432452,-49.2907957449888)) ;
#51082 = CARTESIAN_POINT('Ctrl Pts',(31.3434184878396,587.162843557593,-49.290420210537)) ;
#51083 = CARTESIAN_POINT('Ctrl Pts',(31.3387791966602,587.167459934781,-49.2900439230894)) ;
#51084 = CARTESIAN_POINT('Ctrl Pts',(31.3341171101784,587.172054319618,-49.2896669504441)) ;
#51085 = CARTESIAN_POINT('Ctrl Pts',(31.2835431316144,587.221893875607,-49.285577578323)) ;
#51086 = CARTESIAN_POINT('Ctrl Pts',(31.23028090373,587.26914702563,-49.281408189495)) ;
#51087 = CARTESIAN_POINT('Ctrl Pts',(31.1746498895808,587.313549893559,-49.277233146996)) ;
#51088 = CARTESIAN_POINT('Ctrl Pts',(31.1190876190499,587.357897892566,-49.2730632636251)) ;
#51089 = CARTESIAN_POINT('Ctrl Pts',(31.0611626005585,587.399402981729,-49.2688880941617)) ;
#51090 = CARTESIAN_POINT('Ctrl Pts',(31.0012105162553,587.437838534679,-49.2647623759951)) ;
#51091 = CARTESIAN_POINT('Ctrl Pts',(30.9412984971703,587.476248401636,-49.2606394149936)) ;
#51092 = CARTESIAN_POINT('Ctrl Pts',(30.8793621854795,587.511592996215,-49.2565660081323)) ;
#51093 = CARTESIAN_POINT('Ctrl Pts',(30.815752194817,587.543678693284,-49.2525735976269)) ;
#51094 = CARTESIAN_POINT('Ctrl Pts',(30.7521633355493,587.575753731407,-49.2485825134101)) ;
#51095 = CARTESIAN_POINT('Ctrl Pts',(30.6869019273906,587.604572051931,-49.2446724121268)) ;
#51096 = CARTESIAN_POINT('Ctrl Pts',(30.6203332569447,587.629971459751,-49.2408499953985)) ;
#51097 = CARTESIAN_POINT('Ctrl Pts',(30.553764328658,587.655370965951,-49.2370275638647)) ;
#51098 = CARTESIAN_POINT('Ctrl Pts',(30.4858881272273,587.677351423859,-49.2332927529147)) ;
#51099 = CARTESIAN_POINT('Ctrl Pts',(30.4170848505969,587.695782599759,-49.229627736439)) ;
#51100 = CARTESIAN_POINT('Ctrl Pts',(30.3482126673851,587.71423223451,-49.225959049444)) ;
#51101 = CARTESIAN_POINT('Ctrl Pts',(30.2784115413041,587.729125234615,-49.2223601185614)) ;
#51102 = CARTESIAN_POINT('Ctrl Pts',(30.2080778479719,587.7403656115,-49.2187902775781)) ;
#51103 = CARTESIAN_POINT('Ctrl Pts',(30.1377062821471,587.751612040975,-49.2152185143472)) ;
#51104 = CARTESIAN_POINT('Ctrl Pts',(30.0668015934413,587.759201521747,-49.2116755348893)) ;
#51105 = CARTESIAN_POINT('Ctrl Pts',(29.9957758320383,587.76307726195,-49.2081016313498)) ;
#51106 = CARTESIAN_POINT('Ctrl Pts',(29.9285127086579,587.76674768218,-49.2047170577813)) ;
#51107 = CARTESIAN_POINT('Ctrl Pts',(29.86114066399,587.767087135098,-49.2013042591977)) ;
#51108 = CARTESIAN_POINT('Ctrl Pts',(29.7940228864242,587.764086216671,-49.1978020133309)) ;
#51109 = CARTESIAN_POINT('Ctrl Pts',(29.790146426521,587.763912895379,-49.1975997373295)) ;
#51110 = CARTESIAN_POINT('Ctrl Pts',(29.7862708020056,587.763728438147,-49.1973971629529)) ;
#51111 = CARTESIAN_POINT('Ctrl Pts',(29.782396078083,587.763532845537,-49.197194278406)) ;
#51112 = CARTESIAN_POINT('Ctrl Pts',(29.7393732962058,587.761361093854,-49.1949415611081)) ;
#51113 = CARTESIAN_POINT('Ctrl Pts',(29.6964635965521,587.757816517172,-49.1926503845548)) ;
#51114 = CARTESIAN_POINT('Ctrl Pts',(29.6537643586418,587.752906705734,-49.1903039237657)) ;
#51115 = CARTESIAN_POINT('Ctrl Pts',(29.6537316936418,587.752902949718,-49.1903021287186)) ;
#51116 = CARTESIAN_POINT('Ctrl Pts',(29.6536990287645,587.752899192904,-49.1903003336392)) ;
#51117 = CARTESIAN_POINT('Ctrl Pts',(29.6536663640099,587.752895435292,-49.1902985385274)) ;
#51118 = CARTESIAN_POINT('Ctrl Pts',(29.5893679958149,587.745498828152,-49.1867649819548)) ;
#51119 = CARTESIAN_POINT('Ctrl Pts',(29.5253262751425,587.734974334743,-49.1830973483189)) ;
#51120 = CARTESIAN_POINT('Ctrl Pts',(29.4618575879369,587.721385123318,-49.1793605809766)) ;
#51121 = CARTESIAN_POINT('Ctrl Pts',(29.4556601922994,587.720058205695,-49.1789957045841)) ;
#51122 = CARTESIAN_POINT('Ctrl Pts',(29.4494682887654,587.718702096905,-49.178630169034)) ;
#51123 = CARTESIAN_POINT('Ctrl Pts',(29.4432821898818,587.717316875284,-49.1782640347885)) ;
#51124 = CARTESIAN_POINT('Ctrl Pts',(29.3742108042705,587.701850071642,-49.1741759333643)) ;
#51125 = CARTESIAN_POINT('Ctrl Pts',(29.3058592650622,587.682749896166,-49.1700139311333)) ;
#51126 = CARTESIAN_POINT('Ctrl Pts',(29.2386150934843,587.66014120432,-49.1658496212785)) ;
#51127 = CARTESIAN_POINT('Ctrl Pts',(29.2350456187028,587.658941083128,-49.1656285701649)) ;
#51128 = CARTESIAN_POINT('Ctrl Pts',(29.2314792738871,587.657731083287,-49.165407512549)) ;
#51129 = CARTESIAN_POINT('Ctrl Pts',(29.2279161201886,587.656511226047,-49.1651864591392)) ;
#51130 = CARTESIAN_POINT('Ctrl Pts',(29.1605148218425,587.633436172678,-49.161004970468)) ;
#51131 = CARTESIAN_POINT('Ctrl Pts',(29.0942511943318,587.606831581313,-49.1568251938135)) ;
#51132 = CARTESIAN_POINT('Ctrl Pts',(29.0294972717457,587.576859537621,-49.1526995732383)) ;
#51133 = CARTESIAN_POINT('Ctrl Pts',(28.9647862388391,587.546907345874,-49.1485766852627)) ;
#51134 = CARTESIAN_POINT('Ctrl Pts',(28.9015828172753,587.513592293906,-49.1445080396037)) ;
#51135 = CARTESIAN_POINT('Ctrl Pts',(28.8402394930402,587.47710674899,-49.1405226886402)) ;
#51136 = CARTESIAN_POINT('Ctrl Pts',(28.778912778203,587.440631082948,-49.1365384167554)) ;
#51137 = CARTESIAN_POINT('Ctrl Pts',(28.7194451568417,587.400986656831,-49.1326374267466)) ;
#51138 = CARTESIAN_POINT('Ctrl Pts',(28.6621707030406,587.35839521496,-49.1288240727973)) ;
#51139 = CARTESIAN_POINT('Ctrl Pts',(28.6536921476701,587.352090241726,-49.1282595674994)) ;
#51140 = CARTESIAN_POINT('Ctrl Pts',(28.6452616206402,587.34572074037,-49.1276969384294)) ;
#51141 = CARTESIAN_POINT('Ctrl Pts',(28.6368801712448,587.339287485482,-49.1271361537871)) ;
#51142 = CARTESIAN_POINT('',(30.4186978426039,583.72539083489,-49.522160171753)) ;
#51143 = CARTESIAN_POINT('Ctrl Pts',(30.4186978426039,583.72539083489,-49.522160171753)) ;
#51144 = CARTESIAN_POINT('Ctrl Pts',(30.4888501130091,583.74412603812,-49.5182232094813)) ;
#51145 = CARTESIAN_POINT('Ctrl Pts',(30.558074738389,583.766601784023,-49.5142862472096)) ;
#51146 = CARTESIAN_POINT('Ctrl Pts',(30.6259577141875,583.792703219057,-49.5103492849379)) ;
#51147 = CARTESIAN_POINT('Ctrl Pts',(30.6937865685899,583.81878384407,-49.5064154615077)) ;
#51148 = CARTESIAN_POINT('Ctrl Pts',(30.760275471702,583.848484245838,-49.5024816380774)) ;
#51149 = CARTESIAN_POINT('Ctrl Pts',(30.8250269986058,583.881640206794,-49.4985478146471)) ;
#51150 = CARTESIAN_POINT('Ctrl Pts',(30.8897595713106,583.91478646227,-49.4946151427336)) ;
#51151 = CARTESIAN_POINT('Ctrl Pts',(30.9527553659939,583.95138606332,-49.4906824708202)) ;
#51152 = CARTESIAN_POINT('Ctrl Pts',(31.0136393435251,583.991227734612,-49.4867497989067)) ;
#51153 = CARTESIAN_POINT('Ctrl Pts',(31.0745166320784,584.031065028725,-49.4828175590536)) ;
#51154 = CARTESIAN_POINT('Ctrl Pts',(31.1332821791065,584.074143433347,-49.4788853192006)) ;
#51155 = CARTESIAN_POINT('Ctrl Pts',(31.1895891663767,584.120207833062,-49.4749530793475)) ;
#51156 = CARTESIAN_POINT('Ctrl Pts',(31.2459058658637,584.166280178283,-49.4710201612346)) ;
#51157 = CARTESIAN_POINT('Ctrl Pts',(31.2997628065398,584.215339250336,-49.4670872431217)) ;
#51158 = CARTESIAN_POINT('Ctrl Pts',(31.3508466536646,584.267089971263,-49.4631543250089)) ;
#51159 = CARTESIAN_POINT('Ctrl Pts',(31.4019537376977,584.318864232445,-49.4592196178989)) ;
#51160 = CARTESIAN_POINT('Ctrl Pts',(31.4502848981567,584.37333224797,-49.4552849107888)) ;
#51161 = CARTESIAN_POINT('Ctrl Pts',(31.4955650057395,584.430163496731,-49.4513502036788)) ;
#51162 = CARTESIAN_POINT('Ctrl Pts',(31.5409123064666,584.487079079883,-49.4474096576837)) ;
#51163 = CARTESIAN_POINT('Ctrl Pts',(31.5831992298913,584.54636453527,-49.4434691116887)) ;
#51164 = CARTESIAN_POINT('Ctrl Pts',(31.6221924502075,584.607658166397,-49.4395285656936)) ;
#51165 = CARTESIAN_POINT('Ctrl Pts',(31.6612182030292,584.669002935526,-49.4355847320544)) ;
#51166 = CARTESIAN_POINT('Ctrl Pts',(31.6969445538274,584.732358816368,-49.4316408984151)) ;
#51167 = CARTESIAN_POINT('Ctrl Pts',(31.7291841391883,584.7973394706,-49.4276970647759)) ;
#51168 = CARTESIAN_POINT('Ctrl Pts',(31.7614851795532,584.862443990767,-49.4237457134124)) ;
#51169 = CARTESIAN_POINT('Ctrl Pts',(31.7902860006525,584.929179046084,-49.4197943620489)) ;
#51170 = CARTESIAN_POINT('Ctrl Pts',(31.8154475092004,584.997138693451,-49.4158430106855)) ;
#51171 = CARTESIAN_POINT('Ctrl Pts',(31.8258590807965,585.025259691556,-49.4142079824222)) ;
#51172 = CARTESIAN_POINT('Ctrl Pts',(31.8356481175698,585.053590198989,-49.4125729541589)) ;
#51173 = CARTESIAN_POINT('Ctrl Pts',(31.8448073056395,585.082100861462,-49.4109379258956)) ;
#51174 = CARTESIAN_POINT('Ctrl Pts',(31.8703011837991,585.161458043541,-49.4063869535808)) ;
#51175 = CARTESIAN_POINT('Ctrl Pts',(31.8909902102017,585.242454756208,-49.4018359812659)) ;
#51176 = CARTESIAN_POINT('Ctrl Pts',(31.9066925957177,585.324549985801,-49.3972850089511)) ;
#51177 = CARTESIAN_POINT('Ctrl Pts',(31.9222261861017,585.405762720496,-49.392782957991)) ;
#51178 = CARTESIAN_POINT('Ctrl Pts',(31.9328796837084,585.488050365867,-49.3882809070309)) ;
#51179 = CARTESIAN_POINT('Ctrl Pts',(31.9385232994617,585.570867992043,-49.3837788560708)) ;
#51180 = CARTESIAN_POINT('Ctrl Pts',(31.941675217269,585.617121025933,-49.3812644937877)) ;
#51181 = CARTESIAN_POINT('Ctrl Pts',(31.9432653173924,585.663538997459,-49.3787501315046)) ;
#51182 = CARTESIAN_POINT('Ctrl Pts',(31.9432775542228,585.710024266058,-49.3762357692215)) ;
#51183 = CARTESIAN_POINT('',(29.3554857494733,583.724023010006,-49.520969598848)) ;
#51184 = CARTESIAN_POINT('Origin',(29.8885276254156,585.710565160562,-49.522160171753)) ;
#51185 = CARTESIAN_POINT('',(31.9432771921379,585.711899534809,-49.3167515585946)) ;
#51186 = CARTESIAN_POINT('Ctrl Pts',(29.3561032364248,583.725994216376,-49.5197697712619)) ;
#51187 = CARTESIAN_POINT('Ctrl Pts',(29.3727496069743,583.721528297083,-49.5188380786254)) ;
#51188 = CARTESIAN_POINT('Ctrl Pts',(29.389452098046,583.717271838321,-49.5179182347525)) ;
#51189 = CARTESIAN_POINT('Ctrl Pts',(29.42760619351,583.708058322594,-49.5158469303205)) ;
#51190 = CARTESIAN_POINT('Ctrl Pts',(29.4490880857081,583.703234803234,-49.5147020929892)) ;
#51191 = CARTESIAN_POINT('Ctrl Pts',(29.5663997223961,583.678867367023,-49.5085458593304)) ;
#51192 = CARTESIAN_POINT('Ctrl Pts',(29.6634613133756,583.665837660712,-49.50379362785)) ;
#51193 = CARTESIAN_POINT('Ctrl Pts',(29.8914659820262,583.651669118604,-49.4927219890668)) ;
#51194 = CARTESIAN_POINT('Ctrl Pts',(30.0223150288558,583.656019056726,-49.4864219419482)) ;
#51195 = CARTESIAN_POINT('Ctrl Pts',(30.2079227031544,583.680003598257,-49.476865979507)) ;
#51196 = CARTESIAN_POINT('Ctrl Pts',(30.2636620249336,583.689558760685,-49.4739182958809)) ;
#51197 = CARTESIAN_POINT('Ctrl Pts',(30.368021836059,583.711914837146,-49.4682127044214)) ;
#51198 = CARTESIAN_POINT('Ctrl Pts',(30.41670492817,583.724225328291,-49.465472590941)) ;
#51199 = CARTESIAN_POINT('Ctrl Pts',(30.5448306417442,583.761667801151,-49.458034393887)) ;
#51200 = CARTESIAN_POINT('Ctrl Pts',(30.6232726258301,583.7898669098,-49.4532402606485)) ;
#51201 = CARTESIAN_POINT('Ctrl Pts',(30.8144589531098,583.872025401809,-49.4409931195026)) ;
#51202 = CARTESIAN_POINT('Ctrl Pts',(30.9244067011359,583.931652770115,-49.4334202284699)) ;
#51203 = CARTESIAN_POINT('Ctrl Pts',(31.0665972759726,584.02644139404,-49.4232832711087)) ;
#51204 = CARTESIAN_POINT('Ctrl Pts',(31.1040705280601,584.053285202713,-49.4205781844057)) ;
#51205 = CARTESIAN_POINT('Ctrl Pts',(31.1698897288773,584.103869088047,-49.4158069079045)) ;
#51206 = CARTESIAN_POINT('Ctrl Pts',(31.1985584653246,584.12715722885,-49.4137214875302)) ;
#51207 = CARTESIAN_POINT('Ctrl Pts',(31.2492766783299,584.170677643862,-49.4100429487759)) ;
#51208 = CARTESIAN_POINT('Ctrl Pts',(31.2715393300356,584.190640749755,-49.4084346002827)) ;
#51209 = CARTESIAN_POINT('Ctrl Pts',(31.3366367885136,584.251629149287,-49.4037303262696)) ;
#51210 = CARTESIAN_POINT('Ctrl Pts',(31.3781421201879,584.294032697368,-49.4007260188503)) ;
#51211 = CARTESIAN_POINT('Ctrl Pts',(31.4872332340532,584.415591058406,-49.3926218442998)) ;
#51212 = CARTESIAN_POINT('Ctrl Pts',(31.5507321885579,584.498172831176,-49.3876553770832)) ;
#51213 = CARTESIAN_POINT('Ctrl Pts',(31.6648373497383,584.672488688262,-49.3775365661717)) ;
#51214 = CARTESIAN_POINT('Ctrl Pts',(31.7152352371349,584.763984231751,-49.3723964178044)) ;
#51215 = CARTESIAN_POINT('Ctrl Pts',(31.7802896740693,584.906820069323,-49.3642967745992)) ;
#51216 = CARTESIAN_POINT('Ctrl Pts',(31.8002618798508,584.955554371325,-49.361522981914)) ;
#51217 = CARTESIAN_POINT('Ctrl Pts',(31.8364526279581,585.054540627552,-49.3558401155416)) ;
#51218 = CARTESIAN_POINT('Ctrl Pts',(31.8526499290609,585.10475755557,-49.3529329405142)) ;
#51219 = CARTESIAN_POINT('Ctrl Pts',(31.9001636109969,585.274118188881,-49.3430319257071)) ;
#51220 = CARTESIAN_POINT('Ctrl Pts',(31.9226980651836,585.395432614009,-49.3357653093595)) ;
#51221 = CARTESIAN_POINT('Ctrl Pts',(31.9403021513818,585.582466556225,-49.324508207457)) ;
#51222 = CARTESIAN_POINT('Ctrl Pts',(31.943319230883,585.64716575147,-49.3206092009813)) ;
#51223 = CARTESIAN_POINT('Ctrl Pts',(31.9432771921379,585.711899534809,-49.3167515585946)) ;
#51224 = CARTESIAN_POINT('Ctrl Pts',(31.9432771921379,585.711899534809,-49.3167515585946)) ;
#51225 = CARTESIAN_POINT('Ctrl Pts',(31.9432348751065,585.777061840039,-49.3128683795542)) ;
#51226 = CARTESIAN_POINT('Ctrl Pts',(31.9400934612341,585.842180325114,-49.3090321149406)) ;
#51227 = CARTESIAN_POINT('Ctrl Pts',(31.9306699451326,585.940273858617,-49.3034191596782)) ;
#51228 = CARTESIAN_POINT('Ctrl Pts',(31.9266694830996,585.973413788179,-49.3015520048186)) ;
#51229 = CARTESIAN_POINT('Ctrl Pts',(31.9172136969372,586.03839582843,-49.2979677778171)) ;
#51230 = CARTESIAN_POINT('Ctrl Pts',(31.91181152813,586.07023519843,-49.2962493140222)) ;
#51231 = CARTESIAN_POINT('Ctrl Pts',(31.8748589370945,586.260689961285,-49.286127665874)) ;
#51232 = CARTESIAN_POINT('Ctrl Pts',(31.8254194120802,586.415272833367,-49.2785375829958)) ;
#51233 = CARTESIAN_POINT('Ctrl Pts',(31.7288202952011,586.627295713425,-49.2672078164776)) ;
#51234 = CARTESIAN_POINT('Ctrl Pts',(31.6959363401496,586.690537026551,-49.2637043358643)) ;
#51235 = CARTESIAN_POINT('Ctrl Pts',(31.6291816385339,586.804082274015,-49.257044942509)) ;
#51236 = CARTESIAN_POINT('Ctrl Pts',(31.5962416654096,586.85484130385,-49.2539200585485)) ;
#51237 = CARTESIAN_POINT('Ctrl Pts',(31.5322057216826,586.944581623722,-49.2480677964579)) ;
#51238 = CARTESIAN_POINT('Ctrl Pts',(31.5018382578407,586.984025999526,-49.2453703059187)) ;
#51239 = CARTESIAN_POINT('Ctrl Pts',(31.4244182089832,587.077368510806,-49.2386557729236)) ;
#51240 = CARTESIAN_POINT('Ctrl Pts',(31.3759279939045,587.12998394573,-49.2345805764577)) ;
#51241 = CARTESIAN_POINT('Ctrl Pts',(31.2220061019296,587.280435885778,-49.2220304549604)) ;
#51242 = CARTESIAN_POINT('Ctrl Pts',(31.108958555868,587.369842396659,-49.213274993064)) ;
#51243 = CARTESIAN_POINT('Ctrl Pts',(30.9298807886466,587.483200319502,-49.2006428123861)) ;
#51244 = CARTESIAN_POINT('Ctrl Pts',(30.8704503577371,587.51679912355,-49.1966338336946)) ;
#51245 = CARTESIAN_POINT('Ctrl Pts',(30.7818980334419,587.561196694896,-49.1910304785662)) ;
#51246 = CARTESIAN_POINT('Ctrl Pts',(30.7540320136384,587.574391960404,-49.1893183707379)) ;
#51247 = CARTESIAN_POINT('Ctrl Pts',(30.6938494436853,587.601248715634,-49.1857441530688)) ;
#51248 = CARTESIAN_POINT('Ctrl Pts',(30.6614599368688,587.614719435174,-49.1838922022212)) ;
#51249 = CARTESIAN_POINT('Ctrl Pts',(30.5010704301565,587.676657465136,-49.1749954499452)) ;
#51250 = CARTESIAN_POINT('Ctrl Pts',(30.3687817933728,587.713086423931,-49.1684820778909)) ;
#51251 = CARTESIAN_POINT('Ctrl Pts',(30.1208877559366,587.755347753783,-49.1562934538899)) ;
#51252 = CARTESIAN_POINT('Ctrl Pts',(30.0065283230978,587.765120962132,-49.1506760898893)) ;
#51253 = CARTESIAN_POINT('Ctrl Pts',(29.8391519457605,587.765400484348,-49.1420354531627)) ;
#51254 = CARTESIAN_POINT('Ctrl Pts',(29.7863647142763,587.76345293798,-49.1392521210079)) ;
#51255 = CARTESIAN_POINT('Ctrl Pts',(29.6805672758382,587.755458985498,-49.1335273754377)) ;
#51256 = CARTESIAN_POINT('Ctrl Pts',(29.6276009230757,587.749377257029,-49.1305869222901)) ;
#51257 = CARTESIAN_POINT('Ctrl Pts',(29.4523709481474,587.722316853398,-49.1205932892199)) ;
#51258 = CARTESIAN_POINT('Ctrl Pts',(29.3317892717943,587.692335160207,-49.1132622141688)) ;
#51259 = CARTESIAN_POINT('Ctrl Pts',(29.1027772765574,587.612832383946,-49.0987110132526)) ;
#51260 = CARTESIAN_POINT('Ctrl Pts',(28.9944563572668,587.564389142153,-49.091532428306)) ;
#51261 = CARTESIAN_POINT('Ctrl Pts',(28.8578944241586,587.488546846559,-49.0825276131734)) ;
#51262 = CARTESIAN_POINT('Ctrl Pts',(28.8253896238524,587.469303816088,-49.0803892924135)) ;
#51263 = CARTESIAN_POINT('Ctrl Pts',(28.7683979620093,587.433406537484,-49.0766745880042)) ;
#51264 = CARTESIAN_POINT('Ctrl Pts',(28.7437085161875,587.417100282464,-49.0750797082498)) ;
#51265 = CARTESIAN_POINT('Ctrl Pts',(28.6724653421315,587.367805219593,-49.0705010853089)) ;
#51266 = CARTESIAN_POINT('Ctrl Pts',(28.6269205256296,587.333402382128,-49.0676013084715)) ;
#51267 = CARTESIAN_POINT('Ctrl Pts',(28.4764516346427,587.20957518737,-49.0579018197985)) ;
#51268 = CARTESIAN_POINT('Ctrl Pts',(28.3791168681472,587.111519152382,-49.051394557796)) ;
#51269 = CARTESIAN_POINT('Ctrl Pts',(28.250033603472,586.952276155568,-49.0413120464771)) ;
#51270 = CARTESIAN_POINT('Ctrl Pts',(28.2103249863393,586.898059918791,-49.0379547049008)) ;
#51271 = CARTESIAN_POINT('Ctrl Pts',(28.1435333773355,586.796808043188,-49.0317195456947)) ;
#51272 = CARTESIAN_POINT('Ctrl Pts',(28.1155222290976,586.750459228287,-49.0288778747164)) ;
#51273 = CARTESIAN_POINT('Ctrl Pts',(28.0641614017278,586.657354613131,-49.0231607390919)) ;
#51274 = CARTESIAN_POINT('Ctrl Pts',(28.0407002835535,586.610707256361,-49.0202922820085)) ;
#51275 = CARTESIAN_POINT('Ctrl Pts',(27.942410589137,586.395202517148,-49.0069960877451)) ;
#51276 = CARTESIAN_POINT('Ctrl Pts',(27.8887905528058,586.217642569628,-48.9958166242235)) ;
#51277 = CARTESIAN_POINT('Ctrl Pts',(27.8470966723024,585.957190937153,-48.9800230846765)) ;
#51278 = CARTESIAN_POINT('Ctrl Pts',(27.8391099652609,585.878356639662,-48.9753360542625)) ;
#51279 = CARTESIAN_POINT('Ctrl Pts',(27.8343230697207,585.767554791414,-48.9690418959603)) ;
#51280 = CARTESIAN_POINT('Ctrl Pts',(27.8336878743545,585.73582680545,-48.9672735116628)) ;
#51281 = CARTESIAN_POINT('Ctrl Pts',(27.8338943420504,585.670270209594,-48.963707112722)) ;
#51282 = CARTESIAN_POINT('Ctrl Pts',(27.8348360297956,585.636452145458,-48.9619142450768)) ;
#51283 = CARTESIAN_POINT('Ctrl Pts',(27.8418201985542,585.503628712772,-48.9550041610073)) ;
#51284 = CARTESIAN_POINT('Ctrl Pts',(27.8541891817581,585.405148119242,-48.9501645139598)) ;
#51285 = CARTESIAN_POINT('Ctrl Pts',(27.8735990520585,585.307997890694,-48.9453612460011)) ;
#51286 = CARTESIAN_POINT('Origin',(29.8885276254068,535.710565160562,-51.0680854522906)) ;
#51287 = CARTESIAN_POINT('',(28.6364363648369,537.33975668942,-47.7296625859471)) ;
#51288 = CARTESIAN_POINT('',(28.6364362717721,537.339756617897,-47.6715263025693)) ;
#51289 = CARTESIAN_POINT('',(28.6364362890686,537.33975663119,-51.0680854522906)) ;
#51290 = CARTESIAN_POINT('',(28.0059001157431,534.887332980459,-47.5221601717529)) ;
#51291 = CARTESIAN_POINT('Ctrl Pts',(28.6364362717721,537.339756617897,-47.6715263025693)) ;
#51292 = CARTESIAN_POINT('Ctrl Pts',(28.6229519010584,537.329393401282,-47.6705367994022)) ;
#51293 = CARTESIAN_POINT('Ctrl Pts',(28.6095949668397,537.318861834874,-47.6695424325092)) ;
#51294 = CARTESIAN_POINT('Ctrl Pts',(28.4906899310523,537.22268988732,-47.6605649924041)) ;
#51295 = CARTESIAN_POINT('Ctrl Pts',(28.3937593383079,537.126946666423,-47.6523161876422)) ;
#51296 = CARTESIAN_POINT('Ctrl Pts',(28.2733592557547,536.981786770602,-47.6412515673653)) ;
#51297 = CARTESIAN_POINT('Ctrl Pts',(28.2412941831759,536.939953656133,-47.6382097796865)) ;
#51298 = CARTESIAN_POINT('Ctrl Pts',(28.1936375284346,536.872561707023,-47.6335914716711)) ;
#51299 = CARTESIAN_POINT('Ctrl Pts',(28.1769368227079,536.847818738453,-47.6319533520939)) ;
#51300 = CARTESIAN_POINT('Ctrl Pts',(28.1385328243379,536.788157366576,-47.6281454212355)) ;
#51301 = CARTESIAN_POINT('Ctrl Pts',(28.1173274645108,536.752936125062,-47.6260044508062)) ;
#51302 = CARTESIAN_POINT('Ctrl Pts',(28.043699593253,536.621900176307,-47.6183401545964)) ;
#51303 = CARTESIAN_POINT('Ctrl Pts',(27.9978773581579,536.522579550768,-47.6130954377196)) ;
#51304 = CARTESIAN_POINT('Ctrl Pts',(27.914113775103,536.294922003483,-47.601417465512)) ;
#51305 = CARTESIAN_POINT('Ctrl Pts',(27.8803609476191,536.165588216216,-47.5949920208164)) ;
#51306 = CARTESIAN_POINT('Ctrl Pts',(27.8500194767232,535.975175062434,-47.5851524228382)) ;
#51307 = CARTESIAN_POINT('Ctrl Pts',(27.8432162098397,535.916074775029,-47.5820513032532)) ;
#51308 = CARTESIAN_POINT('Ctrl Pts',(27.8350054810978,535.800971259178,-47.5758826170011)) ;
#51309 = CARTESIAN_POINT('Ctrl Pts',(27.8333057220121,535.745041214447,-47.5728266951823)) ;
#51310 = CARTESIAN_POINT('Ctrl Pts',(27.8352084047887,535.562791639009,-47.5626630893591)) ;
#51311 = CARTESIAN_POINT('Ctrl Pts',(27.8481740452597,535.436873093049,-47.5553003425646)) ;
#51312 = CARTESIAN_POINT('Ctrl Pts',(27.8934226483909,535.20745811273,-47.5415298922178)) ;
#51313 = CARTESIAN_POINT('Ctrl Pts',(27.9224812278494,535.103750171493,-47.5351707299196)) ;
#51314 = CARTESIAN_POINT('Ctrl Pts',(27.9674385603888,534.981221504937,-47.5277695608863)) ;
#51315 = CARTESIAN_POINT('Ctrl Pts',(27.9757135688146,534.95978701585,-47.5264795198703)) ;
#51316 = CARTESIAN_POINT('Ctrl Pts',(27.9913001477852,534.921345339113,-47.5241793117858)) ;
#51317 = CARTESIAN_POINT('Ctrl Pts',(27.9984852948278,534.904289734789,-47.5231636235137)) ;
#51318 = CARTESIAN_POINT('Ctrl Pts',(28.0059001157432,534.887332980459,-47.522160171753)) ;
#51319 = CARTESIAN_POINT('',(28.6659533919829,534.056441033381,-47.5234100306407)) ;
#51320 = CARTESIAN_POINT('Origin',(29.8885276254069,535.710565160562,-47.522160171753)) ;
#51321 = CARTESIAN_POINT('Ctrl Pts',(28.6670126483642,534.058324644366,-47.5246598895284)) ;
#51322 = CARTESIAN_POINT('Ctrl Pts',(28.6536810751985,534.068180785848,-47.5255549008763)) ;
#51323 = CARTESIAN_POINT('Ctrl Pts',(28.640468807915,534.07819827049,-47.5264390170894)) ;
#51324 = CARTESIAN_POINT('Ctrl Pts',(28.6099842628224,534.101898048799,-47.5284758797812)) ;
#51325 = CARTESIAN_POINT('Ctrl Pts',(28.5928077462511,534.115700567163,-47.5296212187846)) ;
#51326 = CARTESIAN_POINT('Ctrl Pts',(28.4802750207493,534.209146697694,-47.5371339803449)) ;
#51327 = CARTESIAN_POINT('Ctrl Pts',(28.3920809257021,534.297028599388,-47.5430782761334)) ;
#51328 = CARTESIAN_POINT('Ctrl Pts',(28.2370086491919,534.482445296616,-47.5547981044329)) ;
#51329 = CARTESIAN_POINT('Ctrl Pts',(28.1695245285968,534.578832731799,-47.5605465545282)) ;
#51330 = CARTESIAN_POINT('Ctrl Pts',(28.0840728699006,534.72631397182,-47.5693391362522)) ;
#51331 = CARTESIAN_POINT('Ctrl Pts',(28.0592849438008,534.773186954468,-47.5721304322513)) ;
#51332 = CARTESIAN_POINT('Ctrl Pts',(28.0134445313532,534.868628663493,-47.5778373464681)) ;
#51333 = CARTESIAN_POINT('Ctrl Pts',(27.9924011151873,534.917156561869,-47.5807504812757)) ;
#51334 = CARTESIAN_POINT('Ctrl Pts',(27.9334882784982,535.068789752369,-47.5899032425551)) ;
#51335 = CARTESIAN_POINT('Ctrl Pts',(27.9019958013547,535.174150679075,-47.5963435171337)) ;
#51336 = CARTESIAN_POINT('Ctrl Pts',(27.8589907377098,535.375562679116,-47.6086396102651)) ;
#51337 = CARTESIAN_POINT('Ctrl Pts',(27.8455367596986,535.47090865252,-47.6144504973346)) ;
#51338 = CARTESIAN_POINT('Ctrl Pts',(27.8359039934508,535.608291488259,-47.6225776598932)) ;
#51339 = CARTESIAN_POINT('Ctrl Pts',(27.834255557408,535.649817193532,-47.6250012461652)) ;
#51340 = CARTESIAN_POINT('Ctrl Pts',(27.8335450457281,535.725856249888,-47.6293469310298)) ;
#51341 = CARTESIAN_POINT('Ctrl Pts',(27.8340912333028,535.760351154407,-47.631283574115)) ;
#51342 = CARTESIAN_POINT('Ctrl Pts',(27.8367782705162,535.825827155142,-47.6348727041961)) ;
#51343 = CARTESIAN_POINT('Ctrl Pts',(27.8387532182284,535.8568036467,-47.6365319357389)) ;
#51344 = CARTESIAN_POINT('Ctrl Pts',(27.8476334616252,535.959416044123,-47.6419314961922)) ;
#51345 = CARTESIAN_POINT('Ctrl Pts',(27.8576001589336,536.0307388095,-47.6455294958112)) ;
#51346 = CARTESIAN_POINT('Ctrl Pts',(27.9027819236631,536.263939819916,-47.6571878545444)) ;
#51347 = CARTESIAN_POINT('Ctrl Pts',(27.953801714464,536.422075056185,-47.6649737327569)) ;
#51348 = CARTESIAN_POINT('Ctrl Pts',(28.048524016192,536.6270894273,-47.6764039246535)) ;
#51349 = CARTESIAN_POINT('Ctrl Pts',(28.0761957010942,536.680659016126,-47.6795203056941)) ;
#51350 = CARTESIAN_POINT('Ctrl Pts',(28.1309358672665,536.776090513973,-47.6853633150728)) ;
#51351 = CARTESIAN_POINT('Ctrl Pts',(28.1572495080626,536.818332529484,-47.6880608936032)) ;
#51352 = CARTESIAN_POINT('Ctrl Pts',(28.2252830102685,536.919195210623,-47.6947972782927)) ;
#51353 = CARTESIAN_POINT('Ctrl Pts',(28.2685956302042,536.976656720144,-47.6988948491933)) ;
#51354 = CARTESIAN_POINT('Ctrl Pts',(28.4105620069439,537.145759982907,-47.7117623876639)) ;
#51355 = CARTESIAN_POINT('Ctrl Pts',(28.5183981870897,537.249040178714,-47.7208335961535)) ;
#51356 = CARTESIAN_POINT('Ctrl Pts',(28.6364363648367,537.33975668942,-47.7296625859469)) ;
#51357 = CARTESIAN_POINT('Origin',(29.8885276254068,535.710565160562,-51.0680854522906)) ;
#51358 = CARTESIAN_POINT('',(28.6364362890749,537.339756631195,-48.4293659750649)) ;
#51359 = CARTESIAN_POINT('',(28.6364362059859,537.339756567338,-48.3712578505663)) ;
#51360 = CARTESIAN_POINT('',(28.6364362890686,537.33975663119,-51.0680854522906)) ;
#51361 = CARTESIAN_POINT('',(31.9432771143099,535.709988359856,-47.9195437309321)) ;
#51362 = CARTESIAN_POINT('Ctrl Pts',(28.6364362059859,537.339756567338,-48.3712578505663)) ;
#51363 = CARTESIAN_POINT('Ctrl Pts',(28.6109373565783,537.320159796562,-48.3696379689333)) ;
#51364 = CARTESIAN_POINT('Ctrl Pts',(28.5858931562955,537.299960229751,-48.3679995024793)) ;
#51365 = CARTESIAN_POINT('Ctrl Pts',(28.5209233590622,537.244989154561,-48.3636076747014)) ;
#51366 = CARTESIAN_POINT('Ctrl Pts',(28.4818601041241,537.209259333955,-48.3608192591648)) ;
#51367 = CARTESIAN_POINT('Ctrl Pts',(28.4064121405063,537.134698907347,-48.3550976484189)) ;
#51368 = CARTESIAN_POINT('Ctrl Pts',(28.370069686407,537.095883888854,-48.3521660506704)) ;
#51369 = CARTESIAN_POINT('Ctrl Pts',(28.2294668051104,536.933527814266,-48.3400650873756)) ;
#51370 = CARTESIAN_POINT('Ctrl Pts',(28.1384583225618,536.799308462096,-48.3303582116747)) ;
#51371 = CARTESIAN_POINT('Ctrl Pts',(28.0340965091599,536.597888948285,-48.3167281960818)) ;
#51372 = CARTESIAN_POINT('Ctrl Pts',(28.0068447712792,536.538531741233,-48.3128227017384)) ;
#51373 = CARTESIAN_POINT('Ctrl Pts',(27.9652482588921,536.435215982338,-48.3063124780048)) ;
#51374 = CARTESIAN_POINT('Ctrl Pts',(27.9494749449593,536.391885701308,-48.3036649114146)) ;
#51375 = CARTESIAN_POINT('Ctrl Pts',(27.9261319140714,536.32035984946,-48.2994690889924)) ;
#51376 = CARTESIAN_POINT('Ctrl Pts',(27.9176826683432,536.292473133652,-48.297877310712)) ;
#51377 = CARTESIAN_POINT('Ctrl Pts',(27.897985545229,536.222102142919,-48.2939698362875)) ;
#51378 = CARTESIAN_POINT('Ctrl Pts',(27.8875022599321,536.179421104986,-48.2916936989802)) ;
#51379 = CARTESIAN_POINT('Ctrl Pts',(27.8488082412559,535.99678238639,-48.2822248553158)) ;
#51380 = CARTESIAN_POINT('Ctrl Pts',(27.8338529795646,535.854418611201,-48.2754888178683)) ;
#51381 = CARTESIAN_POINT('Ctrl Pts',(27.8337277627725,535.616273478408,-48.2638635308259)) ;
#51382 = CARTESIAN_POINT('Ctrl Pts',(27.8403176878507,535.521021106146,-48.2591232807637)) ;
#51383 = CARTESIAN_POINT('Ctrl Pts',(27.8606540207356,535.375292854597,-48.2514929143581)) ;
#51384 = CARTESIAN_POINT('Ctrl Pts',(27.8697462887423,535.324300818853,-48.2487516402753)) ;
#51385 = CARTESIAN_POINT('Ctrl Pts',(27.8924007465118,535.220181739395,-48.2429801555364)) ;
#51386 = CARTESIAN_POINT('Ctrl Pts',(27.9061824106991,535.167145387741,-48.2399446718402)) ;
#51387 = CARTESIAN_POINT('Ctrl Pts',(27.9415050553485,535.050569173866,-48.2330478030471)) ;
#51388 = CARTESIAN_POINT('Ctrl Pts',(27.9640711615652,534.987407076322,-48.2291571791792)) ;
#51389 = CARTESIAN_POINT('Ctrl Pts',(28.0448067054993,534.792139840619,-48.2166811149391)) ;
#51390 = CARTESIAN_POINT('Ctrl Pts',(28.1138158620912,534.66499969055,-48.2078571390363)) ;
#51391 = CARTESIAN_POINT('Ctrl Pts',(28.2243861453056,534.504241605859,-48.196381660404)) ;
#51392 = CARTESIAN_POINT('Ctrl Pts',(28.2547511106737,534.463425038424,-48.1934408918052)) ;
#51393 = CARTESIAN_POINT('Ctrl Pts',(28.3050630369977,534.400791710184,-48.1889367908077)) ;
#51394 = CARTESIAN_POINT('Ctrl Pts',(28.3240176395631,534.378208054442,-48.1873158913631)) ;
#51395 = CARTESIAN_POINT('Ctrl Pts',(28.3697977513185,534.325987975007,-48.1835821376272)) ;
#51396 = CARTESIAN_POINT('Ctrl Pts',(28.397013332639,534.29671228002,-48.181495871264)) ;
#51397 = CARTESIAN_POINT('Ctrl Pts',(28.5028096550975,534.189365137898,-48.1737896786604)) ;
#51398 = CARTESIAN_POINT('Ctrl Pts',(28.5868088374752,534.116891445342,-48.1684616328046)) ;
#51399 = CARTESIAN_POINT('Ctrl Pts',(28.7789323167666,533.976503336049,-48.156943450731)) ;
#51400 = CARTESIAN_POINT('Ctrl Pts',(28.8883571196168,533.911168768337,-48.1507570506228)) ;
#51401 = CARTESIAN_POINT('Ctrl Pts',(29.0511683329638,533.833422846335,-48.1414566686948)) ;
#51402 = CARTESIAN_POINT('Ctrl Pts',(29.1000976247429,533.812352502543,-48.1386537063286)) ;
#51403 = CARTESIAN_POINT('Ctrl Pts',(29.1991013448848,533.774207278837,-48.1329360761211)) ;
#51404 = CARTESIAN_POINT('Ctrl Pts',(29.2491263254306,533.757118031754,-48.1300246034284)) ;
#51405 = CARTESIAN_POINT('Ctrl Pts',(29.41057820935,533.708830106848,-48.120540071454)) ;
#51406 = CARTESIAN_POINT('Ctrl Pts',(29.5239917132856,533.685105683524,-48.1137327182557)) ;
#51407 = CARTESIAN_POINT('Ctrl Pts',(29.7727717963409,533.654642022534,-48.0987142656839)) ;
#51408 = CARTESIAN_POINT('Ctrl Pts',(29.9080539638011,533.651477732356,-48.0904915867883)) ;
#51409 = CARTESIAN_POINT('Ctrl Pts',(30.0778754093109,533.664253544935,-48.0807259281393)) ;
#51410 = CARTESIAN_POINT('Ctrl Pts',(30.1130065495387,533.667808845587,-48.0787376010803)) ;
#51411 = CARTESIAN_POINT('Ctrl Pts',(30.1784829863121,533.676144896028,-48.0751135142922)) ;
#51412 = CARTESIAN_POINT('Ctrl Pts',(30.2088443519621,533.680703792574,-48.0734680958025)) ;
#51413 = CARTESIAN_POINT('Ctrl Pts',(30.3049223018832,533.697339775831,-48.0683440146239)) ;
#51414 = CARTESIAN_POINT('Ctrl Pts',(30.3701623005118,533.711943004209,-48.0649864858338)) ;
#51415 = CARTESIAN_POINT('Ctrl Pts',(30.5659881420948,533.765925033592,-48.0549772917546)) ;
#51416 = CARTESIAN_POINT('Ctrl Pts',(30.6934660938249,533.815135456908,-48.0485353932678)) ;
#51417 = CARTESIAN_POINT('Ctrl Pts',(30.8834635381441,533.911131694173,-48.0380034610122)) ;
#51418 = CARTESIAN_POINT('Ctrl Pts',(30.9498039733512,533.949443590365,-48.0341342628143)) ;
#51419 = CARTESIAN_POINT('Ctrl Pts',(31.0557736414362,534.018807172911,-48.0275105421192)) ;
#51420 = CARTESIAN_POINT('Ctrl Pts',(31.0966778689256,534.047772108312,-48.0248356681508)) ;
#51421 = CARTESIAN_POINT('Ctrl Pts',(31.1827523776767,534.113576633226,-48.0189228758712)) ;
#51422 = CARTESIAN_POINT('Ctrl Pts',(31.2274954869947,534.150900404863,-48.015666532343)) ;
#51423 = CARTESIAN_POINT('Ctrl Pts',(31.3199694784192,534.234955234246,-48.0085243131655)) ;
#51424 = CARTESIAN_POINT('Ctrl Pts',(31.3671293792817,534.282214335788,-48.0046196854311)) ;
#51425 = CARTESIAN_POINT('Ctrl Pts',(31.5042084026115,534.433657704003,-47.9924851855872)) ;
#51426 = CARTESIAN_POINT('Ctrl Pts',(31.5860366787711,534.544641150565,-47.9840709416786)) ;
#51427 = CARTESIAN_POINT('Ctrl Pts',(31.6811007971023,534.705044609478,-47.9731237842977)) ;
#51428 = CARTESIAN_POINT('Ctrl Pts',(31.704530820794,534.748004361622,-47.9703015186387)) ;
#51429 = CARTESIAN_POINT('Ctrl Pts',(31.7395079098674,534.81796896631,-47.9659248578064)) ;
#51430 = CARTESIAN_POINT('Ctrl Pts',(31.7520469900934,534.844452099457,-47.9643183313891)) ;
#51431 = CARTESIAN_POINT('Ctrl Pts',(31.7812462894337,534.909695373233,-47.9604830276036)) ;
#51432 = CARTESIAN_POINT('Ctrl Pts',(31.7972869857427,534.948715727084,-47.9582877085315)) ;
#51433 = CARTESIAN_POINT('Ctrl Pts',(31.8319311008321,535.0409702687,-47.9532642090832)) ;
#51434 = CARTESIAN_POINT('Ctrl Pts',(31.8495675686885,535.094531569758,-47.9504733186191)) ;
#51435 = CARTESIAN_POINT('Ctrl Pts',(31.905219379795,535.290314283257,-47.9405093302048)) ;
#51436 = CARTESIAN_POINT('Ctrl Pts',(31.9301326190769,535.435783171807,-47.9335159171135)) ;
#51437 = CARTESIAN_POINT('Ctrl Pts',(31.9419369878692,535.625057469517,-47.9239369811701)) ;
#51438 = CARTESIAN_POINT('Ctrl Pts',(31.9432655974392,535.667518055835,-47.9217603139583)) ;
#51439 = CARTESIAN_POINT('Ctrl Pts',(31.9432775441096,535.709987153938,-47.919544539831)) ;
#51440 = CARTESIAN_POINT('Ctrl Pts',(31.9432775444593,535.709988398555,-47.9195444748946)) ;
#51441 = CARTESIAN_POINT('Ctrl Pts',(31.9432897614835,535.753512294332,-47.9172736671991)) ;
#51442 = CARTESIAN_POINT('Ctrl Pts',(31.9419190958385,535.79702374984,-47.9149628739012)) ;
#51443 = CARTESIAN_POINT('Ctrl Pts',(31.9358760518337,535.892426708692,-47.9097903438074)) ;
#51444 = CARTESIAN_POINT('Ctrl Pts',(31.930610071471,535.944248248271,-47.9069113174683)) ;
#51445 = CARTESIAN_POINT('Ctrl Pts',(31.9006628291596,536.157882650572,-47.894734617352)) ;
#51446 = CARTESIAN_POINT('Ctrl Pts',(31.858664665141,536.316638422322,-47.8848850330862)) ;
#51447 = CARTESIAN_POINT('Ctrl Pts',(31.7641216900513,536.554795412575,-47.8694839341399)) ;
#51448 = CARTESIAN_POINT('Ctrl Pts',(31.7241586760957,536.638487194049,-47.8639549100924)) ;
#51449 = CARTESIAN_POINT('Ctrl Pts',(31.6627136730293,536.747541295564,-47.8568315313557)) ;
#51450 = CARTESIAN_POINT('Ctrl Pts',(31.6460742161577,536.775499891421,-47.855013526813)) ;
#51451 = CARTESIAN_POINT('Ctrl Pts',(31.6109596809507,536.831434589283,-47.8514118218475)) ;
#51452 = CARTESIAN_POINT('Ctrl Pts',(31.5924501733249,536.859377025864,-47.8496305838173)) ;
#51453 = CARTESIAN_POINT('Ctrl Pts',(31.4990206132572,536.99319105263,-47.8411255546595)) ;
#51454 = CARTESIAN_POINT('Ctrl Pts',(31.4148682444253,537.092270037291,-47.8348933711343)) ;
#51455 = CARTESIAN_POINT('Ctrl Pts',(31.2359450420417,537.26647824529,-47.8227593885476)) ;
#51456 = CARTESIAN_POINT('Ctrl Pts',(31.1427982617474,537.342496847014,-47.8168876740319)) ;
#51457 = CARTESIAN_POINT('Ctrl Pts',(30.9991748428906,537.44011428871,-47.8079246422935)) ;
#51458 = CARTESIAN_POINT('Ctrl Pts',(30.9536300446027,537.468528062422,-47.8050970577741)) ;
#51459 = CARTESIAN_POINT('Ctrl Pts',(30.8605190212433,537.521669230653,-47.7993132744161)) ;
#51460 = CARTESIAN_POINT('Ctrl Pts',(30.8129937074386,537.546382942972,-47.7963596086639)) ;
#51461 = CARTESIAN_POINT('Ctrl Pts',(30.6626442170341,537.617246945069,-47.7869931032003)) ;
#51462 = CARTESIAN_POINT('Ctrl Pts',(30.5569627822929,537.656812971335,-47.7803653748098)) ;
#51463 = CARTESIAN_POINT('Ctrl Pts',(30.3562777350725,537.713665690896,-47.7678730689376)) ;
#51464 = CARTESIAN_POINT('Ctrl Pts',(30.2622527716955,537.733318666073,-47.7620602555263)) ;
#51465 = CARTESIAN_POINT('Ctrl Pts',(30.1107729669971,537.754054344038,-47.7530165131444)) ;
#51466 = CARTESIAN_POINT('Ctrl Pts',(30.05404613902,537.759429651115,-47.7497018429617)) ;
#51467 = CARTESIAN_POINT('Ctrl Pts',(29.9677666229353,537.763997759885,-47.744839498185)) ;
#51468 = CARTESIAN_POINT('Ctrl Pts',(29.9383351986624,537.764922437003,-47.7432125918351)) ;
#51469 = CARTESIAN_POINT('Ctrl Pts',(29.8744250774901,537.765555839649,-47.7397629580682)) ;
#51470 = CARTESIAN_POINT('Ctrl Pts',(29.839953758065,537.765030169449,-47.7379531173712)) ;
#51471 = CARTESIAN_POINT('Ctrl Pts',(29.6927721689412,537.759078744344,-47.7303812126777)) ;
#51472 = CARTESIAN_POINT('Ctrl Pts',(29.5805894497075,537.74524140175,-47.724993027963)) ;
#51473 = CARTESIAN_POINT('Ctrl Pts',(29.3347550937227,537.694108620168,-47.7130131154768)) ;
#51474 = CARTESIAN_POINT('Ctrl Pts',(29.2026079582314,537.652373390694,-47.7064367229642)) ;
#51475 = CARTESIAN_POINT('Ctrl Pts',(29.0246296991013,537.575709820794,-47.6965920527537)) ;
#51476 = CARTESIAN_POINT('Ctrl Pts',(28.9745204955043,537.551672004371,-47.6937062239928)) ;
#51477 = CARTESIAN_POINT('Ctrl Pts',(28.8814101810037,537.502267568968,-47.6880896084753)) ;
#51478 = CARTESIAN_POINT('Ctrl Pts',(28.8382389188391,537.477306815434,-47.6853753235415)) ;
#51479 = CARTESIAN_POINT('Ctrl Pts',(28.7410910438642,537.416318150144,-47.6789977661128)) ;
#51480 = CARTESIAN_POINT('Ctrl Pts',(28.6878377483695,537.379260473703,-47.6752982193288)) ;
#51481 = CARTESIAN_POINT('Ctrl Pts',(28.6364362717721,537.339756617897,-47.6715263025693)) ;
#51482 = CARTESIAN_POINT('Ctrl Pts',(28.6364363648367,537.33975668942,-47.7296625859469)) ;
#51483 = CARTESIAN_POINT('Ctrl Pts',(28.6660459719102,537.362512718769,-47.7318773178551)) ;
#51484 = CARTESIAN_POINT('Ctrl Pts',(28.6962636054984,537.384452512989,-47.734071696501)) ;
#51485 = CARTESIAN_POINT('Ctrl Pts',(28.7490501031617,537.420623168944,-47.7377734537237)) ;
#51486 = CARTESIAN_POINT('Ctrl Pts',(28.7713202615108,537.435255059537,-47.7392968165599)) ;
#51487 = CARTESIAN_POINT('Ctrl Pts',(28.8165336432896,537.463717658096,-47.7423038814074)) ;
#51488 = CARTESIAN_POINT('Ctrl Pts',(28.8394763173039,537.477541783534,-47.7437870181451)) ;
#51489 = CARTESIAN_POINT('Ctrl Pts',(28.8925447807788,537.508119992424,-47.747109858126)) ;
#51490 = CARTESIAN_POINT('Ctrl Pts',(28.9228347712996,537.52457255355,-47.7489307975608)) ;
#51491 = CARTESIAN_POINT('Ctrl Pts',(29.0795026035766,537.604632314948,-47.7580411470102)) ;
#51492 = CARTESIAN_POINT('Ctrl Pts',(29.2118042502731,537.65583276028,-47.7647513513814)) ;
#51493 = CARTESIAN_POINT('Ctrl Pts',(29.4230576751126,537.713396723879,-47.7753602418018)) ;
#51494 = CARTESIAN_POINT('Ctrl Pts',(29.4988744684411,537.72951686742,-47.7791437532152)) ;
#51495 = CARTESIAN_POINT('Ctrl Pts',(29.6380035302706,537.750968418156,-47.7862229273434)) ;
#51496 = CARTESIAN_POINT('Ctrl Pts',(29.700998013372,537.757719131493,-47.7894772513634)) ;
#51497 = CARTESIAN_POINT('Ctrl Pts',(29.8133813905988,537.764531640296,-47.7954297810772)) ;
#51498 = CARTESIAN_POINT('Ctrl Pts',(29.8626506906498,537.765742781107,-47.7980888454819)) ;
#51499 = CARTESIAN_POINT('Ctrl Pts',(29.978040418492,537.764429421712,-47.8044504349252)) ;
#51500 = CARTESIAN_POINT('Ctrl Pts',(30.0440867152625,537.760484893908,-47.8081956368863)) ;
#51501 = CARTESIAN_POINT('Ctrl Pts',(30.2561079644868,537.737516726513,-47.8205492276318)) ;
#51502 = CARTESIAN_POINT('Ctrl Pts',(30.4002582688995,537.706002848547,-47.8294934326989)) ;
#51503 = CARTESIAN_POINT('Ctrl Pts',(30.6097949661098,537.635979283451,-47.8426982223909)) ;
#51504 = CARTESIAN_POINT('Ctrl Pts',(30.6784982833515,537.608826028134,-47.8470542292525)) ;
#51505 = CARTESIAN_POINT('Ctrl Pts',(30.7739258916887,537.565029800985,-47.8530060354114)) ;
#51506 = CARTESIAN_POINT('Ctrl Pts',(30.8019589495922,537.551383673851,-47.8547414012516)) ;
#51507 = CARTESIAN_POINT('Ctrl Pts',(30.8597879536473,537.521586582734,-47.8582773697266)) ;
#51508 = CARTESIAN_POINT('Ctrl Pts',(30.8895160489951,537.505326339535,-47.860071504798)) ;
#51509 = CARTESIAN_POINT('Ctrl Pts',(31.0443915833832,537.41556867621,-47.8693635898957)) ;
#51510 = CARTESIAN_POINT('Ctrl Pts',(31.161904253365,537.329694517413,-47.8762430399588)) ;
#51511 = CARTESIAN_POINT('Ctrl Pts',(31.3506788637338,537.158377277678,-47.88861378739)) ;
#51512 = CARTESIAN_POINT('Ctrl Pts',(31.4259151389213,537.078221051206,-47.89401157208)) ;
#51513 = CARTESIAN_POINT('Ctrl Pts',(31.5270596417343,536.951513786517,-47.9023868249005)) ;
#51514 = CARTESIAN_POINT('Ctrl Pts',(31.5581549586403,536.909349780766,-47.9051488721096)) ;
#51515 = CARTESIAN_POINT('Ctrl Pts',(31.6174540091543,536.822153538575,-47.9108405047916)) ;
#51516 = CARTESIAN_POINT('Ctrl Pts',(31.6455896826167,536.77712380655,-47.9137696934752)) ;
#51517 = CARTESIAN_POINT('Ctrl Pts',(31.732414537059,536.625388029269,-47.9236245451744)) ;
#51518 = CARTESIAN_POINT('Ctrl Pts',(31.7833610427512,536.514566987941,-47.9308155449626)) ;
#51519 = CARTESIAN_POINT('Ctrl Pts',(31.8617261896303,536.294517151395,-47.9448317156167)) ;
#51520 = CARTESIAN_POINT('Ctrl Pts',(31.8905889544197,536.186238106078,-47.9516112696373)) ;
#51521 = CARTESIAN_POINT('Ctrl Pts',(31.9179322861602,536.035006209979,-47.9605385585402)) ;
#51522 = CARTESIAN_POINT('Ctrl Pts',(31.9241136350263,535.993647084515,-47.962924360334)) ;
#51523 = CARTESIAN_POINT('Ctrl Pts',(31.9324460946066,535.92326133233,-47.966858419421)) ;
#51524 = CARTESIAN_POINT('Ctrl Pts',(31.9352500514238,535.89433081867,-47.9684373779893)) ;
#51525 = CARTESIAN_POINT('Ctrl Pts',(31.9410632027104,535.817378948874,-47.9725442344738)) ;
#51526 = CARTESIAN_POINT('Ctrl Pts',(31.9430014798801,535.7692963048,-47.975018867384)) ;
#51527 = CARTESIAN_POINT('Ctrl Pts',(31.943980337516,535.579936201775,-47.984555301875)) ;
#51528 = CARTESIAN_POINT('Ctrl Pts',(31.9301437139032,535.438979707353,-47.9912197198367)) ;
#51529 = CARTESIAN_POINT('Ctrl Pts',(31.8838428720012,535.211613933217,-48.0025773169541)) ;
#51530 = CARTESIAN_POINT('Ctrl Pts',(31.8598608655246,535.123983324473,-48.0071050777366)) ;
#51531 = CARTESIAN_POINT('Ctrl Pts',(31.8134105482822,534.989839354403,-48.014478168151)) ;
#51532 = CARTESIAN_POINT('Ctrl Pts',(31.7948523605926,534.942095689224,-48.0171929570401)) ;
#51533 = CARTESIAN_POINT('Ctrl Pts',(31.7527450622742,534.844710425386,-48.0229461371169)) ;
#51534 = CARTESIAN_POINT('Ctrl Pts',(31.7289499489372,534.795220458472,-48.0259915044107)) ;
#51535 = CARTESIAN_POINT('Ctrl Pts',(31.6290810709249,534.607187704454,-48.0380596045783)) ;
#51536 = CARTESIAN_POINT('Ctrl Pts',(31.539115539315,534.476663386456,-48.0475755529853)) ;
#51537 = CARTESIAN_POINT('Ctrl Pts',(31.3936804647077,534.310396722979,-48.0608417533435)) ;
#51538 = CARTESIAN_POINT('Ctrl Pts',(31.3500983344297,534.264961995106,-48.0646012090386)) ;
#51539 = CARTESIAN_POINT('Ctrl Pts',(31.2718645101486,534.190563627827,-48.0709042393895)) ;
#51540 = CARTESIAN_POINT('Ctrl Pts',(31.2382170198493,534.160608793194,-48.0734876321035)) ;
#51541 = CARTESIAN_POINT('Ctrl Pts',(31.181369745335,534.113256602909,-48.0776103992252)) ;
#51542 = CARTESIAN_POINT('Ctrl Pts',(31.1587417426899,534.095203995221,-48.0791904427315)) ;
#51543 = CARTESIAN_POINT('Ctrl Pts',(31.1006465377737,534.050831799082,-48.0830971593247)) ;
#51544 = CARTESIAN_POINT('Ctrl Pts',(31.0646999927773,534.025167222701,-48.0853831688788)) ;
#51545 = CARTESIAN_POINT('Ctrl Pts',(30.9151257349926,533.925494760977,-48.0944941962105)) ;
#51546 = CARTESIAN_POINT('Ctrl Pts',(30.7951276440468,533.861656871508,-48.1009140460509)) ;
#51547 = CARTESIAN_POINT('Ctrl Pts',(30.5773987270047,533.772159928521,-48.1123812269167)) ;
#51548 = CARTESIAN_POINT('Ctrl Pts',(30.4824549290364,533.740995184651,-48.1173244356803)) ;
#51549 = CARTESIAN_POINT('Ctrl Pts',(30.3353562124117,533.704318336775,-48.1251747936067)) ;
#51550 = CARTESIAN_POINT('Ctrl Pts',(30.2846301301824,533.693690285201,-48.1279135276775)) ;
#51551 = CARTESIAN_POINT('Ctrl Pts',(30.180547010276,533.675960998018,-48.1336238953026)) ;
#51552 = CARTESIAN_POINT('Ctrl Pts',(30.1272045696466,533.669016248177,-48.1365982345536)) ;
#51553 = CARTESIAN_POINT('Ctrl Pts',(29.9051259251516,533.648925918834,-48.149198132912)) ;
#51554 = CARTESIAN_POINT('Ctrl Pts',(29.735380185855,533.654559287559,-48.1594168093959)) ;
#51555 = CARTESIAN_POINT('Ctrl Pts',(29.4845561586807,533.694135330239,-48.1746470997079)) ;
#51556 = CARTESIAN_POINT('Ctrl Pts',(29.4017199246338,533.712515392963,-48.1796832363303)) ;
#51557 = CARTESIAN_POINT('Ctrl Pts',(29.2895396983399,533.744800099161,-48.1863171665115)) ;
#51558 = CARTESIAN_POINT('Ctrl Pts',(29.2590370330932,533.754354349092,-48.1881010093543)) ;
#51559 = CARTESIAN_POINT('Ctrl Pts',(29.1975154126042,533.775212832741,-48.1916402352516)) ;
#51560 = CARTESIAN_POINT('Ctrl Pts',(29.1665213127764,533.786560567338,-48.1933928627051)) ;
#51561 = CARTESIAN_POINT('Ctrl Pts',(29.0101605586639,533.848119372036,-48.202142122044)) ;
#51562 = CARTESIAN_POINT('Ctrl Pts',(28.8896773064733,533.909859961679,-48.2085926857946)) ;
#51563 = CARTESIAN_POINT('Ctrl Pts',(28.6750745216497,534.04804561447,-48.2209552361665)) ;
#51564 = CARTESIAN_POINT('Ctrl Pts',(28.579943276341,534.121841425235,-48.2268267184197)) ;
#51565 = CARTESIAN_POINT('Ctrl Pts',(28.4531105372464,534.239388859163,-48.2357482155519)) ;
#51566 = CARTESIAN_POINT('Ctrl Pts',(28.4158075464454,534.276732247989,-48.2385273902011)) ;
#51567 = CARTESIAN_POINT('Ctrl Pts',(28.3442113023573,534.35415048482,-48.2442128033654)) ;
#51568 = CARTESIAN_POINT('Ctrl Pts',(28.309941324366,534.394192021872,-48.2471167087464)) ;
#51569 = CARTESIAN_POINT('Ctrl Pts',(28.174983697265,534.564736134942,-48.2593607093954)) ;
#51570 = CARTESIAN_POINT('Ctrl Pts',(28.0886506241526,534.705785183858,-48.2692666928378)) ;
#51571 = CARTESIAN_POINT('Ctrl Pts',(27.9934576786508,534.9138173918,-48.283009016606)) ;
#51572 = CARTESIAN_POINT('Ctrl Pts',(27.9695507903834,534.973255351297,-48.2868371165224)) ;
#51573 = CARTESIAN_POINT('Ctrl Pts',(27.933466461241,535.076684624439,-48.2932363467774)) ;
#51574 = CARTESIAN_POINT('Ctrl Pts',(27.919905782499,535.120143827584,-48.2958487176514)) ;
#51575 = CARTESIAN_POINT('Ctrl Pts',(27.9000978580295,535.191929603653,-48.3000003258659)) ;
#51576 = CARTESIAN_POINT('Ctrl Pts',(27.8929878337704,535.219997167993,-48.3015816682146)) ;
#51577 = CARTESIAN_POINT('Ctrl Pts',(27.8766337334246,535.29081255544,-48.3054676855118)) ;
#51578 = CARTESIAN_POINT('Ctrl Pts',(27.8681568358877,535.3337207632,-48.3077330754487)) ;
#51579 = CARTESIAN_POINT('Ctrl Pts',(27.839073549619,535.51042548027,-48.3168174950013)) ;
#51580 = CARTESIAN_POINT('Ctrl Pts',(27.8303406821866,535.645835563483,-48.3232280107875)) ;
#51581 = CARTESIAN_POINT('Ctrl Pts',(27.8384461539867,535.881720685387,-48.3347206892156)) ;
#51582 = CARTESIAN_POINT('Ctrl Pts',(27.8492888562128,535.98191502232,-48.3397026946008)) ;
#51583 = CARTESIAN_POINT('Ctrl Pts',(27.87677739035,536.13193167462,-48.3475983376188)) ;
#51584 = CARTESIAN_POINT('Ctrl Pts',(27.888055826285,536.182582829214,-48.350339811795)) ;
#51585 = CARTESIAN_POINT('Ctrl Pts',(27.9148894365981,536.284704012378,-48.3560492903768)) ;
#51586 = CARTESIAN_POINT('Ctrl Pts',(27.9305719722151,536.336098541244,-48.3590196961411)) ;
#51587 = CARTESIAN_POINT('Ctrl Pts',(28.0041409314059,536.547180239176,-48.3716475431238)) ;
#51588 = CARTESIAN_POINT('Ctrl Pts',(28.0796920896114,536.699976212486,-48.3819036165961)) ;
#51589 = CARTESIAN_POINT('Ctrl Pts',(28.2196062326397,536.912155696837,-48.3971448334858)) ;
#51590 = CARTESIAN_POINT('Ctrl Pts',(28.2703602318251,536.979681034504,-48.402157057251)) ;
#51591 = CARTESIAN_POINT('Ctrl Pts',(28.3458550789782,537.068202567596,-48.408767890696)) ;
#51592 = CARTESIAN_POINT('Ctrl Pts',(28.3671485886185,537.092022388839,-48.4105507195528)) ;
#51593 = CARTESIAN_POINT('Ctrl Pts',(28.4115793806403,537.139450430223,-48.4140910037266)) ;
#51594 = CARTESIAN_POINT('Ctrl Pts',(28.434747921837,537.163016221716,-48.4158455698408)) ;
#51595 = CARTESIAN_POINT('Ctrl Pts',(28.5148079957574,537.240612940701,-48.4216497193311)) ;
#51596 = CARTESIAN_POINT('Ctrl Pts',(28.5742250409781,537.291945084075,-48.4255364649937)) ;
#51597 = CARTESIAN_POINT('Ctrl Pts',(28.6364362890811,537.3397566312,-48.4293659750649)) ;
#51598 = CARTESIAN_POINT('Origin',(29.8885276254068,535.710565160562,-51.0680854522906)) ;
#51599 = CARTESIAN_POINT('',(28.6368808924516,537.339275726356,-49.1271194481244)) ;
#51600 = CARTESIAN_POINT('',(28.6364362889498,537.339756631099,-49.0682055192064)) ;
#51601 = CARTESIAN_POINT('',(28.6364362890686,537.33975663119,-51.0680854522906)) ;
#51602 = CARTESIAN_POINT('',(31.943277537214,535.709963140231,-49.3762357707893)) ;
#51603 = CARTESIAN_POINT('Ctrl Pts',(31.9427353807384,535.709924613476,-49.3752968619707)) ;
#51604 = CARTESIAN_POINT('Ctrl Pts',(31.9426199546863,535.780830487742,-49.3712221291559)) ;
#51605 = CARTESIAN_POINT('Ctrl Pts',(31.9388610049111,535.851778410132,-49.3672024739762)) ;
#51606 = CARTESIAN_POINT('Ctrl Pts',(31.9314849812218,535.922371758857,-49.3632673200693)) ;
#51607 = CARTESIAN_POINT('Ctrl Pts',(31.9241108995947,535.992946520782,-49.3593332022646)) ;
#51608 = CARTESIAN_POINT('Ctrl Pts',(31.913121663627,536.063166873767,-49.3554835715093)) ;
#51609 = CARTESIAN_POINT('Ctrl Pts',(31.8985781724063,536.132640674243,-49.3517232456352)) ;
#51610 = CARTESIAN_POINT('Ctrl Pts',(31.8840335242281,536.202120001468,-49.3479626206213)) ;
#51611 = CARTESIAN_POINT('Ctrl Pts',(31.865933961411,536.270852586537,-49.3442912423131)) ;
#51612 = CARTESIAN_POINT('Ctrl Pts',(31.8443754859495,536.338451052282,-49.3406896571612)) ;
#51613 = CARTESIAN_POINT('Ctrl Pts',(31.8227923040914,536.406126987072,-49.3370839445287)) ;
#51614 = CARTESIAN_POINT('Ctrl Pts',(31.7977420713674,536.472666069719,-49.3335479997593)) ;
#51615 = CARTESIAN_POINT('Ctrl Pts',(31.7693585376145,536.537685961532,-49.3300398756539)) ;
#51616 = CARTESIAN_POINT('Ctrl Pts',(31.7409575727637,536.602745783825,-49.3265295971143)) ;
#51617 = CARTESIAN_POINT('Ctrl Pts',(31.7092188973427,536.666284313147,-49.3230468284672)) ;
#51618 = CARTESIAN_POINT('Ctrl Pts',(31.6743178484239,536.727927574273,-49.3195310381818)) ;
#51619 = CARTESIAN_POINT('Ctrl Pts',(31.6414276231321,536.78601925945,-49.3162178101228)) ;
#51620 = CARTESIAN_POINT('Ctrl Pts',(31.605728525571,536.842427954752,-49.3128747645005)) ;
#51621 = CARTESIAN_POINT('Ctrl Pts',(31.5674065174128,536.896850717022,-49.3094413669133)) ;
#51622 = CARTESIAN_POINT('Ctrl Pts',(31.5649871231534,536.900286604778,-49.3092246052452)) ;
#51623 = CARTESIAN_POINT('Ctrl Pts',(31.5625572732845,536.903714594207,-49.3090074834512)) ;
#51624 = CARTESIAN_POINT('Ctrl Pts',(31.5601170139572,536.907134616038,-49.3087899862986)) ;
#51625 = CARTESIAN_POINT('Ctrl Pts',(31.5338502905483,536.943947411504,-49.3064488672681)) ;
#51626 = CARTESIAN_POINT('Ctrl Pts',(31.5063786491928,536.97983508785,-49.3040640238)) ;
#51627 = CARTESIAN_POINT('Ctrl Pts',(31.4777715977333,537.014707694267,-49.3016158100282)) ;
#51628 = CARTESIAN_POINT('Ctrl Pts',(31.4777498830234,537.014734164962,-49.3016139516664)) ;
#51629 = CARTESIAN_POINT('Ctrl Pts',(31.4777281676594,537.014760635073,-49.301612093268)) ;
#51630 = CARTESIAN_POINT('Ctrl Pts',(31.4777064516412,537.014787104599,-49.3016102348332)) ;
#51631 = CARTESIAN_POINT('Ctrl Pts',(31.4368869866815,537.064541709808,-49.2981169463691)) ;
#51632 = CARTESIAN_POINT('Ctrl Pts',(31.3935987794868,537.112410718029,-49.294485333284)) ;
#51633 = CARTESIAN_POINT('Ctrl Pts',(31.3480628704188,537.158164346995,-49.2907804710927)) ;
#51634 = CARTESIAN_POINT('Ctrl Pts',(31.3434468252196,537.162802462795,-49.2904049035092)) ;
#51635 = CARTESIAN_POINT('Ctrl Pts',(31.3388077255577,537.167418832085,-49.290028583204)) ;
#51636 = CARTESIAN_POINT('Ctrl Pts',(31.3341458310762,537.172013210475,-49.2896515779672)) ;
#51637 = CARTESIAN_POINT('Ctrl Pts',(31.2835734989649,537.221853126567,-49.2855618170084)) ;
#51638 = CARTESIAN_POINT('Ctrl Pts',(31.2303129280193,537.269106762271,-49.2813920692415)) ;
#51639 = CARTESIAN_POINT('Ctrl Pts',(31.1746835629705,537.313510240679,-49.2772166934141)) ;
#51640 = CARTESIAN_POINT('Ctrl Pts',(31.1191229434999,537.357858846219,-49.2730464774268)) ;
#51641 = CARTESIAN_POINT('Ctrl Pts',(31.0611995686604,537.399364666718,-49.2688710009134)) ;
#51642 = CARTESIAN_POINT('Ctrl Pts',(31.0012491055257,537.437801073993,-49.2647450006894)) ;
#51643 = CARTESIAN_POINT('Ctrl Pts',(30.9413387091166,537.476211793044,-49.2606217579973)) ;
#51644 = CARTESIAN_POINT('Ctrl Pts',(30.8794039979015,537.511557362762,-49.2565480944349)) ;
#51645 = CARTESIAN_POINT('Ctrl Pts',(30.815795572546,537.543644156167,-49.2525554549385)) ;
#51646 = CARTESIAN_POINT('Ctrl Pts',(30.7522082799242,537.575720289322,-49.2485641419233)) ;
#51647 = CARTESIAN_POINT('Ctrl Pts',(30.686948403443,537.604539826175,-49.2446538395684)) ;
#51648 = CARTESIAN_POINT('Ctrl Pts',(30.6203812176618,537.629940570116,-49.2408312549402)) ;
#51649 = CARTESIAN_POINT('Ctrl Pts',(30.5538137750593,537.655341412055,-49.2370086555642)) ;
#51650 = CARTESIAN_POINT('Ctrl Pts',(30.4859390124216,537.677323325623,-49.2332737099885)) ;
#51651 = CARTESIAN_POINT('Ctrl Pts',(30.4171371153688,537.695756075853,-49.2296085996251)) ;
#51652 = CARTESIAN_POINT('Ctrl Pts',(30.3482663065826,537.71420728826,-49.2259398183002)) ;
#51653 = CARTESIAN_POINT('Ctrl Pts',(30.2784664955002,537.729101984314,-49.222340833987)) ;
#51654 = CARTESIAN_POINT('Ctrl Pts',(30.2081340439748,537.740344173802,-49.2187709892463)) ;
#51655 = CARTESIAN_POINT('Ctrl Pts',(30.1377637201469,537.751592416934,-49.2151992222317)) ;
#51656 = CARTESIAN_POINT('Ctrl Pts',(30.0668602002263,537.759183828206,-49.2116562888183)) ;
#51657 = CARTESIAN_POINT('Ctrl Pts',(29.9958355179518,537.763061612476,-49.2080824899406)) ;
#51658 = CARTESIAN_POINT('Ctrl Pts',(29.9285703348079,537.766734136743,-49.204697860424)) ;
#51659 = CARTESIAN_POINT('Ctrl Pts',(29.8611961404133,537.76707549024,-49.2012850560164)) ;
#51660 = CARTESIAN_POINT('Ctrl Pts',(29.7940761550714,537.764076262402,-49.1977828519104)) ;
#51661 = CARTESIAN_POINT('Ctrl Pts',(29.7902028026375,537.763903183305,-49.1975807471166)) ;
#51662 = CARTESIAN_POINT('Ctrl Pts',(29.7863302840043,537.763718986147,-49.1973783446039)) ;
#51663 = CARTESIAN_POINT('Ctrl Pts',(29.7824586642199,537.763523671486,-49.1971756326062)) ;
#51664 = CARTESIAN_POINT('Ctrl Pts',(29.7394170961748,537.761352319517,-49.1949220429648)) ;
#51665 = CARTESIAN_POINT('Ctrl Pts',(29.6964886714984,537.757806947959,-49.1926299836999)) ;
#51666 = CARTESIAN_POINT('Ctrl Pts',(29.6537708961817,537.752895156457,-49.1902826080212)) ;
#51667 = CARTESIAN_POINT('Ctrl Pts',(29.6537386176986,537.752891445,-49.1902808342929)) ;
#51668 = CARTESIAN_POINT('Ctrl Pts',(29.6537063393353,537.752887732763,-49.1902790605331)) ;
#51669 = CARTESIAN_POINT('Ctrl Pts',(29.6536740610918,537.752884019747,-49.1902772867416)) ;
#51670 = CARTESIAN_POINT('Ctrl Pts',(29.5893740015573,537.745487483915,-49.1867437953227)) ;
#51671 = CARTESIAN_POINT('Ctrl Pts',(29.5253306330089,537.734962903227,-49.1830762567584)) ;
#51672 = CARTESIAN_POINT('Ctrl Pts',(29.4618603629612,537.72137346018,-49.1793396131153)) ;
#51673 = CARTESIAN_POINT('Ctrl Pts',(29.4556644772076,537.720046876309,-49.1789748467908)) ;
#51674 = CARTESIAN_POINT('Ctrl Pts',(29.449474081227,537.718691115574,-49.1786094219356)) ;
#51675 = CARTESIAN_POINT('Ctrl Pts',(29.4432894873336,537.717306256261,-49.178243398962)) ;
#51676 = CARTESIAN_POINT('Ctrl Pts',(29.3742159037184,537.701839243031,-49.1741554153508)) ;
#51677 = CARTESIAN_POINT('Ctrl Pts',(29.3058622453113,537.682738637951,-49.1699935618367)) ;
#51678 = CARTESIAN_POINT('Ctrl Pts',(29.2386160666126,537.660129319953,-49.1658294303658)) ;
#51679 = CARTESIAN_POINT('Ctrl Pts',(29.23504794841,537.658929657449,-49.1656084793231)) ;
#51680 = CARTESIAN_POINT('Ctrl Pts',(29.2314829579231,537.65772012384,-49.165387521867)) ;
#51681 = CARTESIAN_POINT('Ctrl Pts',(29.2279211562329,537.656500740354,-49.1651665686925)) ;
#51682 = CARTESIAN_POINT('Ctrl Pts',(29.1605197194827,537.633425845665,-49.1609853809922)) ;
#51683 = CARTESIAN_POINT('Ctrl Pts',(29.0942559948543,537.606821413716,-49.1568059334518)) ;
#51684 = CARTESIAN_POINT('Ctrl Pts',(29.0295020143273,537.576849542796,-49.1526806630055)) ;
#51685 = CARTESIAN_POINT('Ctrl Pts',(28.9647908786836,537.546897502956,-49.1485581220707)) ;
#51686 = CARTESIAN_POINT('Ctrl Pts',(28.9015873956338,537.51358261161,-49.1444898445045)) ;
#51687 = CARTESIAN_POINT('Ctrl Pts',(28.8402440473705,537.477097248407,-49.1405048762514)) ;
#51688 = CARTESIAN_POINT('Ctrl Pts',(28.7789172502295,537.440621729364,-49.1365209831874)) ;
#51689 = CARTESIAN_POINT('Ctrl Pts',(28.7194495875471,537.400977465339,-49.1326203867606)) ;
#51690 = CARTESIAN_POINT('Ctrl Pts',(28.6621751277739,537.358386212482,-49.1288074354721)) ;
#51691 = CARTESIAN_POINT('Ctrl Pts',(28.6536953228304,537.352080338661,-49.1282429066522)) ;
#51692 = CARTESIAN_POINT('Ctrl Pts',(28.6452635611451,537.345709918296,-49.1276802548137)) ;
#51693 = CARTESIAN_POINT('Ctrl Pts',(28.6368808924516,537.339275726356,-49.1271194481244)) ;
#51694 = CARTESIAN_POINT('',(30.4186978425951,533.72539083489,-49.522160171753)) ;
#51695 = CARTESIAN_POINT('Ctrl Pts',(30.4186978425951,533.72539083489,-49.522160171753)) ;
#51696 = CARTESIAN_POINT('Ctrl Pts',(30.4888567936994,533.744127822299,-49.5182228345589)) ;
#51697 = CARTESIAN_POINT('Ctrl Pts',(30.558087616928,533.766605982304,-49.5142854973648)) ;
#51698 = CARTESIAN_POINT('Ctrl Pts',(30.6259762638657,533.792710351632,-49.5103481601707)) ;
#51699 = CARTESIAN_POINT('Ctrl Pts',(30.6938110350337,533.818794004787,-49.506413947609)) ;
#51700 = CARTESIAN_POINT('Ctrl Pts',(30.7603053193206,533.848497980627,-49.5024797350474)) ;
#51701 = CARTESIAN_POINT('Ctrl Pts',(30.8250616606322,533.881657955873,-49.4985455224858)) ;
#51702 = CARTESIAN_POINT('Ctrl Pts',(30.8897993492147,533.91480837956,-49.4946124431537)) ;
#51703 = CARTESIAN_POINT('Ctrl Pts',(30.9527996772528,533.951412621011,-49.4906793638217)) ;
#51704 = CARTESIAN_POINT('Ctrl Pts',(31.013687583735,533.991259303341,-49.4867462844896)) ;
#51705 = CARTESIAN_POINT('Ctrl Pts',(31.074568968254,534.031101717522,-49.4828136264465)) ;
#51706 = CARTESIAN_POINT('Ctrl Pts',(31.1333379955336,534.074185630533,-49.4788809684033)) ;
#51707 = CARTESIAN_POINT('Ctrl Pts',(31.1896478347493,534.120255831111,-49.4749483103601)) ;
#51708 = CARTESIAN_POINT('Ctrl Pts',(31.2459675257825,534.166334092006,-49.4710149642697)) ;
#51709 = CARTESIAN_POINT('Ctrl Pts',(31.2998268175,534.215399387038,-49.4670816181793)) ;
#51710 = CARTESIAN_POINT('Ctrl Pts',(31.3509123698971,534.267156548428,-49.463148272089)) ;
#51711 = CARTESIAN_POINT('Ctrl Pts',(31.4020212719486,534.318937366444,-49.4592131281855)) ;
#51712 = CARTESIAN_POINT('Ctrl Pts',(31.4503535920648,534.373412168299,-49.4552779842821)) ;
#51713 = CARTESIAN_POINT('Ctrl Pts',(31.4956342011548,534.430250349007,-49.4513428403787)) ;
#51714 = CARTESIAN_POINT('Ctrl Pts',(31.5409821077165,534.487173004415,-49.44740184794)) ;
#51715 = CARTESIAN_POINT('Ctrl Pts',(31.5832689630283,534.546465688977,-49.4434608555014)) ;
#51716 = CARTESIAN_POINT('Ctrl Pts',(31.6222614450573,534.607766627239,-49.4395198630628)) ;
#51717 = CARTESIAN_POINT('Ctrl Pts',(31.6612865134216,534.669118795194,-49.4355755771047)) ;
#51718 = CARTESIAN_POINT('Ctrl Pts',(31.6970114993853,534.732482158629,-49.4316312911465)) ;
#51719 = CARTESIAN_POINT('Ctrl Pts',(31.7292490458786,534.797470305294,-49.4276870051883)) ;
#51720 = CARTESIAN_POINT('Ctrl Pts',(31.7615480685897,534.862582382776,-49.4237351975727)) ;
#51721 = CARTESIAN_POINT('Ctrl Pts',(31.7903461900897,534.929325007906,-49.419783389957)) ;
#51722 = CARTESIAN_POINT('Ctrl Pts',(31.8155043249335,534.997292167956,-49.4158315823414)) ;
#51723 = CARTESIAN_POINT('Ctrl Pts',(31.8258890467887,535.025347508973,-49.4142003635262)) ;
#51724 = CARTESIAN_POINT('Ctrl Pts',(31.8356541601606,535.053611326253,-49.4125691447109)) ;
#51725 = CARTESIAN_POINT('Ctrl Pts',(31.8447924034538,535.082054475949,-49.4109379258957)) ;
#51726 = CARTESIAN_POINT('Ctrl Pts',(31.8702884146574,535.161411836006,-49.4063867696335)) ;
#51727 = CARTESIAN_POINT('Ctrl Pts',(31.8909796284462,535.242409214064,-49.4018356133713)) ;
#51728 = CARTESIAN_POINT('Ctrl Pts',(31.906684111172,535.324505629577,-49.3972844571091)) ;
#51729 = CARTESIAN_POINT('Ctrl Pts',(31.9222193282413,535.405717195592,-49.3927823540036)) ;
#51730 = CARTESIAN_POINT('Ctrl Pts',(31.932874645567,535.488004119788,-49.3882802508982)) ;
#51731 = CARTESIAN_POINT('Ctrl Pts',(31.9385201320457,535.570821519473,-49.3837781477928)) ;
#51732 = CARTESIAN_POINT('Ctrl Pts',(31.9416727614126,535.617069538546,-49.381264022125)) ;
#51733 = CARTESIAN_POINT('Ctrl Pts',(31.9432639189038,535.663482614069,-49.3787498964571)) ;
#51734 = CARTESIAN_POINT('Ctrl Pts',(31.9432775372141,535.709963140231,-49.3762357707893)) ;
#51735 = CARTESIAN_POINT('',(29.3554672321407,533.72404407569,-49.5209785487821)) ;
#51736 = CARTESIAN_POINT('Origin',(29.8885276254068,535.710565160562,-49.522160171753)) ;
#51737 = CARTESIAN_POINT('',(31.9432771819323,535.711915145219,-49.3167693044577)) ;
#51738 = CARTESIAN_POINT('Ctrl Pts',(29.3560800705629,533.726000431499,-49.5197877449898)) ;
#51739 = CARTESIAN_POINT('Ctrl Pts',(29.3727232359274,533.721535163839,-49.5188564377852)) ;
#51740 = CARTESIAN_POINT('Ctrl Pts',(29.3894225027156,533.717279276791,-49.5179369715456)) ;
#51741 = CARTESIAN_POINT('Ctrl Pts',(29.4275700894734,533.708066669072,-49.5158664643182)) ;
#51742 = CARTESIAN_POINT('Ctrl Pts',(29.4490486950172,533.703243462867,-49.5147220435414)) ;
#51743 = CARTESIAN_POINT('Ctrl Pts',(29.5664110730149,533.678862888878,-49.5085644277625)) ;
#51744 = CARTESIAN_POINT('Ctrl Pts',(29.6635282606455,533.665827630833,-49.5038106332384)) ;
#51745 = CARTESIAN_POINT('Ctrl Pts',(29.8915725628636,533.651670337441,-49.4927393155173)) ;
#51746 = CARTESIAN_POINT('Ctrl Pts',(30.0224045088476,533.65602595308,-49.4864409899781)) ;
#51747 = CARTESIAN_POINT('Ctrl Pts',(30.2079858419884,533.680013778618,-49.4768874456396)) ;
#51748 = CARTESIAN_POINT('Ctrl Pts',(30.2637160955301,533.689569047045,-49.4739405330125)) ;
#51749 = CARTESIAN_POINT('Ctrl Pts',(30.3680315882367,533.711918078274,-49.4682378815688)) ;
#51750 = CARTESIAN_POINT('Ctrl Pts',(30.4166798891431,533.724219577228,-49.4655000002555)) ;
#51751 = CARTESIAN_POINT('Ctrl Pts',(30.5445911424325,533.761595219636,-49.4580750887874)) ;
#51752 = CARTESIAN_POINT('Ctrl Pts',(30.6228598065772,533.789717209359,-49.4532925867747)) ;
#51753 = CARTESIAN_POINT('Ctrl Pts',(30.8140677135829,533.871815859139,-49.4410475906918)) ;
#51754 = CARTESIAN_POINT('Ctrl Pts',(30.9241891067755,533.931513110172,-49.4334636245622)) ;
#51755 = CARTESIAN_POINT('Ctrl Pts',(31.0665555861296,534.026411614519,-49.4233144062885)) ;
#51756 = CARTESIAN_POINT('Ctrl Pts',(31.1040477223569,534.053267848236,-49.4206079819085)) ;
#51757 = CARTESIAN_POINT('Ctrl Pts',(31.1698936576313,534.103871969374,-49.4158347599524)) ;
#51758 = CARTESIAN_POINT('Ctrl Pts',(31.1985707888151,534.127167169066,-49.4137487080267)) ;
#51759 = CARTESIAN_POINT('Ctrl Pts',(31.2493004256202,534.170698534935,-49.4100692849863)) ;
#51760 = CARTESIAN_POINT('Ctrl Pts',(31.2715663529941,534.190665243779,-49.4084606671827)) ;
#51761 = CARTESIAN_POINT('Ctrl Pts',(31.3366761739484,534.251667683194,-49.4037553528811)) ;
#51762 = CARTESIAN_POINT('Ctrl Pts',(31.3781898803372,534.294082346143,-49.4007502827554)) ;
#51763 = CARTESIAN_POINT('Ctrl Pts',(31.4873264227819,534.415701166193,-49.3926420604992)) ;
#51764 = CARTESIAN_POINT('Ctrl Pts',(31.55085602518,534.498337347723,-49.387672378011)) ;
#51765 = CARTESIAN_POINT('Ctrl Pts',(31.6648889251331,534.672592225477,-49.3775567511667)) ;
#51766 = CARTESIAN_POINT('Ctrl Pts',(31.7152113557656,534.763954895763,-49.37242335646)) ;
#51767 = CARTESIAN_POINT('Ctrl Pts',(31.7802066507066,534.906626139092,-49.3643321820162)) ;
#51768 = CARTESIAN_POINT('Ctrl Pts',(31.8001756990715,534.955337738357,-49.3615594048482)) ;
#51769 = CARTESIAN_POINT('Ctrl Pts',(31.8363684585771,535.054291381281,-49.3558778863244)) ;
#51770 = CARTESIAN_POINT('Ctrl Pts',(31.8525698956854,535.104498811128,-49.3529710065729)) ;
#51771 = CARTESIAN_POINT('Ctrl Pts',(31.9000570651526,535.273676769314,-49.3430798085291)) ;
#51772 = CARTESIAN_POINT('Ctrl Pts',(31.922591208741,535.39481190557,-49.335823589588)) ;
#51773 = CARTESIAN_POINT('Ctrl Pts',(31.9402776177387,535.581936393661,-49.3245597660857)) ;
#51774 = CARTESIAN_POINT('Ctrl Pts',(31.9433198919006,535.64690826683,-49.320643686283)) ;
#51775 = CARTESIAN_POINT('Ctrl Pts',(31.9432771819323,535.711915145219,-49.3167693044577)) ;
#51776 = CARTESIAN_POINT('Ctrl Pts',(31.9432771821887,535.711914754875,-49.316769327722)) ;
#51777 = CARTESIAN_POINT('Ctrl Pts',(31.9432442412748,535.762067106419,-49.3137802691297)) ;
#51778 = CARTESIAN_POINT('Ctrl Pts',(31.941375124574,535.81220422679,-49.3108186377364)) ;
#51779 = CARTESIAN_POINT('Ctrl Pts',(31.935239464843,535.895105881199,-49.3060138397542)) ;
#51780 = CARTESIAN_POINT('Ctrl Pts',(31.9320147090053,535.927925272046,-49.3041359273484)) ;
#51781 = CARTESIAN_POINT('Ctrl Pts',(31.9244399497136,535.989697261163,-49.3006647157832)) ;
#51782 = CARTESIAN_POINT('Ctrl Pts',(31.9202587559306,536.018660315781,-49.2990652834471)) ;
#51783 = CARTESIAN_POINT('Ctrl Pts',(31.908350508511,536.09029170372,-49.295181798816)) ;
#51784 = CARTESIAN_POINT('Ctrl Pts',(31.8998895435613,536.132821597177,-49.2929352499796)) ;
#51785 = CARTESIAN_POINT('Ctrl Pts',(31.8569359724237,536.317915483408,-49.2832956882657)) ;
#51786 = CARTESIAN_POINT('Ctrl Pts',(31.8085816250829,536.456826069626,-49.2763964087115)) ;
#51787 = CARTESIAN_POINT('Ctrl Pts',(31.7057618926767,536.674120685695,-49.2646638002179)) ;
#51788 = CARTESIAN_POINT('Ctrl Pts',(31.659934744771,536.755980875926,-49.2600041806642)) ;
#51789 = CARTESIAN_POINT('Ctrl Pts',(31.5805394180119,536.87750203505,-49.2524774593003)) ;
#51790 = CARTESIAN_POINT('Ctrl Pts',(31.5507872934754,536.919505907853,-49.2497534889718)) ;
#51791 = CARTESIAN_POINT('Ctrl Pts',(31.4863647494126,537.003577295079,-49.2440172155548)) ;
#51792 = CARTESIAN_POINT('Ctrl Pts',(31.45153460719,537.045470484097,-49.2409995908442)) ;
#51793 = CARTESIAN_POINT('Ctrl Pts',(31.3064081366201,537.206550656237,-49.2287249406726)) ;
#51794 = CARTESIAN_POINT('Ctrl Pts',(31.1838318185616,537.313852215177,-49.2189349912047)) ;
#51795 = CARTESIAN_POINT('Ctrl Pts',(30.9992486535197,537.440325784766,-49.2055003678904)) ;
#51796 = CARTESIAN_POINT('Ctrl Pts',(30.9470260259433,537.472766870433,-49.2018322810649)) ;
#51797 = CARTESIAN_POINT('Ctrl Pts',(30.8546840726854,537.524542022241,-49.1956566208903)) ;
#51798 = CARTESIAN_POINT('Ctrl Pts',(30.8152451609863,537.545003912148,-49.1931110486386)) ;
#51799 = CARTESIAN_POINT('Ctrl Pts',(30.7489496785119,537.576715299247,-49.1890192263442)) ;
#51800 = CARTESIAN_POINT('Ctrl Pts',(30.7224665776565,537.588699467579,-49.1874343691132)) ;
#51801 = CARTESIAN_POINT('Ctrl Pts',(30.6541063944406,537.617902503545,-49.1834660876428)) ;
#51802 = CARTESIAN_POINT('Ctrl Pts',(30.6119000927807,537.634306166757,-49.1811267062722)) ;
#51803 = CARTESIAN_POINT('Ctrl Pts',(30.4405285772705,537.694471602745,-49.1719380640321)) ;
#51804 = CARTESIAN_POINT('Ctrl Pts',(30.3076890610578,537.72672458864,-49.1654883249192)) ;
#51805 = CARTESIAN_POINT('Ctrl Pts',(30.0753224501381,537.75916413168,-49.154053407005)) ;
#51806 = CARTESIAN_POINT('Ctrl Pts',(29.9771775838908,537.765750941677,-49.1491818034942)) ;
#51807 = CARTESIAN_POINT('Ctrl Pts',(29.8269908818347,537.765050517608,-49.1414011947215)) ;
#51808 = CARTESIAN_POINT('Ctrl Pts',(29.7750682356347,537.762837843774,-49.138653428477)) ;
#51809 = CARTESIAN_POINT('Ctrl Pts',(29.6690509062983,537.754284405276,-49.1328974098437)) ;
#51810 = CARTESIAN_POINT('Ctrl Pts',(29.6150131225046,537.74775621618,-49.1298852279418)) ;
#51811 = CARTESIAN_POINT('Ctrl Pts',(29.398899056158,537.712894370113,-49.1175034461975)) ;
#51812 = CARTESIAN_POINT('Ctrl Pts',(29.2402503322034,537.667291745539,-49.1075843390555)) ;
#51813 = CARTESIAN_POINT('Ctrl Pts',(29.0328830950625,537.579669339908,-49.0940780794124)) ;
#51814 = CARTESIAN_POINT('Ctrl Pts',(28.9780709480623,537.553591837422,-49.0904601762015)) ;
#51815 = CARTESIAN_POINT('Ctrl Pts',(28.8855561250087,537.504440720834,-49.0843545219273)) ;
#51816 = CARTESIAN_POINT('Ctrl Pts',(28.8472941897546,537.482506148734,-49.081829938437)) ;
#51817 = CARTESIAN_POINT('Ctrl Pts',(28.7849406839166,537.444042639508,-49.0777535852956)) ;
#51818 = CARTESIAN_POINT('Ctrl Pts',(28.7604467942342,537.428203695349,-49.076164555607)) ;
#51819 = CARTESIAN_POINT('Ctrl Pts',(28.7022966236552,537.388820082287,-49.072418156034)) ;
#51820 = CARTESIAN_POINT('Ctrl Pts',(28.6689956370738,537.364779643092,-49.0702908162921)) ;
#51821 = CARTESIAN_POINT('Ctrl Pts',(28.6364362889498,537.339756631099,-49.0682055192064)) ;
#51822 = CARTESIAN_POINT('Origin',(179.888527625407,535.710565160536,-51.0680854522974)) ;
#51823 = CARTESIAN_POINT('',(178.636454084242,537.33977030723,-47.7297172548539)) ;
#51824 = CARTESIAN_POINT('',(178.636454031283,537.33977026653,-47.6715235483075)) ;
#51825 = CARTESIAN_POINT('',(178.636454050035,537.339770280941,-51.0680854522974)) ;
#51826 = CARTESIAN_POINT('',(178.005900115743,534.887332980433,-47.5221601717597)) ;
#51827 = CARTESIAN_POINT('Ctrl Pts',(178.636454031283,537.33977026653,-47.6715235483074)) ;
#51828 = CARTESIAN_POINT('Ctrl Pts',(178.622241244291,537.328847482636,-47.6704814600419)) ;
#51829 = CARTESIAN_POINT('Ctrl Pts',(178.608170085452,537.317737714185,-47.6694339709133)) ;
#51830 = CARTESIAN_POINT('Ctrl Pts',(178.487795454974,537.220111933605,-47.6603392051397)) ;
#51831 = CARTESIAN_POINT('Ctrl Pts',(178.390257733755,537.123352082591,-47.6520244043183)) ;
#51832 = CARTESIAN_POINT('Ctrl Pts',(178.270766695043,536.978408908741,-47.6410250446098)) ;
#51833 = CARTESIAN_POINT('Ctrl Pts',(178.239914709743,536.938023679574,-47.6380976511002)) ;
#51834 = CARTESIAN_POINT('Ctrl Pts',(178.193334887254,536.872121366306,-47.6335859562082)) ;
#51835 = CARTESIAN_POINT('Ctrl Pts',(178.176614522369,536.847334760524,-47.6319467323779)) ;
#51836 = CARTESIAN_POINT('Ctrl Pts',(178.137892637096,536.787139091179,-47.6281088021966)) ;
#51837 = CARTESIAN_POINT('Ctrl Pts',(178.116416799119,536.751410008282,-47.6259405168292)) ;
#51838 = CARTESIAN_POINT('Ctrl Pts',(178.042631843038,536.619741986076,-47.6182538607249)) ;
#51839 = CARTESIAN_POINT('Ctrl Pts',(177.996904655671,536.5203182312,-47.6130098299662)) ;
#51840 = CARTESIAN_POINT('Ctrl Pts',(177.913976207121,536.29407751075,-47.6014095683289)) ;
#51841 = CARTESIAN_POINT('Ctrl Pts',(177.880648984741,536.166371915471,-47.5950602972033)) ;
#51842 = CARTESIAN_POINT('Ctrl Pts',(177.850344127141,535.977660837293,-47.585308473829)) ;
#51843 = CARTESIAN_POINT('Ctrl Pts',(177.843470324144,535.91858396682,-47.5822086935008)) ;
#51844 = CARTESIAN_POINT('Ctrl Pts',(177.835129018986,535.803648919444,-47.5760493617157)) ;
#51845 = CARTESIAN_POINT('Ctrl Pts',(177.833358928503,535.747864828306,-47.5730017673884)) ;
#51846 = CARTESIAN_POINT('Ctrl Pts',(177.834390525618,535.63319364148,-47.5666077983981)) ;
#51847 = CARTESIAN_POINT('Ctrl Pts',(177.837451587011,535.574359951797,-47.5632571137478)) ;
#51848 = CARTESIAN_POINT('Ctrl Pts',(177.860528500515,535.332069906454,-47.5491992978391)) ;
#51849 = CARTESIAN_POINT('Ctrl Pts',(177.902678893347,535.151601443863,-47.538034543782)) ;
#51850 = CARTESIAN_POINT('Ctrl Pts',(177.980123617115,534.948275115569,-47.5257870782419)) ;
#51851 = CARTESIAN_POINT('Ctrl Pts',(177.99264445056,534.917647004273,-47.523954068162)) ;
#51852 = CARTESIAN_POINT('Ctrl Pts',(178.005900115743,534.887332980433,-47.5221601717592)) ;
#51853 = CARTESIAN_POINT('',(178.665833051125,534.0564728875,-47.5234367538311)) ;
#51854 = CARTESIAN_POINT('Origin',(179.888527625407,535.710565160536,-47.5221601717598)) ;
#51855 = CARTESIAN_POINT('Ctrl Pts',(178.66691495143,534.058396876953,-47.5247133359024)) ;
#51856 = CARTESIAN_POINT('Ctrl Pts',(178.653554632771,534.068275492082,-47.5256108747939)) ;
#51857 = CARTESIAN_POINT('Ctrl Pts',(178.640314154938,534.078316154102,-47.5264974635798)) ;
#51858 = CARTESIAN_POINT('Ctrl Pts',(178.609741628923,534.10208984521,-47.5285415549366)) ;
#51859 = CARTESIAN_POINT('Ctrl Pts',(178.592506376018,534.115944372768,-47.529691568149)) ;
#51860 = CARTESIAN_POINT('Ctrl Pts',(178.480887460634,534.208674458136,-47.5371483885131)) ;
#51861 = CARTESIAN_POINT('Ctrl Pts',(178.393517563906,534.295617517028,-47.543040828045)) ;
#51862 = CARTESIAN_POINT('Ctrl Pts',(178.238400994016,534.480493399766,-47.554746511401)) ;
#51863 = CARTESIAN_POINT('Ctrl Pts',(178.17033202049,534.577518430838,-47.5605359409273)) ;
#51864 = CARTESIAN_POINT('Ctrl Pts',(178.0843676294,534.725769974689,-47.569377909882)) ;
#51865 = CARTESIAN_POINT('Ctrl Pts',(178.059533375984,534.772698322752,-47.5721734120944)) ;
#51866 = CARTESIAN_POINT('Ctrl Pts',(178.013598200371,534.868280411217,-47.5778903672997)) ;
#51867 = CARTESIAN_POINT('Ctrl Pts',(177.992508280832,534.91689403092,-47.58080939126)) ;
#51868 = CARTESIAN_POINT('Ctrl Pts',(177.933132345828,535.069678090164,-47.5900337950995)) ;
#51869 = CARTESIAN_POINT('Ctrl Pts',(177.901389966094,535.176163280757,-47.5965450728088)) ;
#51870 = CARTESIAN_POINT('Ctrl Pts',(177.85863217262,535.377973848484,-47.6088662704022)) ;
#51871 = CARTESIAN_POINT('Ctrl Pts',(177.845384512702,535.472533506183,-47.6146279962836)) ;
#51872 = CARTESIAN_POINT('Ctrl Pts',(177.83587297935,535.608974478693,-47.6226983222894)) ;
#51873 = CARTESIAN_POINT('Ctrl Pts',(177.834242565512,535.650357026585,-47.6251131677995)) ;
#51874 = CARTESIAN_POINT('Ctrl Pts',(177.833548742366,535.726175030821,-47.6294456249277)) ;
#51875 = CARTESIAN_POINT('Ctrl Pts',(177.834098391708,535.760592294423,-47.631377639716)) ;
#51876 = CARTESIAN_POINT('Ctrl Pts',(177.836788018584,535.8260042097,-47.634962833962)) ;
#51877 = CARTESIAN_POINT('Ctrl Pts',(177.838766611096,535.856994141036,-47.6366225394175)) ;
#51878 = CARTESIAN_POINT('Ctrl Pts',(177.847683417546,535.959909738471,-47.6420371816208)) ;
#51879 = CARTESIAN_POINT('Ctrl Pts',(177.857712919098,536.031518797643,-47.6456483375471)) ;
#51880 = CARTESIAN_POINT('Ctrl Pts',(177.90335162002,536.266417695381,-47.657388391457)) ;
#51881 = CARTESIAN_POINT('Ctrl Pts',(177.955078554029,536.425877429872,-47.6652397567559)) ;
#51882 = CARTESIAN_POINT('Ctrl Pts',(178.050738467198,536.631487382625,-47.6767287643819)) ;
#51883 = CARTESIAN_POINT('Ctrl Pts',(178.078288131683,536.684525530326,-47.6798209461223)) ;
#51884 = CARTESIAN_POINT('Ctrl Pts',(178.132999386801,536.779492003157,-47.6856461779284)) ;
#51885 = CARTESIAN_POINT('Ctrl Pts',(178.159454084318,536.821775344459,-47.6883518928744)) ;
#51886 = CARTESIAN_POINT('Ctrl Pts',(178.228469563014,536.923644446014,-47.695170288032)) ;
#51887 = CARTESIAN_POINT('Ctrl Pts',(178.272724187717,536.981994100583,-47.6993455034216)) ;
#51888 = CARTESIAN_POINT('Ctrl Pts',(178.414445354432,537.149474191995,-47.7121467206265)) ;
#51889 = CARTESIAN_POINT('Ctrl Pts',(178.520532853448,537.250682750497,-47.7210498099191)) ;
#51890 = CARTESIAN_POINT('Ctrl Pts',(178.636454084242,537.33977030723,-47.7297172548539)) ;
#51891 = CARTESIAN_POINT('Origin',(179.888527625407,535.710565160536,-51.0680854522974)) ;
#51892 = CARTESIAN_POINT('',(178.636454050042,537.339770280947,-48.4293891818575)) ;
#51893 = CARTESIAN_POINT('',(178.636454050035,537.339770280941,-48.3712393117967)) ;
#51894 = CARTESIAN_POINT('',(178.636454050035,537.339770280941,-51.0680854522974)) ;
#51895 = CARTESIAN_POINT('',(181.943277552311,535.710017082759,-47.9194801829612)) ;
#51896 = CARTESIAN_POINT('Ctrl Pts',(178.636454050035,537.339770280941,-48.3712393117967)) ;
#51897 = CARTESIAN_POINT('Ctrl Pts',(178.61681784653,537.324679503714,-48.3699919406657)) ;
#51898 = CARTESIAN_POINT('Ctrl Pts',(178.597447145434,537.309228100014,-48.3687333142884)) ;
#51899 = CARTESIAN_POINT('Ctrl Pts',(178.53619493261,537.258527921646,-48.3646541659042)) ;
#51900 = CARTESIAN_POINT('Ctrl Pts',(178.495451670995,537.221965527656,-48.3617871416412)) ;
#51901 = CARTESIAN_POINT('Ctrl Pts',(178.419091441373,537.147727686935,-48.3560701383734)) ;
#51902 = CARTESIAN_POINT('Ctrl Pts',(178.383344862517,537.110244761674,-48.3532296844346)) ;
#51903 = CARTESIAN_POINT('Ctrl Pts',(178.285708819313,536.999796288613,-48.3449692570823)) ;
#51904 = CARTESIAN_POINT('Ctrl Pts',(178.2274514836,536.923811742882,-48.3394070274034)) ;
#51905 = CARTESIAN_POINT('Ctrl Pts',(178.099180161897,536.729866740007,-48.3255872806016)) ;
#51906 = CARTESIAN_POINT('Ctrl Pts',(178.035261483984,536.608420374485,-48.3172233934903)) ;
#51907 = CARTESIAN_POINT('Ctrl Pts',(177.96633307106,536.438134095399,-48.3064756171413)) ;
#51908 = CARTESIAN_POINT('Ctrl Pts',(177.950257036136,536.394155862429,-48.3037846453818)) ;
#51909 = CARTESIAN_POINT('Ctrl Pts',(177.926626139136,536.32194923244,-48.2995449213575)) ;
#51910 = CARTESIAN_POINT('Ctrl Pts',(177.918147228565,536.29404547518,-48.2979504864009)) ;
#51911 = CARTESIAN_POINT('Ctrl Pts',(177.898542956795,536.224217629692,-48.2940696480827)) ;
#51912 = CARTESIAN_POINT('Ctrl Pts',(177.88814575171,536.182105970463,-48.2918209449869)) ;
#51913 = CARTESIAN_POINT('Ctrl Pts',(177.866756075967,536.081946641437,-48.2866210903349)) ;
#51914 = CARTESIAN_POINT('Ctrl Pts',(177.85691814294,536.023691392238,-48.2837120782991)) ;
#51915 = CARTESIAN_POINT('Ctrl Pts',(177.828580044645,535.796683649006,-48.2725614363835)) ;
#51916 = CARTESIAN_POINT('Ctrl Pts',(177.828502451848,535.626333647324,-48.2645239715233)) ;
#51917 = CARTESIAN_POINT('Ctrl Pts',(177.85601137451,535.404309255045,-48.2530204633537)) ;
#51918 = CARTESIAN_POINT('Ctrl Pts',(177.864763379831,535.350992423478,-48.250184514104)) ;
#51919 = CARTESIAN_POINT('Ctrl Pts',(177.886104562335,535.246846390212,-48.2444671461068)) ;
#51920 = CARTESIAN_POINT('Ctrl Pts',(177.898556008103,535.196030932204,-48.24159216538)) ;
#51921 = CARTESIAN_POINT('Ctrl Pts',(177.941407423834,535.046146656137,-48.2328388124249)) ;
#51922 = CARTESIAN_POINT('Ctrl Pts',(177.977371222526,534.948852930602,-48.2267844777629)) ;
#51923 = CARTESIAN_POINT('Ctrl Pts',(178.076475489919,534.732548601796,-48.2125910509409)) ;
#51924 = CARTESIAN_POINT('Ctrl Pts',(178.144284352135,534.616186123,-48.2043923758195)) ;
#51925 = CARTESIAN_POINT('Ctrl Pts',(178.247791903485,534.472913818179,-48.1941182136836)) ;
#51926 = CARTESIAN_POINT('Ctrl Pts',(178.273675922731,534.439325978522,-48.1916974722371)) ;
#51927 = CARTESIAN_POINT('Ctrl Pts',(178.319142746753,534.383958966747,-48.1877195471781)) ;
#51928 = CARTESIAN_POINT('Ctrl Pts',(178.338181747529,534.361758022489,-48.1861303511333)) ;
#51929 = CARTESIAN_POINT('Ctrl Pts',(178.389902506627,534.303990534366,-48.1820036036833)) ;
#51930 = CARTESIAN_POINT('Ctrl Pts',(178.42337409428,534.269157775859,-48.1795195938335)) ;
#51931 = CARTESIAN_POINT('Ctrl Pts',(178.508728658754,534.186381007479,-48.1735325044469)) ;
#51932 = CARTESIAN_POINT('Ctrl Pts',(178.561915306547,534.139870008612,-48.1700918698385)) ;
#51933 = CARTESIAN_POINT('Ctrl Pts',(178.733413332153,534.004835267902,-48.1595104238687)) ;
#51934 = CARTESIAN_POINT('Ctrl Pts',(178.858932391316,533.926263119798,-48.1524274739569)) ;
#51935 = CARTESIAN_POINT('Ctrl Pts',(179.040596208193,533.838146157368,-48.1420539146653)) ;
#51936 = CARTESIAN_POINT('Ctrl Pts',(179.090322079901,533.816414217006,-48.1392077861016)) ;
#51937 = CARTESIAN_POINT('Ctrl Pts',(179.18933198082,533.777734954425,-48.1334948978683)) ;
#51938 = CARTESIAN_POINT('Ctrl Pts',(179.238515931001,533.760644328828,-48.1306357841272)) ;
#51939 = CARTESIAN_POINT('Ctrl Pts',(179.383738495676,533.716287018275,-48.1221158578994)) ;
#51940 = CARTESIAN_POINT('Ctrl Pts',(179.481169690976,533.694129539853,-48.1162953426907)) ;
#51941 = CARTESIAN_POINT('Ctrl Pts',(179.714214922398,533.658713979496,-48.102252649518)) ;
#51942 = CARTESIAN_POINT('Ctrl Pts',(179.850308016329,533.651677714594,-48.093947686279)) ;
#51943 = CARTESIAN_POINT('Ctrl Pts',(180.030456657865,533.660241816041,-48.0834283459741)) ;
#51944 = CARTESIAN_POINT('Ctrl Pts',(180.074738376255,533.663788227966,-48.0808835460415)) ;
#51945 = CARTESIAN_POINT('Ctrl Pts',(180.147774755263,533.672027840135,-48.0767916304269)) ;
#51946 = CARTESIAN_POINT('Ctrl Pts',(180.176601900043,533.675901331577,-48.0752059894901)) ;
#51947 = CARTESIAN_POINT('Ctrl Pts',(180.250162087207,533.68738058732,-48.0712321752011)) ;
#51948 = CARTESIAN_POINT('Ctrl Pts',(180.294741366709,533.695857664443,-48.0688883242128)) ;
#51949 = CARTESIAN_POINT('Ctrl Pts',(180.401053808762,533.719746552248,-48.06337697629)) ;
#51950 = CARTESIAN_POINT('Ctrl Pts',(180.462423730457,533.736562651236,-48.0602593885099)) ;
#51951 = CARTESIAN_POINT('Ctrl Pts',(180.67122633419,533.804340257326,-48.0495907810143)) ;
#51952 = CARTESIAN_POINT('Ctrl Pts',(180.813562497029,533.869201881747,-48.0421664624997)) ;
#51953 = CARTESIAN_POINT('Ctrl Pts',(180.994395316116,533.977911858992,-48.0313605436958)) ;
#51954 = CARTESIAN_POINT('Ctrl Pts',(181.040434135106,534.008172298556,-48.028479989484)) ;
#51955 = CARTESIAN_POINT('Ctrl Pts',(181.126766735997,534.070023736512,-48.0227868124446)) ;
#51956 = CARTESIAN_POINT('Ctrl Pts',(181.167204890963,534.101342975496,-48.0199861807067)) ;
#51957 = CARTESIAN_POINT('Ctrl Pts',(181.274979489639,534.19144309082,-48.0121268326259)) ;
#51958 = CARTESIAN_POINT('Ctrl Pts',(181.339709689749,534.253153739325,-48.0069492620272)) ;
#51959 = CARTESIAN_POINT('Ctrl Pts',(181.51000038868,534.438127290328,-47.9920464639506)) ;
#51960 = CARTESIAN_POINT('Ctrl Pts',(181.605285557693,534.569945891328,-47.9820652095229)) ;
#51961 = CARTESIAN_POINT('Ctrl Pts',(181.702850138356,534.745308503317,-47.9704548150123)) ;
#51962 = CARTESIAN_POINT('Ctrl Pts',(181.720658563074,534.779553215839,-47.9682616028805)) ;
#51963 = CARTESIAN_POINT('Ctrl Pts',(181.750455348452,534.841021728951,-47.9644807979488)) ;
#51964 = CARTESIAN_POINT('Ctrl Pts',(181.762834472073,534.868036512242,-47.9628730883071)) ;
#51965 = CARTESIAN_POINT('Ctrl Pts',(181.796020306939,534.944812569609,-47.958437123859)) ;
#51966 = CARTESIAN_POINT('Ctrl Pts',(181.815460302174,534.995137516539,-47.9556805832737)) ;
#51967 = CARTESIAN_POINT('Ctrl Pts',(181.860682373304,535.127481722694,-47.9486790861811)) ;
#51968 = CARTESIAN_POINT('Ctrl Pts',(181.883339355026,535.210457074341,-47.9445258986763)) ;
#51969 = CARTESIAN_POINT('Ctrl Pts',(181.919415715015,535.384978693358,-47.9358756317244)) ;
#51970 = CARTESIAN_POINT('Ctrl Pts',(181.93198670496,535.476499536271,-47.9313838294082)) ;
#51971 = CARTESIAN_POINT('Ctrl Pts',(181.941626372663,535.61563888671,-47.924358540693)) ;
#51972 = CARTESIAN_POINT('Ctrl Pts',(181.943264963639,535.662822005758,-47.9219435873794)) ;
#51973 = CARTESIAN_POINT('Ctrl Pts',(181.943277552311,535.710017082759,-47.9194801829612)) ;
#51974 = CARTESIAN_POINT('Ctrl Pts',(181.943277552624,535.710018258454,-47.9194801215943)) ;
#51975 = CARTESIAN_POINT('Ctrl Pts',(181.943289182331,535.753711894313,-47.9171994784251)) ;
#51976 = CARTESIAN_POINT('Ctrl Pts',(181.941907122319,535.797392922001,-47.9148785468896)) ;
#51977 = CARTESIAN_POINT('Ctrl Pts',(181.935807836813,535.893285140802,-47.9096765599099)) ;
#51978 = CARTESIAN_POINT('Ctrl Pts',(181.930483325185,535.945424826066,-47.9067778059617)) ;
#51979 = CARTESIAN_POINT('Ctrl Pts',(181.899871429793,536.162643392762,-47.894386332717)) ;
#51980 = CARTESIAN_POINT('Ctrl Pts',(181.856505277595,536.324507726671,-47.8843162387126)) ;
#51981 = CARTESIAN_POINT('Ctrl Pts',(181.760655183561,536.562096114654,-47.868923340987)) ;
#51982 = CARTESIAN_POINT('Ctrl Pts',(181.721894328725,536.642625116597,-47.8636035240152)) ;
#51983 = CARTESIAN_POINT('Ctrl Pts',(181.662105794812,536.748575747719,-47.8566824597145)) ;
#51984 = CARTESIAN_POINT('Ctrl Pts',(181.64553099857,536.776391143384,-47.8548737936266)) ;
#51985 = CARTESIAN_POINT('Ctrl Pts',(181.61040251692,536.832294406511,-47.8512741825207)) ;
#51986 = CARTESIAN_POINT('Ctrl Pts',(181.591802550929,536.860340992242,-47.8494863364649)) ;
#51987 = CARTESIAN_POINT('Ctrl Pts',(181.499101817306,536.9929326575,-47.8410586031852)) ;
#51988 = CARTESIAN_POINT('Ctrl Pts',(181.416012823482,537.090859172478,-47.8348961676524)) ;
#51989 = CARTESIAN_POINT('Ctrl Pts',(181.237719945758,537.265022725074,-47.8227870929446)) ;
#51990 = CARTESIAN_POINT('Ctrl Pts',(181.143801406468,537.341804745452,-47.8168668400908)) ;
#51991 = CARTESIAN_POINT('Ctrl Pts',(180.999193941225,537.440105869839,-47.8078436098311)) ;
#51992 = CARTESIAN_POINT('Ctrl Pts',(180.953543430938,537.468584318471,-47.8050099607897)) ;
#51993 = CARTESIAN_POINT('Ctrl Pts',(180.860275747129,537.521801245292,-47.7992175498136)) ;
#51994 = CARTESIAN_POINT('Ctrl Pts',(180.812702534486,537.546530994621,-47.796261516008)) ;
#51995 = CARTESIAN_POINT('Ctrl Pts',(180.661918162597,537.617566219307,-47.786870025466)) ;
#51996 = CARTESIAN_POINT('Ctrl Pts',(180.555825367047,537.657227384585,-47.7802179886134)) ;
#51997 = CARTESIAN_POINT('Ctrl Pts',(180.355248261042,537.713878343011,-47.7677376528832)) ;
#51998 = CARTESIAN_POINT('Ctrl Pts',(180.261781089591,537.733378562018,-47.7619624973742)) ;
#51999 = CARTESIAN_POINT('Ctrl Pts',(180.111044672498,537.754019928219,-47.7529668189346)) ;
#52000 = CARTESIAN_POINT('Ctrl Pts',(180.054492459894,537.759388708774,-47.7496635970557)) ;
#52001 = CARTESIAN_POINT('Ctrl Pts',(179.968382870824,537.763973965642,-47.744812096897)) ;
#52002 = CARTESIAN_POINT('Ctrl Pts',(179.938946271435,537.764907607887,-47.7431853149115)) ;
#52003 = CARTESIAN_POINT('Ctrl Pts',(179.87501806743,537.765560039696,-47.739735646073)) ;
#52004 = CARTESIAN_POINT('Ctrl Pts',(179.840533702508,537.765044015645,-47.7379257465054)) ;
#52005 = CARTESIAN_POINT('Ctrl Pts',(179.693200965336,537.759127210237,-47.7303492195271)) ;
#52006 = CARTESIAN_POINT('Ctrl Pts',(179.580879348399,537.745292849729,-47.7249582791518)) ;
#52007 = CARTESIAN_POINT('Ctrl Pts',(179.334288381766,537.694022409274,-47.7129510924467)) ;
#52008 = CARTESIAN_POINT('Ctrl Pts',(179.201550247138,537.652044534648,-47.7063503629113)) ;
#52009 = CARTESIAN_POINT('Ctrl Pts',(179.022973899834,537.574944681291,-47.6964728773845)) ;
#52010 = CARTESIAN_POINT('Ctrl Pts',(178.972805295937,537.550822227816,-47.6935832826104)) ;
#52011 = CARTESIAN_POINT('Ctrl Pts',(178.879618558127,537.501260740286,-47.6879606784832)) ;
#52012 = CARTESIAN_POINT('Ctrl Pts',(178.836428328765,537.47623064679,-47.6852442933513)) ;
#52013 = CARTESIAN_POINT('Ctrl Pts',(178.739916262091,537.415499816828,-47.6789059786744)) ;
#52014 = CARTESIAN_POINT('Ctrl Pts',(178.687279541144,537.378830590225,-47.6752500987332)) ;
#52015 = CARTESIAN_POINT('Ctrl Pts',(178.636454031283,537.33977026653,-47.6715235483074)) ;
#52016 = CARTESIAN_POINT('Ctrl Pts',(178.636454084242,537.33977030723,-47.7297172548539)) ;
#52017 = CARTESIAN_POINT('Ctrl Pts',(178.685687477448,537.37760705793,-47.7333984418258)) ;
#52018 = CARTESIAN_POINT('Ctrl Pts',(178.736606611229,537.413190289609,-47.7370242250661)) ;
#52019 = CARTESIAN_POINT('Ctrl Pts',(178.81115013104,537.46040467576,-47.7419998958145)) ;
#52020 = CARTESIAN_POINT('Ctrl Pts',(178.833494913938,537.473967190394,-47.7434510381069)) ;
#52021 = CARTESIAN_POINT('Ctrl Pts',(178.884590621336,537.503661479162,-47.7466683557087)) ;
#52022 = CARTESIAN_POINT('Ctrl Pts',(178.913483882856,537.519535555978,-47.7484173758533)) ;
#52023 = CARTESIAN_POINT('Ctrl Pts',(179.062251292068,537.59666827089,-47.7571337599225)) ;
#52024 = CARTESIAN_POINT('Ctrl Pts',(179.187567416033,537.646741921251,-47.7635554209541)) ;
#52025 = CARTESIAN_POINT('Ctrl Pts',(179.396521964938,537.707262613412,-47.774072988367)) ;
#52026 = CARTESIAN_POINT('Ctrl Pts',(179.477470882733,537.725484920213,-47.7781011992131)) ;
#52027 = CARTESIAN_POINT('Ctrl Pts',(179.624237138341,537.749309043585,-47.7855481689957)) ;
#52028 = CARTESIAN_POINT('Ctrl Pts',(179.689642272061,537.756724871013,-47.788915922458)) ;
#52029 = CARTESIAN_POINT('Ctrl Pts',(179.804441588076,537.76418477248,-47.7949809709441)) ;
#52030 = CARTESIAN_POINT('Ctrl Pts',(179.853692118013,537.76561014154,-47.7976317136049)) ;
#52031 = CARTESIAN_POINT('Ctrl Pts',(179.966529828995,537.764818463141,-47.8038352455562)) ;
#52032 = CARTESIAN_POINT('Ctrl Pts',(180.030055466799,537.76142097971,-47.8074232914933)) ;
#52033 = CARTESIAN_POINT('Ctrl Pts',(180.240322480307,537.740359586022,-47.819617383276)) ;
#52034 = CARTESIAN_POINT('Ctrl Pts',(180.385300255133,537.709823286097,-47.8285802680629)) ;
#52035 = CARTESIAN_POINT('Ctrl Pts',(180.59961835303,537.639914291865,-47.8420724700505)) ;
#52036 = CARTESIAN_POINT('Ctrl Pts',(180.672087200866,537.611637101074,-47.8466703459523)) ;
#52037 = CARTESIAN_POINT('Ctrl Pts',(180.771414483415,537.566231969079,-47.8528671189628)) ;
#52038 = CARTESIAN_POINT('Ctrl Pts',(180.799742361165,537.55248714087,-47.8546214501462)) ;
#52039 = CARTESIAN_POINT('Ctrl Pts',(180.857528093276,537.522789460561,-47.8581560180192)) ;
#52040 = CARTESIAN_POINT('Ctrl Pts',(180.886933737727,537.506756782897,-47.8599313551668)) ;
#52041 = CARTESIAN_POINT('Ctrl Pts',(181.02800350684,537.425306566577,-47.8683969585011)) ;
#52042 = CARTESIAN_POINT('Ctrl Pts',(181.133720115245,537.350152378984,-47.8745943726628)) ;
#52043 = CARTESIAN_POINT('Ctrl Pts',(181.319259516789,537.189889052216,-47.8864586667367)) ;
#52044 = CARTESIAN_POINT('Ctrl Pts',(181.400293523093,537.106972648024,-47.8920931915066)) ;
#52045 = CARTESIAN_POINT('Ctrl Pts',(181.508904298271,536.975240139511,-47.9008373333092)) ;
#52046 = CARTESIAN_POINT('Ctrl Pts',(181.542175965983,536.931413138843,-47.9037142096324)) ;
#52047 = CARTESIAN_POINT('Ctrl Pts',(181.602880850663,536.844408458367,-47.9094002714266)) ;
#52048 = CARTESIAN_POINT('Ctrl Pts',(181.630539202881,536.801437566428,-47.912197582475)) ;
#52049 = CARTESIAN_POINT('Ctrl Pts',(181.70221812751,536.680385981463,-47.9200649155108)) ;
#52050 = CARTESIAN_POINT('Ctrl Pts',(181.742773293613,536.600394060534,-47.92525409321)) ;
#52051 = CARTESIAN_POINT('Ctrl Pts',(181.825000726815,536.407981178919,-47.937645641096)) ;
#52052 = CARTESIAN_POINT('Ctrl Pts',(181.862320735848,536.294051458501,-47.9449225581174)) ;
#52053 = CARTESIAN_POINT('Ctrl Pts',(181.899846458246,536.133248562576,-47.9547314664799)) ;
#52054 = CARTESIAN_POINT('Ctrl Pts',(181.908707131037,536.08863911412,-47.9574030989414)) ;
#52055 = CARTESIAN_POINT('Ctrl Pts',(181.922017294556,536.007646758512,-47.9621243266189)) ;
#52056 = CARTESIAN_POINT('Ctrl Pts',(181.92698775211,535.971368515585,-47.9641927971265)) ;
#52057 = CARTESIAN_POINT('Ctrl Pts',(181.934265639859,535.905128903429,-47.9678620142713)) ;
#52058 = CARTESIAN_POINT('Ctrl Pts',(181.936890223218,535.875215636876,-47.969477156334)) ;
#52059 = CARTESIAN_POINT('Ctrl Pts',(181.942795410697,535.785322881013,-47.9742283013494)) ;
#52060 = CARTESIAN_POINT('Ctrl Pts',(181.944103114246,535.725242506601,-47.9772698330283)) ;
#52061 = CARTESIAN_POINT('Ctrl Pts',(181.939807372805,535.530777245452,-47.9869191182631)) ;
#52062 = CARTESIAN_POINT('Ctrl Pts',(181.923654142591,535.396981089927,-47.9932757005685)) ;
#52063 = CARTESIAN_POINT('Ctrl Pts',(181.880006417125,535.200153733712,-48.0031982680774)) ;
#52064 = CARTESIAN_POINT('Ctrl Pts',(181.862262496659,535.135345816245,-48.0065581455773)) ;
#52065 = CARTESIAN_POINT('Ctrl Pts',(181.824716310563,535.020607722103,-48.0127700932045)) ;
#52066 = CARTESIAN_POINT('Ctrl Pts',(181.806070139393,534.970363904315,-48.0155846515336)) ;
#52067 = CARTESIAN_POINT('Ctrl Pts',(181.765484718173,534.872867392984,-48.0212662086155)) ;
#52068 = CARTESIAN_POINT('Ctrl Pts',(181.743669947075,534.825606549667,-48.0241272649742)) ;
#52069 = CARTESIAN_POINT('Ctrl Pts',(181.637263841788,534.616349464793,-48.037310963502)) ;
#52070 = CARTESIAN_POINT('Ctrl Pts',(181.533094672285,534.46526905478,-48.0483661238227)) ;
#52071 = CARTESIAN_POINT('Ctrl Pts',(181.356431001054,534.27053028914,-48.0641163596042)) ;
#52072 = CARTESIAN_POINT('Ctrl Pts',(181.299055818234,534.214285394287,-48.0688725918868)) ;
#52073 = CARTESIAN_POINT('Ctrl Pts',(181.214643608276,534.140718643376,-48.0752298539368)) ;
#52074 = CARTESIAN_POINT('Ctrl Pts',(181.190274298195,534.120452697429,-48.0769969582583)) ;
#52075 = CARTESIAN_POINT('Ctrl Pts',(181.139306206774,534.080024295535,-48.0805382092355)) ;
#52076 = CARTESIAN_POINT('Ctrl Pts',(181.11266591736,534.059930040175,-48.0823082034492)) ;
#52077 = CARTESIAN_POINT('Ctrl Pts',(180.953855587551,533.946103305297,-48.0924699359517)) ;
#52078 = CARTESIAN_POINT('Ctrl Pts',(180.81144783541,533.867610934047,-48.1000769692788)) ;
#52079 = CARTESIAN_POINT('Ctrl Pts',(180.570904824445,533.769979519519,-48.1127366084379)) ;
#52080 = CARTESIAN_POINT('Ctrl Pts',(180.478037008903,533.739781721875,-48.1175760540537)) ;
#52081 = CARTESIAN_POINT('Ctrl Pts',(180.333230600594,533.703849705101,-48.1253071526701)) ;
#52082 = CARTESIAN_POINT('Ctrl Pts',(180.282630468146,533.693302172839,-48.1280403114051)) ;
#52083 = CARTESIAN_POINT('Ctrl Pts',(180.178433531459,533.675652461824,-48.1337593693304)) ;
#52084 = CARTESIAN_POINT('Ctrl Pts',(180.124846742387,533.668735682704,-48.1367489086414)) ;
#52085 = CARTESIAN_POINT('Ctrl Pts',(179.904910132251,533.649120960526,-48.1492346210964)) ;
#52086 = CARTESIAN_POINT('Ctrl Pts',(179.737601533126,533.654592126093,-48.159301603949)) ;
#52087 = CARTESIAN_POINT('Ctrl Pts',(179.487761388751,533.693439602165,-48.1744722269792)) ;
#52088 = CARTESIAN_POINT('Ctrl Pts',(179.403601174043,533.712001199492,-48.1795913309669)) ;
#52089 = CARTESIAN_POINT('Ctrl Pts',(179.290062045862,533.744639780057,-48.1863067908646)) ;
#52090 = CARTESIAN_POINT('Ctrl Pts',(179.259484878687,533.754209058198,-48.1880953221101)) ;
#52091 = CARTESIAN_POINT('Ctrl Pts',(179.197961285549,533.77505501519,-48.1916352548595)) ;
#52092 = CARTESIAN_POINT('Ctrl Pts',(179.167037319044,533.786368339009,-48.1933842396946)) ;
#52093 = CARTESIAN_POINT('Ctrl Pts',(179.009921108121,533.848169089616,-48.2021772461662)) ;
#52094 = CARTESIAN_POINT('Ctrl Pts',(178.888678795771,533.910348738732,-48.2086665715154)) ;
#52095 = CARTESIAN_POINT('Ctrl Pts',(178.673966415221,534.048896898901,-48.2210444597538)) ;
#52096 = CARTESIAN_POINT('Ctrl Pts',(178.57933642824,534.122385320502,-48.226889775387)) ;
#52097 = CARTESIAN_POINT('Ctrl Pts',(178.452950738439,534.239545158775,-48.2357814647762)) ;
#52098 = CARTESIAN_POINT('Ctrl Pts',(178.415658974168,534.276885243045,-48.2385603147672)) ;
#52099 = CARTESIAN_POINT('Ctrl Pts',(178.344055460991,534.354326682618,-48.2442473141203)) ;
#52100 = CARTESIAN_POINT('Ctrl Pts',(178.309769405397,534.394396923196,-48.2471532337662)) ;
#52101 = CARTESIAN_POINT('Ctrl Pts',(178.175002471345,534.564751096159,-48.2593832535293)) ;
#52102 = CARTESIAN_POINT('Ctrl Pts',(178.088817253075,534.705535772939,-48.2692705151715)) ;
#52103 = CARTESIAN_POINT('Ctrl Pts',(177.993640978736,534.913372349241,-48.2830021825533)) ;
#52104 = CARTESIAN_POINT('Ctrl Pts',(177.969679022503,534.972911745534,-48.2868374235868)) ;
#52105 = CARTESIAN_POINT('Ctrl Pts',(177.933527588759,535.076492484416,-48.2932467352559)) ;
#52106 = CARTESIAN_POINT('Ctrl Pts',(177.919948078301,535.119998914121,-48.2958621955047)) ;
#52107 = CARTESIAN_POINT('Ctrl Pts',(177.90012185313,535.191837338889,-48.3000171060359)) ;
#52108 = CARTESIAN_POINT('Ctrl Pts',(177.893009336659,535.219909412402,-48.3015988068127)) ;
#52109 = CARTESIAN_POINT('Ctrl Pts',(177.876657549292,535.290701370407,-48.3054837502227)) ;
#52110 = CARTESIAN_POINT('Ctrl Pts',(177.868183479543,535.333581232832,-48.3077478081702)) ;
#52111 = CARTESIAN_POINT('Ctrl Pts',(177.83909292664,535.510238707624,-48.3168304746283)) ;
#52112 = CARTESIAN_POINT('Ctrl Pts',(177.830348255772,535.645630785443,-48.3232403425754)) ;
#52113 = CARTESIAN_POINT('Ctrl Pts',(177.838429805884,535.88156067798,-48.3347349174434)) ;
#52114 = CARTESIAN_POINT('Ctrl Pts',(177.849272749966,535.981816591309,-48.339719750075)) ;
#52115 = CARTESIAN_POINT('Ctrl Pts',(177.876771223467,536.131903443152,-48.3476189791927)) ;
#52116 = CARTESIAN_POINT('Ctrl Pts',(177.888051210792,536.182564349684,-48.3503609527888)) ;
#52117 = CARTESIAN_POINT('Ctrl Pts',(177.914888722308,536.284702240533,-48.3560713388705)) ;
#52118 = CARTESIAN_POINT('Ctrl Pts',(177.930573436248,536.336103750902,-48.3590421460671)) ;
#52119 = CARTESIAN_POINT('Ctrl Pts',(178.004141518487,536.547178733051,-48.37166963816)) ;
#52120 = CARTESIAN_POINT('Ctrl Pts',(178.079685826321,536.69996237271,-48.3819248012611)) ;
#52121 = CARTESIAN_POINT('Ctrl Pts',(178.219595310628,536.912141291437,-48.3971658400929)) ;
#52122 = CARTESIAN_POINT('Ctrl Pts',(178.270355455873,536.97967566915,-48.4021787262244)) ;
#52123 = CARTESIAN_POINT('Ctrl Pts',(178.345859865158,537.068208090769,-48.4087903721179)) ;
#52124 = CARTESIAN_POINT('Ctrl Pts',(178.367155882681,537.092030505018,-48.4105733956411)) ;
#52125 = CARTESIAN_POINT('Ctrl Pts',(178.411595647049,537.139467452332,-48.4141143447367)) ;
#52126 = CARTESIAN_POINT('Ctrl Pts',(178.434770842369,537.163039368276,-48.415869368546)) ;
#52127 = CARTESIAN_POINT('Ctrl Pts',(178.514834388777,537.240636309498,-48.4216735689377)) ;
#52128 = CARTESIAN_POINT('Ctrl Pts',(178.574247376926,537.29196332856,-48.4255599821672)) ;
#52129 = CARTESIAN_POINT('Ctrl Pts',(178.636454050048,537.339770280952,-48.4293891818575)) ;
#52130 = CARTESIAN_POINT('Origin',(179.888527625407,535.710565160536,-51.0680854522974)) ;
#52131 = CARTESIAN_POINT('',(178.636879422838,537.339310206396,-49.1271677662019)) ;
#52132 = CARTESIAN_POINT('',(178.63645405003,537.339770280938,-49.068197094383)) ;
#52133 = CARTESIAN_POINT('',(178.636454050035,537.339770280941,-51.0680854522974)) ;
#52134 = CARTESIAN_POINT('',(181.943277580094,535.710133636274,-49.3762357667005)) ;
#52135 = CARTESIAN_POINT('Ctrl Pts',(181.942732094631,535.710094699042,-49.3752911028376)) ;
#52136 = CARTESIAN_POINT('Ctrl Pts',(181.942612236032,535.781018676224,-49.3712179668236)) ;
#52137 = CARTESIAN_POINT('Ctrl Pts',(181.938847034173,535.851983770071,-49.3672000176889)) ;
#52138 = CARTESIAN_POINT('Ctrl Pts',(181.931463151663,535.922593192326,-49.3632666223797)) ;
#52139 = CARTESIAN_POINT('Ctrl Pts',(181.924081156149,535.993184569906,-49.3593342322741)) ;
#52140 = CARTESIAN_POINT('Ctrl Pts',(181.913082344595,536.063420436168,-49.3554863828943)) ;
#52141 = CARTESIAN_POINT('Ctrl Pts',(181.898527821528,536.132908506928,-49.3517278271686)) ;
#52142 = CARTESIAN_POINT('Ctrl Pts',(181.883972033896,536.202402615143,-49.3479689448817)) ;
#52143 = CARTESIAN_POINT('Ctrl Pts',(181.865859822924,536.271148727557,-49.3442992991325)) ;
#52144 = CARTESIAN_POINT('Ctrl Pts',(181.844287389052,536.33875934524,-49.340699365354)) ;
#52145 = CARTESIAN_POINT('Ctrl Pts',(181.822690028396,536.406448086481,-49.3370952718792)) ;
#52146 = CARTESIAN_POINT('Ctrl Pts',(181.797624237622,536.472998575918,-49.3335608658333)) ;
#52147 = CARTESIAN_POINT('Ctrl Pts',(181.769223963578,536.538028362011,-49.3300541262992)) ;
#52148 = CARTESIAN_POINT('Ctrl Pts',(181.740806087874,536.603098451665,-49.3265452133903)) ;
#52149 = CARTESIAN_POINT('Ctrl Pts',(181.709049279655,536.666645717014,-49.3230636557219)) ;
#52150 = CARTESIAN_POINT('Ctrl Pts',(181.674129078134,536.72829607859,-49.3195488526866)) ;
#52151 = CARTESIAN_POINT('Ctrl Pts',(181.641232218846,536.786374302125,-49.3162377039577)) ;
#52152 = CARTESIAN_POINT('Ctrl Pts',(181.605527529697,536.842769255252,-49.3128965589948)) ;
#52153 = CARTESIAN_POINT('Ctrl Pts',(181.567200958708,536.897178224159,-49.309464902831)) ;
#52154 = CARTESIAN_POINT('Ctrl Pts',(181.564766879856,536.900633678617,-49.3092469620792)) ;
#52155 = CARTESIAN_POINT('Ctrl Pts',(181.562322224758,536.904081140274,-49.3090286562612)) ;
#52156 = CARTESIAN_POINT('Ctrl Pts',(181.559867040392,536.907520538678,-49.3088099698756)) ;
#52157 = CARTESIAN_POINT('Ctrl Pts',(181.533655540383,536.944239488394,-49.3064752783248)) ;
#52158 = CARTESIAN_POINT('Ctrl Pts',(181.506245088415,536.980037446018,-49.3040969780512)) ;
#52159 = CARTESIAN_POINT('Ctrl Pts',(181.477704697016,537.01482513965,-49.3016555691048)) ;
#52160 = CARTESIAN_POINT('Ctrl Pts',(181.477682537963,537.014852149172,-49.3016536735699)) ;
#52161 = CARTESIAN_POINT('Ctrl Pts',(181.47766037823,537.014879158086,-49.3016517779969)) ;
#52162 = CARTESIAN_POINT('Ctrl Pts',(181.477638217815,537.014906166391,-49.3016498823858)) ;
#52163 = CARTESIAN_POINT('Ctrl Pts',(181.436814508576,537.064660614799,-49.2981578054215)) ;
#52164 = CARTESIAN_POINT('Ctrl Pts',(181.393521978287,537.112529155155,-49.2945273176486)) ;
#52165 = CARTESIAN_POINT('Ctrl Pts',(181.347981718345,537.158282002969,-49.2908235105092)) ;
#52166 = CARTESIAN_POINT('Ctrl Pts',(181.343365148449,537.162920123616,-49.2904480430753)) ;
#52167 = CARTESIAN_POINT('Ctrl Pts',(181.338725522968,537.167536493735,-49.2900718221704)) ;
#52168 = CARTESIAN_POINT('Ctrl Pts',(181.334063101611,537.172130868916,-49.2896949156048)) ;
#52169 = CARTESIAN_POINT('Ctrl Pts',(181.283485863795,537.221969952159,-49.2856062905021)) ;
#52170 = CARTESIAN_POINT('Ctrl Pts',(181.230220348857,537.269222364421,-49.2814375954658)) ;
#52171 = CARTESIAN_POINT('Ctrl Pts',(181.174586059164,537.31362423241,-49.2772632006393)) ;
#52172 = CARTESIAN_POINT('Ctrl Pts',(181.11902049435,537.357971250897,-49.2730939624307)) ;
#52173 = CARTESIAN_POINT('Ctrl Pts',(181.061092190998,537.399475095859,-49.2689193920925)) ;
#52174 = CARTESIAN_POINT('Ctrl Pts',(181.001136864184,537.43790914616,-49.264794227375)) ;
#52175 = CARTESIAN_POINT('Ctrl Pts',(180.941221589826,537.476317521041,-49.2606718184257)) ;
#52176 = CARTESIAN_POINT('Ctrl Pts',(180.879282064005,537.51166036401,-49.2565989179649)) ;
#52177 = CARTESIAN_POINT('Ctrl Pts',(180.815668928836,537.543744055674,-49.2526069624869)) ;
#52178 = CARTESIAN_POINT('Ctrl Pts',(180.7520769123,537.57581709602,-49.24861633228)) ;
#52179 = CARTESIAN_POINT('Ctrl Pts',(180.686812415575,537.604633163758,-49.2447066336286)) ;
#52180 = CARTESIAN_POINT('Ctrl Pts',(180.620240751481,537.630030069174,-49.2408845573474)) ;
#52181 = CARTESIAN_POINT('Ctrl Pts',(180.553668817217,537.65542707766,-49.2370624655548)) ;
#52182 = CARTESIAN_POINT('Ctrl Pts',(180.485789704087,537.677404786938,-49.2333279321044)) ;
#52183 = CARTESIAN_POINT('Ctrl Pts',(180.416983636269,537.695832968407,-49.2296631161707)) ;
#52184 = CARTESIAN_POINT('Ctrl Pts',(180.348108656542,537.714279606405,-49.2259946297836)) ;
#52185 = CARTESIAN_POINT('Ctrl Pts',(180.278304854469,537.729169363093,-49.2223958222781)) ;
#52186 = CARTESIAN_POINT('Ctrl Pts',(180.207968634237,537.74040625583,-49.2188260103383)) ;
#52187 = CARTESIAN_POINT('Ctrl Pts',(180.137594532266,537.751649200542,-49.2152542757663)) ;
#52188 = CARTESIAN_POINT('Ctrl Pts',(180.066687456419,537.759234954533,-49.2117112303463)) ;
#52189 = CARTESIAN_POINT('Ctrl Pts',(179.995659490086,537.763106735024,-49.2081371490813)) ;
#52190 = CARTESIAN_POINT('Ctrl Pts',(179.928400267569,537.766773078845,-49.2047527085643)) ;
#52191 = CARTESIAN_POINT('Ctrl Pts',(179.861032305697,537.767108839787,-49.201339947582)) ;
#52192 = CARTESIAN_POINT('Ctrl Pts',(179.793918731335,537.764104628672,-49.1978376486995)) ;
#52193 = CARTESIAN_POINT('Ctrl Pts',(179.790036214827,537.763930835227,-49.1976350409058)) ;
#52194 = CARTESIAN_POINT('Ctrl Pts',(179.786154536828,537.763745870956,-49.1974321334632)) ;
#52195 = CARTESIAN_POINT('Ctrl Pts',(179.782273762848,537.763549736425,-49.1972289145198)) ;
#52196 = CARTESIAN_POINT('Ctrl Pts',(179.739287724431,537.76137721967,-49.1949779260948)) ;
#52197 = CARTESIAN_POINT('Ctrl Pts',(179.696414650976,537.757834212928,-49.1926884999008)) ;
#52198 = CARTESIAN_POINT('Ctrl Pts',(179.653751674576,537.752928288526,-49.1903438535763)) ;
#52199 = CARTESIAN_POINT('Ctrl Pts',(179.653718285716,537.752924449056,-49.1903420186113)) ;
#52200 = CARTESIAN_POINT('Ctrl Pts',(179.653684896984,537.752920608751,-49.1903401836125)) ;
#52201 = CARTESIAN_POINT('Ctrl Pts',(179.65365150838,537.752916767612,-49.1903383485799)) ;
#52202 = CARTESIAN_POINT('Ctrl Pts',(179.589356052093,537.745519998755,-49.1868046799592)) ;
#52203 = CARTESIAN_POINT('Ctrl Pts',(179.525317171513,537.734995616538,-49.1831368770369)) ;
#52204 = CARTESIAN_POINT('Ctrl Pts',(179.461851214523,537.721406764875,-49.1793998856796)) ;
#52205 = CARTESIAN_POINT('Ctrl Pts',(179.455650975345,537.720079216462,-49.1790348042829)) ;
#52206 = CARTESIAN_POINT('Ctrl Pts',(179.449456232737,537.718722449947,-49.1786690625444)) ;
#52207 = CARTESIAN_POINT('Ctrl Pts',(179.443267299683,537.717336543757,-49.1783027210199)) ;
#52208 = CARTESIAN_POINT('Ctrl Pts',(179.374199730459,537.701870037523,-49.1742144042798)) ;
#52209 = CARTESIAN_POINT('Ctrl Pts',(179.305851875357,537.682770540929,-49.1700521274263)) ;
#52210 = CARTESIAN_POINT('Ctrl Pts',(179.238611196729,537.660162868676,-49.1658874860574)) ;
#52211 = CARTESIAN_POINT('Ctrl Pts',(179.23503962159,537.658962033083,-49.165666275774)) ;
#52212 = CARTESIAN_POINT('Ctrl Pts',(179.231471179888,537.657751307145,-49.1654450588195)) ;
#52213 = CARTESIAN_POINT('Ctrl Pts',(179.227905932883,537.656530712147,-49.1652238459231)) ;
#52214 = CARTESIAN_POINT('Ctrl Pts',(179.160504656848,537.633455267364,-49.1610417986558)) ;
#52215 = CARTESIAN_POINT('Ctrl Pts',(179.094240989185,537.606850259365,-49.1568614088824)) ;
#52216 = CARTESIAN_POINT('Ctrl Pts',(179.029486970148,537.576877752761,-49.1527351337744)) ;
#52217 = CARTESIAN_POINT('Ctrl Pts',(178.964775922315,537.546925136113,-49.1486115968904)) ;
#52218 = CARTESIAN_POINT('Ctrl Pts',(178.901572425724,537.513609621424,-49.1445422608489)) ;
#52219 = CARTESIAN_POINT('Ctrl Pts',(178.840228975474,537.477123555206,-49.1405561895766)) ;
#52220 = CARTESIAN_POINT('Ctrl Pts',(178.778902241526,537.440647431568,-49.1365712045225)) ;
#52221 = CARTESIAN_POINT('Ctrl Pts',(178.719434543581,537.401002500273,-49.1326694711559)) ;
#52222 = CARTESIAN_POINT('Ctrl Pts',(178.662159968225,537.358410485806,-49.1288553535565)) ;
#52223 = CARTESIAN_POINT('Ctrl Pts',(178.653684781395,537.352107946191,-49.1282909607339)) ;
#52224 = CARTESIAN_POINT('Ctrl Pts',(178.645257583569,537.345740928522,-49.1277284421922)) ;
#52225 = CARTESIAN_POINT('Ctrl Pts',(178.636879422838,537.339310206396,-49.1271677662019)) ;
#52226 = CARTESIAN_POINT('',(180.418697842595,533.725390834864,-49.5221601717598)) ;
#52227 = CARTESIAN_POINT('Ctrl Pts',(180.418697842595,533.725390834864,-49.5221601717598)) ;
#52228 = CARTESIAN_POINT('Ctrl Pts',(180.488838649278,533.744122976537,-49.518223852835)) ;
#52229 = CARTESIAN_POINT('Ctrl Pts',(180.558052648722,533.766594582606,-49.5142875339101)) ;
#52230 = CARTESIAN_POINT('Ctrl Pts',(180.625925910679,533.792690990686,-49.5103512149853)) ;
#52231 = CARTESIAN_POINT('Ctrl Pts',(180.693744619936,533.818766423945,-49.5064180598516)) ;
#52232 = CARTESIAN_POINT('Ctrl Pts',(180.760224305597,533.848460701642,-49.5024849047179)) ;
#52233 = CARTESIAN_POINT('Ctrl Pts',(180.824967594848,533.88160979035,-49.4985517495843)) ;
#52234 = CARTESIAN_POINT('Ctrl Pts',(180.889691398045,533.914748902039,-49.4946197782285)) ;
#52235 = CARTESIAN_POINT('Ctrl Pts',(180.952679430811,533.951340554724,-49.4906878068727)) ;
#52236 = CARTESIAN_POINT('Ctrl Pts',(181.013556689828,533.99117364994,-49.4867558355169)) ;
#52237 = CARTESIAN_POINT('Ctrl Pts',(181.074426964584,534.031002175228,-49.4828243152641)) ;
#52238 = CARTESIAN_POINT('Ctrl Pts',(181.133186561213,534.07407115205,-49.4788927950113)) ;
#52239 = CARTESIAN_POINT('Ctrl Pts',(181.189488680937,534.120125631823,-49.4749612747585)) ;
#52240 = CARTESIAN_POINT('Ctrl Pts',(181.24580026511,534.166187853405,-49.4710290936129)) ;
#52241 = CARTESIAN_POINT('Ctrl Pts',(181.299653194963,534.215236283368,-49.4670969124672)) ;
#52242 = CARTESIAN_POINT('Ctrl Pts',(181.350734142247,534.266975999933,-49.4631647313215)) ;
#52243 = CARTESIAN_POINT('Ctrl Pts',(181.401838125353,534.318739049403,-49.4592307768919)) ;
#52244 = CARTESIAN_POINT('Ctrl Pts',(181.450167318291,534.373195469547,-49.4552968224622)) ;
#52245 = CARTESIAN_POINT('Ctrl Pts',(181.495446588511,534.430014884867,-49.4513628680326)) ;
#52246 = CARTESIAN_POINT('Ctrl Pts',(181.540792862541,534.486918380989,-49.4474230921767)) ;
#52247 = CARTESIAN_POINT('Ctrl Pts',(181.583079917915,534.546191490856,-49.4434833163208)) ;
#52248 = CARTESIAN_POINT('Ctrl Pts',(181.622074419214,534.607472654813,-49.4395435404648)) ;
#52249 = CARTESIAN_POINT('Ctrl Pts',(181.661101355421,534.668804791314,-49.4356004875759)) ;
#52250 = CARTESIAN_POINT('Ctrl Pts',(181.696830057013,534.732147907397,-49.431657434687)) ;
#52251 = CARTESIAN_POINT('Ctrl Pts',(181.72907314629,534.79711579245,-49.4277143817981)) ;
#52252 = CARTESIAN_POINT('Ctrl Pts',(181.76137764778,534.862207419418,-49.423763818723)) ;
#52253 = CARTESIAN_POINT('Ctrl Pts',(181.790183098063,534.928929571959,-49.419813255648)) ;
#52254 = CARTESIAN_POINT('Ctrl Pts',(181.815350386823,534.99687642685,-49.4158626925729)) ;
#52255 = CARTESIAN_POINT('Ctrl Pts',(181.825808223044,535.025110579802,-49.4142211036828)) ;
#52256 = CARTESIAN_POINT('Ctrl Pts',(181.835638465713,535.053556030198,-49.4125795147927)) ;
#52257 = CARTESIAN_POINT('Ctrl Pts',(181.844833710026,535.082183058801,-49.4109379259025)) ;
#52258 = CARTESIAN_POINT('Ctrl Pts',(181.870323447816,535.161538802694,-49.4063873485671)) ;
#52259 = CARTESIAN_POINT('Ctrl Pts',(181.891008381187,535.242533191184,-49.4018367712316)) ;
#52260 = CARTESIAN_POINT('Ctrl Pts',(181.906706975086,535.32462517164,-49.3972861938962)) ;
#52261 = CARTESIAN_POINT('Ctrl Pts',(181.922237610317,535.405838853072,-49.3927843030172)) ;
#52262 = CARTESIAN_POINT('Ctrl Pts',(181.932887947934,535.488126649793,-49.3882824121382)) ;
#52263 = CARTESIAN_POINT('Ctrl Pts',(181.938528448063,535.570943566185,-49.3837805212593)) ;
#52264 = CARTESIAN_POINT('Ctrl Pts',(181.941679434335,535.617208074757,-49.381265603073)) ;
#52265 = CARTESIAN_POINT('Ctrl Pts',(181.943267815266,535.663637337958,-49.3787506848868)) ;
#52266 = CARTESIAN_POINT('Ctrl Pts',(181.943277580094,535.710133636274,-49.3762357667005)) ;
#52267 = CARTESIAN_POINT('',(179.355529476285,533.723981678234,-49.5209531416429)) ;
#52268 = CARTESIAN_POINT('Origin',(179.888527625407,535.710565160536,-49.5221601717598)) ;
#52269 = CARTESIAN_POINT('Ctrl Pts',(179.35615550176,533.725980195244,-49.5197367207334)) ;
#52270 = CARTESIAN_POINT('Ctrl Pts',(179.386645754433,533.717801074244,-49.5180294859388)) ;
#52271 = CARTESIAN_POINT('Ctrl Pts',(179.417322303353,533.710325199925,-49.5163621213256)) ;
#52272 = CARTESIAN_POINT('Ctrl Pts',(179.622903662318,533.665217608102,-49.5054480379446)) ;
#52273 = CARTESIAN_POINT('Ctrl Pts',(179.801923802628,533.649856959711,-49.4971291703748)) ;
#52274 = CARTESIAN_POINT('Ctrl Pts',(180.047717573492,533.660892458951,-49.485012096855)) ;
#52275 = CARTESIAN_POINT('Ctrl Pts',(180.114555802346,533.667183176172,-49.4816539730302)) ;
#52276 = CARTESIAN_POINT('Ctrl Pts',(180.23424793227,533.684393154191,-49.4754314008979)) ;
#52277 = CARTESIAN_POINT('Ctrl Pts',(180.287207316818,533.694145231136,-49.472603422141)) ;
#52278 = CARTESIAN_POINT('Ctrl Pts',(180.390698302709,533.717438814379,-49.4668972475788)) ;
#52279 = CARTESIAN_POINT('Ctrl Pts',(180.441216797588,533.730852555527,-49.4640251044105)) ;
#52280 = CARTESIAN_POINT('Ctrl Pts',(180.65792497081,533.797334656294,-49.4513013214398)) ;
#52281 = CARTESIAN_POINT('Ctrl Pts',(180.81746876098,533.869513342516,-49.4408032426431)) ;
#52282 = CARTESIAN_POINT('Ctrl Pts',(181.037110801698,534.004769463289,-49.4253764557488)) ;
#52283 = CARTESIAN_POINT('Ctrl Pts',(181.105540710678,534.052897009306,-49.4204246101205)) ;
#52284 = CARTESIAN_POINT('Ctrl Pts',(181.195790796679,534.124980360512,-49.4138717576755)) ;
#52285 = CARTESIAN_POINT('Ctrl Pts',(181.220262775655,534.145477956014,-49.41209288984)) ;
#52286 = CARTESIAN_POINT('Ctrl Pts',(181.269176698201,534.188426483131,-49.4085509733121)) ;
#52287 = CARTESIAN_POINT('Ctrl Pts',(181.293572257131,534.210915908282,-49.4067913841307)) ;
#52288 = CARTESIAN_POINT('Ctrl Pts',(181.413278697187,534.326756018982,-49.3981294082487)) ;
#52289 = CARTESIAN_POINT('Ctrl Pts',(181.499892092085,534.428650202827,-49.3917554730396)) ;
#52290 = CARTESIAN_POINT('Ctrl Pts',(181.623697003062,534.606858943087,-49.3812561991762)) ;
#52291 = CARTESIAN_POINT('Ctrl Pts',(181.667140637198,534.678327334671,-49.3771939039362)) ;
#52292 = CARTESIAN_POINT('Ctrl Pts',(181.736988274943,534.810801955952,-49.369689875594)) ;
#52293 = CARTESIAN_POINT('Ctrl Pts',(181.76501496088,534.870818336318,-49.3662998245454)) ;
#52294 = CARTESIAN_POINT('Ctrl Pts',(181.808861072802,534.977918947993,-49.3601970782553)) ;
#52295 = CARTESIAN_POINT('Ctrl Pts',(181.825962549433,535.024419149913,-49.3575312027147)) ;
#52296 = CARTESIAN_POINT('Ctrl Pts',(181.86132212056,535.132468189636,-49.3512810088282)) ;
#52297 = CARTESIAN_POINT('Ctrl Pts',(181.878408942312,535.194343014748,-49.3476608654176)) ;
#52298 = CARTESIAN_POINT('Ctrl Pts',(181.924965648381,535.400010234328,-49.3354964877004)) ;
#52299 = CARTESIAN_POINT('Ctrl Pts',(181.941935976674,535.546157336872,-49.326610785419)) ;
#52300 = CARTESIAN_POINT('Ctrl Pts',(181.943858047043,535.768996053101,-49.3133059277999)) ;
#52301 = CARTESIAN_POINT('Ctrl Pts',(181.940280670191,535.845133634881,-49.308812340963)) ;
#52302 = CARTESIAN_POINT('Ctrl Pts',(181.929263808215,535.952190298597,-49.3027147707102)) ;
#52303 = CARTESIAN_POINT('Ctrl Pts',(181.925325785789,535.983402940241,-49.3009641218704)) ;
#52304 = CARTESIAN_POINT('Ctrl Pts',(181.915727075197,536.047577823389,-49.2974378479214)) ;
#52305 = CARTESIAN_POINT('Ctrl Pts',(181.909975421435,536.080516829146,-49.2956673991572)) ;
#52306 = CARTESIAN_POINT('Ctrl Pts',(181.895615113128,536.15236137623,-49.2918641429117)) ;
#52307 = CARTESIAN_POINT('Ctrl Pts',(181.886673590913,536.191186753956,-49.2898467372816)) ;
#52308 = CARTESIAN_POINT('Ctrl Pts',(181.854447986343,536.314591035259,-49.2834880027757)) ;
#52309 = CARTESIAN_POINT('Ctrl Pts',(181.82687567018,536.397950309466,-49.2792712225611)) ;
#52310 = CARTESIAN_POINT('Ctrl Pts',(181.747185681869,536.595486203075,-49.2689783750769)) ;
#52311 = CARTESIAN_POINT('Ctrl Pts',(181.689785794362,536.707139456508,-49.26288796729)) ;
#52312 = CARTESIAN_POINT('Ctrl Pts',(181.594309382983,536.857336006462,-49.2537261138182)) ;
#52313 = CARTESIAN_POINT('Ctrl Pts',(181.564339655096,536.900703029251,-49.250956476311)) ;
#52314 = CARTESIAN_POINT('Ctrl Pts',(181.501853638212,536.984075525302,-49.2453503902744)) ;
#52315 = CARTESIAN_POINT('Ctrl Pts',(181.469433382929,537.024104568198,-49.2425189484251)) ;
#52316 = CARTESIAN_POINT('Ctrl Pts',(181.368551378238,537.1395120866,-49.2339115252726)) ;
#52317 = CARTESIAN_POINT('Ctrl Pts',(181.29596259545,537.211059055025,-49.2279652371632)) ;
#52318 = CARTESIAN_POINT('Ctrl Pts',(181.115758623106,537.364053576331,-49.2138677783475)) ;
#52319 = CARTESIAN_POINT('Ctrl Pts',(181.004824180477,537.440883735331,-49.2056485411836)) ;
#52320 = CARTESIAN_POINT('Ctrl Pts',(180.849733588312,537.527132198193,-49.1953182933574)) ;
#52321 = CARTESIAN_POINT('Ctrl Pts',(180.811650056526,537.546778170894,-49.1928681465783)) ;
#52322 = CARTESIAN_POINT('Ctrl Pts',(180.74705806749,537.577580865455,-49.1888888216884)) ;
#52323 = CARTESIAN_POINT('Ctrl Pts',(180.720884240904,537.589395861228,-49.1873250373415)) ;
#52324 = CARTESIAN_POINT('Ctrl Pts',(180.65272788296,537.6184578222,-49.1833730240811)) ;
#52325 = CARTESIAN_POINT('Ctrl Pts',(180.610407892758,537.634869168835,-49.1810299284733)) ;
#52326 = CARTESIAN_POINT('Ctrl Pts',(180.507305367133,537.67097063546,-49.1755073434259)) ;
#52327 = CARTESIAN_POINT('Ctrl Pts',(180.446080180925,537.689254498746,-49.1723782979835)) ;
#52328 = CARTESIAN_POINT('Ctrl Pts',(180.223772643284,537.744502436524,-49.1612495035639)) ;
#52329 = CARTESIAN_POINT('Ctrl Pts',(180.059239454266,537.764864176168,-49.1533859499329)) ;
#52330 = CARTESIAN_POINT('Ctrl Pts',(179.841632287978,537.765448490495,-49.1421589582639)) ;
#52331 = CARTESIAN_POINT('Ctrl Pts',(179.789237030738,537.763583764509,-49.1393986005986)) ;
#52332 = CARTESIAN_POINT('Ctrl Pts',(179.684831578572,537.755861986112,-49.1337552721455)) ;
#52333 = CARTESIAN_POINT('Ctrl Pts',(179.632859975274,537.750017176451,-49.1308747110985)) ;
#52334 = CARTESIAN_POINT('Ctrl Pts',(179.468617674125,537.725169679011,-49.1215274928822)) ;
#52335 = CARTESIAN_POINT('Ctrl Pts',(179.357688670585,537.698820597104,-49.1148350393141)) ;
#52336 = CARTESIAN_POINT('Ctrl Pts',(179.115814682438,537.619676163128,-49.0995968615698)) ;
#52337 = CARTESIAN_POINT('Ctrl Pts',(178.98694741049,537.562306659906,-49.091019789403)) ;
#52338 = CARTESIAN_POINT('Ctrl Pts',(178.836039648971,537.475608581037,-49.0810857387213)) ;
#52339 = CARTESIAN_POINT('Ctrl Pts',(178.80753618604,537.458297124332,-49.0792162124116)) ;
#52340 = CARTESIAN_POINT('Ctrl Pts',(178.757341218784,537.426113339013,-49.0759540762785)) ;
#52341 = CARTESIAN_POINT('Ctrl Pts',(178.735491174142,537.411504682479,-49.0745453838288)) ;
#52342 = CARTESIAN_POINT('Ctrl Pts',(178.687662906414,537.378182055663,-49.0714736136423)) ;
#52343 = CARTESIAN_POINT('Ctrl Pts',(178.66183693877,537.359277489613,-49.0698228176136)) ;
#52344 = CARTESIAN_POINT('Ctrl Pts',(178.63645405003,537.339770280938,-49.0681970943831)) ;
#52345 = CARTESIAN_POINT('Origin',(29.8885276254157,585.710565160562,-48.522160171753)) ;
#52346 = CARTESIAN_POINT('',(31.4521967054837,586.286174104269,-47.6539767957637)) ;
#52347 = CARTESIAN_POINT('',(31.4519519036773,586.286117526679,-47.522160171753)) ;
#52348 = CARTESIAN_POINT('',(31.4519519036773,586.286117526679,-48.5221601717531)) ;
#52349 = CARTESIAN_POINT('',(29.9644663285049,587.375713641869,-47.5221677112006)) ;
#52350 = CARTESIAN_POINT('Origin',(29.8885276254157,585.710565160562,-47.522160171753)) ;
#52351 = CARTESIAN_POINT('Ctrl Pts',(29.9644663292412,587.375713658016,-47.5221677113392)) ;
#52352 = CARTESIAN_POINT('Ctrl Pts',(30.0172117431049,587.373277266171,-47.5257729693611)) ;
#52353 = CARTESIAN_POINT('Ctrl Pts',(30.0699288534817,587.368272470247,-47.5294752834428)) ;
#52354 = CARTESIAN_POINT('Ctrl Pts',(30.1223497103767,587.360732154157,-47.5332205362781)) ;
#52355 = CARTESIAN_POINT('Ctrl Pts',(30.1822042172788,587.352122567664,-47.537496892579)) ;
#52356 = CARTESIAN_POINT('Ctrl Pts',(30.2416737256479,587.340207082712,-47.5418286678001)) ;
#52357 = CARTESIAN_POINT('Ctrl Pts',(30.3003811691045,587.325072957424,-47.5461497278178)) ;
#52358 = CARTESIAN_POINT('Ctrl Pts',(30.3590287596007,587.309954261563,-47.5504663824616)) ;
#52359 = CARTESIAN_POINT('Ctrl Pts',(30.4169159760224,587.291623764065,-47.5547720457429)) ;
#52360 = CARTESIAN_POINT('Ctrl Pts',(30.4736830094216,587.270203172543,-47.559021543743)) ;
#52361 = CARTESIAN_POINT('Ctrl Pts',(30.5304137076198,587.248796291821,-47.5632683217425)) ;
#52362 = CARTESIAN_POINT('Ctrl Pts',(30.5860257065395,587.224303361531,-47.5674588881871)) ;
#52363 = CARTESIAN_POINT('Ctrl Pts',(30.640174533252,587.196877873331,-47.5715719488526)) ;
#52364 = CARTESIAN_POINT('Ctrl Pts',(30.6943092455541,587.169459533846,-47.5756839374094)) ;
#52365 = CARTESIAN_POINT('Ctrl Pts',(30.7469814967011,587.139110137708,-47.5797184700438)) ;
#52366 = CARTESIAN_POINT('Ctrl Pts',(30.7978617422621,587.106014648331,-47.5836788440787)) ;
#52367 = CARTESIAN_POINT('Ctrl Pts',(30.8487848475891,587.072891280453,-47.5876425541962)) ;
#52368 = CARTESIAN_POINT('Ctrl Pts',(30.8979127734843,587.037017070334,-47.5915321047031)) ;
#52369 = CARTESIAN_POINT('Ctrl Pts',(30.9449313656306,586.998610227493,-47.5953744366989)) ;
#52370 = CARTESIAN_POINT('Ctrl Pts',(30.9919676158759,586.960188960745,-47.5992182117043)) ;
#52371 = CARTESIAN_POINT('Ctrl Pts',(31.0368926718298,586.919232960551,-47.6030150058583)) ;
#52372 = CARTESIAN_POINT('Ctrl Pts',(31.0794114305104,586.875995869049,-47.6068124945089)) ;
#52373 = CARTESIAN_POINT('Ctrl Pts',(31.1220109466605,586.832676655721,-47.6106171958718)) ;
#52374 = CARTESIAN_POINT('Ctrl Pts',(31.1621945398082,586.787067423539,-47.6144230682816)) ;
#52375 = CARTESIAN_POINT('Ctrl Pts',(31.1996904671793,586.739462053043,-47.6182932968595)) ;
#52376 = CARTESIAN_POINT('Ctrl Pts',(31.2333844159271,586.696683729475,-47.6217710954496)) ;
#52377 = CARTESIAN_POINT('Ctrl Pts',(31.2649083917971,586.652293270558,-47.6253014502317)) ;
#52378 = CARTESIAN_POINT('Ctrl Pts',(31.2940874544249,586.606534862519,-47.6289347067773)) ;
#52379 = CARTESIAN_POINT('Ctrl Pts',(31.2967009856576,586.602436340572,-47.6292601329083)) ;
#52380 = CARTESIAN_POINT('Ctrl Pts',(31.2992957374993,586.598326833112,-47.6295863845744)) ;
#52381 = CARTESIAN_POINT('Ctrl Pts',(31.3018716034924,586.594206508618,-47.6299134979525)) ;
#52382 = CARTESIAN_POINT('Ctrl Pts',(31.3018890076405,586.59417866915,-47.6299157081333)) ;
#52383 = CARTESIAN_POINT('Ctrl Pts',(31.3019064109265,586.594150829189,-47.6299179183535)) ;
#52384 = CARTESIAN_POINT('Ctrl Pts',(31.3019238133503,586.594122988734,-47.629920128613)) ;
#52385 = CARTESIAN_POINT('Ctrl Pts',(31.331784986765,586.546350984788,-47.6337127579626)) ;
#52386 = CARTESIAN_POINT('Ctrl Pts',(31.3592023676582,586.496958448299,-47.6376306020833)) ;
#52387 = CARTESIAN_POINT('Ctrl Pts',(31.3840375644497,586.44622538852,-47.6416083928178)) ;
#52388 = CARTESIAN_POINT('Ctrl Pts',(31.3866785765017,586.440830358899,-47.6420313970467)) ;
#52389 = CARTESIAN_POINT('Ctrl Pts',(31.3892903905504,586.43542021845,-47.6424550791829)) ;
#52390 = CARTESIAN_POINT('Ctrl Pts',(31.391872843012,586.429995338376,-47.642879360737)) ;
#52391 = CARTESIAN_POINT('Ctrl Pts',(31.4142029661715,586.383087121489,-47.6465480669371)) ;
#52392 = CARTESIAN_POINT('Ctrl Pts',(31.4343386697815,586.335072588071,-47.6502614936775)) ;
#52393 = CARTESIAN_POINT('Ctrl Pts',(31.4521967054837,586.286174104269,-47.6539767957637)) ;
#52394 = CARTESIAN_POINT('Origin',(29.8885276254157,585.710565160562,-48.522160171753)) ;
#52395 = CARTESIAN_POINT('',(31.4519519011282,586.286117533603,-48.355726152802)) ;
#52396 = CARTESIAN_POINT('',(31.4519307013587,586.286106548708,-48.1612775350459)) ;
#52397 = CARTESIAN_POINT('',(31.4519519036773,586.286117526679,-48.5221601717531)) ;
#52398 = CARTESIAN_POINT('',(31.5236569526671,585.391334705933,-47.522160171753)) ;
#52399 = CARTESIAN_POINT('Ctrl Pts',(31.4519307013587,586.286106548708,-48.1612775350459)) ;
#52400 = CARTESIAN_POINT('Ctrl Pts',(31.4307799415804,586.343123822471,-48.1569517643851)) ;
#52401 = CARTESIAN_POINT('Ctrl Pts',(31.4064967643115,586.399036969702,-48.1526486462426)) ;
#52402 = CARTESIAN_POINT('Ctrl Pts',(31.3792408298284,586.453499502786,-48.1484091084437)) ;
#52403 = CARTESIAN_POINT('Ctrl Pts',(31.3519986288077,586.507934593803,-48.144171706823)) ;
#52404 = CARTESIAN_POINT('Ctrl Pts',(31.3217867261071,586.560920578791,-48.1399979131416)) ;
#52405 = CARTESIAN_POINT('Ctrl Pts',(31.2887947141343,586.612128861891,-48.1359042980891)) ;
#52406 = CARTESIAN_POINT('Ctrl Pts',(31.2558070590083,586.663330382545,-48.1318112236296)) ;
#52407 = CARTESIAN_POINT('Ctrl Pts',(31.2200399857983,586.712754605879,-48.1277982748074)) ;
#52408 = CARTESIAN_POINT('Ctrl Pts',(31.1817130950373,586.760090581968,-48.1238572931125)) ;
#52409 = CARTESIAN_POINT('Ctrl Pts',(31.1433492593098,586.807472187274,-48.1199125125329)) ;
#52410 = CARTESIAN_POINT('Ctrl Pts',(31.1024205399601,586.852761339475,-48.11603968801)) ;
#52411 = CARTESIAN_POINT('Ctrl Pts',(31.059178620734,586.895665555711,-48.1122072045106)) ;
#52412 = CARTESIAN_POINT('Ctrl Pts',(31.0159161277447,586.938590185037,-48.1083728975813)) ;
#52413 = CARTESIAN_POINT('Ctrl Pts',(30.9703380380091,586.979127289515,-48.1045786603127)) ;
#52414 = CARTESIAN_POINT('Ctrl Pts',(30.9227303036629,587.017007018988,-48.1007727915254)) ;
#52415 = CARTESIAN_POINT('Ctrl Pts',(30.8750327440127,587.054958219163,-48.0969597419024)) ;
#52416 = CARTESIAN_POINT('Ctrl Pts',(30.825297653982,587.090241462823,-48.0931344909291)) ;
#52417 = CARTESIAN_POINT('Ctrl Pts',(30.7738498578355,587.12261490586,-48.0892311392184)) ;
#52418 = CARTESIAN_POINT('Ctrl Pts',(30.7324088206022,587.148691611934,-48.0860870017491)) ;
#52419 = CARTESIAN_POINT('Ctrl Pts',(30.6898572447864,587.172880722555,-48.0828917299347)) ;
#52420 = CARTESIAN_POINT('Ctrl Pts',(30.6463835469031,587.195074223284,-48.0796086475328)) ;
#52421 = CARTESIAN_POINT('Ctrl Pts',(30.6463569495885,587.195087801322,-48.079606638935)) ;
#52422 = CARTESIAN_POINT('Ctrl Pts',(30.6463303519284,587.195101378614,-48.0796046303043)) ;
#52423 = CARTESIAN_POINT('Ctrl Pts',(30.6463037539227,587.19511495516,-48.0796026216407)) ;
#52424 = CARTESIAN_POINT('Ctrl Pts',(30.5969598112004,587.22030181766,-48.0758762001295)) ;
#52425 = CARTESIAN_POINT('Ctrl Pts',(30.5462426003204,587.243005533324,-48.0720268035916)) ;
#52426 = CARTESIAN_POINT('Ctrl Pts',(30.4944371047044,587.263110400219,-48.0681175601719)) ;
#52427 = CARTESIAN_POINT('Ctrl Pts',(30.4895940946485,587.264989893338,-48.0677521065657)) ;
#52428 = CARTESIAN_POINT('Ctrl Pts',(30.48474161048,587.266846682069,-48.0673861299368)) ;
#52429 = CARTESIAN_POINT('Ctrl Pts',(30.4798799075965,587.268680677295,-48.0670196818603)) ;
#52430 = CARTESIAN_POINT('Ctrl Pts',(30.4223039395851,587.290400237913,-48.0626799261751)) ;
#52431 = CARTESIAN_POINT('Ctrl Pts',(30.3634290732152,587.308922130295,-48.0582747193363)) ;
#52432 = CARTESIAN_POINT('Ctrl Pts',(30.3036482873888,587.324138482308,-48.0538756019817)) ;
#52433 = CARTESIAN_POINT('Ctrl Pts',(30.2447665225575,587.339126001264,-48.0495426413161)) ;
#52434 = CARTESIAN_POINT('Ctrl Pts',(30.1850058966653,587.350907103944,-48.045215873412)) ;
#52435 = CARTESIAN_POINT('Ctrl Pts',(30.1247435266456,587.359417808461,-48.040943152075)) ;
#52436 = CARTESIAN_POINT('Ctrl Pts',(30.0645180032693,587.367923309218,-48.036673043238)) ;
#52437 = CARTESIAN_POINT('Ctrl Pts',(30.0037913375607,587.373162539151,-48.0324570503659)) ;
#52438 = CARTESIAN_POINT('Ctrl Pts',(29.9429416361881,587.375106883817,-48.0283191850485)) ;
#52439 = CARTESIAN_POINT('Ctrl Pts',(29.8821064426302,587.377050764912,-48.024182306283)) ;
#52440 = CARTESIAN_POINT('Ctrl Pts',(29.8211482924624,587.375701301232,-48.0201235209901)) ;
#52441 = CARTESIAN_POINT('Ctrl Pts',(29.7604466594093,587.371064453128,-48.0161420673551)) ;
#52442 = CARTESIAN_POINT('Ctrl Pts',(29.6980479193189,587.366297967202,-48.0120492995323)) ;
#52443 = CARTESIAN_POINT('Ctrl Pts',(29.6359203077301,587.358057352657,-48.0080382404948)) ;
#52444 = CARTESIAN_POINT('Ctrl Pts',(29.5744771200985,587.346388751218,-48.0040817200879)) ;
#52445 = CARTESIAN_POINT('Ctrl Pts',(29.514627676142,587.335022815711,-48.0002278258568)) ;
#52446 = CARTESIAN_POINT('Ctrl Pts',(29.4554277481429,587.320404294539,-47.9964253109212)) ;
#52447 = CARTESIAN_POINT('Ctrl Pts',(29.3972588143385,587.302615983661,-47.9926275534585)) ;
#52448 = CARTESIAN_POINT('Ctrl Pts',(29.3367663910192,587.284117139666,-47.9886780990492)) ;
#52449 = CARTESIAN_POINT('Ctrl Pts',(29.2773893147356,587.262189397615,-47.9847333742759)) ;
#52450 = CARTESIAN_POINT('Ctrl Pts',(29.2195525913832,587.236977680796,-47.980722871614)) ;
#52451 = CARTESIAN_POINT('Ctrl Pts',(29.1694833278862,587.215151892275,-47.9772509786211)) ;
#52452 = CARTESIAN_POINT('Ctrl Pts',(29.1205675372531,587.190864738412,-47.9737291323648)) ;
#52453 = CARTESIAN_POINT('Ctrl Pts',(29.0730774892506,587.164249422843,-47.9701065357073)) ;
#52454 = CARTESIAN_POINT('Ctrl Pts',(29.0657368158185,587.160135416897,-47.9695465805134)) ;
#52455 = CARTESIAN_POINT('Ctrl Pts',(29.0584301072712,587.155965801168,-47.9689842181129)) ;
#52456 = CARTESIAN_POINT('Ctrl Pts',(29.0511582586619,587.15174108262,-47.9684192609029)) ;
#52457 = CARTESIAN_POINT('Ctrl Pts',(29.051131846989,587.151725738257,-47.9684172089536)) ;
#52458 = CARTESIAN_POINT('Ctrl Pts',(29.0511054357758,587.151710393167,-47.96841515697)) ;
#52459 = CARTESIAN_POINT('Ctrl Pts',(29.0510790250225,587.15169504735,-47.9684131049522)) ;
#52460 = CARTESIAN_POINT('Ctrl Pts',(29.0030794916229,587.123805193757,-47.9646837187795)) ;
#52461 = CARTESIAN_POINT('Ctrl Pts',(28.9564309626375,587.093407305578,-47.9608314366137)) ;
#52462 = CARTESIAN_POINT('Ctrl Pts',(28.9113857090435,587.060679387765,-47.9569193612993)) ;
#52463 = CARTESIAN_POINT('Ctrl Pts',(28.9071765430953,587.057621191258,-47.9565538050445)) ;
#52464 = CARTESIAN_POINT('Ctrl Pts',(28.9029813896465,587.054542684994,-47.9561877266996)) ;
#52465 = CARTESIAN_POINT('Ctrl Pts',(28.8988004622044,587.051444036078,-47.9558211777507)) ;
#52466 = CARTESIAN_POINT('Ctrl Pts',(28.8493826163757,587.01481853694,-47.9514886319951)) ;
#52467 = CARTESIAN_POINT('Ctrl Pts',(28.8019497425696,586.975373500213,-47.9470909996863)) ;
#52468 = CARTESIAN_POINT('Ctrl Pts',(28.7568040004953,586.933380274201,-47.9426992373383)) ;
#52469 = CARTESIAN_POINT('Ctrl Pts',(28.7122319909216,586.89192071709,-47.9383632874918)) ;
#52470 = CARTESIAN_POINT('Ctrl Pts',(28.6698889901391,586.84797757195,-47.9340333518222)) ;
#52471 = CARTESIAN_POINT('Ctrl Pts',(28.6300337605279,586.801834383049,-47.9297571682477)) ;
#52472 = CARTESIAN_POINT('Ctrl Pts',(28.5902028650029,586.755719367423,-47.925483595548)) ;
#52473 = CARTESIAN_POINT('Ctrl Pts',(28.5528565856751,586.707407050929,-47.9212638443896)) ;
#52474 = CARTESIAN_POINT('Ctrl Pts',(28.5182244800743,586.657200914689,-47.9171217491355)) ;
#52475 = CARTESIAN_POINT('Ctrl Pts',(28.4836007390349,586.607006904549,-47.9129806543059)) ;
#52476 = CARTESIAN_POINT('Ctrl Pts',(28.4516898961422,586.554919985649,-47.9089171797078)) ;
#52477 = CARTESIAN_POINT('Ctrl Pts',(28.4226932061505,586.501263517939,-47.9049303377222)) ;
#52478 = CARTESIAN_POINT('Ctrl Pts',(28.3930074424623,586.446331964673,-47.9008487529248)) ;
#52479 = CARTESIAN_POINT('Ctrl Pts',(28.3663762908088,586.389755253745,-47.8968474592338)) ;
#52480 = CARTESIAN_POINT('Ctrl Pts',(28.3429834443105,586.331902521544,-47.8928994043826)) ;
#52481 = CARTESIAN_POINT('Ctrl Pts',(28.320104812319,586.27532149068,-47.8890381344841)) ;
#52482 = CARTESIAN_POINT('Ctrl Pts',(28.300323889067,586.217519948497,-47.8852274348512)) ;
#52483 = CARTESIAN_POINT('Ctrl Pts',(28.2837785816813,586.158864668577,-47.8814205514702)) ;
#52484 = CARTESIAN_POINT('Ctrl Pts',(28.2666754719051,586.098231906186,-47.8774853242271)) ;
#52485 = CARTESIAN_POINT('Ctrl Pts',(28.2530306485098,586.036686735904,-47.8735537450999)) ;
#52486 = CARTESIAN_POINT('Ctrl Pts',(28.2429516138147,585.974658674776,-47.8695565520771)) ;
#52487 = CARTESIAN_POINT('Ctrl Pts',(28.2341794744453,585.920673465528,-47.8660776540136)) ;
#52488 = CARTESIAN_POINT('Ctrl Pts',(28.2281080884414,585.866321616251,-47.862548405409)) ;
#52489 = CARTESIAN_POINT('Ctrl Pts',(28.2247736387295,585.811904521213,-47.8589182141461)) ;
#52490 = CARTESIAN_POINT('Ctrl Pts',(28.2242788682371,585.803830033596,-47.8583795610927)) ;
#52491 = CARTESIAN_POINT('Ctrl Pts',(28.223844294058,585.795754040162,-47.8578386855792)) ;
#52492 = CARTESIAN_POINT('Ctrl Pts',(28.2234699704405,585.787677451147,-47.857295422325)) ;
#52493 = CARTESIAN_POINT('Ctrl Pts',(28.2234684541509,585.787644734943,-47.857293221704)) ;
#52494 = CARTESIAN_POINT('Ctrl Pts',(28.2234669388499,585.787612018729,-47.8572910210438)) ;
#52495 = CARTESIAN_POINT('Ctrl Pts',(28.2234654245374,585.787579302505,-47.8572888203444)) ;
#52496 = CARTESIAN_POINT('Ctrl Pts',(28.2208975126388,585.732100408197,-47.8535569602791)) ;
#52497 = CARTESIAN_POINT('Ctrl Pts',(28.2211715555489,585.6763966939,-47.8497027637132)) ;
#52498 = CARTESIAN_POINT('Ctrl Pts',(28.2242746982778,585.62077759501,-47.8457897027703)) ;
#52499 = CARTESIAN_POINT('Ctrl Pts',(28.224556744825,585.615722340975,-47.8454340422595)) ;
#52500 = CARTESIAN_POINT('Ctrl Pts',(28.2248621419837,585.610667814763,-47.8450778954639)) ;
#52501 = CARTESIAN_POINT('Ctrl Pts',(28.2251908671879,585.605614265628,-47.8447213100422)) ;
#52502 = CARTESIAN_POINT('Ctrl Pts',(28.2291850993401,585.544210247373,-47.8403885575222)) ;
#52503 = CARTESIAN_POINT('Ctrl Pts',(28.2366266261737,585.482945411913,-47.8359917090826)) ;
#52504 = CARTESIAN_POINT('Ctrl Pts',(28.2474511325718,585.422221922197,-47.8316017875513)) ;
#52505 = CARTESIAN_POINT('Ctrl Pts',(28.2581147419081,585.3624010354,-47.827277118462)) ;
#52506 = CARTESIAN_POINT('Ctrl Pts',(28.2720610984026,585.303105348989,-47.8229594508306)) ;
#52507 = CARTESIAN_POINT('Ctrl Pts',(28.2891925640849,585.244704728804,-47.818695940337)) ;
#52508 = CARTESIAN_POINT('Ctrl Pts',(28.3063140801705,585.186338026478,-47.8144349060011)) ;
#52509 = CARTESIAN_POINT('Ctrl Pts',(28.3266168980108,585.128865287691,-47.8102280971683)) ;
#52510 = CARTESIAN_POINT('Ctrl Pts',(28.3499707951118,585.072642760978,-47.8060986683029)) ;
#52511 = CARTESIAN_POINT('Ctrl Pts',(28.3733198454859,585.01643190235,-47.8019700964341)) ;
#52512 = CARTESIAN_POINT('Ctrl Pts',(28.3997187320752,584.961470768536,-47.7979188721716)) ;
#52513 = CARTESIAN_POINT('Ctrl Pts',(28.4290051501343,584.908102651446,-47.7939432696954)) ;
#52514 = CARTESIAN_POINT('Ctrl Pts',(28.4590986110284,584.853263874598,-47.7898581119473)) ;
#52515 = CARTESIAN_POINT('Ctrl Pts',(28.4922412383819,584.800107328767,-47.7858527879754)) ;
#52516 = CARTESIAN_POINT('Ctrl Pts',(28.5282203181192,584.748990154992,-47.7818990589373)) ;
#52517 = CARTESIAN_POINT('Ctrl Pts',(28.563282523068,584.699175628429,-47.7780460849631)) ;
#52518 = CARTESIAN_POINT('Ctrl Pts',(28.6010385236517,584.651298038033,-47.7742417386034)) ;
#52519 = CARTESIAN_POINT('Ctrl Pts',(28.6412549150907,584.605670911219,-47.7704383928721)) ;
#52520 = CARTESIAN_POINT('Ctrl Pts',(28.683048791265,584.558254064007,-47.7664858612089)) ;
#52521 = CARTESIAN_POINT('Ctrl Pts',(28.7275004729346,584.513268348445,-47.7625339815812)) ;
#52522 = CARTESIAN_POINT('Ctrl Pts',(28.7743022676147,584.471040595246,-47.7585114229537)) ;
#52523 = CARTESIAN_POINT('Ctrl Pts',(28.8146927457334,584.434597566655,-47.7550399093646)) ;
#52524 = CARTESIAN_POINT('Ctrl Pts',(28.8568341583957,584.400207859665,-47.7515150920462)) ;
#52525 = CARTESIAN_POINT('Ctrl Pts',(28.9004946041224,584.368062445012,-47.7478863622271)) ;
#52526 = CARTESIAN_POINT('Ctrl Pts',(28.9073968524377,584.362980599638,-47.7473126989522)) ;
#52527 = CARTESIAN_POINT('Ctrl Pts',(28.9143370917191,584.357954741647,-47.7467364386732)) ;
#52528 = CARTESIAN_POINT('Ctrl Pts',(28.9213144393905,584.352985510748,-47.7461573814348)) ;
#52529 = CARTESIAN_POINT('Ctrl Pts',(28.9213428665735,584.352965265055,-47.7461550222338)) ;
#52530 = CARTESIAN_POINT('Ctrl Pts',(28.9213712943725,584.352945020302,-47.7461526629863)) ;
#52531 = CARTESIAN_POINT('Ctrl Pts',(28.9213997227874,584.352924776489,-47.7461503036923)) ;
#52532 = CARTESIAN_POINT('Ctrl Pts',(28.966188167755,584.321031021641,-47.7424332794709)) ;
#52533 = CARTESIAN_POINT('Ctrl Pts',(29.012678507572,584.291357561665,-47.7385907161729)) ;
#52534 = CARTESIAN_POINT('Ctrl Pts',(29.0606107579876,584.264058947249,-47.7346854302868)) ;
#52535 = CARTESIAN_POINT('Ctrl Pts',(29.0652818423194,584.261398647994,-47.7343048531272)) ;
#52536 = CARTESIAN_POINT('Ctrl Pts',(29.0699665795344,584.258760899231,-47.7339236803004)) ;
#52537 = CARTESIAN_POINT('Ctrl Pts',(29.0746647027699,584.256145841362,-47.733541969942)) ;
#52538 = CARTESIAN_POINT('Ctrl Pts',(29.1284270591468,584.226220770002,-47.7291739175751)) ;
#52539 = CARTESIAN_POINT('Ctrl Pts',(29.183948470999,584.199267172114,-47.7247361715027)) ;
#52540 = CARTESIAN_POINT('Ctrl Pts',(29.2408544318338,584.175450784657,-47.7203020289527)) ;
#52541 = CARTESIAN_POINT('Ctrl Pts',(29.29669672858,584.152079563851,-47.7159507676707)) ;
#52542 = CARTESIAN_POINT('Ctrl Pts',(29.3538722052045,584.131728897117,-47.7116032602347)) ;
#52543 = CARTESIAN_POINT('Ctrl Pts',(29.4120195720763,584.114516711758,-47.7073085328236)) ;
#52544 = CARTESIAN_POINT('Ctrl Pts',(29.4701302786454,584.097315378204,-47.7030165131192)) ;
#52545 = CARTESIAN_POINT('Ctrl Pts',(29.5292116364245,584.083248435898,-47.6987773495737)) ;
#52546 = CARTESIAN_POINT('Ctrl Pts',(29.5888962456398,584.072398855542,-47.6946164046111)) ;
#52547 = CARTESIAN_POINT('Ctrl Pts',(29.648565919294,584.0615519902,-47.6904565008893)) ;
#52548 = CARTESIAN_POINT('Ctrl Pts',(29.7088385196163,584.053920903689,-47.686374787176)) ;
#52549 = CARTESIAN_POINT('Ctrl Pts',(29.7693403765114,584.049554530518,-47.6823719266044)) ;
#52550 = CARTESIAN_POINT('Ctrl Pts',(29.8319369391989,584.045036984016,-47.6782304782992)) ;
#52551 = CARTESIAN_POINT('Ctrl Pts',(29.8947788908135,584.044014527707,-47.6741734692833)) ;
#52552 = CARTESIAN_POINT('Ctrl Pts',(29.9574456165983,584.046501475673,-47.6701746338271)) ;
#52553 = CARTESIAN_POINT('Ctrl Pts',(30.0180948327723,584.048908358159,-47.666304537967)) ;
#52554 = CARTESIAN_POINT('Ctrl Pts',(30.078579797218,584.054602405714,-47.662488549878)) ;
#52555 = CARTESIAN_POINT('Ctrl Pts',(30.1385141518014,584.063556938655,-47.6586810573511)) ;
#52556 = CARTESIAN_POINT('Ctrl Pts',(30.2014391007573,584.072958283379,-47.6546835792007)) ;
#52557 = CARTESIAN_POINT('Ctrl Pts',(30.2637569006503,584.085954563593,-47.6506950903516)) ;
#52558 = CARTESIAN_POINT('Ctrl Pts',(30.3250171285409,584.102461888914,-47.6466435972635)) ;
#52559 = CARTESIAN_POINT('Ctrl Pts',(30.3778105795844,584.116687736601,-47.6431520610848)) ;
#52560 = CARTESIAN_POINT('Ctrl Pts',(30.4298195954929,584.133521283782,-47.6396130697671)) ;
#52561 = CARTESIAN_POINT('Ctrl Pts',(30.4807536481331,584.15286909452,-47.6359748345754)) ;
#52562 = CARTESIAN_POINT('Ctrl Pts',(30.4889046723152,584.155965342806,-47.6353926043878)) ;
#52563 = CARTESIAN_POINT('Ctrl Pts',(30.4970282706236,584.159125949638,-47.6348078325743)) ;
#52564 = CARTESIAN_POINT('Ctrl Pts',(30.5051233723068,584.162350499438,-47.6342203068854)) ;
#52565 = CARTESIAN_POINT('Ctrl Pts',(30.5051408025854,584.162357442501,-47.6342190418319)) ;
#52566 = CARTESIAN_POINT('Ctrl Pts',(30.5051582327318,584.16236438586,-47.6342177767657)) ;
#52567 = CARTESIAN_POINT('Ctrl Pts',(30.5051756627462,584.162371329516,-47.6342165116867)) ;
#52568 = CARTESIAN_POINT('Ctrl Pts',(30.5573892114869,584.183171823977,-47.630426826679)) ;
#52569 = CARTESIAN_POINT('Ctrl Pts',(30.6085975773506,584.206713047159,-47.626512651755)) ;
#52570 = CARTESIAN_POINT('Ctrl Pts',(30.6585215269897,584.2328521311,-47.6225363273908)) ;
#52571 = CARTESIAN_POINT('Ctrl Pts',(30.6635495891892,584.235484714076,-47.6221358541436)) ;
#52572 = CARTESIAN_POINT('Ctrl Pts',(30.6685646018945,584.238143610051,-47.6217347504899)) ;
#52573 = CARTESIAN_POINT('Ctrl Pts',(30.6735662663411,584.240828647163,-47.6213330801159)) ;
#52574 = CARTESIAN_POINT('Ctrl Pts',(30.7281138703226,584.27011136747,-47.6169525070642)) ;
#52575 = CARTESIAN_POINT('Ctrl Pts',(30.7810772240688,584.302508244197,-47.6125051654418)) ;
#52576 = CARTESIAN_POINT('Ctrl Pts',(30.832118315781,584.337794643179,-47.60806028493)) ;
#52577 = CARTESIAN_POINT('Ctrl Pts',(30.8830961268198,584.373037294134,-47.6036209151749)) ;
#52578 = CARTESIAN_POINT('Ctrl Pts',(30.9321567446921,584.411162079793,-47.5991843410106)) ;
#52579 = CARTESIAN_POINT('Ctrl Pts',(30.9789917031901,584.451918727176,-47.5947989528455)) ;
#52580 = CARTESIAN_POINT('Ctrl Pts',(31.0257833074872,584.49263764693,-47.5904176241481)) ;
#52581 = CARTESIAN_POINT('Ctrl Pts',(31.070353511841,584.535983515777,-47.5860875232072)) ;
#52582 = CARTESIAN_POINT('Ctrl Pts',(31.112419599329,584.581682212606,-47.5818328533529)) ;
#52583 = CARTESIAN_POINT('Ctrl Pts',(31.1544599489697,584.627352949001,-47.5775807866892)) ;
#52584 = CARTESIAN_POINT('Ctrl Pts',(31.1939992242414,584.675373687706,-47.5734040517902)) ;
#52585 = CARTESIAN_POINT('Ctrl Pts',(31.2307792211875,584.725446151378,-47.5693018382)) ;
#52586 = CARTESIAN_POINT('Ctrl Pts',(31.2675624397705,584.775523001001,-47.5651992652882)) ;
#52587 = CARTESIAN_POINT('Ctrl Pts',(31.3015857225035,584.827652045966,-47.5611710924071)) ;
#52588 = CARTESIAN_POINT('Ctrl Pts',(31.332616267389,584.881509006654,-47.5571925755217)) ;
#52589 = CARTESIAN_POINT('Ctrl Pts',(31.3636455912645,584.935363848142,-47.5532142151856)) ;
#52590 = CARTESIAN_POINT('Ctrl Pts',(31.3916820678538,584.990946608284,-47.5492852144427)) ;
#52591 = CARTESIAN_POINT('Ctrl Pts',(31.416522243606,585.047905215767,-47.5453600602187)) ;
#52592 = CARTESIAN_POINT('Ctrl Pts',(31.4413870439082,585.104920287427,-47.5414310149129)) ;
#52593 = CARTESIAN_POINT('Ctrl Pts',(31.4630486289947,585.163314038115,-47.5375053197114)) ;
#52594 = CARTESIAN_POINT('Ctrl Pts',(31.4813391707566,585.222703536039,-47.5335224252991)) ;
#52595 = CARTESIAN_POINT('Ctrl Pts',(31.4984177883923,585.278157909114,-47.529803435909)) ;
#52596 = CARTESIAN_POINT('Ctrl Pts',(31.5125570804919,585.334480084893,-47.5260339239252)) ;
#52597 = CARTESIAN_POINT('Ctrl Pts',(31.523656952667,585.391334705933,-47.522160171753)) ;
#52598 = CARTESIAN_POINT('Origin',(29.8885276254157,585.710565160562,-47.522160171753)) ;
#52599 = CARTESIAN_POINT('Ctrl Pts',(31.4519518985791,586.286117540527,-48.355726152802)) ;
#52600 = CARTESIAN_POINT('Ctrl Pts',(31.4434820923154,586.30912483085,-48.3540957748191)) ;
#52601 = CARTESIAN_POINT('Ctrl Pts',(31.4345047739506,586.331944217182,-48.3524484063256)) ;
#52602 = CARTESIAN_POINT('Ctrl Pts',(31.3977455599149,586.419647652667,-48.3459926605691)) ;
#52603 = CARTESIAN_POINT('Ctrl Pts',(31.3663605758364,586.482927804222,-48.3410625763967)) ;
#52604 = CARTESIAN_POINT('Ctrl Pts',(31.2785534651235,586.63490332075,-48.328535319917)) ;
#52605 = CARTESIAN_POINT('Ctrl Pts',(31.2175745308427,586.720616863932,-48.3208259901791)) ;
#52606 = CARTESIAN_POINT('Ctrl Pts',(31.1122495956988,586.842470426917,-48.3091819134654)) ;
#52607 = CARTESIAN_POINT('Ctrl Pts',(31.0734280608116,586.883048528962,-48.3051714342576)) ;
#52608 = CARTESIAN_POINT('Ctrl Pts',(31.0107179042492,586.942293027323,-48.2991977981767)) ;
#52609 = CARTESIAN_POINT('Ctrl Pts',(30.9882475352005,586.962396315996,-48.2971492841245)) ;
#52610 = CARTESIAN_POINT('Ctrl Pts',(30.9328771429415,587.009290909575,-48.2923306471091)) ;
#52611 = CARTESIAN_POINT('Ctrl Pts',(30.8994771595535,587.035456204803,-48.2896004631163)) ;
#52612 = CARTESIAN_POINT('Ctrl Pts',(30.815785738447,587.096009165938,-48.2830759481163)) ;
#52613 = CARTESIAN_POINT('Ctrl Pts',(30.7645373235593,587.128969438512,-48.2793399671403)) ;
#52614 = CARTESIAN_POINT('Ctrl Pts',(30.6050431270322,587.219598301561,-48.268127635221)) ;
#52615 = CARTESIAN_POINT('Ctrl Pts',(30.4921467594447,587.26819662629,-48.2607012196546)) ;
#52616 = CARTESIAN_POINT('Ctrl Pts',(30.3256890081963,587.319011110516,-48.2495284044689)) ;
#52617 = CARTESIAN_POINT('Ctrl Pts',(30.2757654955829,587.33175432779,-48.2461559803733)) ;
#52618 = CARTESIAN_POINT('Ctrl Pts',(30.1687055260016,587.353854555756,-48.2388306597564)) ;
#52619 = CARTESIAN_POINT('Ctrl Pts',(30.1115115655679,587.362587079098,-48.2348619921694)) ;
#52620 = CARTESIAN_POINT('Ctrl Pts',(29.9858394415985,587.375130120162,-48.2260048679559)) ;
#52621 = CARTESIAN_POINT('Ctrl Pts',(29.9173459661159,587.377722585799,-48.2210890939331)) ;
#52622 = CARTESIAN_POINT('Ctrl Pts',(29.7352369839165,587.373389001206,-48.2078743745191)) ;
#52623 = CARTESIAN_POINT('Ctrl Pts',(29.6221505526748,587.35905760391,-48.1995036984888)) ;
#52624 = CARTESIAN_POINT('Ctrl Pts',(29.4802874975646,587.326088693546,-48.1893377525639)) ;
#52625 = CARTESIAN_POINT('Ctrl Pts',(29.4493846048396,587.317963778217,-48.1871464048208)) ;
#52626 = CARTESIAN_POINT('Ctrl Pts',(29.3834550593428,587.298585781513,-48.1825469955573)) ;
#52627 = CARTESIAN_POINT('Ctrl Pts',(29.3485297743631,587.287051967299,-48.1801540135514)) ;
#52628 = CARTESIAN_POINT('Ctrl Pts',(29.2153641266709,587.238129118544,-48.1710955704189)) ;
#52629 = CARTESIAN_POINT('Ctrl Pts',(29.1203571942751,587.192631114113,-48.1647620970404)) ;
#52630 = CARTESIAN_POINT('Ctrl Pts',(28.9502432465714,587.090382174046,-48.1526245190228)) ;
#52631 = CARTESIAN_POINT('Ctrl Pts',(28.8744171500099,587.035649869731,-48.1468612904288)) ;
#52632 = CARTESIAN_POINT('Ctrl Pts',(28.7653265369692,586.942034221644,-48.1376049626789)) ;
#52633 = CARTESIAN_POINT('Ctrl Pts',(28.7285879982721,586.907492844215,-48.1342947388423)) ;
#52634 = CARTESIAN_POINT('Ctrl Pts',(28.6520689312175,586.828714286352,-48.1269183641127)) ;
#52635 = CARTESIAN_POINT('Ctrl Pts',(28.6129790806541,586.783906639688,-48.1228277465482)) ;
#52636 = CARTESIAN_POINT('Ctrl Pts',(28.5318026543341,586.680144856249,-48.1135611775892)) ;
#52637 = CARTESIAN_POINT('Ctrl Pts',(28.4909969376601,586.620341792121,-48.108350738309)) ;
#52638 = CARTESIAN_POINT('Ctrl Pts',(28.398980177153,586.464614810847,-48.0952056364894)) ;
#52639 = CARTESIAN_POINT('Ctrl Pts',(28.3530159852892,586.365965819127,-48.0872350874343)) ;
#52640 = CARTESIAN_POINT('Ctrl Pts',(28.3066817501423,586.234284057102,-48.0775251205083)) ;
#52641 = CARTESIAN_POINT('Ctrl Pts',(28.2972052233884,586.204742757341,-48.075405885814)) ;
#52642 = CARTESIAN_POINT('Ctrl Pts',(28.2777097233127,586.137573634432,-48.0707402797996)) ;
#52643 = CARTESIAN_POINT('Ctrl Pts',(28.26817368348,586.099826346297,-48.0682187418209)) ;
#52644 = CARTESIAN_POINT('Ctrl Pts',(28.2488926753565,586.010420568848,-48.0624052876878)) ;
#52645 = CARTESIAN_POINT('Ctrl Pts',(28.2402520817229,585.958566265076,-48.0591552791752)) ;
#52646 = CARTESIAN_POINT('Ctrl Pts',(28.2180236567539,585.770763684508,-48.0475533311717)) ;
#52647 = CARTESIAN_POINT('Ctrl Pts',(28.2187086349124,585.633694396307,-48.0393524164731)) ;
#52648 = CARTESIAN_POINT('Ctrl Pts',(28.2427019025735,585.44696022208,-48.0272773716683)) ;
#52649 = CARTESIAN_POINT('Ctrl Pts',(28.2516753408951,585.396012303652,-48.0238945161476)) ;
#52650 = CARTESIAN_POINT('Ctrl Pts',(28.275567948487,585.289605813336,-48.0165927403749)) ;
#52651 = CARTESIAN_POINT('Ctrl Pts',(28.2910137821265,585.23433642384,-48.012660232188)) ;
#52652 = CARTESIAN_POINT('Ctrl Pts',(28.3307370662613,585.116103024297,-48.0039221943929)) ;
#52653 = CARTESIAN_POINT('Ctrl Pts',(28.3560510063055,585.053594533359,-47.9990913492981)) ;
#52654 = CARTESIAN_POINT('Ctrl Pts',(28.4356104065225,584.886948200739,-47.9857054012247)) ;
#52655 = CARTESIAN_POINT('Ctrl Pts',(28.4971821595587,584.786728527473,-47.9770612025327)) ;
#52656 = CARTESIAN_POINT('Ctrl Pts',(28.5880558327149,584.668774692363,-47.9666824044219)) ;
#52657 = CARTESIAN_POINT('Ctrl Pts',(28.6080493415936,584.644295841396,-47.9645182147761)) ;
#52658 = CARTESIAN_POINT('Ctrl Pts',(28.6533595746993,584.591935417487,-47.9598898545011)) ;
#52659 = CARTESIAN_POINT('Ctrl Pts',(28.6789483862941,584.564314205919,-47.957444546878)) ;
#52660 = CARTESIAN_POINT('Ctrl Pts',(28.7404506589192,584.502282894467,-47.9518769547255)) ;
#52661 = CARTESIAN_POINT('Ctrl Pts',(28.7770125723721,584.468566065907,-47.9487913869087)) ;
#52662 = CARTESIAN_POINT('Ctrl Pts',(28.9300296203272,584.339634161256,-47.936488708907)) ;
#52663 = CARTESIAN_POINT('Ctrl Pts',(29.0576059344332,584.25876059873,-47.9274946523805)) ;
#52664 = CARTESIAN_POINT('Ctrl Pts',(29.2401925518158,584.175063157958,-47.9145226693446)) ;
#52665 = CARTESIAN_POINT('Ctrl Pts',(29.2870135986645,584.156124838573,-47.9111964579189)) ;
#52666 = CARTESIAN_POINT('Ctrl Pts',(29.3930438224229,584.118745574372,-47.9036212642135)) ;
#52667 = CARTESIAN_POINT('Ctrl Pts',(29.4525652720331,584.101425986229,-47.8993394303105)) ;
#52668 = CARTESIAN_POINT('Ctrl Pts',(29.6704561507284,584.051001330273,-47.8835425147065)) ;
#52669 = CARTESIAN_POINT('Ctrl Pts',(29.8324466201678,584.037678042522,-47.871471761408)) ;
#52670 = CARTESIAN_POINT('Ctrl Pts',(30.0297368999949,584.050169926224,-47.857532286556)) ;
#52671 = CARTESIAN_POINT('Ctrl Pts',(30.0655909462358,584.053609670541,-47.8550353021252)) ;
#52672 = CARTESIAN_POINT('Ctrl Pts',(30.1333240279881,584.0623319556,-47.8504214657627)) ;
#52673 = CARTESIAN_POINT('Ctrl Pts',(30.165214136751,584.067384476811,-47.8482954856133)) ;
#52674 = CARTESIAN_POINT('Ctrl Pts',(30.235039137753,584.080537890546,-47.8437040606502)) ;
#52675 = CARTESIAN_POINT('Ctrl Pts',(30.2728800108991,584.08904339965,-47.8412572218737)) ;
#52676 = CARTESIAN_POINT('Ctrl Pts',(30.400986006455,584.122575253693,-47.833010927125)) ;
#52677 = CARTESIAN_POINT('Ctrl Pts',(30.4894222289005,584.153885137202,-47.8273739750085)) ;
#52678 = CARTESIAN_POINT('Ctrl Pts',(30.6495351696288,584.226261624706,-47.8165814671852)) ;
#52679 = CARTESIAN_POINT('Ctrl Pts',(30.7217000115368,584.265535491428,-47.811468224425)) ;
#52680 = CARTESIAN_POINT('Ctrl Pts',(30.8327702045291,584.337077130835,-47.8029241742964)) ;
#52681 = CARTESIAN_POINT('Ctrl Pts',(30.8736191757821,584.366073755343,-47.799620470658)) ;
#52682 = CARTESIAN_POINT('Ctrl Pts',(30.9624623585322,584.43536345828,-47.7920193414021)) ;
#52683 = CARTESIAN_POINT('Ctrl Pts',(31.0096117297751,584.476610613006,-47.7876853302185)) ;
#52684 = CARTESIAN_POINT('Ctrl Pts',(31.1407662981794,584.605080633558,-47.7746958260141)) ;
#52685 = CARTESIAN_POINT('Ctrl Pts',(31.217720517408,584.6989139922,-47.7657921836445)) ;
#52686 = CARTESIAN_POINT('Ctrl Pts',(31.3145920495733,584.847392708989,-47.7529620027299)) ;
#52687 = CARTESIAN_POINT('Ctrl Pts',(31.3429517098784,584.896084763225,-47.748933560168)) ;
#52688 = CARTESIAN_POINT('Ctrl Pts',(31.3826562844653,584.972968817756,-47.7429361312224)) ;
#52689 = CARTESIAN_POINT('Ctrl Pts',(31.3957877698077,585.000187637959,-47.7408811769365)) ;
#52690 = CARTESIAN_POINT('Ctrl Pts',(31.4256401872173,585.066626463372,-47.7360395404856)) ;
#52691 = CARTESIAN_POINT('Ctrl Pts',(31.4416100700602,585.106158218874,-47.7332930325006)) ;
#52692 = CARTESIAN_POINT('Ctrl Pts',(31.4767960265537,585.203897847987,-47.7267233752158)) ;
#52693 = CARTESIAN_POINT('Ctrl Pts',(31.4943513299144,585.26263715905,-47.722958663885)) ;
#52694 = CARTESIAN_POINT('Ctrl Pts',(31.5368042679642,585.439739969753,-47.7118059565235)) ;
#52695 = CARTESIAN_POINT('Ctrl Pts',(31.5521019910453,585.559969909567,-47.7044627376934)) ;
#52696 = CARTESIAN_POINT('Ctrl Pts',(31.5551863622036,585.732531768951,-47.6933701959639)) ;
#52697 = CARTESIAN_POINT('Ctrl Pts',(31.5536999385663,585.78428131776,-47.6899780448717)) ;
#52698 = CARTESIAN_POINT('Ctrl Pts',(31.5454131947141,585.894143126491,-47.6825877391369)) ;
#52699 = CARTESIAN_POINT('Ctrl Pts',(31.5379559238235,585.952133936346,-47.6785727010562)) ;
#52700 = CARTESIAN_POINT('Ctrl Pts',(31.5102876804173,586.103773434535,-47.6677499481555)) ;
#52701 = CARTESIAN_POINT('Ctrl Pts',(31.4850246340391,586.196272217906,-47.6608060977828)) ;
#52702 = CARTESIAN_POINT('Ctrl Pts',(31.4519662334624,586.286078599909,-47.653833696077)) ;
#52703 = CARTESIAN_POINT('Origin',(29.8885276254157,585.710565160562,-48.522160171753)) ;
#52704 = CARTESIAN_POINT('',(31.4519519036772,586.286117526679,-49.0537704297649)) ;
#52705 = CARTESIAN_POINT('',(31.4519519037552,586.286117526467,-48.8631174034081)) ;
#52706 = CARTESIAN_POINT('',(31.4519519036773,586.286117526679,-48.5221601717531)) ;
#52707 = CARTESIAN_POINT('',(31.5549951295688,585.711651406811,-49.0928293408672)) ;
#52708 = CARTESIAN_POINT('Ctrl Pts',(31.5545272840244,585.711631704242,-49.0925609297511)) ;
#52709 = CARTESIAN_POINT('Ctrl Pts',(31.5544977221009,585.757809048348,-49.0892228343914)) ;
#52710 = CARTESIAN_POINT('Ctrl Pts',(31.5525482815855,585.803968862486,-49.0859127753278)) ;
#52711 = CARTESIAN_POINT('Ctrl Pts',(31.5460913158,585.880852396666,-49.080499904251)) ;
#52712 = CARTESIAN_POINT('Ctrl Pts',(31.5426392122963,585.911638093734,-49.0783597445402)) ;
#52713 = CARTESIAN_POINT('Ctrl Pts',(31.5338748303722,585.974031563823,-49.0741012708764)) ;
#52714 = CARTESIAN_POINT('Ctrl Pts',(31.5285053045551,586.005616576846,-49.0719902830301)) ;
#52715 = CARTESIAN_POINT('Ctrl Pts',(31.5052725851344,586.121878570276,-49.0643251078782)) ;
#52716 = CARTESIAN_POINT('Ctrl Pts',(31.481757603648,586.20515364275,-49.0590354631716)) ;
#52717 = CARTESIAN_POINT('Ctrl Pts',(31.4519519036772,586.286117526679,-49.0537704297648)) ;
#52718 = CARTESIAN_POINT('',(28.6194567455633,586.789923813611,-49.5221601717529)) ;
#52719 = CARTESIAN_POINT('Ctrl Pts',(31.5549951295688,585.711651406811,-49.0928293408672)) ;
#52720 = CARTESIAN_POINT('Ctrl Pts',(31.5549004634924,585.651788058804,-49.0970785373116)) ;
#52721 = CARTESIAN_POINT('Ctrl Pts',(31.5515533777371,585.591824499677,-49.1013669242796)) ;
#52722 = CARTESIAN_POINT('Ctrl Pts',(31.5449787198106,585.532138025659,-49.1056345435034)) ;
#52723 = CARTESIAN_POINT('Ctrl Pts',(31.5384111864713,585.472516230519,-49.1098975381481)) ;
#52724 = CARTESIAN_POINT('Ctrl Pts',(31.5286233097781,585.413170884277,-49.1141395515163)) ;
#52725 = CARTESIAN_POINT('Ctrl Pts',(31.5156767976258,585.354469497454,-49.1183211131778)) ;
#52726 = CARTESIAN_POINT('Ctrl Pts',(31.5027392387105,585.295808705922,-49.1224997830556)) ;
#52727 = CARTESIAN_POINT('Ctrl Pts',(31.486647481512,585.237791002754,-49.1266179865489)) ;
#52728 = CARTESIAN_POINT('Ctrl Pts',(31.4674977847107,585.180774747157,-49.1306592310771)) ;
#52729 = CARTESIAN_POINT('Ctrl Pts',(31.4483537584412,585.123775374985,-49.1346992789281)) ;
#52730 = CARTESIAN_POINT('Ctrl Pts',(31.426153560656,585.06777695046,-49.1386624357151)) ;
#52731 = CARTESIAN_POINT('Ctrl Pts',(31.4010278693363,585.013128286434,-49.1425556647614)) ;
#52732 = CARTESIAN_POINT('Ctrl Pts',(31.3758819407826,584.958435606193,-49.1464520295697)) ;
#52733 = CARTESIAN_POINT('Ctrl Pts',(31.3478056647439,584.905095035362,-49.1502784917524)) ;
#52734 = CARTESIAN_POINT('Ctrl Pts',(31.3169659821272,584.853444993432,-49.1540643342011)) ;
#52735 = CARTESIAN_POINT('Ctrl Pts',(31.2861148200487,584.801775725796,-49.1578515858547)) ;
#52736 = CARTESIAN_POINT('Ctrl Pts',(31.2524979705717,584.751798528007,-49.1615984774341)) ;
#52737 = CARTESIAN_POINT('Ctrl Pts',(31.216321245005,584.70383758609,-49.1653534658704)) ;
#52738 = CARTESIAN_POINT('Ctrl Pts',(31.1800774948503,584.655787786977,-49.1691154111705)) ;
#52739 = CARTESIAN_POINT('Ctrl Pts',(31.1412640853418,584.609762194078,-49.1728859737232)) ;
#52740 = CARTESIAN_POINT('Ctrl Pts',(31.1001307191771,584.566066556702,-49.1767272898374)) ;
#52741 = CARTESIAN_POINT('Ctrl Pts',(31.0641200442947,584.527812712244,-49.1800902138723)) ;
#52742 = CARTESIAN_POINT('Ctrl Pts',(31.0263318317532,584.491344652427,-49.1835078935255)) ;
#52743 = CARTESIAN_POINT('Ctrl Pts',(30.9869628963889,584.456849398685,-49.1870249440584)) ;
#52744 = CARTESIAN_POINT('Ctrl Pts',(30.9869382635993,584.456827815314,-49.1870271446453)) ;
#52745 = CARTESIAN_POINT('Ctrl Pts',(30.9869136301907,584.456806232714,-49.1870293452712)) ;
#52746 = CARTESIAN_POINT('Ctrl Pts',(30.9868889961631,584.456784650885,-49.187031545936)) ;
#52747 = CARTESIAN_POINT('Ctrl Pts',(30.9451149164525,584.420186451609,-49.1907634060781)) ;
#52748 = CARTESIAN_POINT('Ctrl Pts',(30.9013931355104,584.385670009117,-49.1946176026786)) ;
#52749 = CARTESIAN_POINT('Ctrl Pts',(30.8559735946312,584.3534182028,-49.1985306636151)) ;
#52750 = CARTESIAN_POINT('Ctrl Pts',(30.851845386038,584.350486817291,-49.1988863240086)) ;
#52751 = CARTESIAN_POINT('Ctrl Pts',(30.8477031876204,584.347574141802,-49.1992424706862)) ;
#52752 = CARTESIAN_POINT('Ctrl Pts',(30.8435472083229,584.3446803141,-49.1995990559895)) ;
#52753 = CARTESIAN_POINT('Ctrl Pts',(30.793049249511,584.309518350659,-49.2039318085532)) ;
#52754 = CARTESIAN_POINT('Ctrl Pts',(30.740510754993,584.277138369889,-49.2083286569907)) ;
#52755 = CARTESIAN_POINT('Ctrl Pts',(30.6862862482676,584.247740832729,-49.2127185784724)) ;
#52756 = CARTESIAN_POINT('Ctrl Pts',(30.6328677448689,584.218780266124,-49.2170432473307)) ;
#52757 = CARTESIAN_POINT('Ctrl Pts',(30.5778131003371,584.192713711564,-49.2213609146856)) ;
#52758 = CARTESIAN_POINT('Ctrl Pts',(30.521472363694,584.169695440192,-49.2256244248628)) ;
#52759 = CARTESIAN_POINT('Ctrl Pts',(30.4651643485759,584.146690537352,-49.2298854588822)) ;
#52760 = CARTESIAN_POINT('Ctrl Pts',(30.4075717531272,584.126730253415,-49.2340922673582)) ;
#52761 = CARTESIAN_POINT('Ctrl Pts',(30.349054296051,584.109934893663,-49.23822169583)) ;
#52762 = CARTESIAN_POINT('Ctrl Pts',(30.2905489833374,584.093143019519,-49.2423502673049)) ;
#52763 = CARTESIAN_POINT('Ctrl Pts',(30.231119203068,584.079514793908,-49.2464014911362)) ;
#52764 = CARTESIAN_POINT('Ctrl Pts',(30.1711345470063,584.069137360875,-49.250377093143)) ;
#52765 = CARTESIAN_POINT('Ctrl Pts',(30.1094968953937,584.0584739572,-49.2544622507071)) ;
#52766 = CARTESIAN_POINT('Ctrl Pts',(30.0472733406778,584.051243342123,-49.2584675744432)) ;
#52767 = CARTESIAN_POINT('Ctrl Pts',(29.9848757320995,584.04750188289,-49.2624213031963)) ;
#52768 = CARTESIAN_POINT('Ctrl Pts',(29.9240682407258,584.043855769598,-49.2662742766118)) ;
#52769 = CARTESIAN_POINT('Ctrl Pts',(29.8630955529396,584.043523410377,-49.2700786223735)) ;
#52770 = CARTESIAN_POINT('Ctrl Pts',(29.8023483198256,584.046517803162,-49.2738819674629)) ;
#52771 = CARTESIAN_POINT('Ctrl Pts',(29.7392182745368,584.049629651102,-49.2778344988859)) ;
#52772 = CARTESIAN_POINT('Ctrl Pts',(29.6763318499431,584.056335241496,-49.281786378225)) ;
#52773 = CARTESIAN_POINT('Ctrl Pts',(29.6141364158333,584.066597786271,-49.2858089365303)) ;
#52774 = CARTESIAN_POINT('Ctrl Pts',(29.5604610580425,584.075454477611,-49.2892804495018)) ;
#52775 = CARTESIAN_POINT('Ctrl Pts',(29.5072993619206,584.086960329732,-49.292805266168)) ;
#52776 = CARTESIAN_POINT('Ctrl Pts',(29.4549452226018,584.101053103059,-49.2964339952949)) ;
#52777 = CARTESIAN_POINT('Ctrl Pts',(29.4466685882797,584.103281021098,-49.2970076588949)) ;
#52778 = CARTESIAN_POINT('Ctrl Pts',(29.4384120397071,584.105573549329,-49.2975839195019)) ;
#52779 = CARTESIAN_POINT('Ctrl Pts',(29.4301766273081,584.107930396578,-49.2981629770717)) ;
#52780 = CARTESIAN_POINT('Ctrl Pts',(29.4301430748617,584.107939998767,-49.298165336249)) ;
#52781 = CARTESIAN_POINT('Ctrl Pts',(29.4301095227661,584.107949602025,-49.2981676954727)) ;
#52782 = CARTESIAN_POINT('Ctrl Pts',(29.4300759710213,584.107959206349,-49.2981700547429)) ;
#52783 = CARTESIAN_POINT('Ctrl Pts',(29.377215290868,584.123090793065,-49.3018870783155)) ;
#52784 = CARTESIAN_POINT('Ctrl Pts',(29.3250293931448,584.140937305961,-49.3057296409284)) ;
#52785 = CARTESIAN_POINT('Ctrl Pts',(29.2738012079945,584.161391841912,-49.3096349260873)) ;
#52786 = CARTESIAN_POINT('Ctrl Pts',(29.2688089330185,584.16338517171,-49.3100155028599)) ;
#52787 = CARTESIAN_POINT('Ctrl Pts',(29.2638257762798,584.165403235723,-49.3103966752985)) ;
#52788 = CARTESIAN_POINT('Ctrl Pts',(29.2588520139343,584.167445912848,-49.3107783852673)) ;
#52789 = CARTESIAN_POINT('Ctrl Pts',(29.201935368766,584.190821040376,-49.3151464369237)) ;
#52790 = CARTESIAN_POINT('Ctrl Pts',(29.1462451621245,584.217424136405,-49.3195841822428)) ;
#52791 = CARTESIAN_POINT('Ctrl Pts',(29.0921444734093,584.247065735209,-49.3240183239897)) ;
#52792 = CARTESIAN_POINT('Ctrl Pts',(29.0390550187489,584.276153282025,-49.328369584072)) ;
#52793 = CARTESIAN_POINT('Ctrl Pts',(28.9874959042153,584.308166435024,-49.3327170902622)) ;
#52794 = CARTESIAN_POINT('Ctrl Pts',(28.9377845894302,584.342896253063,-49.3370118163971)) ;
#52795 = CARTESIAN_POINT('Ctrl Pts',(28.8881046161158,584.377604175009,-49.341303834838)) ;
#52796 = CARTESIAN_POINT('Ctrl Pts',(28.840270017296,584.415025243138,-49.3455429970899)) ;
#52797 = CARTESIAN_POINT('Ctrl Pts',(28.7945747320282,584.45492394412,-49.3497039407454)) ;
#52798 = CARTESIAN_POINT('Ctrl Pts',(28.7488908814825,584.49481266091,-49.3538638431724)) ;
#52799 = CARTESIAN_POINT('Ctrl Pts',(28.7053453092586,584.537177769595,-49.3579455555769)) ;
#52800 = CARTESIAN_POINT('Ctrl Pts',(28.66420925332,584.581757633295,-49.361948414843)) ;
#52801 = CARTESIAN_POINT('Ctrl Pts',(28.6216489710894,584.627880955952,-49.3660898624418)) ;
#52802 = CARTESIAN_POINT('Ctrl Pts',(28.5816682634495,584.676375284731,-49.3701468707268)) ;
#52803 = CARTESIAN_POINT('Ctrl Pts',(28.5445405706483,584.726920694313,-49.3741457054608)) ;
#52804 = CARTESIAN_POINT('Ctrl Pts',(28.5086081821852,584.775838824018,-49.3780158000512)) ;
#52805 = CARTESIAN_POINT('Ctrl Pts',(28.4753482118881,584.826678049973,-49.3818317868948)) ;
#52806 = CARTESIAN_POINT('Ctrl Pts',(28.4449806910114,584.87911967072,-49.3856392782212)) ;
#52807 = CARTESIAN_POINT('Ctrl Pts',(28.4130978897292,584.934178026652,-49.3896367559816)) ;
#52808 = CARTESIAN_POINT('Ctrl Pts',(28.3844042744588,584.9910031002,-49.393625244486)) ;
#52809 = CARTESIAN_POINT('Ctrl Pts',(28.3591150911948,585.049190431488,-49.3976767373463)) ;
#52810 = CARTESIAN_POINT('Ctrl Pts',(28.3373211325259,585.099335676587,-49.4011682723248)) ;
#52811 = CARTESIAN_POINT('Ctrl Pts',(28.3180550420476,585.150493499069,-49.4047072625028)) ;
#52812 = CARTESIAN_POINT('Ctrl Pts',(28.3014249098296,585.202378498608,-49.4083454966198)) ;
#52813 = CARTESIAN_POINT('Ctrl Pts',(28.2987635686985,585.210681720828,-49.4089277278356)) ;
#52814 = CARTESIAN_POINT('Ctrl Pts',(28.2961696451147,585.219003627598,-49.4095125006894)) ;
#52815 = CARTESIAN_POINT('Ctrl Pts',(28.2936434817717,585.227343122656,-49.4101000274321)) ;
#52816 = CARTESIAN_POINT('Ctrl Pts',(28.2936380424176,585.22736107932,-49.4101012924991)) ;
#52817 = CARTESIAN_POINT('Ctrl Pts',(28.2936326033777,585.227379036065,-49.4101025575789)) ;
#52818 = CARTESIAN_POINT('Ctrl Pts',(28.2936271646519,585.227396992892,-49.4101038226715)) ;
#52819 = CARTESIAN_POINT('Ctrl Pts',(28.277335033442,585.281188082002,-49.4138935070696)) ;
#52820 = CARTESIAN_POINT('Ctrl Pts',(28.2638124112331,585.335902103654,-49.4178076815085)) ;
#52821 = CARTESIAN_POINT('Ctrl Pts',(28.2531216984605,585.391231667786,-49.4217840055249)) ;
#52822 = CARTESIAN_POINT('Ctrl Pts',(28.2520449872732,585.396804164396,-49.4221844795292)) ;
#52823 = CARTESIAN_POINT('Ctrl Pts',(28.2509969847544,585.402382864411,-49.4225855839438)) ;
#52824 = CARTESIAN_POINT('Ctrl Pts',(28.249977742813,585.40796742709,-49.4229872550822)) ;
#52825 = CARTESIAN_POINT('Ctrl Pts',(28.2388620219692,585.468871945688,-49.4273678285887)) ;
#52826 = CARTESIAN_POINT('Ctrl Pts',(28.2311688113756,585.53047949232,-49.4318151708419)) ;
#52827 = CARTESIAN_POINT('Ctrl Pts',(28.2269332318505,585.592385741501,-49.4362600521213)) ;
#52828 = CARTESIAN_POINT('Ctrl Pts',(28.2227029035984,585.65421523929,-49.4406994226351)) ;
#52829 = CARTESIAN_POINT('Ctrl Pts',(28.2219212701929,585.716342796566,-49.4451359976939)) ;
#52830 = CARTESIAN_POINT('Ctrl Pts',(28.2245849858367,585.778371201992,-49.4495213868474)) ;
#52831 = CARTESIAN_POINT('Ctrl Pts',(28.2272462357256,585.840342188806,-49.4539027165228)) ;
#52832 = CARTESIAN_POINT('Ctrl Pts',(28.2333463380861,585.902214290954,-49.458232818535)) ;
#52833 = CARTESIAN_POINT('Ctrl Pts',(28.242847247488,585.963595559647,-49.4624874895138)) ;
#52834 = CARTESIAN_POINT('Ctrl Pts',(28.252342343799,586.024939272474,-49.4667395572903)) ;
#52835 = CARTESIAN_POINT('Ctrl Pts',(28.2652341409681,586.085792768793,-49.4709162933552)) ;
#52836 = CARTESIAN_POINT('Ctrl Pts',(28.2814504238792,586.145768203664,-49.4750185081275)) ;
#52837 = CARTESIAN_POINT('Ctrl Pts',(28.2976681271212,586.205748891586,-49.4791210821994)) ;
#52838 = CARTESIAN_POINT('Ctrl Pts',(28.3172110937834,586.264851297271,-49.4831492562576)) ;
#52839 = CARTESIAN_POINT('Ctrl Pts',(28.3399709414953,586.322691223682,-49.4871277743043)) ;
#52840 = CARTESIAN_POINT('Ctrl Pts',(28.3627298935716,586.380528874002,-49.4911061357901)) ;
#52841 = CARTESIAN_POINT('Ctrl Pts',(28.3887057972037,586.437103961319,-49.4950351376672)) ;
#52842 = CARTESIAN_POINT('Ctrl Pts',(28.417750243145,586.492037906295,-49.4989602929812)) ;
#52843 = CARTESIAN_POINT('Ctrl Pts',(28.4468234812195,586.547026307999,-49.5028893393523)) ;
#52844 = CARTESIAN_POINT('Ctrl Pts',(28.4789717865111,586.600369927032,-49.5068150355747)) ;
#52845 = CARTESIAN_POINT('Ctrl Pts',(28.5140004099809,586.651698795954,-49.5107979309393)) ;
#52846 = CARTESIAN_POINT('Ctrl Pts',(28.5467080078033,586.699626571443,-49.5145169163532)) ;
#52847 = CARTESIAN_POINT('Ctrl Pts',(28.5819267144592,586.745797359943,-49.5182864241681)) ;
#52848 = CARTESIAN_POINT('Ctrl Pts',(28.6194567455635,586.789923813611,-49.5221601717529)) ;
#52849 = CARTESIAN_POINT('',(31.1430459483832,586.808139740278,-49.5221526322664)) ;
#52850 = CARTESIAN_POINT('Origin',(29.8885276254156,585.710565160562,-49.522160171753)) ;
#52851 = CARTESIAN_POINT('',(31.5540518914521,585.711428744506,-48.8998571438181)) ;
#52852 = CARTESIAN_POINT('Ctrl Pts',(31.1430459605378,586.808139750912,-49.5221526321279)) ;
#52853 = CARTESIAN_POINT('Ctrl Pts',(31.1082549275998,586.847858648898,-49.5185473794)) ;
#52854 = CARTESIAN_POINT('Ctrl Pts',(31.0714734883611,586.885954048843,-49.5148450709363)) ;
#52855 = CARTESIAN_POINT('Ctrl Pts',(31.0328944158098,586.922236962595,-49.5110998238165)) ;
#52856 = CARTESIAN_POINT('Ctrl Pts',(30.9888444934954,586.963665110718,-49.5068234679126)) ;
#52857 = CARTESIAN_POINT('Ctrl Pts',(30.9424499583342,587.002731060734,-49.5024916930553)) ;
#52858 = CARTESIAN_POINT('Ctrl Pts',(30.8940141285388,587.039194414828,-49.4981706333717)) ;
#52859 = CARTESIAN_POINT('Ctrl Pts',(30.8456276796615,587.075620594089,-49.493853979061)) ;
#52860 = CARTESIAN_POINT('Ctrl Pts',(30.7952042286405,587.109449763238,-49.4895483160835)) ;
#52861 = CARTESIAN_POINT('Ctrl Pts',(30.743063267547,587.140476495768,-49.485298818357)) ;
#52862 = CARTESIAN_POINT('Ctrl Pts',(30.6909556806126,587.171483368843,-49.4810520406306)) ;
#52863 = CARTESIAN_POINT('Ctrl Pts',(30.6371328205902,587.199691487015,-49.4768614744286)) ;
#52864 = CARTESIAN_POINT('Ctrl Pts',(30.5819294674629,587.224927230988,-49.4727484139713)) ;
#52865 = CARTESIAN_POINT('Ctrl Pts',(30.5267405036143,587.250156397024,-49.4686364256223)) ;
#52866 = CARTESIAN_POINT('Ctrl Pts',(30.4701717770591,587.272414680804,-49.4646018931605)) ;
#52867 = CARTESIAN_POINT('Ctrl Pts',(30.4125733656241,587.291559756921,-49.4606415192554)) ;
#52868 = CARTESIAN_POINT('Ctrl Pts',(30.3549264352746,587.310720960189,-49.4566778092681)) ;
#52869 = CARTESIAN_POINT('Ctrl Pts',(30.2962480859876,587.326763513427,-49.4527882588481)) ;
#52870 = CARTESIAN_POINT('Ctrl Pts',(30.2369047928652,587.339577852312,-49.448945926886)) ;
#52871 = CARTESIAN_POINT('Ctrl Pts',(30.1775392130304,587.352397003695,-49.4451021519142)) ;
#52872 = CARTESIAN_POINT('Ctrl Pts',(30.1175082069774,587.361985176315,-49.4413053577402)) ;
#52873 = CARTESIAN_POINT('Ctrl Pts',(30.057194073834,587.368269792658,-49.4375078690049)) ;
#52874 = CARTESIAN_POINT('Ctrl Pts',(29.996765383819,587.374566345606,-49.4337031675583)) ;
#52875 = CARTESIAN_POINT('Ctrl Pts',(29.9360525884205,587.377546250347,-49.4298972949997)) ;
#52876 = CARTESIAN_POINT('Ctrl Pts',(29.8754548815714,587.377180281353,-49.4260270661981)) ;
#52877 = CARTESIAN_POINT('Ctrl Pts',(29.8210016094304,587.376851420572,-49.4225492675629)) ;
#52878 = CARTESIAN_POINT('Ctrl Pts',(29.7666408751731,587.373820856864,-49.4190189126796)) ;
#52879 = CARTESIAN_POINT('Ctrl Pts',(29.7126726647831,587.368104063971,-49.4153856559798)) ;
#52880 = CARTESIAN_POINT('Ctrl Pts',(29.7078388194358,587.367592020075,-49.4150602310515)) ;
#52881 = CARTESIAN_POINT('Ctrl Pts',(29.7030080940045,587.367058444666,-49.4147339805939)) ;
#52882 = CARTESIAN_POINT('Ctrl Pts',(29.6981806865841,587.366503359557,-49.4144068684306)) ;
#52883 = CARTESIAN_POINT('Ctrl Pts',(29.6981480689928,587.366499608985,-49.4144046582151)) ;
#52884 = CARTESIAN_POINT('Ctrl Pts',(29.698115451553,587.366495857431,-49.4144024479602)) ;
#52885 = CARTESIAN_POINT('Ctrl Pts',(29.6980828342647,587.366492104895,-49.414400237666)) ;
#52886 = CARTESIAN_POINT('Ctrl Pts',(29.6429112083997,587.360144749872,-49.4106615600452)) ;
#52887 = CARTESIAN_POINT('Ctrl Pts',(29.58797454581,587.350956557579,-49.4068004115545)) ;
#52888 = CARTESIAN_POINT('Ctrl Pts',(29.533575462541,587.338989812433,-49.4028798514077)) ;
#52889 = CARTESIAN_POINT('Ctrl Pts',(29.5285116112468,587.337875863185,-49.4025148979493)) ;
#52890 = CARTESIAN_POINT('Ctrl Pts',(29.5234524442729,587.336737863875,-49.4021494296769)) ;
#52891 = CARTESIAN_POINT('Ctrl Pts',(29.5183982213193,587.335575881509,-49.4017834974551)) ;
#52892 = CARTESIAN_POINT('Ctrl Pts',(29.4584472249493,587.321792951626,-49.3974429684558)) ;
#52893 = CARTESIAN_POINT('Ctrl Pts',(29.3991873543754,587.304631710942,-49.3930378230853)) ;
#52894 = CARTESIAN_POINT('Ctrl Pts',(29.3410040316313,587.284219960435,-49.3886388765359)) ;
#52895 = CARTESIAN_POINT('Ctrl Pts',(29.2835610543231,587.264067936352,-49.3842959037578)) ;
#52896 = CARTESIAN_POINT('Ctrl Pts',(29.2271671710291,587.240747966385,-49.3799592650711)) ;
#52897 = CARTESIAN_POINT('Ctrl Pts',(29.1721729220915,587.21441638561,-49.3756765623397)) ;
#52898 = CARTESIAN_POINT('Ctrl Pts',(29.1172118889562,587.188100708764,-49.3713964463043)) ;
#52899 = CARTESIAN_POINT('Ctrl Pts',(29.0636487152697,587.15877715734,-49.3671703361583)) ;
#52900 = CARTESIAN_POINT('Ctrl Pts',(29.0118151758906,587.126632032098,-49.3630219371472)) ;
#52901 = CARTESIAN_POINT('Ctrl Pts',(28.9599938148718,587.094494459397,-49.358874512808)) ;
#52902 = CARTESIAN_POINT('Ctrl Pts',(28.9099013067565,587.059536620886,-49.3548047650706)) ;
#52903 = CARTESIAN_POINT('Ctrl Pts',(28.8618514567854,587.02197437252,-49.3508115819677)) ;
#52904 = CARTESIAN_POINT('Ctrl Pts',(28.8126592671132,586.983519117254,-49.3467234647164)) ;
#52905 = CARTESIAN_POINT('Ctrl Pts',(28.7656082490994,586.942333905959,-49.3427155690382)) ;
#52906 = CARTESIAN_POINT('Ctrl Pts',(28.7210144421838,586.898683596496,-49.3387607110024)) ;
#52907 = CARTESIAN_POINT('Ctrl Pts',(28.6774006108051,586.85599252865,-49.3348927633337)) ;
#52908 = CARTESIAN_POINT('Ctrl Pts',(28.6361373799858,586.810943459451,-49.3310751940078)) ;
#52909 = CARTESIAN_POINT('Ctrl Pts',(28.5974978886643,586.763817419732,-49.3272611266717)) ;
#52910 = CARTESIAN_POINT('Ctrl Pts',(28.5575560895066,586.715103041019,-49.3233185097712)) ;
#52911 = CARTESIAN_POINT('Ctrl Pts',(28.5204185737604,586.66416887415,-49.3193792044937)) ;
#52912 = CARTESIAN_POINT('Ctrl Pts',(28.4863557060612,586.611365641621,-49.315373822326)) ;
#52913 = CARTESIAN_POINT('Ctrl Pts',(28.4567183675625,586.565422731291,-49.3118888289846)) ;
#52914 = CARTESIAN_POINT('Ctrl Pts',(28.4294080495839,586.518064194444,-49.3083531635697)) ;
#52915 = CARTESIAN_POINT('Ctrl Pts',(28.4045783576044,586.469551626168,-49.3047162086791)) ;
#52916 = CARTESIAN_POINT('Ctrl Pts',(28.4008846903444,586.462334892055,-49.3041751749354)) ;
#52917 = CARTESIAN_POINT('Ctrl Pts',(28.3972458323923,586.455092581239,-49.3036318996998)) ;
#52918 = CARTESIAN_POINT('Ctrl Pts',(28.3936622003196,586.447825511975,-49.3030862163398)) ;
#52919 = CARTESIAN_POINT('Ctrl Pts',(28.3936486456252,586.447798025084,-49.3030841523525)) ;
#52920 = CARTESIAN_POINT('Ctrl Pts',(28.3936350917208,586.447770537839,-49.3030820883307)) ;
#52921 = CARTESIAN_POINT('Ctrl Pts',(28.3936215386065,586.44774305024,-49.3030800242744)) ;
#52922 = CARTESIAN_POINT('Ctrl Pts',(28.369105706428,586.398021535994,-49.2993464132927)) ;
#52923 = CARTESIAN_POINT('Ctrl Pts',(28.3470946232122,586.346959372583,-49.2954902524912)) ;
#52924 = CARTESIAN_POINT('Ctrl Pts',(28.3277003414553,586.294843528449,-49.2915747618002)) ;
#52925 = CARTESIAN_POINT('Ctrl Pts',(28.3259022254139,586.29001167458,-49.291211742086)) ;
#52926 = CARTESIAN_POINT('Ctrl Pts',(28.3241265948477,586.28517079955,-49.2908482123818)) ;
#52927 = CARTESIAN_POINT('Ctrl Pts',(28.3223735335455,586.280321154001,-49.290484223071)) ;
#52928 = CARTESIAN_POINT('Ctrl Pts',(28.301455594047,586.222454043439,-49.2861410170623)) ;
#52929 = CARTESIAN_POINT('Ctrl Pts',(28.2837519466565,586.163332258295,-49.2817330394404)) ;
#52930 = CARTESIAN_POINT('Ctrl Pts',(28.269365237472,586.103349954343,-49.27733166919)) ;
#52931 = CARTESIAN_POINT('Ctrl Pts',(28.2551945664532,586.044268375271,-49.272996392161)) ;
#52932 = CARTESIAN_POINT('Ctrl Pts',(28.2442415172068,585.984351936258,-49.2686678082078)) ;
#52933 = CARTESIAN_POINT('Ctrl Pts',(28.2365651414893,585.923978458449,-49.2643935745064)) ;
#52934 = CARTESIAN_POINT('Ctrl Pts',(28.2288935295783,585.863642447223,-49.2601219933097)) ;
#52935 = CARTESIAN_POINT('Ctrl Pts',(28.2244943989448,585.80284995105,-49.2559048289096)) ;
#52936 = CARTESIAN_POINT('Ctrl Pts',(28.2233914542907,585.74197937957,-49.2517658773966)) ;
#52937 = CARTESIAN_POINT('Ctrl Pts',(28.2222887826853,585.681123877412,-49.2476279505364)) ;
#52938 = CARTESIAN_POINT('Ctrl Pts',(28.2244806974172,585.620190359768,-49.2435681999355)) ;
#52939 = CARTESIAN_POINT('Ctrl Pts',(28.2299563119541,585.559558208652,-49.2395856489644)) ;
#52940 = CARTESIAN_POINT('Ctrl Pts',(28.2355849365913,585.497231757936,-49.2354918099325)) ;
#52941 = CARTESIAN_POINT('Ctrl Pts',(28.2446837012938,585.435223824145,-49.2314795365644)) ;
#52942 = CARTESIAN_POINT('Ctrl Pts',(28.2572010712248,585.373947134114,-49.2275214453289)) ;
#52943 = CARTESIAN_POINT('Ctrl Pts',(28.2693936536096,585.314260387171,-49.2236660544807)) ;
#52944 = CARTESIAN_POINT('Ctrl Pts',(28.2848298640616,585.255267569577,-49.219861702331)) ;
#52945 = CARTESIAN_POINT('Ctrl Pts',(28.3034218749836,585.197349148697,-49.2160616096605)) ;
#52946 = CARTESIAN_POINT('Ctrl Pts',(28.3227567704007,585.137116470525,-49.2121096759688)) ;
#52947 = CARTESIAN_POINT('Ctrl Pts',(28.3455055208302,585.078046121607,-49.2081619304247)) ;
#52948 = CARTESIAN_POINT('Ctrl Pts',(28.371517494248,585.020561337141,-49.2041477630991)) ;
#52949 = CARTESIAN_POINT('Ctrl Pts',(28.3940194411683,584.970833484969,-49.200675263007)) ;
#52950 = CARTESIAN_POINT('Ctrl Pts',(28.4189635994826,584.922291233137,-49.1971523990756)) ;
#52951 = CARTESIAN_POINT('Ctrl Pts',(28.4462133426358,584.875204601401,-49.1935285002376)) ;
#52952 = CARTESIAN_POINT('Ctrl Pts',(28.4504490032766,584.867885523506,-49.1929652066465)) ;
#52953 = CARTESIAN_POINT('Ctrl Pts',(28.4547403539537,584.860601513723,-49.1923994719366)) ;
#52954 = CARTESIAN_POINT('Ctrl Pts',(28.4590868675054,584.85335347353,-49.1918311058089)) ;
#52955 = CARTESIAN_POINT('Ctrl Pts',(28.4591022226987,584.853327867936,-49.1918290979073)) ;
#52956 = CARTESIAN_POINT('Ctrl Pts',(28.4591175785805,584.853302262792,-49.1918270899728)) ;
#52957 = CARTESIAN_POINT('Ctrl Pts',(28.4591329351506,584.853276658097,-49.1918250820054)) ;
#52958 = CARTESIAN_POINT('Ctrl Pts',(28.4876439124845,584.805739031774,-49.1880970938573)) ;
#52959 = CARTESIAN_POINT('Ctrl Pts',(28.5186379375329,584.759581449879,-49.1842460094343)) ;
#52960 = CARTESIAN_POINT('Ctrl Pts',(28.5519343532963,584.715053248464,-49.1803349721041)) ;
#52961 = CARTESIAN_POINT('Ctrl Pts',(28.5550479549378,584.710889344397,-49.1799692446835)) ;
#52962 = CARTESIAN_POINT('Ctrl Pts',(28.5581816542848,584.706739701188,-49.1796029930094)) ;
#52963 = CARTESIAN_POINT('Ctrl Pts',(28.5613352815921,584.702604530114,-49.1792362687144)) ;
#52964 = CARTESIAN_POINT('Ctrl Pts',(28.5986481131138,584.653678348742,-49.1748972899763)) ;
#52965 = CARTESIAN_POINT('Ctrl Pts',(28.6387561539551,584.606775674653,-49.1704928166311)) ;
#52966 = CARTESIAN_POINT('Ctrl Pts',(28.681383484678,584.562195913215,-49.1660942438563)) ;
#52967 = CARTESIAN_POINT('Ctrl Pts',(28.7233976927919,584.518257356825,-49.1617589371686)) ;
#52968 = CARTESIAN_POINT('Ctrl Pts',(28.7678589922592,584.476575000279,-49.157429649602)) ;
#52969 = CARTESIAN_POINT('Ctrl Pts',(28.8144811521911,584.437403214667,-49.153154203207)) ;
#52970 = CARTESIAN_POINT('Ctrl Pts',(28.8610746801217,584.398255485569,-49.148881382486)) ;
#52971 = CARTESIAN_POINT('Ctrl Pts',(28.909826357949,584.361615128034,-49.1446624721032)) ;
#52972 = CARTESIAN_POINT('Ctrl Pts',(28.9604303812696,584.327707055385,-49.1405214176195)) ;
#52973 = CARTESIAN_POINT('Ctrl Pts',(29.0110221426583,584.293807199048,-49.1363813665605)) ;
#52974 = CARTESIAN_POINT('Ctrl Pts',(29.0634653525719,584.262638340035,-49.1323191363699)) ;
#52975 = CARTESIAN_POINT('Ctrl Pts',(29.1174347103728,584.234396814664,-49.12833387015)) ;
#52976 = CARTESIAN_POINT('Ctrl Pts',(29.1728496356943,584.205398840941,-49.1242418587021)) ;
#52977 = CARTESIAN_POINT('Ctrl Pts',(29.2298736888144,584.179487448832,-49.1202309763558)) ;
#52978 = CARTESIAN_POINT('Ctrl Pts',(29.2881328095016,584.156842272946,-49.1162740363857)) ;
#52979 = CARTESIAN_POINT('Ctrl Pts',(29.3449446176583,584.134759663856,-49.112415397398)) ;
#52980 = CARTESIAN_POINT('Ctrl Pts',(29.4029308467287,584.115783191148,-49.1086076904091)) ;
#52981 = CARTESIAN_POINT('Ctrl Pts',(29.4617236953144,584.100045151821,-49.1048042023169)) ;
#52982 = CARTESIAN_POINT('Ctrl Pts',(29.5227632148621,584.083705709487,-49.1008553702507)) ;
#52983 = CARTESIAN_POINT('Ctrl Pts',(29.5846723184021,584.070857799057,-49.0969106653445)) ;
#52984 = CARTESIAN_POINT('Ctrl Pts',(29.6470154064052,584.061603646524,-49.0928998653571)) ;
#52985 = CARTESIAN_POINT('Ctrl Pts',(29.7010540955114,584.053582191577,-49.0894233232011)) ;
#52986 = CARTESIAN_POINT('Ctrl Pts',(29.7554197479734,584.048260564658,-49.0858964661079)) ;
#52987 = CARTESIAN_POINT('Ctrl Pts',(29.809810853575,584.045670322028,-49.0822685563521)) ;
#52988 = CARTESIAN_POINT('Ctrl Pts',(29.8181398865501,584.045273672318,-49.0817130063288)) ;
#52989 = CARTESIAN_POINT('Ctrl Pts',(29.8264695910836,584.044941006331,-49.0811550866721)) ;
#52990 = CARTESIAN_POINT('Ctrl Pts',(29.8347989676782,584.044672368068,-49.0805946151893)) ;
#52991 = CARTESIAN_POINT('Ctrl Pts',(29.8348284924448,584.044671415838,-49.0805926285113)) ;
#52992 = CARTESIAN_POINT('Ctrl Pts',(29.8348580172073,584.044670464412,-49.0805906418011)) ;
#52993 = CARTESIAN_POINT('Ctrl Pts',(29.8348875419656,584.044669513791,-49.0805886550589)) ;
#52994 = CARTESIAN_POINT('Ctrl Pts',(29.8903175165627,584.042884811547,-49.0768587322658)) ;
#52995 = CARTESIAN_POINT('Ctrl Pts',(29.9459321440122,584.043937425318,-49.0730059557604)) ;
#52996 = CARTESIAN_POINT('Ctrl Pts',(30.0014236513393,584.04781044237,-49.0690934740472)) ;
#52997 = CARTESIAN_POINT('Ctrl Pts',(30.0065959059976,584.0481714387,-49.0687287992936)) ;
#52998 = CARTESIAN_POINT('Ctrl Pts',(30.0117670612265,584.048556915355,-49.0683636058366)) ;
#52999 = CARTESIAN_POINT('Ctrl Pts',(30.0169368498329,584.048966844287,-49.067997944812)) ;
#53000 = CARTESIAN_POINT('Ctrl Pts',(30.0782730130214,584.053830383164,-49.0636596157266)) ;
#53001 = CARTESIAN_POINT('Ctrl Pts',(30.1394218342725,584.062139185518,-49.0592561361515)) ;
#53002 = CARTESIAN_POINT('Ctrl Pts',(30.1999823563176,584.07382344307,-49.0548587678238)) ;
#53003 = CARTESIAN_POINT('Ctrl Pts',(30.2596856714703,584.085342315222,-49.0505236422628)) ;
#53004 = CARTESIAN_POINT('Ctrl Pts',(30.3188174004899,584.100141355125,-49.0461947433676)) ;
#53005 = CARTESIAN_POINT('Ctrl Pts',(30.3770085797434,584.118117662475,-49.0419198022215)) ;
#53006 = CARTESIAN_POINT('Ctrl Pts',(30.4351642463517,584.136082999327,-49.0376474699668)) ;
#53007 = CARTESIAN_POINT('Ctrl Pts',(30.4923805778851,584.157221615747,-49.0334291645333)) ;
#53008 = CARTESIAN_POINT('Ctrl Pts',(30.548302767096,584.181398204428,-49.0292887349009)) ;
#53009 = CARTESIAN_POINT('Ctrl Pts',(30.6042116002257,584.205569018935,-49.025149294141)) ;
#53010 = CARTESIAN_POINT('Ctrl Pts',(30.6588268789108,584.232776375357,-49.0210876943239)) ;
#53011 = CARTESIAN_POINT('Ctrl Pts',(30.7118072538956,584.262853095794,-49.0171029811632)) ;
#53012 = CARTESIAN_POINT('Ctrl Pts',(30.7661843114642,584.293722706647,-49.0130132219459)) ;
#53013 = CARTESIAN_POINT('Ctrl Pts',(30.8188389230425,584.32761524715,-49.0090044413065)) ;
#53014 = CARTESIAN_POINT('Ctrl Pts',(30.8694177914357,584.364313765642,-49.0050493917579)) ;
#53015 = CARTESIAN_POINT('Ctrl Pts',(30.9187607530955,584.400115547067,-49.0011909847899)) ;
#53016 = CARTESIAN_POINT('Ctrl Pts',(30.9661279918959,584.438587919974,-48.9973833526409)) ;
#53017 = CARTESIAN_POINT('Ctrl Pts',(31.0112089557346,584.479493276818,-48.9935797119252)) ;
#53018 = CARTESIAN_POINT('Ctrl Pts',(31.0579836525257,584.521935485249,-48.9896331649567)) ;
#53019 = CARTESIAN_POINT('Ctrl Pts',(31.102296402178,584.566997512617,-48.9856904925102)) ;
#53020 = CARTESIAN_POINT('Ctrl Pts',(31.143825788243,584.614369021137,-48.9816815573379)) ;
#53021 = CARTESIAN_POINT('Ctrl Pts',(31.1798354338611,584.655444302904,-48.978205456472)) ;
#53022 = CARTESIAN_POINT('Ctrl Pts',(31.2137531507878,584.698256546786,-48.9746788816414)) ;
#53023 = CARTESIAN_POINT('Ctrl Pts',(31.2453891710365,584.742569517941,-48.9710511387411)) ;
#53024 = CARTESIAN_POINT('Ctrl Pts',(31.2502212057411,584.74933780968,-48.970497043142)) ;
#53025 = CARTESIAN_POINT('Ctrl Pts',(31.2550001060564,584.756141138826,-48.9699405873914)) ;
#53026 = CARTESIAN_POINT('Ctrl Pts',(31.2597252983142,584.762978695664,-48.9693815908545)) ;
#53027 = CARTESIAN_POINT('Ctrl Pts',(31.2597422102587,584.763003167976,-48.9693795901489)) ;
#53028 = CARTESIAN_POINT('Ctrl Pts',(31.2597591215152,584.763027640727,-48.9693775894108)) ;
#53029 = CARTESIAN_POINT('Ctrl Pts',(31.2597760320838,584.763052113917,-48.9693755886401)) ;
#53030 = CARTESIAN_POINT('Ctrl Pts',(31.291512138973,584.808981010507,-48.9656207372716)) ;
#53031 = CARTESIAN_POINT('Ctrl Pts',(31.3209299268057,584.856619987665,-48.9617415914158)) ;
#53032 = CARTESIAN_POINT('Ctrl Pts',(31.3478772797298,584.905699548094,-48.957802345134)) ;
#53033 = CARTESIAN_POINT('Ctrl Pts',(31.3505714667192,584.910606505505,-48.9574085006584)) ;
#53034 = CARTESIAN_POINT('Ctrl Pts',(31.3532409612405,584.915527819945,-48.9570140554231)) ;
#53035 = CARTESIAN_POINT('Ctrl Pts',(31.3558856132298,584.920463193576,-48.956619073583)) ;
#53036 = CARTESIAN_POINT('Ctrl Pts',(31.3849334868214,584.974671501491,-48.9522807399917)) ;
#53037 = CARTESIAN_POINT('Ctrl Pts',(31.410984647693,585.030581948043,-48.9478783028844)) ;
#53038 = CARTESIAN_POINT('Ctrl Pts',(31.4338829509442,585.08782613794,-48.9434824085856)) ;
#53039 = CARTESIAN_POINT('Ctrl Pts',(31.4567460818547,585.144982399393,-48.9390932664854)) ;
#53040 = CARTESIAN_POINT('Ctrl Pts',(31.4764664101212,585.203468299925,-48.9347109833581)) ;
#53041 = CARTESIAN_POINT('Ctrl Pts',(31.49292594124,585.262910672511,-48.9303843986088)) ;
#53042 = CARTESIAN_POINT('Ctrl Pts',(31.5093706759025,585.322299608796,-48.9260617032851)) ;
#53043 = CARTESIAN_POINT('Ctrl Pts',(31.522560610632,585.382643343148,-48.9217947462704)) ;
#53044 = CARTESIAN_POINT('Ctrl Pts',(31.5324116742823,585.443562888578,-48.9176072870562)) ;
#53045 = CARTESIAN_POINT('Ctrl Pts',(31.5422576410633,585.504450914674,-48.9134219944033)) ;
#53046 = CARTESIAN_POINT('Ctrl Pts',(31.5487681465865,585.565914190783,-48.9093161225875)) ;
#53047 = CARTESIAN_POINT('Ctrl Pts',(31.5518921895599,585.627566870626,-48.9052874063687)) ;
#53048 = CARTESIAN_POINT('Ctrl Pts',(31.5533073133279,585.655494198564,-48.9034624852251)) ;
#53049 = CARTESIAN_POINT('Ctrl Pts',(31.5540280230629,585.683460285665,-48.9016530418679)) ;
#53050 = CARTESIAN_POINT('Ctrl Pts',(31.5540518914521,585.711428744506,-48.8998571438181)) ;
#53051 = CARTESIAN_POINT('Ctrl Pts',(31.5545274105876,585.711411214421,-48.8995834207373)) ;
#53052 = CARTESIAN_POINT('Ctrl Pts',(31.5544903932093,585.784303671105,-48.8949620477403)) ;
#53053 = CARTESIAN_POINT('Ctrl Pts',(31.5496696402885,585.857118891942,-48.8904723599722)) ;
#53054 = CARTESIAN_POINT('Ctrl Pts',(31.5263027539008,586.033479051458,-48.8795927983639)) ;
#53055 = CARTESIAN_POINT('Ctrl Pts',(31.5027036142072,586.13602033832,-48.8732665485696)) ;
#53056 = CARTESIAN_POINT('Ctrl Pts',(31.4639986027888,586.25256609756,-48.8654275397895)) ;
#53057 = CARTESIAN_POINT('Ctrl Pts',(31.4581092953798,586.269391653842,-48.8642790344837)) ;
#53058 = CARTESIAN_POINT('Ctrl Pts',(31.451951903833,586.286117526255,-48.8631174034081)) ;
#53059 = CARTESIAN_POINT('Origin',(29.8885276254069,535.710565160562,-48.522160171753)) ;
#53060 = CARTESIAN_POINT('',(31.4521854151178,536.286177671927,-47.6539925072191)) ;
#53061 = CARTESIAN_POINT('',(31.4519498093679,536.286123215583,-47.522160171753)) ;
#53062 = CARTESIAN_POINT('',(31.4519498093678,536.286123215583,-48.5221601717531)) ;
#53063 = CARTESIAN_POINT('',(29.9642548136477,537.375716565857,-47.5221676802302)) ;
#53064 = CARTESIAN_POINT('Origin',(29.8885276254069,535.710565160562,-47.522160171753)) ;
#53065 = CARTESIAN_POINT('Ctrl Pts',(29.9642548143816,537.375716581994,-47.5221676803692)) ;
#53066 = CARTESIAN_POINT('Ctrl Pts',(30.0170574073778,537.373284149692,-47.5257769798607)) ;
#53067 = CARTESIAN_POINT('Ctrl Pts',(30.0698319721191,537.368277725697,-47.5294835831224)) ;
#53068 = CARTESIAN_POINT('Ctrl Pts',(30.1223097046126,537.360730277946,-47.5332331994959)) ;
#53069 = CARTESIAN_POINT('Ctrl Pts',(30.1821635812742,537.352121979048,-47.5375098529502)) ;
#53070 = CARTESIAN_POINT('Ctrl Pts',(30.2416325433276,537.340207859062,-47.5418418996151)) ;
#53071 = CARTESIAN_POINT('Ctrl Pts',(30.3003395339928,537.32507516245,-47.5461632085829)) ;
#53072 = CARTESIAN_POINT('Ctrl Pts',(30.3589866688338,537.309957894666,-47.5504801116784)) ;
#53073 = CARTESIAN_POINT('Ctrl Pts',(30.416873522907,537.291628889203,-47.5547860009387)) ;
#53074 = CARTESIAN_POINT('Ctrl Pts',(30.4736402945146,537.27020984188,-47.5590357020397)) ;
#53075 = CARTESIAN_POINT('Ctrl Pts',(30.5303707287166,537.248804505264,-47.5632826828325)) ;
#53076 = CARTESIAN_POINT('Ctrl Pts',(30.5859825640855,537.224313171479,-47.5674734291859)) ;
#53077 = CARTESIAN_POINT('Ctrl Pts',(30.6401313340043,537.196889321788,-47.5715866433701)) ;
#53078 = CARTESIAN_POINT('Ctrl Pts',(30.6942659880685,537.169472621124,-47.5756987852949)) ;
#53079 = CARTESIAN_POINT('Ctrl Pts',(30.746938287709,537.139124906016,-47.5797334448799)) ;
#53080 = CARTESIAN_POINT('Ctrl Pts',(30.7978186947913,537.106031130019,-47.5836939134857)) ;
#53081 = CARTESIAN_POINT('Ctrl Pts',(30.8487419661031,537.07290947415,-47.5876577185906)) ;
#53082 = CARTESIAN_POINT('Ctrl Pts',(30.8978701708745,537.037037008071,-47.5915473315807)) ;
#53083 = CARTESIAN_POINT('Ctrl Pts',(30.9448891615152,536.998631930822,-47.5953896858911)) ;
#53084 = CARTESIAN_POINT('Ctrl Pts',(30.9919258102846,536.960212430426,-47.5992334832097)) ;
#53085 = CARTESIAN_POINT('Ctrl Pts',(31.0368513845029,536.919258218283,-47.6030302593924)) ;
#53086 = CARTESIAN_POINT('Ctrl Pts',(31.0793707884461,536.876022923814,-47.6068276814917)) ;
#53087 = CARTESIAN_POINT('Ctrl Pts',(31.1219709625019,536.832705499323,-47.6106323171967)) ;
#53088 = CARTESIAN_POINT('Ctrl Pts',(31.1621553398343,536.787098063884,-47.6144380750506)) ;
#53089 = CARTESIAN_POINT('Ctrl Pts',(31.1996521844407,536.73949448145,-47.6183081328949)) ;
#53090 = CARTESIAN_POINT('Ctrl Pts',(31.2333481056982,536.696716306856,-47.6217858965775)) ;
#53091 = CARTESIAN_POINT('Ctrl Pts',(31.2648740144835,536.652325877933,-47.6253161745565)) ;
#53092 = CARTESIAN_POINT('Ctrl Pts',(31.2940549538489,536.606567395771,-47.6289493146419)) ;
#53093 = CARTESIAN_POINT('Ctrl Pts',(31.2966758844579,536.602457527853,-47.6292756306641)) ;
#53094 = CARTESIAN_POINT('Ctrl Pts',(31.2992779311643,536.598336612712,-47.6296027764757)) ;
#53095 = CARTESIAN_POINT('Ctrl Pts',(31.3018609866169,536.594204820238,-47.6299307885563)) ;
#53096 = CARTESIAN_POINT('Ctrl Pts',(31.3018781850347,536.594177310068,-47.629932972516)) ;
#53097 = CARTESIAN_POINT('Ctrl Pts',(31.3018953826107,536.594149799416,-47.629935156514)) ;
#53098 = CARTESIAN_POINT('Ctrl Pts',(31.3019125793448,536.594122288282,-47.6299373405505)) ;
#53099 = CARTESIAN_POINT('Ctrl Pts',(31.3317744651969,536.546349592843,-47.6337298889883)) ;
#53100 = CARTESIAN_POINT('Ctrl Pts',(31.359192467101,536.496956319906,-47.6376476228927)) ;
#53101 = CARTESIAN_POINT('Ctrl Pts',(31.384028189051,536.446222500673,-47.6416252768862)) ;
#53102 = CARTESIAN_POINT('Ctrl Pts',(31.3866683921264,536.440829156931,-47.6420481280651)) ;
#53103 = CARTESIAN_POINT('Ctrl Pts',(31.3892794152376,536.435420711993,-47.6424716564076)) ;
#53104 = CARTESIAN_POINT('Ctrl Pts',(31.3918610949582,536.429997536727,-47.6428957835048)) ;
#53105 = CARTESIAN_POINT('Ctrl Pts',(31.4141913480305,536.383089752166,-47.646564273186)) ;
#53106 = CARTESIAN_POINT('Ctrl Pts',(31.434327202609,536.335075674395,-47.6502774611457)) ;
#53107 = CARTESIAN_POINT('Ctrl Pts',(31.4521854151178,536.286177671927,-47.6539925072191)) ;
#53108 = CARTESIAN_POINT('Origin',(29.8885276254069,535.710565160562,-48.522160171753)) ;
#53109 = CARTESIAN_POINT('',(31.4519498068212,536.2861232225,-48.3557322092704)) ;
#53110 = CARTESIAN_POINT('',(31.4519274540278,536.286111640514,-48.1612746756653)) ;
#53111 = CARTESIAN_POINT('',(31.4519498093678,536.286123215583,-48.5221601717531)) ;
#53112 = CARTESIAN_POINT('',(31.5236569526584,535.391334705934,-47.522160171753)) ;
#53113 = CARTESIAN_POINT('Ctrl Pts',(31.4519274540278,536.286111640514,-48.1612746756653)) ;
#53114 = CARTESIAN_POINT('Ctrl Pts',(31.4307763993745,536.343129105232,-48.1569488744972)) ;
#53115 = CARTESIAN_POINT('Ctrl Pts',(31.4064929013936,536.399042410981,-48.1526457224962)) ;
#53116 = CARTESIAN_POINT('Ctrl Pts',(31.3792366254787,536.453505067295,-48.1484061457518)) ;
#53117 = CARTESIAN_POINT('Ctrl Pts',(31.3519940803956,536.507940287082,-48.1441687047693)) ;
#53118 = CARTESIAN_POINT('Ctrl Pts',(31.3217818123083,536.560926365304,-48.1399948666501)) ;
#53119 = CARTESIAN_POINT('Ctrl Pts',(31.2887894185131,536.612134703357,-48.1359011995699)) ;
#53120 = CARTESIAN_POINT('Ctrl Pts',(31.2558013785795,536.66333628367,-48.1318080727131)) ;
#53121 = CARTESIAN_POINT('Ctrl Pts',(31.220033903596,536.712760528073,-48.1277950639092)) ;
#53122 = CARTESIAN_POINT('Ctrl Pts',(31.1817065990466,536.760096483813,-48.1238540114814)) ;
#53123 = CARTESIAN_POINT('Ctrl Pts',(31.1433423463772,536.807478072153,-48.1199091598175)) ;
#53124 = CARTESIAN_POINT('Ctrl Pts',(31.1024131976471,536.85276716559,-48.1160362534294)) ;
#53125 = CARTESIAN_POINT('Ctrl Pts',(31.0591708420407,536.895671278289,-48.1122036736627)) ;
#53126 = CARTESIAN_POINT('Ctrl Pts',(31.0159079097594,536.938595806712,-48.1083692701806)) ;
#53127 = CARTESIAN_POINT('Ctrl Pts',(30.9703293733988,536.979132765155,-48.1045749219151)) ;
#53128 = CARTESIAN_POINT('Ctrl Pts',(30.9227211915417,537.017012300491,-48.1007689239922)) ;
#53129 = CARTESIAN_POINT('Ctrl Pts',(30.8750231851506,537.054963304879,-48.0969557451189)) ;
#53130 = CARTESIAN_POINT('Ctrl Pts',(30.825287647601,537.090246304601,-48.0931303466352)) ;
#53131 = CARTESIAN_POINT('Ctrl Pts',(30.7738394110681,537.122619453151,-48.089226826036)) ;
#53132 = CARTESIAN_POINT('Ctrl Pts',(30.7324041251834,537.148692079844,-48.0860830158126)) ;
#53133 = CARTESIAN_POINT('Ctrl Pts',(30.6898586330363,537.172877634962,-48.0828880724602)) ;
#53134 = CARTESIAN_POINT('Ctrl Pts',(30.6463912714896,537.195068149825,-48.0796053349554)) ;
#53135 = CARTESIAN_POINT('Ctrl Pts',(30.6463647388652,537.195081694991,-48.0796033311613)) ;
#53136 = CARTESIAN_POINT('Ctrl Pts',(30.6463382058969,537.195095239413,-48.0796013273345)) ;
#53137 = CARTESIAN_POINT('Ctrl Pts',(30.6463116725847,537.195108783094,-48.079599323475)) ;
#53138 = CARTESIAN_POINT('Ctrl Pts',(30.5969681857448,537.220295703685,-48.0758727847674)) ;
#53139 = CARTESIAN_POINT('Ctrl Pts',(30.5462514251147,537.242999512425,-48.0720232603926)) ;
#53140 = CARTESIAN_POINT('Ctrl Pts',(30.4944463678682,537.263104505909,-48.0681138788279)) ;
#53141 = CARTESIAN_POINT('Ctrl Pts',(30.4896029522929,537.264984184145,-48.0677483786129)) ;
#53142 = CARTESIAN_POINT('Ctrl Pts',(30.4847500607543,537.266841154097,-48.0673823551886)) ;
#53143 = CARTESIAN_POINT('Ctrl Pts',(30.4798879487158,537.268675326625,-48.0670158601448)) ;
#53144 = CARTESIAN_POINT('Ctrl Pts',(30.4223124608371,537.290394977941,-48.0626759496729)) ;
#53145 = CARTESIAN_POINT('Ctrl Pts',(30.3634380633247,537.308917002742,-48.0582705761492)) ;
#53146 = CARTESIAN_POINT('Ctrl Pts',(30.3036577270648,537.324133525588,-48.0538712807422)) ;
#53147 = CARTESIAN_POINT('Ctrl Pts',(30.2447759697572,537.339121323607,-48.0495381126691)) ;
#53148 = CARTESIAN_POINT('Ctrl Pts',(30.1850153196505,537.350902695154,-48.045211126453)) ;
#53149 = CARTESIAN_POINT('Ctrl Pts',(30.1247528952844,537.359413652336,-48.0409381775236)) ;
#53150 = CARTESIAN_POINT('Ctrl Pts',(30.0645273363901,537.367919402949,-48.036667842566)) ;
#53151 = CARTESIAN_POINT('Ctrl Pts',(30.003800605354,537.373158868586,-48.0324516142783)) ;
#53152 = CARTESIAN_POINT('Ctrl Pts',(29.9429508114481,537.375103428451,-48.0283135052074)) ;
#53153 = CARTESIAN_POINT('Ctrl Pts',(29.8821155448548,537.377047524072,-48.0241763840708)) ;
#53154 = CARTESIAN_POINT('Ctrl Pts',(29.8211572945153,537.37569825651,-48.0201173480267)) ;
#53155 = CARTESIAN_POINT('Ctrl Pts',(29.7604555381149,537.371061579568,-48.0161356354981)) ;
#53156 = CARTESIAN_POINT('Ctrl Pts',(29.6980574154047,537.366295326432,-48.0120426503574)) ;
#53157 = CARTESIAN_POINT('Ctrl Pts',(29.6359303902143,537.358055001222,-48.0080313634024)) ;
#53158 = CARTESIAN_POINT('Ctrl Pts',(29.574487749723,537.346386736832,-48.0040746050507)) ;
#53159 = CARTESIAN_POINT('Ctrl Pts',(29.5146381758799,537.335021003758,-48.0002204363617)) ;
#53160 = CARTESIAN_POINT('Ctrl Pts',(29.4554380951338,537.320402658138,-47.9964176386363)) ;
#53161 = CARTESIAN_POINT('Ctrl Pts',(29.3972689929696,537.302614489539,-47.9926195892224)) ;
#53162 = CARTESIAN_POINT('Ctrl Pts',(29.336777386634,537.284116096882,-47.9886698959756)) ;
#53163 = CARTESIAN_POINT('Ctrl Pts',(29.2774010738504,537.262188882748,-47.9847249222463)) ;
#53164 = CARTESIAN_POINT('Ctrl Pts',(29.2195650502174,537.236977757016,-47.9807141626381)) ;
#53165 = CARTESIAN_POINT('Ctrl Pts',(29.1694956145773,537.215152141111,-47.9772419932625)) ;
#53166 = CARTESIAN_POINT('Ctrl Pts',(29.1205796400799,537.190865130713,-47.9737198631058)) ;
#53167 = CARTESIAN_POINT('Ctrl Pts',(29.0730894036172,537.164249925727,-47.970096974239)) ;
#53168 = CARTESIAN_POINT('Ctrl Pts',(29.0657493701776,537.160136311874,-47.9695370249229)) ;
#53169 = CARTESIAN_POINT('Ctrl Pts',(29.0584432953211,537.155967097591,-47.9689746686405)) ;
#53170 = CARTESIAN_POINT('Ctrl Pts',(29.0511720738838,537.15174278969,-47.9684097178374)) ;
#53171 = CARTESIAN_POINT('Ctrl Pts',(29.0511458435209,537.15172755083,-47.9684076798215)) ;
#53172 = CARTESIAN_POINT('Ctrl Pts',(29.0511196136116,537.151712311252,-47.9684056417719)) ;
#53173 = CARTESIAN_POINT('Ctrl Pts',(29.0510933841558,537.151697070958,-47.9684036036885)) ;
#53174 = CARTESIAN_POINT('Ctrl Pts',(29.0030948273822,537.123808115142,-47.9646740157731)) ;
#53175 = CARTESIAN_POINT('Ctrl Pts',(28.9564471739132,537.093411201235,-47.9608215272907)) ;
#53176 = CARTESIAN_POINT('Ctrl Pts',(28.911402686255,537.060684312441,-47.9569092390924)) ;
#53177 = CARTESIAN_POINT('Ctrl Pts',(28.907192685099,537.057625553272,-47.9565435841878)) ;
#53178 = CARTESIAN_POINT('Ctrl Pts',(28.9029967015222,537.054546476073,-47.9561774069107)) ;
#53179 = CARTESIAN_POINT('Ctrl Pts',(28.8988149491624,537.051447248039,-47.955810758779)) ;
#53180 = CARTESIAN_POINT('Ctrl Pts',(28.8493969261517,537.014821998832,-47.9514778800595)) ;
#53181 = CARTESIAN_POINT('Ctrl Pts',(28.8019638330814,536.975377158774,-47.9470799052921)) ;
#53182 = CARTESIAN_POINT('Ctrl Pts',(28.7568178425373,536.933384066512,-47.9426877957958)) ;
#53183 = CARTESIAN_POINT('Ctrl Pts',(28.7122458337714,536.891924870382,-47.938351527157)) ;
#53184 = CARTESIAN_POINT('Ctrl Pts',(28.6699027807026,536.847982052344,-47.9340212680818)) ;
#53185 = CARTESIAN_POINT('Ctrl Pts',(28.6300474554127,536.801839145611,-47.9297447615701)) ;
#53186 = CARTESIAN_POINT('Ctrl Pts',(28.5902164977647,536.755724450761,-47.9254708697248)) ;
#53187 = CARTESIAN_POINT('Ctrl Pts',(28.5528701088114,536.707412413854,-47.9212507998254)) ;
#53188 = CARTESIAN_POINT('Ctrl Pts',(28.5182378571019,536.657206506776,-47.9171083924019)) ;
#53189 = CARTESIAN_POINT('Ctrl Pts',(28.4836139993599,536.60701276832,-47.9129669889915)) ;
#53190 = CARTESIAN_POINT('Ctrl Pts',(28.4517029987154,536.554926073915,-47.9089032122735)) ;
#53191 = CARTESIAN_POINT('Ctrl Pts',(28.4227061221089,536.501269776009,-47.9049160816052)) ;
#53192 = CARTESIAN_POINT('Ctrl Pts',(28.3930198148266,536.446337744229,-47.9008341527891)) ;
#53193 = CARTESIAN_POINT('Ctrl Pts',(28.3663881619663,536.38976045835,-47.8968325311477)) ;
#53194 = CARTESIAN_POINT('Ctrl Pts',(28.34299487761,536.331907062595,-47.8928841713042)) ;
#53195 = CARTESIAN_POINT('Ctrl Pts',(28.3201161371515,536.275326173569,-47.8890226570883)) ;
#53196 = CARTESIAN_POINT('Ctrl Pts',(28.3003350793831,536.217524722683,-47.8852117336552)) ;
#53197 = CARTESIAN_POINT('Ctrl Pts',(28.2837896250148,536.158869478422,-47.8814046545605)) ;
#53198 = CARTESIAN_POINT('Ctrl Pts',(28.2666860086315,536.098235495554,-47.8774691433968)) ;
#53199 = CARTESIAN_POINT('Ctrl Pts',(28.253040808891,536.036689007455,-47.8735373106197)) ;
#53200 = CARTESIAN_POINT('Ctrl Pts',(28.242961550844,535.974659553968,-47.8695398976371)) ;
#53201 = CARTESIAN_POINT('Ctrl Pts',(28.2341891644994,535.920672809289,-47.86606078728)) ;
#53202 = CARTESIAN_POINT('Ctrl Pts',(28.2281176798626,535.866319363877,-47.8625313512965)) ;
#53203 = CARTESIAN_POINT('Ctrl Pts',(28.2247832934975,535.811900633933,-47.8589009975942)) ;
#53204 = CARTESIAN_POINT('Ctrl Pts',(28.2242885317416,535.803825892907,-47.858362319716)) ;
#53205 = CARTESIAN_POINT('Ctrl Pts',(28.2238539700256,535.795749645206,-47.8578214199208)) ;
#53206 = CARTESIAN_POINT('Ctrl Pts',(28.2234796626412,535.787672801144,-47.8572781329275)) ;
#53207 = CARTESIAN_POINT('Ctrl Pts',(28.2234781642949,535.787640469671,-47.8572759581586)) ;
#53208 = CARTESIAN_POINT('Ctrl Pts',(28.2234766669142,535.787608138189,-47.8572737833515)) ;
#53209 = CARTESIAN_POINT('Ctrl Pts',(28.2234751704988,535.787575806697,-47.8572716085062)) ;
#53210 = CARTESIAN_POINT('Ctrl Pts',(28.2209073996856,535.732096649492,-47.853539687112)) ;
#53211 = CARTESIAN_POINT('Ctrl Pts',(28.2211816101443,535.676392651554,-47.8496854610932)) ;
#53212 = CARTESIAN_POINT('Ctrl Pts',(28.2242849530107,535.620773255338,-47.8457724017947)) ;
#53213 = CARTESIAN_POINT('Ctrl Pts',(28.2245669508371,535.615719173494,-47.8454168258032)) ;
#53214 = CARTESIAN_POINT('Ctrl Pts',(28.2248722884664,535.610665819014,-47.8450607640144)) ;
#53215 = CARTESIAN_POINT('Ctrl Pts',(28.2252009433535,535.60561344098,-47.8447042640523)) ;
#53216 = CARTESIAN_POINT('Ctrl Pts',(28.22919531299,535.544208404265,-47.8403714740051)) ;
#53217 = CARTESIAN_POINT('Ctrl Pts',(28.2366370952629,535.482942529108,-47.8359746228171)) ;
#53218 = CARTESIAN_POINT('Ctrl Pts',(28.2474619790141,535.422218004487,-47.8315847343143)) ;
#53219 = CARTESIAN_POINT('Ctrl Pts',(28.258125627529,535.362397963767,-47.8272602326301)) ;
#53220 = CARTESIAN_POINT('Ctrl Pts',(28.2720719365899,535.303103095364,-47.8229427665659)) ;
#53221 = CARTESIAN_POINT('Ctrl Pts',(28.289203276634,535.244703256875,-47.8186794877983)) ;
#53222 = CARTESIAN_POINT('Ctrl Pts',(28.3063246657586,535.186337340548,-47.8144186854011)) ;
#53223 = CARTESIAN_POINT('Ctrl Pts',(28.3266272780083,535.128865351449,-47.8102121386028)) ;
#53224 = CARTESIAN_POINT('Ctrl Pts',(28.3499808983447,535.072643531161,-47.806083000012)) ;
#53225 = CARTESIAN_POINT('Ctrl Pts',(28.3733296704721,535.016433382518,-47.8019547186299)) ;
#53226 = CARTESIAN_POINT('Ctrl Pts',(28.3997282072346,534.961472915357,-47.7979038130668)) ;
#53227 = CARTESIAN_POINT('Ctrl Pts',(28.4290142106474,534.90810541461,-47.7939285579771)) ;
#53228 = CARTESIAN_POINT('Ctrl Pts',(28.4591088753211,534.85326430103,-47.7898435359537)) ;
#53229 = CARTESIAN_POINT('Ctrl Pts',(28.4922529685829,534.800105547781,-47.785838386868)) ;
#53230 = CARTESIAN_POINT('Ctrl Pts',(28.5282337480971,534.748986344858,-47.7818848696984)) ;
#53231 = CARTESIAN_POINT('Ctrl Pts',(28.5632957111165,534.699172537969,-47.7780323107858)) ;
#53232 = CARTESIAN_POINT('Ctrl Pts',(28.6010513997611,534.651295626704,-47.7742284091018)) ;
#53233 = CARTESIAN_POINT('Ctrl Pts',(28.6412674151399,534.605669127893,-47.7704255416625)) ;
#53234 = CARTESIAN_POINT('Ctrl Pts',(28.6830642520887,534.558249130826,-47.7664731901229)) ;
#53235 = CARTESIAN_POINT('Ctrl Pts',(28.7275192520828,534.513260600536,-47.7625215272401)) ;
#53236 = CARTESIAN_POINT('Ctrl Pts',(28.7743246561547,534.471030431014,-47.7584992110668)) ;
#53237 = CARTESIAN_POINT('Ctrl Pts',(28.8147152696772,534.434588005401,-47.7550281627714)) ;
#53238 = CARTESIAN_POINT('Ctrl Pts',(28.8568567763365,534.40019889432,-47.7515038375611)) ;
#53239 = CARTESIAN_POINT('Ctrl Pts',(28.900517275209,534.368054060937,-47.7478756307004)) ;
#53240 = CARTESIAN_POINT('Ctrl Pts',(28.9074234764699,534.362969403305,-47.7473017223062)) ;
#53241 = CARTESIAN_POINT('Ctrl Pts',(28.9143677111017,534.3579407967,-47.7467252147108)) ;
#53242 = CARTESIAN_POINT('Ctrl Pts',(28.9213490950115,534.352968881888,-47.7461459076316)) ;
#53243 = CARTESIAN_POINT('Ctrl Pts',(28.9213773075326,534.352948789847,-47.7461435665896)) ;
#53244 = CARTESIAN_POINT('Ctrl Pts',(28.9214055206604,534.352928698732,-47.7461412255018)) ;
#53245 = CARTESIAN_POINT('Ctrl Pts',(28.9214337343949,534.352908608542,-47.7461388843683)) ;
#53246 = CARTESIAN_POINT('Ctrl Pts',(28.9662228141892,534.321015591944,-47.7424223535122)) ;
#53247 = CARTESIAN_POINT('Ctrl Pts',(29.0127137470464,534.291342910262,-47.7385803120396)) ;
#53248 = CARTESIAN_POINT('Ctrl Pts',(29.0606465209006,534.264045111964,-47.7346755810524)) ;
#53249 = CARTESIAN_POINT('Ctrl Pts',(29.0653146261795,534.261386617867,-47.7342953048057)) ;
#53250 = CARTESIAN_POINT('Ctrl Pts',(29.0699963659741,534.258750645376,-47.7339144339779)) ;
#53251 = CARTESIAN_POINT('Ctrl Pts',(29.0746914739163,534.256137334618,-47.7335330265961)) ;
#53252 = CARTESIAN_POINT('Ctrl Pts',(29.1284554251062,534.226212162759,-47.7291655087216)) ;
#53253 = CARTESIAN_POINT('Ctrl Pts',(29.18397844417,534.199258635353,-47.7247283308864)) ;
#53254 = CARTESIAN_POINT('Ctrl Pts',(29.2408859625142,534.175442489054,-47.7202947956306)) ;
#53255 = CARTESIAN_POINT('Ctrl Pts',(29.2967255816198,534.152073265151,-47.7159444579744)) ;
#53256 = CARTESIAN_POINT('Ctrl Pts',(29.3538981316818,534.131724304163,-47.7115979109087)) ;
#53257 = CARTESIAN_POINT('Ctrl Pts',(29.4120423473608,534.114513494693,-47.7073041677962)) ;
#53258 = CARTESIAN_POINT('Ctrl Pts',(29.4701500258677,534.097313500303,-47.7030131228236)) ;
#53259 = CARTESIAN_POINT('Ctrl Pts',(29.5292281351195,534.083247580819,-47.6987749580719)) ;
#53260 = CARTESIAN_POINT('Ctrl Pts',(29.5889093029062,534.072398666365,-47.694615023098)) ;
#53261 = CARTESIAN_POINT('Ctrl Pts',(29.6485756671699,534.061552442913,-47.6904561199688)) ;
#53262 = CARTESIAN_POINT('Ctrl Pts',(29.7088447677984,534.053921655637,-47.6863754183603)) ;
#53263 = CARTESIAN_POINT('Ctrl Pts',(29.7693429677503,534.049555196414,-47.6823735688117)) ;
#53264 = CARTESIAN_POINT('Ctrl Pts',(29.8319435161226,534.045037000136,-47.6782326526117)) ;
#53265 = CARTESIAN_POINT('Ctrl Pts',(29.8947893459226,534.044014349964,-47.6741761960406)) ;
#53266 = CARTESIAN_POINT('Ctrl Pts',(29.957459733137,534.046501514119,-47.6701779083722)) ;
#53267 = CARTESIAN_POINT('Ctrl Pts',(30.0181053442043,534.04890832213,-47.6663087987392)) ;
#53268 = CARTESIAN_POINT('Ctrl Pts',(30.0785865391467,534.054601903472,-47.6624937791813)) ;
#53269 = CARTESIAN_POINT('Ctrl Pts',(30.1385170065825,534.063555529739,-47.6586872219254)) ;
#53270 = CARTESIAN_POINT('Ctrl Pts',(30.2014488234682,534.072957558337,-47.6546900302724)) ;
#53271 = CARTESIAN_POINT('Ctrl Pts',(30.2637731501992,534.085955289501,-47.6507017947997)) ;
#53272 = CARTESIAN_POINT('Ctrl Pts',(30.3250393960605,534.102464729901,-47.6466504651268)) ;
#53273 = CARTESIAN_POINT('Ctrl Pts',(30.3778260115243,534.11668916082,-47.6431598647391)) ;
#53274 = CARTESIAN_POINT('Ctrl Pts',(30.4298281741923,534.133520596369,-47.6396217634346)) ;
#53275 = CARTESIAN_POINT('Ctrl Pts',(30.4807554477069,534.152865574823,-47.635984368866)) ;
#53276 = CARTESIAN_POINT('Ctrl Pts',(30.4889186970596,534.155966425741,-47.6354013225569)) ;
#53277 = CARTESIAN_POINT('Ctrl Pts',(30.4970544327808,534.15913182708,-47.6348157250445)) ;
#53278 = CARTESIAN_POINT('Ctrl Pts',(30.5051615792712,534.162361361118,-47.6342273630226)) ;
#53279 = CARTESIAN_POINT('Ctrl Pts',(30.5051791544077,534.162368362287,-47.6342260875377)) ;
#53280 = CARTESIAN_POINT('Ctrl Pts',(30.5051967294098,534.162375363757,-47.6342248120398)) ;
#53281 = CARTESIAN_POINT('Ctrl Pts',(30.5052143042776,534.162382365529,-47.6342235365289)) ;
#53282 = CARTESIAN_POINT('Ctrl Pts',(30.5574247027775,534.183182822828,-47.6304343227569)) ;
#53283 = CARTESIAN_POINT('Ctrl Pts',(30.608629897713,534.20672373114,-47.6265205232274)) ;
#53284 = CARTESIAN_POINT('Ctrl Pts',(30.658550718741,534.232862233993,-47.6225444679815)) ;
#53285 = CARTESIAN_POINT('Ctrl Pts',(30.6635861589343,534.23549878654,-47.622143409105)) ;
#53286 = CARTESIAN_POINT('Ctrl Pts',(30.6686085101118,534.238161729959,-47.6217417168101)) ;
#53287 = CARTESIAN_POINT('Ctrl Pts',(30.673617472207,534.2408508916,-47.621339455065)) ;
#53288 = CARTESIAN_POINT('Ctrl Pts',(30.7281687379782,534.270137831401,-47.6169585300456)) ;
#53289 = CARTESIAN_POINT('Ctrl Pts',(30.7811353217736,534.30253943713,-47.6125107004893)) ;
#53290 = CARTESIAN_POINT('Ctrl Pts',(30.8321791594224,534.337831003257,-47.6080652262423)) ;
#53291 = CARTESIAN_POINT('Ctrl Pts',(30.8831596432466,534.373078766727,-47.6036252695624)) ;
#53292 = CARTESIAN_POINT('Ctrl Pts',(30.9322224567569,534.411209093894,-47.599188003276)) ;
#53293 = CARTESIAN_POINT('Ctrl Pts',(30.9790590951107,534.451971645344,-47.5948018504151)) ;
#53294 = CARTESIAN_POINT('Ctrl Pts',(31.0258522993938,534.492696395543,-47.5904197650637)) ;
#53295 = CARTESIAN_POINT('Ctrl Pts',(31.0704235967529,534.536048447987,-47.5860888350347)) ;
#53296 = CARTESIAN_POINT('Ctrl Pts',(31.1124902383189,534.581753621128,-47.5818332950153)) ;
#53297 = CARTESIAN_POINT('Ctrl Pts',(31.1545310584144,534.627430739385,-47.577580367144)) ;
#53298 = CARTESIAN_POINT('Ctrl Pts',(31.1940702760404,534.675458143157,-47.57340272979)) ;
#53299 = CARTESIAN_POINT('Ctrl Pts',(31.2308496570034,534.725537499311,-47.5692996009665)) ;
#53300 = CARTESIAN_POINT('Ctrl Pts',(31.2676321070151,534.775621034328,-47.5651961297582)) ;
#53301 = CARTESIAN_POINT('Ctrl Pts',(31.3016540857673,534.827756975292,-47.5611670452076)) ;
#53302 = CARTESIAN_POINT('Ctrl Pts',(31.3326827611293,534.881620991051,-47.5571876285342)) ;
#53303 = CARTESIAN_POINT('Ctrl Pts',(31.3637101458964,534.93548276641,-47.5532083773791)) ;
#53304 = CARTESIAN_POINT('Ctrl Pts',(31.3917441313433,534.991072611886,-47.549278497494)) ;
#53305 = CARTESIAN_POINT('Ctrl Pts',(31.4165812310452,535.048038404901,-47.545352497709)) ;
#53306 = CARTESIAN_POINT('Ctrl Pts',(31.4414428254077,535.105060378299,-47.5414226260537)) ;
#53307 = CARTESIAN_POINT('Ctrl Pts',(31.4631006511519,535.163461117163,-47.5374961381248)) ;
#53308 = CARTESIAN_POINT('Ctrl Pts',(31.4813868456706,535.22285764003,-47.5335125036937)) ;
#53309 = CARTESIAN_POINT('Ctrl Pts',(31.4984440040268,535.27826205429,-47.5297966139138)) ;
#53310 = CARTESIAN_POINT('Ctrl Pts',(31.5125673198299,535.33453253182,-47.5260303504884)) ;
#53311 = CARTESIAN_POINT('Ctrl Pts',(31.5236569526584,535.391334705934,-47.522160171753)) ;
#53312 = CARTESIAN_POINT('Origin',(29.8885276254069,535.710565160562,-47.522160171753)) ;
#53313 = CARTESIAN_POINT('Ctrl Pts',(31.4519498042747,536.286123229417,-48.3557322092704)) ;
#53314 = CARTESIAN_POINT('Ctrl Pts',(31.4435375980647,536.308973799105,-48.3541129334884)) ;
#53315 = CARTESIAN_POINT('Ctrl Pts',(31.4346247554841,536.331639052111,-48.3524768959164)) ;
#53316 = CARTESIAN_POINT('Ctrl Pts',(31.3980363936659,536.419007631093,-48.3460474798456)) ;
#53317 = CARTESIAN_POINT('Ctrl Pts',(31.3667745744052,536.482116170551,-48.3411329619198)) ;
#53318 = CARTESIAN_POINT('Ctrl Pts',(31.2795416155593,536.633332059891,-48.3286756769509)) ;
#53319 = CARTESIAN_POINT('Ctrl Pts',(31.2191064536547,536.718521459963,-48.3210228426008)) ;
#53320 = CARTESIAN_POINT('Ctrl Pts',(31.1140768495141,536.840524596727,-48.3093794549558)) ;
#53321 = CARTESIAN_POINT('Ctrl Pts',(31.0748574789422,536.881633916768,-48.3053192228784)) ;
#53322 = CARTESIAN_POINT('Ctrl Pts',(31.0116610518251,536.941435006098,-48.2992914617993)) ;
#53323 = CARTESIAN_POINT('Ctrl Pts',(30.9891472863017,536.961607208327,-48.2972363119432)) ;
#53324 = CARTESIAN_POINT('Ctrl Pts',(30.9341002736848,537.008291419052,-48.2924405283549)) ;
#53325 = CARTESIAN_POINT('Ctrl Pts',(30.9010916999685,537.034207987955,-48.2897378805944)) ;
#53326 = CARTESIAN_POINT('Ctrl Pts',(30.8187997554234,537.093936790622,-48.28331051432)) ;
#53327 = CARTESIAN_POINT('Ctrl Pts',(30.768607921265,537.12639810772,-48.279641766959)) ;
#53328 = CARTESIAN_POINT('Ctrl Pts',(30.6079765977659,537.218435592228,-48.2683224233389)) ;
#53329 = CARTESIAN_POINT('Ctrl Pts',(30.49249755534,537.26828679375,-48.2607328450771)) ;
#53330 = CARTESIAN_POINT('Ctrl Pts',(30.3233801460445,537.319632298555,-48.2493791966046)) ;
#53331 = CARTESIAN_POINT('Ctrl Pts',(30.2735774770622,537.332270874295,-48.2460138389042)) ;
#53332 = CARTESIAN_POINT('Ctrl Pts',(30.1662553931302,537.354283897131,-48.2386681198289)) ;
#53333 = CARTESIAN_POINT('Ctrl Pts',(30.1086692273945,537.362981636789,-48.234670290237)) ;
#53334 = CARTESIAN_POINT('Ctrl Pts',(29.9816941536233,537.375404675195,-48.2257163471331)) ;
#53335 = CARTESIAN_POINT('Ctrl Pts',(29.9122886418477,537.377839663216,-48.2207312683048)) ;
#53336 = CARTESIAN_POINT('Ctrl Pts',(29.7256897867378,537.372731736576,-48.2071828687329)) ;
#53337 = CARTESIAN_POINT('Ctrl Pts',(29.6090995680451,537.357148793933,-48.1985461025743)) ;
#53338 = CARTESIAN_POINT('Ctrl Pts',(29.465816766739,537.322328208713,-48.1883170822733)) ;
#53339 = CARTESIAN_POINT('Ctrl Pts',(29.4367215658954,537.314415671059,-48.186263453143)) ;
#53340 = CARTESIAN_POINT('Ctrl Pts',(29.3690785968729,537.294032412185,-48.181561139837)) ;
#53341 = CARTESIAN_POINT('Ctrl Pts',(29.3307406787046,537.280937800884,-48.1789454749204)) ;
#53342 = CARTESIAN_POINT('Ctrl Pts',(29.2404289822054,537.246365458977,-48.1728177249305)) ;
#53343 = CARTESIAN_POINT('Ctrl Pts',(29.1889900644198,537.223629098726,-48.1693545796757)) ;
#53344 = CARTESIAN_POINT('Ctrl Pts',(29.0184835421417,537.137705722292,-48.1576654452413)) ;
#53345 = CARTESIAN_POINT('Ctrl Pts',(28.905982853372,537.062714884904,-48.1495440974203)) ;
#53346 = CARTESIAN_POINT('Ctrl Pts',(28.7654839429592,536.942177865081,-48.1376246569897)) ;
#53347 = CARTESIAN_POINT('Ctrl Pts',(28.7287393246251,536.907639573054,-48.1343144477807)) ;
#53348 = CARTESIAN_POINT('Ctrl Pts',(28.6522413966884,536.828902485285,-48.1269414072774)) ;
#53349 = CARTESIAN_POINT('Ctrl Pts',(28.6131748790197,536.784136694127,-48.1228542724197)) ;
#53350 = CARTESIAN_POINT('Ctrl Pts',(28.5320725015873,536.680514248351,-48.1135992380317)) ;
#53351 = CARTESIAN_POINT('Ctrl Pts',(28.4913098596715,536.620813678713,-48.108397049967)) ;
#53352 = CARTESIAN_POINT('Ctrl Pts',(28.3991304209052,536.464955397473,-48.0952380751858)) ;
#53353 = CARTESIAN_POINT('Ctrl Pts',(28.353023778856,536.366034576115,-48.0872442426966)) ;
#53354 = CARTESIAN_POINT('Ctrl Pts',(28.3066145792634,536.234079826741,-48.0775153206307)) ;
#53355 = CARTESIAN_POINT('Ctrl Pts',(28.2971483976233,536.204558351429,-48.0753977671491)) ;
#53356 = CARTESIAN_POINT('Ctrl Pts',(28.2776526871594,536.137362750658,-48.0707307657612)) ;
#53357 = CARTESIAN_POINT('Ctrl Pts',(28.2681104947567,536.099567977191,-48.0682063745697)) ;
#53358 = CARTESIAN_POINT('Ctrl Pts',(28.2488134287677,536.010005988046,-48.0623835007591)) ;
#53359 = CARTESIAN_POINT('Ctrl Pts',(28.2401698091122,535.958041923795,-48.0591271252558)) ;
#53360 = CARTESIAN_POINT('Ctrl Pts',(28.2180401003055,535.770457042348,-48.0475397746605)) ;
#53361 = CARTESIAN_POINT('Ctrl Pts',(28.2187345711917,535.633727927844,-48.0393577355581)) ;
#53362 = CARTESIAN_POINT('Ctrl Pts',(28.2426459436233,535.447306795531,-48.0273042054568)) ;
#53363 = CARTESIAN_POINT('Ctrl Pts',(28.2516115785173,535.396341737346,-48.0239206118743)) ;
#53364 = CARTESIAN_POINT('Ctrl Pts',(28.2754750864591,535.289969296684,-48.0166220183331)) ;
#53365 = CARTESIAN_POINT('Ctrl Pts',(28.2908927234949,535.234749339229,-48.0126936576772)) ;
#53366 = CARTESIAN_POINT('Ctrl Pts',(28.3305243776014,535.116674810865,-48.0039690553726)) ;
#53367 = CARTESIAN_POINT('Ctrl Pts',(28.3557662184974,535.054272026154,-47.9991477148186)) ;
#53368 = CARTESIAN_POINT('Ctrl Pts',(28.4353701154607,534.887311186294,-47.9857406464015)) ;
#53369 = CARTESIAN_POINT('Ctrl Pts',(28.4971543769131,534.786715967458,-47.9770636544323)) ;
#53370 = CARTESIAN_POINT('Ctrl Pts',(28.5882917440669,534.668481620317,-47.9666595873728)) ;
#53371 = CARTESIAN_POINT('Ctrl Pts',(28.6082622562069,534.644041522845,-47.9644987882644)) ;
#53372 = CARTESIAN_POINT('Ctrl Pts',(28.6536053052531,534.591661424027,-47.9598685952331)) ;
#53373 = CARTESIAN_POINT('Ctrl Pts',(28.6792559040783,534.563987127291,-47.9574184549172)) ;
#53374 = CARTESIAN_POINT('Ctrl Pts',(28.7409596624373,534.501792156922,-47.9518353684137)) ;
#53375 = CARTESIAN_POINT('Ctrl Pts',(28.7776682006956,534.467972525959,-47.9487394549282)) ;
#53376 = CARTESIAN_POINT('Ctrl Pts',(28.9305656981363,534.339307778057,-47.9364546280536)) ;
#53377 = CARTESIAN_POINT('Ctrl Pts',(29.057784187646,534.258704192475,-47.9274846601584)) ;
#53378 = CARTESIAN_POINT('Ctrl Pts',(29.2399660973278,534.175158470707,-47.9145414001103)) ;
#53379 = CARTESIAN_POINT('Ctrl Pts',(29.2867935212821,534.156209699931,-47.9112147795177)) ;
#53380 = CARTESIAN_POINT('Ctrl Pts',(29.3927751972407,534.11883138921,-47.9036431981116)) ;
#53381 = CARTESIAN_POINT('Ctrl Pts',(29.4522396252813,534.101516399241,-47.8993656143163)) ;
#53382 = CARTESIAN_POINT('Ctrl Pts',(29.66974165479,534.051127598483,-47.8835975082911)) ;
#53383 = CARTESIAN_POINT('Ctrl Pts',(29.8313899202287,534.037745769076,-47.8715536681794)) ;
#53384 = CARTESIAN_POINT('Ctrl Pts',(30.0285574105528,534.050065737868,-47.8576182398169)) ;
#53385 = CARTESIAN_POINT('Ctrl Pts',(30.0646107414035,534.05350090764,-47.8551065105941)) ;
#53386 = CARTESIAN_POINT('Ctrl Pts',(30.1324093343848,534.062199020259,-47.8504868905879)) ;
#53387 = CARTESIAN_POINT('Ctrl Pts',(30.1641679603495,534.067211327545,-47.8483689220744)) ;
#53388 = CARTESIAN_POINT('Ctrl Pts',(30.2335954821385,534.080238250613,-47.8438022911596)) ;
#53389 = CARTESIAN_POINT('Ctrl Pts',(30.2711731263722,534.088646382792,-47.8413717662144)) ;
#53390 = CARTESIAN_POINT('Ctrl Pts',(30.3973734928361,534.121515201023,-47.8332472451969)) ;
#53391 = CARTESIAN_POINT('Ctrl Pts',(30.4842523194431,534.152002534313,-47.8277112406882)) ;
#53392 = CARTESIAN_POINT('Ctrl Pts',(30.645469916295,534.224038501226,-47.8168750338328)) ;
#53393 = CARTESIAN_POINT('Ctrl Pts',(30.7200094252909,534.264412170001,-47.8116064339739)) ;
#53394 = CARTESIAN_POINT('Ctrl Pts',(30.833231439325,534.337394745914,-47.8028941814984)) ;
#53395 = CARTESIAN_POINT('Ctrl Pts',(30.8740615324785,534.366398397338,-47.7995909204402)) ;
#53396 = CARTESIAN_POINT('Ctrl Pts',(30.9629568464386,534.435774865285,-47.7919828115356)) ;
#53397 = CARTESIAN_POINT('Ctrl Pts',(31.0101687469789,534.477111538993,-47.787640975437)) ;
#53398 = CARTESIAN_POINT('Ctrl Pts',(31.1379081208986,534.60236466765,-47.7749820022143)) ;
#53399 = CARTESIAN_POINT('Ctrl Pts',(31.2121359025443,534.692176375442,-47.7664459392426)) ;
#53400 = CARTESIAN_POINT('Ctrl Pts',(31.3087781660287,534.837714150281,-47.753782702513)) ;
#53401 = CARTESIAN_POINT('Ctrl Pts',(31.3385622549675,534.888141037319,-47.7495846721178)) ;
#53402 = CARTESIAN_POINT('Ctrl Pts',(31.3796701118715,534.966944804672,-47.7434086604974)) ;
#53403 = CARTESIAN_POINT('Ctrl Pts',(31.3929709952149,534.994235706057,-47.7413374390977)) ;
#53404 = CARTESIAN_POINT('Ctrl Pts',(31.4221282223764,535.058461507149,-47.7366349899464)) ;
#53405 = CARTESIAN_POINT('Ctrl Pts',(31.4374083891385,535.095635077976,-47.7340347120364)) ;
#53406 = CARTESIAN_POINT('Ctrl Pts',(31.4704882920144,535.185195183456,-47.7279713655755)) ;
#53407 = CARTESIAN_POINT('Ctrl Pts',(31.487053207048,535.237987156671,-47.7245549000931)) ;
#53408 = CARTESIAN_POINT('Ctrl Pts',(31.5352891797283,535.423588236114,-47.7127863493649)) ;
#53409 = CARTESIAN_POINT('Ctrl Pts',(31.5532545328925,535.559370104463,-47.7045493541162)) ;
#53410 = CARTESIAN_POINT('Ctrl Pts',(31.5549141180346,535.746853850405,-47.6924529456395)) ;
#53411 = CARTESIAN_POINT('Ctrl Pts',(31.5530204561047,535.797877709024,-47.6890942462937)) ;
#53412 = CARTESIAN_POINT('Ctrl Pts',(31.5437271359293,535.909551101256,-47.6815511577299)) ;
#53413 = CARTESIAN_POINT('Ctrl Pts',(31.535328088606,535.970040391314,-47.6773389707263)) ;
#53414 = CARTESIAN_POINT('Ctrl Pts',(31.5066058944178,536.117095652395,-47.6667710894643)) ;
#53415 = CARTESIAN_POINT('Ctrl Pts',(31.4826388185315,536.20275469549,-47.6603239369838)) ;
#53416 = CARTESIAN_POINT('Ctrl Pts',(31.451963599978,536.286085753953,-47.6538547791721)) ;
#53417 = CARTESIAN_POINT('Origin',(29.8885276254069,535.710565160562,-48.522160171753)) ;
#53418 = CARTESIAN_POINT('',(31.4519498093678,536.286123215583,-49.053781357604)) ;
#53419 = CARTESIAN_POINT('',(31.451949809446,536.28612321537,-48.8631108318347)) ;
#53420 = CARTESIAN_POINT('',(31.4519498093678,536.286123215583,-48.5221601717531)) ;
#53421 = CARTESIAN_POINT('',(31.5549889082353,535.711664315652,-49.0928401252964)) ;
#53422 = CARTESIAN_POINT('Ctrl Pts',(31.5545272755358,535.711644868924,-49.0925752748111)) ;
#53423 = CARTESIAN_POINT('Ctrl Pts',(31.55449757292,535.757476270547,-49.0892618616175)) ;
#53424 = CARTESIAN_POINT('Ctrl Pts',(31.5525766500511,535.803290525822,-49.0859760681493)) ;
#53425 = CARTESIAN_POINT('Ctrl Pts',(31.5462160716639,535.879588900661,-49.0806023568414)) ;
#53426 = CARTESIAN_POINT('Ctrl Pts',(31.542816820287,535.910133684156,-49.0784777929953)) ;
#53427 = CARTESIAN_POINT('Ctrl Pts',(31.5341919410292,535.97200840949,-49.0742513050239)) ;
#53428 = CARTESIAN_POINT('Ctrl Pts',(31.5289119118011,536.003316152231,-49.0721567469035)) ;
#53429 = CARTESIAN_POINT('Ctrl Pts',(31.5057653726932,536.120103714187,-49.0644503423696)) ;
#53430 = CARTESIAN_POINT('Ctrl Pts',(31.4820903240614,536.204250763452,-49.0591060070419)) ;
#53431 = CARTESIAN_POINT('Ctrl Pts',(31.4519498093678,536.286123215583,-49.053781357604)) ;
#53432 = CARTESIAN_POINT('',(28.6194567455546,536.789923813611,-49.5221601717529)) ;
#53433 = CARTESIAN_POINT('Ctrl Pts',(31.5549889082353,535.711664315652,-49.0928401252965)) ;
#53434 = CARTESIAN_POINT('Ctrl Pts',(31.5548945150024,535.651801552434,-49.0970896085957)) ;
#53435 = CARTESIAN_POINT('Ctrl Pts',(31.5515477486577,535.591838508281,-49.1013782898962)) ;
#53436 = CARTESIAN_POINT('Ctrl Pts',(31.5449734388419,535.532152475187,-49.1056462076814)) ;
#53437 = CARTESIAN_POINT('Ctrl Pts',(31.5384062586401,535.472531169551,-49.1099094970558)) ;
#53438 = CARTESIAN_POINT('Ctrl Pts',(31.5286187690042,535.413186238494,-49.1141518093791)) ;
#53439 = CARTESIAN_POINT('Ctrl Pts',(31.5156726607986,535.354485191027,-49.1183336692113)) ;
#53440 = CARTESIAN_POINT('Ctrl Pts',(31.5027355157954,535.295824785069,-49.1225126337444)) ;
#53441 = CARTESIAN_POINT('Ctrl Pts',(31.4866441943593,535.237807390759,-49.1266311311775)) ;
#53442 = CARTESIAN_POINT('Ctrl Pts',(31.4674949390496,535.180791368193,-49.1306726625041)) ;
#53443 = CARTESIAN_POINT('Ctrl Pts',(31.448351369271,535.123792274033,-49.1347129938754)) ;
#53444 = CARTESIAN_POINT('Ctrl Pts',(31.4261516385317,535.067794050184,-49.1386764271401)) ;
#53445 = CARTESIAN_POINT('Ctrl Pts',(31.4010264095637,535.013145512418,-49.1425699181009)) ;
#53446 = CARTESIAN_POINT('Ctrl Pts',(31.3758809737919,534.958453023916,-49.1464665403767)) ;
#53447 = CARTESIAN_POINT('Ctrl Pts',(31.3478051928575,534.905112567087,-49.1502932455774)) ;
#53448 = CARTESIAN_POINT('Ctrl Pts',(31.3169659928077,534.853462565541,-49.1540793082628)) ;
#53449 = CARTESIAN_POINT('Ctrl Pts',(31.2861153343653,534.801793373291,-49.1578667776706)) ;
#53450 = CARTESIAN_POINT('Ctrl Pts',(31.2524989797646,534.751816174951,-49.1616138642146)) ;
#53451 = CARTESIAN_POINT('Ctrl Pts',(31.2163227255207,534.703855161998,-49.1653690162118)) ;
#53452 = CARTESIAN_POINT('Ctrl Pts',(31.1800794842795,534.655805340396,-49.1691311215645)) ;
#53453 = CARTESIAN_POINT('Ctrl Pts',(31.1412665653164,534.609779650157,-49.1729018125606)) ;
#53454 = CARTESIAN_POINT('Ctrl Pts',(31.1001336553491,534.566083846947,-49.1767432173366)) ;
#53455 = CARTESIAN_POINT('Ctrl Pts',(31.0641191958142,534.527825412574,-49.1801066097387)) ;
#53456 = CARTESIAN_POINT('Ctrl Pts',(31.0263267587359,534.491353125802,-49.183524739968)) ;
#53457 = CARTESIAN_POINT('Ctrl Pts',(30.9869532174238,534.45685407754,-49.1870422345052)) ;
#53458 = CARTESIAN_POINT('Ctrl Pts',(30.9869288742596,534.45683274809,-49.1870444092384)) ;
#53459 = CARTESIAN_POINT('Ctrl Pts',(30.9869045304909,534.456811419392,-49.1870465840096)) ;
#53460 = CARTESIAN_POINT('Ctrl Pts',(30.9868801861176,534.456790091447,-49.1870487588188)) ;
#53461 = CARTESIAN_POINT('Ctrl Pts',(30.9451058127731,534.420191838465,-49.1907806803159)) ;
#53462 = CARTESIAN_POINT('Ctrl Pts',(30.9013837054678,534.385675350033,-49.1946349063943)) ;
#53463 = CARTESIAN_POINT('Ctrl Pts',(30.8559638071929,534.353423514733,-49.1985479657098)) ;
#53464 = CARTESIAN_POINT('Ctrl Pts',(30.851836545535,534.350492822056,-49.1989035415761)) ;
#53465 = CARTESIAN_POINT('Ctrl Pts',(30.8476953004339,534.347580830664,-49.199259603239)) ;
#53466 = CARTESIAN_POINT('Ctrl Pts',(30.8435402806864,534.344687678229,-49.1996161030745)) ;
#53467 = CARTESIAN_POINT('Ctrl Pts',(30.7930414398575,534.309525187273,-49.2039488931799)) ;
#53468 = CARTESIAN_POINT('Ctrl Pts',(30.7405019731692,534.277144757969,-49.2083457443779)) ;
#53469 = CARTESIAN_POINT('Ctrl Pts',(30.6862764220024,534.247746870581,-49.212735632841)) ;
#53470 = CARTESIAN_POINT('Ctrl Pts',(30.6328585556239,534.218786862126,-49.2170601343038)) ;
#53471 = CARTESIAN_POINT('Ctrl Pts',(30.5778045801627,534.192720780501,-49.2213776000998)) ;
#53472 = CARTESIAN_POINT('Ctrl Pts',(30.5214645329549,534.169702898285,-49.2256408785573)) ;
#53473 = CARTESIAN_POINT('Ctrl Pts',(30.4651572114663,534.146698386252,-49.2299016806438)) ;
#53474 = CARTESIAN_POINT('Ctrl Pts',(30.4075653302754,534.126738409008,-49.2341082270902)) ;
#53475 = CARTESIAN_POINT('Ctrl Pts',(30.3490485980044,534.109943273336,-49.2382373652898)) ;
#53476 = CARTESIAN_POINT('Ctrl Pts',(30.2905440138085,534.093151624335,-49.2423656462802)) ;
#53477 = CARTESIAN_POINT('Ctrl Pts',(30.2311149728027,534.079523540889,-49.2464165514128)) ;
#53478 = CARTESIAN_POINT('Ctrl Pts',(30.1711310570779,534.069146167981,-49.2503918060323)) ;
#53479 = CARTESIAN_POINT('Ctrl Pts',(30.1094908279039,534.058482248553,-49.2544768278722)) ;
#53480 = CARTESIAN_POINT('Ctrl Pts',(30.0472646332882,534.051251403299,-49.2584819767203)) ;
#53481 = CARTESIAN_POINT('Ctrl Pts',(29.9848643783669,534.047510007894,-49.2624354936015)) ;
#53482 = CARTESIAN_POINT('Ctrl Pts',(29.924057600434,534.043864154206,-49.26628805195)) ;
#53483 = CARTESIAN_POINT('Ctrl Pts',(29.8630856380362,534.043531974582,-49.2700919530291)) ;
#53484 = CARTESIAN_POINT('Ctrl Pts',(29.8023391303135,534.046526464964,-49.2738948198168)) ;
#53485 = CARTESIAN_POINT('Ctrl Pts',(29.7392047762322,534.04963866389,-49.2778471711089)) ;
#53486 = CARTESIAN_POINT('Ctrl Pts',(29.6763140819269,534.056345093778,-49.2817988336936)) ;
#53487 = CARTESIAN_POINT('Ctrl Pts',(29.6141145081114,534.06660895403,-49.2858211495323)) ;
#53488 = CARTESIAN_POINT('Ctrl Pts',(29.560439537276,534.075466127253,-49.2892921971954)) ;
#53489 = CARTESIAN_POINT('Ctrl Pts',(29.5072782483975,534.086972424484,-49.2928165217358)) ;
#53490 = CARTESIAN_POINT('Ctrl Pts',(29.454924530345,534.101065601861,-49.2964447278837)) ;
#53491 = CARTESIAN_POINT('Ctrl Pts',(29.4466432325861,534.103294857062,-49.2970186366061)) ;
#53492 = CARTESIAN_POINT('Ctrl Pts',(29.4383820438979,534.105588795292,-49.2975951445327)) ;
#53493 = CARTESIAN_POINT('Ctrl Pts',(29.430142016476,534.107947124849,-49.2981744519464)) ;
#53494 = CARTESIAN_POINT('Ctrl Pts',(29.4301087180222,534.107956655002,-49.298176792963)) ;
#53495 = CARTESIAN_POINT('Ctrl Pts',(29.4300754199139,534.107966186208,-49.2981791340253)) ;
#53496 = CARTESIAN_POINT('Ctrl Pts',(29.4300421221512,534.107975718464,-49.2981814751334)) ;
#53497 = CARTESIAN_POINT('Ctrl Pts',(29.3771816235799,534.12310826182,-49.3018980053008)) ;
#53498 = CARTESIAN_POINT('Ctrl Pts',(29.324995964791,534.140955723634,-49.3057400460438)) ;
#53499 = CARTESIAN_POINT('Ctrl Pts',(29.2737680915368,534.161411177651,-49.309644776254)) ;
#53500 = CARTESIAN_POINT('Ctrl Pts',(29.2687790857812,534.163403303643,-49.3100250520737)) ;
#53501 = CARTESIAN_POINT('Ctrl Pts',(29.2637991871285,534.165420131474,-49.3104059224729)) ;
#53502 = CARTESIAN_POINT('Ctrl Pts',(29.2588286712114,534.167461540257,-49.3107873294248)) ;
#53503 = CARTESIAN_POINT('Ctrl Pts',(29.2019109528873,534.190837852099,-49.3151548465633)) ;
#53504 = CARTESIAN_POINT('Ctrl Pts',(29.1462197990437,534.217442248767,-49.3195920236138)) ;
#53505 = CARTESIAN_POINT('Ctrl Pts',(29.0921183275704,534.247085215786,-49.3240255580288)) ;
#53506 = CARTESIAN_POINT('Ctrl Pts',(29.0390321042312,534.276171913888,-49.3283758943825)) ;
#53507 = CARTESIAN_POINT('Ctrl Pts',(28.9874761485506,534.308183841957,-49.3327224400922)) ;
#53508 = CARTESIAN_POINT('Ctrl Pts',(28.9377678747413,534.342912053716,-49.3370161818138)) ;
#53509 = CARTESIAN_POINT('Ctrl Pts',(28.8880908369075,534.377618442757,-49.3413072254089)) ;
#53510 = CARTESIAN_POINT('Ctrl Pts',(28.8402590636623,534.415037608316,-49.3455453887482)) ;
#53511 = CARTESIAN_POINT('Ctrl Pts',(28.7945664451433,534.454934033315,-49.3497053222925)) ;
#53512 = CARTESIAN_POINT('Ctrl Pts',(28.748885160238,534.49482056239,-49.3538642240053)) ;
#53513 = CARTESIAN_POINT('Ctrl Pts',(28.7053420043622,534.537183120873,-49.3579449241799)) ;
#53514 = CARTESIAN_POINT('Ctrl Pts',(28.6642081615329,534.58176007115,-49.3619467722947)) ;
#53515 = CARTESIAN_POINT('Ctrl Pts',(28.6216448854951,534.627886105312,-49.3660876877613)) ;
#53516 = CARTESIAN_POINT('Ctrl Pts',(28.5816616075933,534.676383345868,-49.3701441435676)) ;
#53517 = CARTESIAN_POINT('Ctrl Pts',(28.5445318003552,534.726931753464,-49.3741424304751)) ;
#53518 = CARTESIAN_POINT('Ctrl Pts',(28.5086016017281,534.775847017514,-49.3780115387049)) ;
#53519 = CARTESIAN_POINT('Ctrl Pts',(28.4753436174409,534.82668300498,-49.3818265568833)) ;
#53520 = CARTESIAN_POINT('Ctrl Pts',(28.4449778114948,534.879121020584,-49.3856331128046)) ;
#53521 = CARTESIAN_POINT('Ctrl Pts',(28.413091261842,534.934185173704,-49.3896303040733)) ;
#53522 = CARTESIAN_POINT('Ctrl Pts',(28.384394710758,534.9910162561,-49.3936185392059)) ;
#53523 = CARTESIAN_POINT('Ctrl Pts',(28.3591034283671,535.049209612495,-49.3976698686656)) ;
#53524 = CARTESIAN_POINT('Ctrl Pts',(28.3373126243316,535.099348629005,-49.4011604677176)) ;
#53525 = CARTESIAN_POINT('Ctrl Pts',(28.3180491561457,535.150499775786,-49.4046985677495)) ;
#53526 = CARTESIAN_POINT('Ctrl Pts',(28.3014210364866,535.202377708198,-49.4083359611142)) ;
#53527 = CARTESIAN_POINT('Ctrl Pts',(28.2987556707882,535.210693360502,-49.4089190086087)) ;
#53528 = CARTESIAN_POINT('Ctrl Pts',(28.2961579274069,535.219027748387,-49.4095046073204)) ;
#53529 = CARTESIAN_POINT('Ctrl Pts',(28.2936281503815,535.227379770461,-49.4100929705568)) ;
#53530 = CARTESIAN_POINT('Ctrl Pts',(28.2936226661343,535.227397876623,-49.4100942460564)) ;
#53531 = CARTESIAN_POINT('Ctrl Pts',(28.2936171822064,535.227415982868,-49.4100955215689)) ;
#53532 = CARTESIAN_POINT('Ctrl Pts',(28.293611698598,535.227434089197,-49.4100967970944)) ;
#53533 = CARTESIAN_POINT('Ctrl Pts',(28.2773215026631,535.281222691997,-49.4138860101986)) ;
#53534 = CARTESIAN_POINT('Ctrl Pts',(28.2638006114948,535.335934037994,-49.4177998091959)) ;
#53535 = CARTESIAN_POINT('Ctrl Pts',(28.2531113952247,535.391260793551,-49.4217758640599)) ;
#53536 = CARTESIAN_POINT('Ctrl Pts',(28.2520331872799,535.396841534542,-49.4221769237666)) ;
#53537 = CARTESIAN_POINT('Ctrl Pts',(28.2509837735385,535.402428496592,-49.4225786168961)) ;
#53538 = CARTESIAN_POINT('Ctrl Pts',(28.2499632061062,535.408021337453,-49.4229808794796)) ;
#53539 = CARTESIAN_POINT('Ctrl Pts',(28.2388485012066,535.468931350599,-49.4273618049979)) ;
#53540 = CARTESIAN_POINT('Ctrl Pts',(28.231156974193,535.530544371899,-49.4318096352455)) ;
#53541 = CARTESIAN_POINT('Ctrl Pts',(28.2269237227364,535.592455990411,-49.4362551103338)) ;
#53542 = CARTESIAN_POINT('Ctrl Pts',(28.2226957254514,535.654290766273,-49.4406950678456)) ;
#53543 = CARTESIAN_POINT('Ctrl Pts',(28.2219170560046,535.716423496026,-49.4451323351127)) ;
#53544 = CARTESIAN_POINT('Ctrl Pts',(28.2245843407441,535.778456896699,-49.4495184890573)) ;
#53545 = CARTESIAN_POINT('Ctrl Pts',(28.2272491519643,535.840432770401,-49.453900575481)) ;
#53546 = CARTESIAN_POINT('Ctrl Pts',(28.2333534079484,535.902309583222,-49.4582315066852)) ;
#53547 = CARTESIAN_POINT('Ctrl Pts',(28.242859035928,535.963695323706,-49.4624870479383)) ;
#53548 = CARTESIAN_POINT('Ctrl Pts',(28.2523588291084,536.025043384042,-49.4667399770305)) ;
#53549 = CARTESIAN_POINT('Ctrl Pts',(28.2652558739135,536.085900991523,-49.470917615664)) ;
#53550 = CARTESIAN_POINT('Ctrl Pts',(28.2814779304573,536.145880242774,-49.4750207457855)) ;
#53551 = CARTESIAN_POINT('Ctrl Pts',(28.2977013405527,536.205864498632,-49.479124218268)) ;
#53552 = CARTESIAN_POINT('Ctrl Pts',(28.3172505126246,536.264970184918,-49.4831533041118)) ;
#53553 = CARTESIAN_POINT('Ctrl Pts',(28.3400170427953,536.322813048898,-49.4871327220622)) ;
#53554 = CARTESIAN_POINT('Ctrl Pts',(28.3627826259513,536.3806535068,-49.4911119744816)) ;
#53555 = CARTESIAN_POINT('Ctrl Pts',(28.3887656233382,536.437231064484,-49.4950418556151)) ;
#53556 = CARTESIAN_POINT('Ctrl Pts',(28.4178176061229,536.49216708494,-49.4989678566015)) ;
#53557 = CARTESIAN_POINT('Ctrl Pts',(28.4468982401289,536.547157283593,-49.5028977294311)) ;
#53558 = CARTESIAN_POINT('Ctrl Pts',(28.4790543540341,536.600502320741,-49.5068242184869)) ;
#53559 = CARTESIAN_POINT('Ctrl Pts',(28.5140911814731,536.651832170997,-49.5108078539714)) ;
#53560 = CARTESIAN_POINT('Ctrl Pts',(28.5467730958851,536.699712013306,-49.514523739326)) ;
#53561 = CARTESIAN_POINT('Ctrl Pts',(28.5819613399247,536.745838071324,-49.5182899981151)) ;
#53562 = CARTESIAN_POINT('Ctrl Pts',(28.6194567455546,536.789923813611,-49.5221601717528)) ;
#53563 = CARTESIAN_POINT('',(31.1431801000586,536.807976208783,-49.5221526632306)) ;
#53564 = CARTESIAN_POINT('Origin',(29.8885276254068,535.710565160562,-49.522160171753)) ;
#53565 = CARTESIAN_POINT('',(31.5540494077382,535.71142659878,-48.8998528498641)) ;
#53566 = CARTESIAN_POINT('Ctrl Pts',(31.1431801122076,536.807976219409,-49.5221526630917)) ;
#53567 = CARTESIAN_POINT('Ctrl Pts',(31.1083565274205,536.847742286154,-49.5185433692491)) ;
#53568 = CARTESIAN_POINT('Ctrl Pts',(31.0715379965842,536.885881586539,-49.5148367719832)) ;
#53569 = CARTESIAN_POINT('Ctrl Pts',(31.0329178907796,536.922204517176,-49.5110871617097)) ;
#53570 = CARTESIAN_POINT('Ctrl Pts',(30.9888693681021,536.963632975243,-49.5068105086626)) ;
#53571 = CARTESIAN_POINT('Ctrl Pts',(30.9424762407452,537.002699349067,-49.5024784623692)) ;
#53572 = CARTESIAN_POINT('Ctrl Pts',(30.894041810257,537.03916323982,-49.4981571537409)) ;
#53573 = CARTESIAN_POINT('Ctrl Pts',(30.8456567620084,537.075589953124,-49.4938402509847)) ;
#53574 = CARTESIAN_POINT('Ctrl Pts',(30.7952347034472,537.109419769151,-49.4895343620322)) ;
#53575 = CARTESIAN_POINT('Ctrl Pts',(30.7430951129014,537.140447259709,-49.4852846612071)) ;
#53576 = CARTESIAN_POINT('Ctrl Pts',(30.6909888978209,537.171454889028,-49.4810376806901)) ;
#53577 = CARTESIAN_POINT('Ctrl Pts',(30.6371673879947,537.199663874653,-49.4768469345805)) ;
#53578 = CARTESIAN_POINT('Ctrl Pts',(30.581965351342,537.224900595741,-49.4727337206037)) ;
#53579 = CARTESIAN_POINT('Ctrl Pts',(30.5267777051169,537.250130737957,-49.4686215788865)) ;
#53580 = CARTESIAN_POINT('Ctrl Pts',(30.4702102626389,537.272390107686,-49.4645869194723)) ;
#53581 = CARTESIAN_POINT('Ctrl Pts',(30.4126130901018,537.291536378296,-49.4606264509924)) ;
#53582 = CARTESIAN_POINT('Ctrl Pts',(30.3549673948026,537.310698778691,-49.4566626460141)) ;
#53583 = CARTESIAN_POINT('Ctrl Pts',(30.2962902352208,537.326742637295,-49.4527730331063)) ;
#53584 = CARTESIAN_POINT('Ctrl Pts',(30.2369480740712,537.33955838851,-49.4489306788226)) ;
#53585 = CARTESIAN_POINT('Ctrl Pts',(30.1775836267898,537.35237895272,-49.4450868815308)) ;
#53586 = CARTESIAN_POINT('Ctrl Pts',(30.1175536955959,537.361968645317,-49.4412901053197)) ;
#53587 = CARTESIAN_POINT('Ctrl Pts',(30.0572405651505,537.368254886535,-49.4374926831251)) ;
#53588 = CARTESIAN_POINT('Ctrl Pts',(29.9968128635493,537.374553069131,-49.4336880473262)) ;
#53589 = CARTESIAN_POINT('Ctrl Pts',(29.9361009840112,537.377534707185,-49.4298822893108)) ;
#53590 = CARTESIAN_POINT('Ctrl Pts',(29.8755041032753,537.377170570117,-49.4260122312284)) ;
#53591 = CARTESIAN_POINT('Ctrl Pts',(29.8210497178999,537.376843344359,-49.422534467494)) ;
#53592 = CARTESIAN_POINT('Ctrl Pts',(29.7666878020697,537.373814310548,-49.4190041894054)) ;
#53593 = CARTESIAN_POINT('Ctrl Pts',(29.7127183637283,537.368098938728,-49.4153710491561)) ;
#53594 = CARTESIAN_POINT('Ctrl Pts',(29.707871034377,537.367585605804,-49.4150447343397)) ;
#53595 = CARTESIAN_POINT('Ctrl Pts',(29.7030268418567,537.367050621183,-49.4147175897395)) ;
#53596 = CARTESIAN_POINT('Ctrl Pts',(29.6981859859229,537.366494006858,-49.4143895788765)) ;
#53597 = CARTESIAN_POINT('Ctrl Pts',(29.698153754034,537.366490300751,-49.4143873948805)) ;
#53598 = CARTESIAN_POINT('Ctrl Pts',(29.6981215222931,537.366486593685,-49.4143852108462)) ;
#53599 = CARTESIAN_POINT('Ctrl Pts',(29.6980892907001,537.36648288566,-49.4143830267734)) ;
#53600 = CARTESIAN_POINT('Ctrl Pts',(29.6429162247681,537.360135600715,-49.4106443970974)) ;
#53601 = CARTESIAN_POINT('Ctrl Pts',(29.5879781605852,537.350947335582,-49.4067833237044)) ;
#53602 = CARTESIAN_POINT('Ctrl Pts',(29.5335777348821,537.338980388243,-49.4028628644713)) ;
#53603 = CARTESIAN_POINT('Ctrl Pts',(29.5285151673266,537.337866730059,-49.4024980219272)) ;
#53604 = CARTESIAN_POINT('Ctrl Pts',(29.5234572819973,537.336729034071,-49.4021326650789)) ;
#53605 = CARTESIAN_POINT('Ctrl Pts',(29.5184043383932,537.335567367242,-49.4017668447478)) ;
#53606 = CARTESIAN_POINT('Ctrl Pts',(29.4584525440487,537.321784507932,-49.3974264865378)) ;
#53607 = CARTESIAN_POINT('Ctrl Pts',(29.3991919237932,537.304623258597,-49.3930215428258)) ;
#53608 = CARTESIAN_POINT('Ctrl Pts',(29.3410079109624,537.284211436378,-49.3886228235456)) ;
#53609 = CARTESIAN_POINT('Ctrl Pts',(29.283564807459,537.264059536236,-49.3842801171112)) ;
#53610 = CARTESIAN_POINT('Ctrl Pts',(29.2271708358056,537.240739690067,-49.3799437695657)) ;
#53611 = CARTESIAN_POINT('Ctrl Pts',(29.1721765345475,537.214408245045,-49.3756613760682)) ;
#53612 = CARTESIAN_POINT('Ctrl Pts',(29.1172154023898,537.188092681492,-49.3713815654409)) ;
#53613 = CARTESIAN_POINT('Ctrl Pts',(29.0636521680889,537.158769250228,-49.3671557788563)) ;
#53614 = CARTESIAN_POINT('Ctrl Pts',(29.0118186029896,537.126624263931,-49.3630077155754)) ;
#53615 = CARTESIAN_POINT('Ctrl Pts',(28.9599971726063,537.094486803072,-49.3588606233943)) ;
#53616 = CARTESIAN_POINT('Ctrl Pts',(28.9099046329241,537.059529090471,-49.3547912200999)) ;
#53617 = CARTESIAN_POINT('Ctrl Pts',(28.8618547835675,537.021966993312,-49.3507983884807)) ;
#53618 = CARTESIAN_POINT('Ctrl Pts',(28.8126618845849,536.983511337865,-49.3467105720748)) ;
#53619 = CARTESIAN_POINT('Ctrl Pts',(28.7656102528472,536.942325674075,-49.3427029869773)) ;
#53620 = CARTESIAN_POINT('Ctrl Pts',(28.7210159321545,536.898674881616,-49.3387484432116)) ;
#53621 = CARTESIAN_POINT('Ctrl Pts',(28.6774021379088,536.855983869591,-49.3348808507591)) ;
#53622 = CARTESIAN_POINT('Ctrl Pts',(28.6361389815893,536.810934885481,-49.3310636388541)) ;
#53623 = CARTESIAN_POINT('Ctrl Pts',(28.5974995922091,536.763808969429,-49.3272499272855)) ;
#53624 = CARTESIAN_POINT('Ctrl Pts',(28.5575571652059,536.715093824286,-49.3233076057742)) ;
#53625 = CARTESIAN_POINT('Ctrl Pts',(28.5204191540007,536.664158850631,-49.319368594247)) ;
#53626 = CARTESIAN_POINT('Ctrl Pts',(28.4863559239369,536.611354798058,-49.315363497479)) ;
#53627 = CARTESIAN_POINT('Ctrl Pts',(28.4567192744058,536.565412730996,-49.3118788705359)) ;
#53628 = CARTESIAN_POINT('Ctrl Pts',(28.4294095880391,536.518055123191,-49.3083435685584)) ;
#53629 = CARTESIAN_POINT('Ctrl Pts',(28.4045804526383,536.469543561243,-49.3047069758659)) ;
#53630 = CARTESIAN_POINT('Ctrl Pts',(28.400885802758,536.462324895202,-49.3041658399569)) ;
#53631 = CARTESIAN_POINT('Ctrl Pts',(28.3972459921483,536.455080639415,-49.303622461235)) ;
#53632 = CARTESIAN_POINT('Ctrl Pts',(28.3936614376786,536.447811612819,-49.3030766729295)) ;
#53633 = CARTESIAN_POINT('Ctrl Pts',(28.3936479789086,536.447784320122,-49.3030746236821)) ;
#53634 = CARTESIAN_POINT('Ctrl Pts',(28.3936345209176,536.447757027077,-49.3030725744006)) ;
#53635 = CARTESIAN_POINT('Ctrl Pts',(28.3936210637055,536.447729733682,-49.3030705250852)) ;
#53636 = CARTESIAN_POINT('Ctrl Pts',(28.3691053918656,536.398008000487,-49.2993371853412)) ;
#53637 = CARTESIAN_POINT('Ctrl Pts',(28.3470945059155,536.346945626636,-49.295481286779)) ;
#53638 = CARTESIAN_POINT('Ctrl Pts',(28.3277004536284,536.294829589099,-49.2915660505046)) ;
#53639 = CARTESIAN_POINT('Ctrl Pts',(28.3259023440706,536.289997677551,-49.2912030513922)) ;
#53640 = CARTESIAN_POINT('Ctrl Pts',(28.3241267206343,536.28515674484,-49.2908395422142)) ;
#53641 = CARTESIAN_POINT('Ctrl Pts',(28.3223736671063,536.280307041621,-49.2904755733562)) ;
#53642 = CARTESIAN_POINT('Ctrl Pts',(28.3014560780051,536.222439955653,-49.2861326648845)) ;
#53643 = CARTESIAN_POINT('Ctrl Pts',(28.2837527935745,536.163318227504,-49.2817249759682)) ;
#53644 = CARTESIAN_POINT('Ctrl Pts',(28.2693664506353,536.103336017163,-49.2773238859157)) ;
#53645 = CARTESIAN_POINT('Ctrl Pts',(28.2551960586974,536.044254189806,-49.2729888598941)) ;
#53646 = CARTESIAN_POINT('Ctrl Pts',(28.2442433287989,535.984337528399,-49.2686605187971)) ;
#53647 = CARTESIAN_POINT('Ctrl Pts',(28.2365673045768,535.923963862056,-49.264386520501)) ;
#53648 = CARTESIAN_POINT('Ctrl Pts',(28.2288960412449,535.863627641189,-49.260115173061)) ;
#53649 = CARTESIAN_POINT('Ctrl Pts',(28.2244972935664,535.802834968857,-49.2558982350145)) ;
#53650 = CARTESIAN_POINT('Ctrl Pts',(28.2233947577476,535.741964260642,-49.2517595022522)) ;
#53651 = CARTESIAN_POINT('Ctrl Pts',(28.2222924944977,535.681108600886,-49.2476217926676)) ;
#53652 = CARTESIAN_POINT('Ctrl Pts',(28.2244848456945,535.620174964973,-49.2435622517888)) ;
#53653 = CARTESIAN_POINT('Ctrl Pts',(28.2299609162811,535.559542739129,-49.2395799019118)) ;
#53654 = CARTESIAN_POINT('Ctrl Pts',(28.2355899482467,535.497216892151,-49.2354863142924)) ;
#53655 = CARTESIAN_POINT('Ctrl Pts',(28.2446890651011,535.435209601131,-49.2314742813798)) ;
#53656 = CARTESIAN_POINT('Ctrl Pts',(28.2572067248696,535.373933582006,-49.2275164187219)) ;
#53657 = CARTESIAN_POINT('Ctrl Pts',(28.269399732289,535.314246789933,-49.2236612053957)) ;
#53658 = CARTESIAN_POINT('Ctrl Pts',(28.2848363846619,535.255253970115,-49.2198570207253)) ;
#53659 = CARTESIAN_POINT('Ctrl Pts',(28.3034288465167,535.197335591793,-49.21605708333)) ;
#53660 = CARTESIAN_POINT('Ctrl Pts',(28.3227638757555,535.137104001859,-49.2121053796116)) ;
#53661 = CARTESIAN_POINT('Ctrl Pts',(28.3455126512619,535.078034749291,-49.2081578506276)) ;
#53662 = CARTESIAN_POINT('Ctrl Pts',(28.3715245405358,535.020551048144,-49.2041438876027)) ;
#53663 = CARTESIAN_POINT('Ctrl Pts',(28.3940266130001,534.970823694814,-49.2006715336377)) ;
#53664 = CARTESIAN_POINT('Ctrl Pts',(28.4189708581868,534.922281953056,-49.1971488057963)) ;
#53665 = CARTESIAN_POINT('Ctrl Pts',(28.4462206482126,534.875195835559,-49.193525032886)) ;
#53666 = CARTESIAN_POINT('Ctrl Pts',(28.4504560760141,534.86787725252,-49.1929617908017)) ;
#53667 = CARTESIAN_POINT('Ctrl Pts',(28.4547471865727,534.860593733717,-49.1923961076298)) ;
#53668 = CARTESIAN_POINT('Ctrl Pts',(28.4590934528131,534.853346180448,-49.1918277931033)) ;
#53669 = CARTESIAN_POINT('Ctrl Pts',(28.4591087695015,534.853320639326,-49.1918257903045)) ;
#53670 = CARTESIAN_POINT('Ctrl Pts',(28.4591240868749,534.853295098651,-49.1918237874731)) ;
#53671 = CARTESIAN_POINT('Ctrl Pts',(28.4591394049333,534.853269558422,-49.191821784609)) ;
#53672 = CARTESIAN_POINT('Ctrl Pts',(28.4876505307747,534.80573215835,-49.1880939028384)) ;
#53673 = CARTESIAN_POINT('Ctrl Pts',(28.5186446965708,534.759574814024,-49.1842429132903)) ;
#53674 = CARTESIAN_POINT('Ctrl Pts',(28.551941243101,534.715046859562,-49.1803319601417)) ;
#53675 = CARTESIAN_POINT('Ctrl Pts',(28.555055086558,534.710882671557,-49.1799662136262)) ;
#53676 = CARTESIAN_POINT('Ctrl Pts',(28.5581890305973,534.706732746596,-49.1795999426863)) ;
#53677 = CARTESIAN_POINT('Ctrl Pts',(28.561342905434,534.702597295999,-49.1792331989668)) ;
#53678 = CARTESIAN_POINT('Ctrl Pts',(28.598655724194,534.653671664327,-49.1748943324464)) ;
#53679 = CARTESIAN_POINT('Ctrl Pts',(28.6387637095503,534.606769532632,-49.1704899595146)) ;
#53680 = CARTESIAN_POINT('Ctrl Pts',(28.6813909443396,534.562190298489,-49.166091475398)) ;
#53681 = CARTESIAN_POINT('Ctrl Pts',(28.7234055354259,534.518251762416,-49.1617562068197)) ;
#53682 = CARTESIAN_POINT('Ctrl Pts',(28.7678672342527,534.47656946284,-49.1574269461224)) ;
#53683 = CARTESIAN_POINT('Ctrl Pts',(28.8144898039614,534.437397772436,-49.1531515172141)) ;
#53684 = CARTESIAN_POINT('Ctrl Pts',(28.8610837398425,534.398250139811,-49.1488787141134)) ;
#53685 = CARTESIAN_POINT('Ctrl Pts',(28.9098358358941,534.361609916743,-49.1446598119804)) ;
#53686 = CARTESIAN_POINT('Ctrl Pts',(28.9604402823742,534.327702017728,-49.1405187574703)) ;
#53687 = CARTESIAN_POINT('Ctrl Pts',(29.0110324645635,534.293802336496,-49.1363787065697)) ;
#53688 = CARTESIAN_POINT('Ctrl Pts',(29.063476100067,534.262633691478,-49.1323164682545)) ;
#53689 = CARTESIAN_POINT('Ctrl Pts',(29.1174458832626,534.234392420078,-49.1283311859706)) ;
#53690 = CARTESIAN_POINT('Ctrl Pts',(29.1728601611725,534.205395274468,-49.1242392380889)) ;
#53691 = CARTESIAN_POINT('Ctrl Pts',(29.2298835036641,534.179484631722,-49.120228407675)) ;
#53692 = CARTESIAN_POINT('Ctrl Pts',(29.2881418672384,534.156840117488,-49.1162715094966)) ;
#53693 = CARTESIAN_POINT('Ctrl Pts',(29.3449540373261,534.134757725959,-49.1124128365347)) ;
#53694 = CARTESIAN_POINT('Ctrl Pts',(29.4029406297045,534.115781507823,-49.108605087979)) ;
#53695 = CARTESIAN_POINT('Ctrl Pts',(29.4617338381584,534.100043761848,-49.1048015503335)) ;
#53696 = CARTESIAN_POINT('Ctrl Pts',(29.5227719799159,534.083705092892,-49.1008527801253)) ;
#53697 = CARTESIAN_POINT('Ctrl Pts',(29.584679651964,534.070857797052,-49.0969081281491)) ;
#53698 = CARTESIAN_POINT('Ctrl Pts',(29.6470212864538,534.061604094066,-49.0928973776251)) ;
#53699 = CARTESIAN_POINT('Ctrl Pts',(29.7010602111156,534.053582806806,-49.0894207821336)) ;
#53700 = CARTESIAN_POINT('Ctrl Pts',(29.7554261004178,534.048261373202,-49.0858938663866)) ;
#53701 = CARTESIAN_POINT('Ctrl Pts',(29.809817441644,534.045671351363,-49.082265892419)) ;
#53702 = CARTESIAN_POINT('Ctrl Pts',(29.818144826443,534.045274815664,-49.0817104449049)) ;
#53703 = CARTESIAN_POINT('Ctrl Pts',(29.8264728825017,534.044942238459,-49.0811526285855)) ;
#53704 = CARTESIAN_POINT('Ctrl Pts',(29.8348006109187,534.04467366373,-49.0805922613776)) ;
#53705 = CARTESIAN_POINT('Ctrl Pts',(29.8348300835497,534.044672713218,-49.0805902781842)) ;
#53706 = CARTESIAN_POINT('Ctrl Pts',(29.8348595561766,534.044671763508,-49.0805882949589)) ;
#53707 = CARTESIAN_POINT('Ctrl Pts',(29.8348890287994,534.044670814599,-49.0805863117016)) ;
#53708 = CARTESIAN_POINT('Ctrl Pts',(29.890318812835,534.042886182233,-49.076856357823)) ;
#53709 = CARTESIAN_POINT('Ctrl Pts',(29.9459332549338,534.043938850658,-49.0730035477567)) ;
#53710 = CARTESIAN_POINT('Ctrl Pts',(30.0014245838222,534.047811909075,-49.069091030408)) ;
#53711 = CARTESIAN_POINT('Ctrl Pts',(30.0065968818473,534.048172913448,-49.0687263481025)) ;
#53712 = CARTESIAN_POINT('Ctrl Pts',(30.0117680804775,534.048558398599,-49.0683611470636)) ;
#53713 = CARTESIAN_POINT('Ctrl Pts',(30.0169379125116,534.04896833648,-49.0679954784291)) ;
#53714 = CARTESIAN_POINT('Ctrl Pts',(30.0782738004613,534.053831918855,-49.0636571149693)) ;
#53715 = CARTESIAN_POINT('Ctrl Pts',(30.1394223551762,534.062140739775,-49.0592535987701)) ;
#53716 = CARTESIAN_POINT('Ctrl Pts',(30.1999826224849,534.073824994113,-49.0548561917299)) ;
#53717 = CARTESIAN_POINT('Ctrl Pts',(30.2596857992854,534.085343884857,-49.0505210198152)) ;
#53718 = CARTESIAN_POINT('Ctrl Pts',(30.3188173992538,534.1001429346,-49.0461920725626)) ;
#53719 = CARTESIAN_POINT('Ctrl Pts',(30.3770084588698,534.118119245693,-49.041917081509)) ;
#53720 = CARTESIAN_POINT('Ctrl Pts',(30.435163997499,534.136084583686,-49.0376446999954)) ;
#53721 = CARTESIAN_POINT('Ctrl Pts',(30.4923802107248,534.157223194246,-49.0334263437376)) ;
#53722 = CARTESIAN_POINT('Ctrl Pts',(30.5483022909304,534.181399772607,-49.029285862068)) ;
#53723 = CARTESIAN_POINT('Ctrl Pts',(30.6042110070796,534.205570573336,-49.0251463698758)) ;
#53724 = CARTESIAN_POINT('Ctrl Pts',(30.6588261784475,534.232777910659,-49.0210847173902)) ;
#53725 = CARTESIAN_POINT('Ctrl Pts',(30.7118064549694,534.262854609005,-49.0170999506058)) ;
#53726 = CARTESIAN_POINT('Ctrl Pts',(30.7661832550543,534.293724108384,-49.0130101481162)) ;
#53727 = CARTESIAN_POINT('Ctrl Pts',(30.8188376283895,534.327616516861,-49.0090013227196)) ;
#53728 = CARTESIAN_POINT('Ctrl Pts',(30.8694162793749,534.364314886816,-49.0050462274439)) ;
#53729 = CARTESIAN_POINT('Ctrl Pts',(30.9187591536091,534.400116613789,-49.0011877661174)) ;
#53730 = CARTESIAN_POINT('Ctrl Pts',(30.9661263148132,534.438588930043,-48.9973800789544)) ;
#53731 = CARTESIAN_POINT('Ctrl Pts',(31.0112072094342,534.479494229899,-48.9935763828663)) ;
#53732 = CARTESIAN_POINT('Ctrl Pts',(31.0579816592757,534.521936220291,-48.9896297932216)) ;
#53733 = CARTESIAN_POINT('Ctrl Pts',(31.1022941894427,534.566998009614,-48.9856870776737)) ;
#53734 = CARTESIAN_POINT('Ctrl Pts',(31.1438233851107,534.614369265271,-48.9816781001226)) ;
#53735 = CARTESIAN_POINT('Ctrl Pts',(31.1798330563521,534.655444545325,-48.9782019441002)) ;
#53736 = CARTESIAN_POINT('Ctrl Pts',(31.2137507985412,534.698256794709,-48.9746753141325)) ;
#53737 = CARTESIAN_POINT('Ctrl Pts',(31.2453868414937,534.742569778528,-48.9710475161283)) ;
#53738 = CARTESIAN_POINT('Ctrl Pts',(31.2502187328431,534.749337866544,-48.9704934289493)) ;
#53739 = CARTESIAN_POINT('Ctrl Pts',(31.2549974929727,534.756140990006,-48.9699369817631)) ;
#53740 = CARTESIAN_POINT('Ctrl Pts',(31.2597225482586,534.762978339268,-48.9693779939512)) ;
#53741 = CARTESIAN_POINT('Ctrl Pts',(31.2597394148422,534.763002745908,-48.9693759985852)) ;
#53742 = CARTESIAN_POINT('Ctrl Pts',(31.2597562807416,534.763027152984,-48.9693740031868)) ;
#53743 = CARTESIAN_POINT('Ctrl Pts',(31.2597731459568,534.763051560497,-48.969372007756)) ;
#53744 = CARTESIAN_POINT('Ctrl Pts',(31.2915091719242,534.808980262594,-48.9656171168737)) ;
#53745 = CARTESIAN_POINT('Ctrl Pts',(31.3209268984216,534.856619043449,-48.9617379323563)) ;
#53746 = CARTESIAN_POINT('Ctrl Pts',(31.3478742086198,534.905698408403,-48.9577986482251)) ;
#53747 = CARTESIAN_POINT('Ctrl Pts',(31.3505683801692,534.91060532593,-48.957404801598)) ;
#53748 = CARTESIAN_POINT('Ctrl Pts',(31.3532378596413,534.915526600376,-48.9570103542243)) ;
#53749 = CARTESIAN_POINT('Ctrl Pts',(31.355882496973,534.920461933907,-48.956615370258)) ;
#53750 = CARTESIAN_POINT('Ctrl Pts',(31.3849303162123,534.974670000392,-48.9522769973864)) ;
#53751 = CARTESIAN_POINT('Ctrl Pts',(31.4109814479544,535.03058020536,-48.9478745219973)) ;
#53752 = CARTESIAN_POINT('Ctrl Pts',(31.4338797458221,535.087824156773,-48.9434785903879)) ;
#53753 = CARTESIAN_POINT('Ctrl Pts',(31.4567428684039,535.144980172726,-48.9390894116014)) ;
#53754 = CARTESIAN_POINT('Ctrl Pts',(31.4764632128134,535.203465830496,-48.9347070927535)) ;
#53755 = CARTESIAN_POINT('Ctrl Pts',(31.492922782912,535.262907965774,-48.9303804733937)) ;
#53756 = CARTESIAN_POINT('Ctrl Pts',(31.5093675553255,535.322296660651,-48.9260577438044)) ;
#53757 = CARTESIAN_POINT('Ctrl Pts',(31.5225575510663,535.382640158892,-48.921790753626)) ;
#53758 = CARTESIAN_POINT('Ctrl Pts',(31.5324086973159,535.443559475755,-48.9176032626775)) ;
#53759 = CARTESIAN_POINT('Ctrl Pts',(31.5422547457475,535.5044472678,-48.9134179386918)) ;
#53760 = CARTESIAN_POINT('Ctrl Pts',(31.5487653550974,535.56591031728,-48.9093120369593)) ;
#53761 = CARTESIAN_POINT('Ctrl Pts',(31.5518895224363,535.627562779872,-48.905283292726)) ;
#53762 = CARTESIAN_POINT('Ctrl Pts',(31.5533047402245,535.655490753082,-48.9034583102956)) ;
#53763 = CARTESIAN_POINT('Ctrl Pts',(31.554025511204,535.683457489442,-48.9016488068729)) ;
#53764 = CARTESIAN_POINT('Ctrl Pts',(31.5540494077382,535.71142659878,-48.8998528498641)) ;
#53765 = CARTESIAN_POINT('Ctrl Pts',(31.5545274117139,535.711408976249,-48.8995776947983)) ;
#53766 = CARTESIAN_POINT('Ctrl Pts',(31.5544905135946,535.784259315344,-48.8949589420851)) ;
#53767 = CARTESIAN_POINT('Ctrl Pts',(31.5496754062171,535.857032561577,-48.8904717193232)) ;
#53768 = CARTESIAN_POINT('Ctrl Pts',(31.5263269800765,536.033357813305,-48.8795942337981)) ;
#53769 = CARTESIAN_POINT('Ctrl Pts',(31.5027341268391,536.135905818928,-48.8732677271662)) ;
#53770 = CARTESIAN_POINT('Ctrl Pts',(31.4640228932515,536.252496795028,-48.86542611162)) ;
#53771 = CARTESIAN_POINT('Ctrl Pts',(31.4581209925059,536.269360067985,-48.8642750641629)) ;
#53772 = CARTESIAN_POINT('Ctrl Pts',(31.4519498095241,536.286123215158,-48.8631108318347)) ;
#53773 = CARTESIAN_POINT('Origin',(179.888527625416,585.710565160536,-48.5221601717598)) ;
#53774 = CARTESIAN_POINT('',(181.452228406464,586.286162990338,-47.6539333933559)) ;
#53775 = CARTESIAN_POINT('',(181.451958155526,586.286100543914,-47.5221601717599)) ;
#53776 = CARTESIAN_POINT('',(181.451958155526,586.286100543914,-48.5221601717599)) ;
#53777 = CARTESIAN_POINT('',(179.965027641828,587.375705669063,-47.522167780513)) ;
#53778 = CARTESIAN_POINT('Origin',(179.888527625416,585.710565160536,-47.5221601717598)) ;
#53779 = CARTESIAN_POINT('Ctrl Pts',(179.965027642569,587.375705685183,-47.5221677806499)) ;
#53780 = CARTESIAN_POINT('Ctrl Pts',(180.01762246723,587.373258842512,-47.525762311554)) ;
#53781 = CARTESIAN_POINT('Ctrl Pts',(180.070188242169,587.368258285171,-47.5294532441289)) ;
#53782 = CARTESIAN_POINT('Ctrl Pts',(180.122459260841,587.360736681846,-47.53318691807)) ;
#53783 = CARTESIAN_POINT('Ctrl Pts',(180.18231591942,587.35212353342,-47.5374624277505)) ;
#53784 = CARTESIAN_POINT('Ctrl Pts',(180.241787318519,587.340204233137,-47.5417934229157)) ;
#53785 = CARTESIAN_POINT('Ctrl Pts',(180.300496361892,587.325066084908,-47.5461137620433)) ;
#53786 = CARTESIAN_POINT('Ctrl Pts',(180.359145578899,587.309943362931,-47.5504296986093)) ;
#53787 = CARTESIAN_POINT('Ctrl Pts',(180.417034131193,587.291608629036,-47.55473470291)) ;
#53788 = CARTESIAN_POINT('Ctrl Pts',(180.473802187684,587.270183631508,-47.5589836032974)) ;
#53789 = CARTESIAN_POINT('Ctrl Pts',(180.530533932692,587.248772338403,-47.563229785891)) ;
#53790 = CARTESIAN_POINT('Ctrl Pts',(180.586146665303,587.224274823582,-47.5674198182745)) ;
#53791 = CARTESIAN_POINT('Ctrl Pts',(180.640295894203,587.196844615246,-47.5715324169017)) ;
#53792 = CARTESIAN_POINT('Ctrl Pts',(180.694431029055,587.169421546487,-47.575643945095)) ;
#53793 = CARTESIAN_POINT('Ctrl Pts',(180.747103370465,587.139067283153,-47.5796780894175)) ;
#53794 = CARTESIAN_POINT('Ctrl Pts',(180.797983356651,587.105966823259,-47.5836381646155)) ;
#53795 = CARTESIAN_POINT('Ctrl Pts',(180.848906212481,587.07283847411,-47.5876015764303)) ;
#53796 = CARTESIAN_POINT('Ctrl Pts',(180.898033538017,587.036959177886,-47.5914909183927)) ;
#53797 = CARTESIAN_POINT('Ctrl Pts',(180.945051161067,586.998547180004,-47.5953331537656)) ;
#53798 = CARTESIAN_POINT('Ctrl Pts',(180.992086453646,586.960120746644,-47.5991768330755)) ;
#53799 = CARTESIAN_POINT('Ctrl Pts',(181.037010181813,586.919159509257,-47.6029736437573)) ;
#53800 = CARTESIAN_POINT('Ctrl Pts',(181.079527223904,586.875917151516,-47.606771285106)) ;
#53801 = CARTESIAN_POINT('Ctrl Pts',(181.122125003189,586.832592679251,-47.6105761379374)) ;
#53802 = CARTESIAN_POINT('Ctrl Pts',(181.162306470872,586.786978160473,-47.6143822988784)) ;
#53803 = CARTESIAN_POINT('Ctrl Pts',(181.199799867271,586.739367527627,-47.6182529742086)) ;
#53804 = CARTESIAN_POINT('Ctrl Pts',(181.233488265211,586.696588635888,-47.6217308360014)) ;
#53805 = CARTESIAN_POINT('Ctrl Pts',(181.265006782421,586.652197947963,-47.6252613718127)) ;
#53806 = CARTESIAN_POINT('Ctrl Pts',(181.294180528072,586.606439609925,-47.6288949212148)) ;
#53807 = CARTESIAN_POINT('Ctrl Pts',(181.296772590363,586.602374020817,-47.6292177589642)) ;
#53808 = CARTESIAN_POINT('Ctrl Pts',(181.299346174913,586.598297624356,-47.6295414099205)) ;
#53809 = CARTESIAN_POINT('Ctrl Pts',(181.30190117783,586.594210584967,-47.6298659093913)) ;
#53810 = CARTESIAN_POINT('Ctrl Pts',(181.301919148052,586.594181839401,-47.6298681917086)) ;
#53811 = CARTESIAN_POINT('Ctrl Pts',(181.301937117354,586.594153093309,-47.6298704740679)) ;
#53812 = CARTESIAN_POINT('Ctrl Pts',(181.301955085738,586.594124346691,-47.6298727564692)) ;
#53813 = CARTESIAN_POINT('Ctrl Pts',(181.331814495238,586.546353935988,-47.6336655937755)) ;
#53814 = CARTESIAN_POINT('Ctrl Pts',(181.35923032566,586.496963105049,-47.6375837284716)) ;
#53815 = CARTESIAN_POINT('Ctrl Pts',(181.384064198115,586.446231808426,-47.6415618847391)) ;
#53816 = CARTESIAN_POINT('Ctrl Pts',(181.386707431822,586.440832140151,-47.6419853062879)) ;
#53817 = CARTESIAN_POINT('Ctrl Pts',(181.389321417815,586.435417334652,-47.6424094078064)) ;
#53818 = CARTESIAN_POINT('Ctrl Pts',(181.391905992078,586.429987764067,-47.6428341105854)) ;
#53819 = CARTESIAN_POINT('Ctrl Pts',(181.414235691607,586.383078421412,-47.6465033746424)) ;
#53820 = CARTESIAN_POINT('Ctrl Pts',(181.434370916039,586.335062710703,-47.6502174215273)) ;
#53821 = CARTESIAN_POINT('Ctrl Pts',(181.452228406464,586.286162990338,-47.6539333933559)) ;
#53822 = CARTESIAN_POINT('Origin',(179.888527625416,585.710565160536,-48.5221601717598)) ;
#53823 = CARTESIAN_POINT('',(181.451958152973,586.286100550849,-48.3557104975402)) ;
#53824 = CARTESIAN_POINT('',(181.451938907901,586.286090578308,-48.1612832669077)) ;
#53825 = CARTESIAN_POINT('',(181.451958155526,586.286100543914,-48.5221601717599)) ;
#53826 = CARTESIAN_POINT('',(181.523656952667,585.391334705907,-47.5221601717598)) ;
#53827 = CARTESIAN_POINT('Ctrl Pts',(181.451938907901,586.286090578308,-48.1612832669077)) ;
#53828 = CARTESIAN_POINT('Ctrl Pts',(181.430789073677,586.343107213038,-48.156957614088)) ;
#53829 = CARTESIAN_POINT('Ctrl Pts',(181.406506905519,586.399019819855,-48.1526546256006)) ;
#53830 = CARTESIAN_POINT('Ctrl Pts',(181.379252048762,586.453481920139,-48.1484152340185)) ;
#53831 = CARTESIAN_POINT('Ctrl Pts',(181.352010931791,586.507916564852,-48.1441779796091)) ;
#53832 = CARTESIAN_POINT('Ctrl Pts',(181.32180018323,586.560902211722,-48.1400043496734)) ;
#53833 = CARTESIAN_POINT('Ctrl Pts',(181.288809381259,586.612110273712,-48.1359109220406)) ;
#53834 = CARTESIAN_POINT('Ctrl Pts',(181.255822943183,586.663311562101,-48.1318180358703)) ;
#53835 = CARTESIAN_POINT('Ctrl Pts',(181.220057144157,586.71273567089,-48.1278052990032)) ;
#53836 = CARTESIAN_POINT('Ctrl Pts',(181.181731570267,586.760071659393,-48.123864562092)) ;
#53837 = CARTESIAN_POINT('Ctrl Pts',(181.143369057262,586.807453271466,-48.1199200270032)) ;
#53838 = CARTESIAN_POINT('Ctrl Pts',(181.102441704118,586.852742558136,-48.1160474809012)) ;
#53839 = CARTESIAN_POINT('Ctrl Pts',(181.059201178604,586.895647046378,-48.1122153193404)) ;
#53840 = CARTESIAN_POINT('Ctrl Pts',(181.015940085903,586.938571941974,-48.1083813350268)) ;
#53841 = CARTESIAN_POINT('Ctrl Pts',(180.970363424739,586.979109451101,-48.1045874640204)) ;
#53842 = CARTESIAN_POINT('Ctrl Pts',(180.922757128082,587.016989733627,-48.1007820160161)) ;
#53843 = CARTESIAN_POINT('Ctrl Pts',(180.875060999456,587.054941495361,-48.0969693872204)) ;
#53844 = CARTESIAN_POINT('Ctrl Pts',(180.825327348887,587.090225448644,-48.0931446119584)) ;
#53845 = CARTESIAN_POINT('Ctrl Pts',(180.773880976884,587.122599757846,-48.0892418000498)) ;
#53846 = CARTESIAN_POINT('Ctrl Pts',(180.732422092433,587.148689114434,-48.086096656444)) ;
#53847 = CARTESIAN_POINT('Ctrl Pts',(180.68985163975,587.172889245008,-48.0829003731834)) ;
#53848 = CARTESIAN_POINT('Ctrl Pts',(180.646358283596,587.1950919934,-48.0796162265107)) ;
#53849 = CARTESIAN_POINT('Ctrl Pts',(180.646331539371,587.195105645952,-48.0796142070768)) ;
#53850 = CARTESIAN_POINT('Ctrl Pts',(180.646304794796,587.19511929775,-48.0796121876096)) ;
#53851 = CARTESIAN_POINT('Ctrl Pts',(180.646278049873,587.195132948793,-48.0796101681093)) ;
#53852 = CARTESIAN_POINT('Ctrl Pts',(180.596932732107,587.220319600387,-48.0758841194851)) ;
#53853 = CARTESIAN_POINT('Ctrl Pts',(180.546214164833,587.243022996417,-48.072035126435)) ;
#53854 = CARTESIAN_POINT('Ctrl Pts',(180.494407351764,587.263127440022,-48.0681263164207)) ;
#53855 = CARTESIAN_POINT('Ctrl Pts',(180.489565625201,587.265006347696,-48.067761009463)) ;
#53856 = CARTESIAN_POINT('Ctrl Pts',(180.484714430368,587.266862563264,-48.0673951800475)) ;
#53857 = CARTESIAN_POINT('Ctrl Pts',(180.479854022457,587.268695997693,-48.0670288797041)) ;
#53858 = CARTESIAN_POINT('Ctrl Pts',(180.422276653952,587.290415230254,-48.0626896122525)) ;
#53859 = CARTESIAN_POINT('Ctrl Pts',(180.363400426402,587.30893667016,-48.058284928138)) ;
#53860 = CARTESIAN_POINT('Ctrl Pts',(180.303618343741,587.324152456611,-48.053886366419)) ;
#53861 = CARTESIAN_POINT('Ctrl Pts',(180.244736625142,587.339139081636,-48.0495540504164)) ;
#53862 = CARTESIAN_POINT('Ctrl Pts',(180.1849761475,587.350919324995,-48.0452279587262)) ;
#53863 = CARTESIAN_POINT('Ctrl Pts',(180.124714023234,587.359429224381,-48.0409559399982)) ;
#53864 = CARTESIAN_POINT('Ctrl Pts',(180.06448868416,587.367933929156,-48.0366865289949)) ;
#53865 = CARTESIAN_POINT('Ctrl Pts',(180.003762299197,587.373172410607,-48.032471260404)) ;
#53866 = CARTESIAN_POINT('Ctrl Pts',(179.942912967287,587.375116074953,-48.0283341424415)) ;
#53867 = CARTESIAN_POINT('Ctrl Pts',(179.882078079596,587.377059277919,-48.0241980065348)) ;
#53868 = CARTESIAN_POINT('Ctrl Pts',(179.82112032378,587.375709197426,-48.0201399873129)) ;
#53869 = CARTESIAN_POINT('Ctrl Pts',(179.760419161553,587.371071815098,-48.0161593215276)) ;
#53870 = CARTESIAN_POINT('Ctrl Pts',(179.698018654521,587.366304608047,-48.0120672159695)) ;
#53871 = CARTESIAN_POINT('Ctrl Pts',(179.635889376445,587.358063108861,-48.0080568482458)) ;
#53872 = CARTESIAN_POINT('Ctrl Pts',(179.574444647537,587.346393487565,-48.0041010454521)) ;
#53873 = CARTESIAN_POINT('Ctrl Pts',(179.514595695523,587.335026937215,-48.0002479785449)) ;
#53874 = CARTESIAN_POINT('Ctrl Pts',(179.455396334987,587.32040788988,-47.9964463123259)) ;
#53875 = CARTESIAN_POINT('Ctrl Pts',(179.397228022023,587.302619162424,-47.9926494263338)) ;
#53876 = CARTESIAN_POINT('Ctrl Pts',(179.336733261059,587.284118972879,-47.9887006834739)) ;
#53877 = CARTESIAN_POINT('Ctrl Pts',(179.277354014927,587.262189665291,-47.9847566954869)) ;
#53878 = CARTESIAN_POINT('Ctrl Pts',(179.219515319863,587.236976205275,-47.9807469470701)) ;
#53879 = CARTESIAN_POINT('Ctrl Pts',(179.169446859135,587.215150001706,-47.9772758810146)) ;
#53880 = CARTESIAN_POINT('Ctrl Pts',(179.120531903364,587.19086254644,-47.9737548797059)) ;
#53881 = CARTESIAN_POINT('Ctrl Pts',(179.073042697654,587.164247054371,-47.9701331480617)) ;
#53882 = CARTESIAN_POINT('Ctrl Pts',(179.06569991298,587.160131764921,-47.9695731556337)) ;
#53883 = CARTESIAN_POINT('Ctrl Pts',(179.058391114115,587.155960834707,-47.9690107550085)) ;
#53884 = CARTESIAN_POINT('Ctrl Pts',(179.051117196837,587.151734771194,-47.9684457584189)) ;
#53885 = CARTESIAN_POINT('Ctrl Pts',(179.051090282242,587.151719134119,-47.9684436678461)) ;
#53886 = CARTESIAN_POINT('Ctrl Pts',(179.051063368125,587.15170349629,-47.9684415772376)) ;
#53887 = CARTESIAN_POINT('Ctrl Pts',(179.051036454486,587.151687857706,-47.9684394865936)) ;
#53888 = CARTESIAN_POINT('Ctrl Pts',(179.00303414808,587.123795379465,-47.964710680897)) ;
#53889 = CARTESIAN_POINT('Ctrl Pts',(178.956383143798,587.093394646366,-47.960858986221)) ;
#53890 = CARTESIAN_POINT('Ctrl Pts',(178.911335735443,587.060663725994,-47.9569475109709)) ;
#53891 = CARTESIAN_POINT('Ctrl Pts',(178.907128659802,587.057606914007,-47.9565822097728)) ;
#53892 = CARTESIAN_POINT('Ctrl Pts',(178.902935584205,587.054529812997,-47.9562163871625)) ;
#53893 = CARTESIAN_POINT('Ctrl Pts',(178.898756721833,587.051432589843,-47.9558500945468)) ;
#53894 = CARTESIAN_POINT('Ctrl Pts',(178.849339627032,587.014806408698,-47.9515185049169)) ;
#53895 = CARTESIAN_POINT('Ctrl Pts',(178.801907620743,586.975360863164,-47.9471218492722)) ;
#53896 = CARTESIAN_POINT('Ctrl Pts',(178.756762820748,586.933367326175,-47.9427310698556)) ;
#53897 = CARTESIAN_POINT('Ctrl Pts',(178.712190612804,586.891906412334,-47.9383959806935)) ;
#53898 = CARTESIAN_POINT('Ctrl Pts',(178.669847599266,586.847961977422,-47.9340669120912)) ;
#53899 = CARTESIAN_POINT('Ctrl Pts',(178.629992517954,586.801817601538,-47.9297915887904)) ;
#53900 = CARTESIAN_POINT('Ctrl Pts',(178.590161679204,586.755701293791,-47.925518866031)) ;
#53901 = CARTESIAN_POINT('Ctrl Pts',(178.552815628851,586.707387777744,-47.9212999582049)) ;
#53902 = CARTESIAN_POINT('Ctrl Pts',(178.518183896022,586.657180564922,-47.9171586830542)) ;
#53903 = CARTESIAN_POINT('Ctrl Pts',(178.483560447977,586.60698536293,-47.9130183986009)) ;
#53904 = CARTESIAN_POINT('Ctrl Pts',(178.451650054233,586.554897366349,-47.9089557114525)) ;
#53905 = CARTESIAN_POINT('Ctrl Pts',(178.422653937972,586.501239960583,-47.9049696146823)) ;
#53906 = CARTESIAN_POINT('Ctrl Pts',(178.392970250437,586.446310201979,-47.9008889974732)) ;
#53907 = CARTESIAN_POINT('Ctrl Pts',(178.366340998771,586.389735597203,-47.8968886187649)) ;
#53908 = CARTESIAN_POINT('Ctrl Pts',(178.342949811355,586.331885246925,-47.8929414084268)) ;
#53909 = CARTESIAN_POINT('Ctrl Pts',(178.320071526454,586.275303391047,-47.8890807492364)) ;
#53910 = CARTESIAN_POINT('Ctrl Pts',(178.300291065518,586.217501151216,-47.8852705986862)) ;
#53911 = CARTESIAN_POINT('Ctrl Pts',(178.283746301024,586.158845320057,-47.8814641815396)) ;
#53912 = CARTESIAN_POINT('Ctrl Pts',(178.266645167158,586.098217003404,-47.8775297617297)) ;
#53913 = CARTESIAN_POINT('Ctrl Pts',(178.253001833031,586.036676586433,-47.8735989005534)) ;
#53914 = CARTESIAN_POINT('Ctrl Pts',(178.242923733702,585.974653496531,-47.869602331551)) ;
#53915 = CARTESIAN_POINT('Ctrl Pts',(178.234152338515,585.920672183732,-47.8661239488747)) ;
#53916 = CARTESIAN_POINT('Ctrl Pts',(178.228081320139,585.866324389926,-47.8625951437717)) ;
#53917 = CARTESIAN_POINT('Ctrl Pts',(178.224746826461,585.811911451861,-47.8589653240946)) ;
#53918 = CARTESIAN_POINT('Ctrl Pts',(178.224252145035,585.803839140932,-47.8584268302347)) ;
#53919 = CARTESIAN_POINT('Ctrl Pts',(178.22381762761,585.795765326998,-47.8578861131905)) ;
#53920 = CARTESIAN_POINT('Ctrl Pts',(178.223443328293,585.787690919578,-47.8573430077773)) ;
#53921 = CARTESIAN_POINT('Ctrl Pts',(178.223441762582,585.787657143973,-47.8573407359433)) ;
#53922 = CARTESIAN_POINT('Ctrl Pts',(178.223440197925,585.787623368358,-47.8573384640674)) ;
#53923 = CARTESIAN_POINT('Ctrl Pts',(178.223438634321,585.787589592732,-47.8573361921497)) ;
#53924 = CARTESIAN_POINT('Ctrl Pts',(178.220870330784,585.732111292547,-47.8536044439544)) ;
#53925 = CARTESIAN_POINT('Ctrl Pts',(178.221143922289,585.67640822179,-47.8497502705975)) ;
#53926 = CARTESIAN_POINT('Ctrl Pts',(178.224246539444,585.620789796714,-47.8458371466104)) ;
#53927 = CARTESIAN_POINT('Ctrl Pts',(178.224528728945,585.615731184964,-47.8454812398231)) ;
#53928 = CARTESIAN_POINT('Ctrl Pts',(178.224834300041,585.610673302273,-47.8451248453797)) ;
#53929 = CARTESIAN_POINT('Ctrl Pts',(178.22516323011,585.605616398388,-47.844768011037)) ;
#53930 = CARTESIAN_POINT('Ctrl Pts',(178.229157110935,585.544215288006,-47.840435315506)) ;
#53931 = CARTESIAN_POINT('Ctrl Pts',(178.236597951157,585.482953409495,-47.836038428256)) ;
#53932 = CARTESIAN_POINT('Ctrl Pts',(178.247421429552,585.42223285034,-47.831648368672)) ;
#53933 = CARTESIAN_POINT('Ctrl Pts',(178.258085000805,585.362409382739,-47.827323168263)) ;
#53934 = CARTESIAN_POINT('Ctrl Pts',(178.272031588538,585.303111185833,-47.8230048746017)) ;
#53935 = CARTESIAN_POINT('Ctrl Pts',(178.289163535409,585.244708151981,-47.8187406547706)) ;
#53936 = CARTESIAN_POINT('Ctrl Pts',(178.30628553143,585.186339040709,-47.8144789117515)) ;
#53937 = CARTESIAN_POINT('Ctrl Pts',(178.326589078513,585.128863989302,-47.8102713110671)) ;
#53938 = CARTESIAN_POINT('Ctrl Pts',(178.349943937351,585.072639270109,-47.8061410125672)) ;
#53939 = CARTESIAN_POINT('Ctrl Pts',(178.373293946666,585.016426225706,-47.8020115717039)) ;
#53940 = CARTESIAN_POINT('Ctrl Pts',(178.39969402403,584.961463025718,-47.7979594006895)) ;
#53941 = CARTESIAN_POINT('Ctrl Pts',(178.428981849489,584.908092986886,-47.7939827726763)) ;
#53942 = CARTESIAN_POINT('Ctrl Pts',(178.459072004302,584.8532608952,-47.7898972063812)) ;
#53943 = CARTESIAN_POINT('Ctrl Pts',(178.492210590527,584.800110655127,-47.7858913648375)) ;
#53944 = CARTESIAN_POINT('Ctrl Pts',(178.528184980514,584.748999271006,-47.7819370164778)) ;
#53945 = CARTESIAN_POINT('Ctrl Pts',(178.563248122558,584.699182561892,-47.7780828335916)) ;
#53946 = CARTESIAN_POINT('Ctrl Pts',(178.601005291661,584.651302907566,-47.7742771976262)) ;
#53947 = CARTESIAN_POINT('Ctrl Pts',(178.641223069236,584.605673871915,-47.7704724715031)) ;
#53948 = CARTESIAN_POINT('Ctrl Pts',(178.683008662682,584.558266072479,-47.7665194251506)) ;
#53949 = CARTESIAN_POINT('Ctrl Pts',(178.72745105857,584.513288439922,-47.7625669319197)) ;
#53950 = CARTESIAN_POINT('Ctrl Pts',(178.774242759903,584.471067628475,-47.7585436949899)) ;
#53951 = CARTESIAN_POINT('Ctrl Pts',(178.81463325317,584.434622717263,-47.7550708457559)) ;
#53952 = CARTESIAN_POINT('Ctrl Pts',(178.856774835547,584.400231167256,-47.7515446221092)) ;
#53953 = CARTESIAN_POINT('Ctrl Pts',(178.900435603904,584.368083976891,-47.7479144055063)) ;
#53954 = CARTESIAN_POINT('Ctrl Pts',(178.907326412993,584.36301031099,-47.747341462553)) ;
#53955 = CARTESIAN_POINT('Ctrl Pts',(178.914255090497,584.357992447896,-47.7467659292308)) ;
#53956 = CARTESIAN_POINT('Ctrl Pts',(178.921220758242,584.353031024268,-47.746187606543)) ;
#53957 = CARTESIAN_POINT('Ctrl Pts',(178.921249751937,584.353010372981,-47.7461851993493)) ;
#53958 = CARTESIAN_POINT('Ctrl Pts',(178.921278746273,584.352989722672,-47.7461827921072)) ;
#53959 = CARTESIAN_POINT('Ctrl Pts',(178.92130774125,584.35296907334,-47.7461803848168)) ;
#53960 = CARTESIAN_POINT('Ctrl Pts',(178.96609389121,584.321073753566,-47.7424620418301)) ;
#53961 = CARTESIAN_POINT('Ctrl Pts',(179.012582022572,584.291398545953,-47.7386180925322)) ;
#53962 = CARTESIAN_POINT('Ctrl Pts',(179.060512232693,584.264098009022,-47.7347113417059)) ;
#53963 = CARTESIAN_POINT('Ctrl Pts',(179.065190679357,584.261433215657,-47.7343300054813)) ;
#53964 = CARTESIAN_POINT('Ctrl Pts',(179.069882824745,584.258791044184,-47.7339480709073)) ;
#53965 = CARTESIAN_POINT('Ctrl Pts',(179.074588400769,584.256171635694,-47.7335655963915)) ;
#53966 = CARTESIAN_POINT('Ctrl Pts',(179.128346800044,584.22624645613,-47.7291960531883)) ;
#53967 = CARTESIAN_POINT('Ctrl Pts',(179.183864273609,584.199292316861,-47.7247567343599)) ;
#53968 = CARTESIAN_POINT('Ctrl Pts',(179.240766466883,584.175474967899,-47.7203209274937)) ;
#53969 = CARTESIAN_POINT('Ctrl Pts',(179.296614645206,584.152098794232,-47.7159672862961)) ;
#53970 = CARTESIAN_POINT('Ctrl Pts',(179.353796625881,584.131743807501,-47.7116173127172)) ;
#53971 = CARTESIAN_POINT('Ctrl Pts',(179.411951071135,584.114528036147,-47.7073200655742)) ;
#53972 = CARTESIAN_POINT('Ctrl Pts',(179.470068534857,584.097323212633,-47.7030255511334)) ;
#53973 = CARTESIAN_POINT('Ctrl Pts',(179.529157213191,584.083253479214,-47.6987838388947)) ;
#53974 = CARTESIAN_POINT('Ctrl Pts',(179.588849648619,584.072401912726,-47.6946203248817)) ;
#53975 = CARTESIAN_POINT('Ctrl Pts',(179.6485268056,584.061553123726,-47.6904578765318)) ;
#53976 = CARTESIAN_POINT('Ctrl Pts',(179.708807388094,584.053920881524,-47.6863735970115)) ;
#53977 = CARTESIAN_POINT('Ctrl Pts',(179.76931765361,584.049554231932,-47.6823681831685)) ;
#53978 = CARTESIAN_POINT('Ctrl Pts',(179.831905341739,584.045037667669,-47.6782252565047)) ;
#53979 = CARTESIAN_POINT('Ctrl Pts',(179.894738737398,584.044015170651,-47.6741667339541)) ;
#53980 = CARTESIAN_POINT('Ctrl Pts',(179.95739747218,584.04650117541,-47.6701664126541)) ;
#53981 = CARTESIAN_POINT('Ctrl Pts',(180.018055012907,584.048907782172,-47.6662938535765)) ;
#53982 = CARTESIAN_POINT('Ctrl Pts',(180.078548744618,584.054602451444,-47.6624754582192)) ;
#53983 = CARTESIAN_POINT('Ctrl Pts',(180.138492202174,584.063558629316,-47.6586656558443)) ;
#53984 = CARTESIAN_POINT('Ctrl Pts',(180.20140211261,584.072958026194,-47.6546673158092)) ;
#53985 = CARTESIAN_POINT('Ctrl Pts',(180.263705718314,584.085950672778,-47.6506780644461)) ;
#53986 = CARTESIAN_POINT('Ctrl Pts',(180.324952967773,584.10245292891,-47.6466260430931)) ;
#53987 = CARTESIAN_POINT('Ctrl Pts',(180.377763463543,584.116682014059,-47.6431321840478)) ;
#53988 = CARTESIAN_POINT('Ctrl Pts',(180.429789581885,584.13352052268,-47.6395909946578)) ;
#53989 = CARTESIAN_POINT('Ctrl Pts',(180.480740563972,584.15287508289,-47.635950694698)) ;
#53990 = CARTESIAN_POINT('Ctrl Pts',(180.488863080554,584.155960553077,-47.6353703644359)) ;
#53991 = CARTESIAN_POINT('Ctrl Pts',(180.496958376483,584.15910993538,-47.63478751536)) ;
#53992 = CARTESIAN_POINT('Ctrl Pts',(180.505025392259,584.162322819237,-47.6342019376836)) ;
#53993 = CARTESIAN_POINT('Ctrl Pts',(180.505042444981,584.162329610895,-47.6342006998413)) ;
#53994 = CARTESIAN_POINT('Ctrl Pts',(180.505059497576,584.162336402837,-47.6341994619868)) ;
#53995 = CARTESIAN_POINT('Ctrl Pts',(180.505076550046,584.162343195063,-47.6341982241201)) ;
#53996 = CARTESIAN_POINT('Ctrl Pts',(180.557298536641,584.183143908574,-47.630407344555)) ;
#53997 = CARTESIAN_POINT('Ctrl Pts',(180.608515361297,584.206686092502,-47.6264922198568)) ;
#53998 = CARTESIAN_POINT('Ctrl Pts',(180.65844762838,584.232826843712,-47.6225152161776)) ;
#53999 = CARTESIAN_POINT('Ctrl Pts',(180.663457052748,584.2354493987,-47.622116225699)) ;
#54000 = CARTESIAN_POINT('Ctrl Pts',(180.668453527044,584.238098070403,-47.6217166124095)) ;
#54001 = CARTESIAN_POINT('Ctrl Pts',(180.673436755783,584.240772688929,-47.621316439284)) ;
#54002 = CARTESIAN_POINT('Ctrl Pts',(180.727975537573,584.270044962764,-47.6169367577736)) ;
#54003 = CARTESIAN_POINT('Ctrl Pts',(180.780931118968,584.302430144093,-47.6124906531587)) ;
#54004 = CARTESIAN_POINT('Ctrl Pts',(180.831965618059,584.33770377131,-47.6080472780278)) ;
#54005 = CARTESIAN_POINT('Ctrl Pts',(180.882937031464,584.372933795454,-47.6036093955221)) ;
#54006 = CARTESIAN_POINT('Ctrl Pts',(180.931992413172,584.411044902159,-47.5991745754653)) ;
#54007 = CARTESIAN_POINT('Ctrl Pts',(180.978823392945,584.451786978966,-47.5947911249208)) ;
#54008 = CARTESIAN_POINT('Ctrl Pts',(181.025611228522,584.49249152113,-47.5904117127383)) ;
#54009 = CARTESIAN_POINT('Ctrl Pts',(181.070178898671,584.535822145435,-47.586083711498)) ;
#54010 = CARTESIAN_POINT('Ctrl Pts',(181.112243766078,584.581504876635,-47.5818312442298)) ;
#54011 = CARTESIAN_POINT('Ctrl Pts',(181.154283113265,584.627159892704,-47.5775813568792)) ;
#54012 = CARTESIAN_POINT('Ctrl Pts',(181.193822672174,584.675164214726,-47.5734069046344)) ;
#54013 = CARTESIAN_POINT('Ctrl Pts',(181.230604314454,584.725219699878,-47.5693070038503)) ;
#54014 = CARTESIAN_POINT('Ctrl Pts',(181.267389569821,584.775280102016,-47.5652067003299)) ;
#54015 = CARTESIAN_POINT('Ctrl Pts',(181.301416192259,584.827392180787,-47.5611808285123)) ;
#54016 = CARTESIAN_POINT('Ctrl Pts',(181.332451455274,584.881231780506,-47.5572045791497)) ;
#54017 = CARTESIAN_POINT('Ctrl Pts',(181.363485675684,584.935069571525,-47.5532284633661)) ;
#54018 = CARTESIAN_POINT('Ctrl Pts',(181.391528392631,584.990634905946,-47.5493016741465)) ;
#54019 = CARTESIAN_POINT('Ctrl Pts',(181.416376235186,585.047575835669,-47.5453786416672)) ;
#54020 = CARTESIAN_POINT('Ctrl Pts',(181.441249031598,585.104573949262,-47.5414516694177)) ;
#54021 = CARTESIAN_POINT('Ctrl Pts',(181.46291995929,585.162950524743,-47.5375279573556)) ;
#54022 = CARTESIAN_POINT('Ctrl Pts',(181.481221277255,585.222322749231,-47.5335469067959)) ;
#54023 = CARTESIAN_POINT('Ctrl Pts',(181.498352981961,585.277900572617,-47.5298202799631)) ;
#54024 = CARTESIAN_POINT('Ctrl Pts',(181.512531780721,585.334350496989,-47.526042753317)) ;
#54025 = CARTESIAN_POINT('Ctrl Pts',(181.523656952667,585.391334705907,-47.52216017176)) ;
#54026 = CARTESIAN_POINT('Origin',(179.888527625416,585.710565160536,-47.5221601717598)) ;
#54027 = CARTESIAN_POINT('Ctrl Pts',(181.45195815042,586.286100557784,-48.3557104975402)) ;
#54028 = CARTESIAN_POINT('Ctrl Pts',(181.443430929173,586.309264585671,-48.3540690235658)) ;
#54029 = CARTESIAN_POINT('Ctrl Pts',(181.434389273589,586.332238109432,-48.3524103290642)) ;
#54030 = CARTESIAN_POINT('Ctrl Pts',(181.397454926864,586.420287834188,-48.345927431339)) ;
#54031 = CARTESIAN_POINT('Ctrl Pts',(181.365940902444,586.483750384691,-48.3409809049559)) ;
#54032 = CARTESIAN_POINT('Ctrl Pts',(181.277531964931,586.636525632691,-48.3283801251284)) ;
#54033 = CARTESIAN_POINT('Ctrl Pts',(181.215982329991,586.722789005932,-48.3206115127961)) ;
#54034 = CARTESIAN_POINT('Ctrl Pts',(181.110335328957,586.844503617117,-48.3089652506152)) ;
#54035 = CARTESIAN_POINT('Ctrl Pts',(181.071917277504,586.884541604414,-48.3050053477068)) ;
#54036 = CARTESIAN_POINT('Ctrl Pts',(181.009695297284,586.943222104851,-48.2990864909969)) ;
#54037 = CARTESIAN_POINT('Ctrl Pts',(180.987264284814,586.963257618225,-48.2970444731123)) ;
#54038 = CARTESIAN_POINT('Ctrl Pts',(180.931510621498,587.010406023872,-48.2921983726469)) ;
#54039 = CARTESIAN_POINT('Ctrl Pts',(180.897659925384,587.036857955258,-48.2894364566215)) ;
#54040 = CARTESIAN_POINT('Ctrl Pts',(180.812339532822,587.098369378618,-48.2827988334593)) ;
#54041 = CARTESIAN_POINT('Ctrl Pts',(180.759854627338,587.131909335231,-48.2789842951599)) ;
#54042 = CARTESIAN_POINT('Ctrl Pts',(180.601584244595,587.220980929433,-48.267887808215)) ;
#54043 = CARTESIAN_POINT('Ctrl Pts',(180.491576631445,587.268170331297,-48.2606445675556)) ;
#54044 = CARTESIAN_POINT('Ctrl Pts',(180.32808376122,587.318363642565,-48.2496730936678)) ;
#54045 = CARTESIAN_POINT('Ctrl Pts',(180.278017792087,587.331219964738,-48.2462922002711)) ;
#54046 = CARTESIAN_POINT('Ctrl Pts',(180.171182203686,587.353417532433,-48.2389847729666)) ;
#54047 = CARTESIAN_POINT('Ctrl Pts',(180.114364578511,587.36218672341,-48.2350441793587)) ;
#54048 = CARTESIAN_POINT('Ctrl Pts',(179.989944623202,587.374849547511,-48.2262802710685)) ;
#54049 = CARTESIAN_POINT('Ctrl Pts',(179.922328375845,587.377593582707,-48.2214312160094)) ;
#54050 = CARTESIAN_POINT('Ctrl Pts',(179.738188563359,587.373858183083,-48.2080771569703)) ;
#54051 = CARTESIAN_POINT('Ctrl Pts',(179.622203633226,587.359267687013,-48.1994865815561)) ;
#54052 = CARTESIAN_POINT('Ctrl Pts',(179.477866907529,587.325469419362,-48.1891498383575)) ;
#54053 = CARTESIAN_POINT('Ctrl Pts',(179.447253870925,587.317374450272,-48.18698070924)) ;
#54054 = CARTESIAN_POINT('Ctrl Pts',(179.381056318005,587.297834644963,-48.1823655551405)) ;
#54055 = CARTESIAN_POINT('Ctrl Pts',(179.345589773519,587.286055749152,-48.1799373293568)) ;
#54056 = CARTESIAN_POINT('Ctrl Pts',(179.210439791717,587.236063539404,-48.1707485761946)) ;
#54057 = CARTESIAN_POINT('Ctrl Pts',(179.114113944203,587.189496009491,-48.1643247946066)) ;
#54058 = CARTESIAN_POINT('Ctrl Pts',(178.945287781856,587.086830253905,-48.1522345871993)) ;
#54059 = CARTESIAN_POINT('Ctrl Pts',(178.871675679258,587.033371361065,-48.1466188642367)) ;
#54060 = CARTESIAN_POINT('Ctrl Pts',(178.764200119052,586.941025428722,-48.1374925328631)) ;
#54061 = CARTESIAN_POINT('Ctrl Pts',(178.727151903909,586.906119552598,-48.1341496452756)) ;
#54062 = CARTESIAN_POINT('Ctrl Pts',(178.650052876733,586.8265090294,-48.1267011960654)) ;
#54063 = CARTESIAN_POINT('Ctrl Pts',(178.610704495145,586.781227050279,-48.1225708510962)) ;
#54064 = CARTESIAN_POINT('Ctrl Pts',(178.52867310389,586.675847107055,-48.1131695099987)) ;
#54065 = CARTESIAN_POINT('Ctrl Pts',(178.487363830371,586.614839249772,-48.1078615898132)) ;
#54066 = CARTESIAN_POINT('Ctrl Pts',(178.397180446647,586.460557692113,-48.0948693689265)) ;
#54067 = CARTESIAN_POINT('Ctrl Pts',(178.35283812052,586.364985797675,-48.0871615625068)) ;
#54068 = CARTESIAN_POINT('Ctrl Pts',(178.307384305074,586.236414576012,-48.0776679428554)) ;
#54069 = CARTESIAN_POINT('Ctrl Pts',(178.297801180886,586.206671821016,-48.0755312737752)) ;
#54070 = CARTESIAN_POINT('Ctrl Pts',(178.278327936602,586.139848362584,-48.0708844293593)) ;
#54071 = CARTESIAN_POINT('Ctrl Pts',(178.268870864757,586.102661679427,-48.0683965412314)) ;
#54072 = CARTESIAN_POINT('Ctrl Pts',(178.249791116583,586.015077597982,-48.0626926234597)) ;
#54073 = CARTESIAN_POINT('Ctrl Pts',(178.241194965258,585.964496304437,-48.0595161829983)) ;
#54074 = CARTESIAN_POINT('Ctrl Pts',(178.217846403679,585.774334032729,-48.0477528209275)) ;
#54075 = CARTESIAN_POINT('Ctrl Pts',(178.218408472952,585.633483604313,-48.0393417606924)) ;
#54076 = CARTESIAN_POINT('Ctrl Pts',(178.243298194302,585.443303573488,-48.0270283038372)) ;
#54077 = CARTESIAN_POINT('Ctrl Pts',(178.25234552833,585.39257802682,-48.0236555769129)) ;
#54078 = CARTESIAN_POINT('Ctrl Pts',(178.27653108666,585.285853806666,-48.0163223463825)) ;
#54079 = CARTESIAN_POINT('Ctrl Pts',(178.292272752844,585.230063844592,-48.0123457209125)) ;
#54080 = CARTESIAN_POINT('Ctrl Pts',(178.332972339751,585.11012542569,-48.0034627637028)) ;
#54081 = CARTESIAN_POINT('Ctrl Pts',(178.359063209572,585.04647405495,-47.9985287102257)) ;
#54082 = CARTESIAN_POINT('Ctrl Pts',(178.438165562215,584.883079041712,-47.9853597944614)) ;
#54083 = CARTESIAN_POINT('Ctrl Pts',(178.49751302551,584.786787754627,-47.9770572571765)) ;
#54084 = CARTESIAN_POINT('Ctrl Pts',(178.585636793927,584.671787558228,-47.9669433352678)) ;
#54085 = CARTESIAN_POINT('Ctrl Pts',(178.60586613944,584.646909407949,-47.9647440450321)) ;
#54086 = CARTESIAN_POINT('Ctrl Pts',(178.650819919919,584.594774802032,-47.9601361288877)) ;
#54087 = CARTESIAN_POINT('Ctrl Pts',(178.675753748137,584.567722847513,-47.9577422910839)) ;
#54088 = CARTESIAN_POINT('Ctrl Pts',(178.775363414293,584.466586868774,-47.948677389504)) ;
#54089 = CARTESIAN_POINT('Ctrl Pts',(178.856098426246,584.398806394709,-47.9423384820082)) ;
#54090 = CARTESIAN_POINT('Ctrl Pts',(179.019328137633,584.286235711831,-47.9302098459965)) ;
#54091 = CARTESIAN_POINT('Ctrl Pts',(179.100248499142,584.239907095803,-47.9244616565643)) ;
#54092 = CARTESIAN_POINT('Ctrl Pts',(179.230280230815,584.179289344805,-47.9152224617741)) ;
#54093 = CARTESIAN_POINT('Ctrl Pts',(179.276890068618,584.160083351187,-47.9119128022261)) ;
#54094 = CARTESIAN_POINT('Ctrl Pts',(179.380237467402,584.122883771237,-47.9045345558958)) ;
#54095 = CARTESIAN_POINT('Ctrl Pts',(179.437211136613,584.105758956359,-47.9004413492104)) ;
#54096 = CARTESIAN_POINT('Ctrl Pts',(179.565291435026,584.074621578854,-47.8911684355796)) ;
#54097 = CARTESIAN_POINT('Ctrl Pts',(179.636642999256,584.062127938558,-47.8859541562891)) ;
#54098 = CARTESIAN_POINT('Ctrl Pts',(179.816715850088,584.042562822711,-47.872787640558)) ;
#54099 = CARTESIAN_POINT('Ctrl Pts',(179.925756002662,584.041431750277,-47.8647990115143)) ;
#54100 = CARTESIAN_POINT('Ctrl Pts',(180.065006146868,584.05364882853,-47.8550745457781)) ;
#54101 = CARTESIAN_POINT('Ctrl Pts',(180.095800522561,584.057218562334,-47.8529566337892)) ;
#54102 = CARTESIAN_POINT('Ctrl Pts',(180.164859570561,584.067184474833,-47.8483016225688)) ;
#54103 = CARTESIAN_POINT('Ctrl Pts',(180.203034951374,584.074061211128,-47.8457889588977)) ;
#54104 = CARTESIAN_POINT('Ctrl Pts',(180.292004002471,584.093316704981,-47.8400020901898)) ;
#54105 = CARTESIAN_POINT('Ctrl Pts',(180.342524364516,584.1067654574,-47.8367693177729)) ;
#54106 = CARTESIAN_POINT('Ctrl Pts',(180.522820007814,584.163965650768,-47.8251640115305)) ;
#54107 = CARTESIAN_POINT('Ctrl Pts',(180.647695520257,584.221284055813,-47.8169463585962)) ;
#54108 = CARTESIAN_POINT('Ctrl Pts',(180.807896397878,584.320255449165,-47.8048675471421)) ;
#54109 = CARTESIAN_POINT('Ctrl Pts',(180.850362479379,584.349288999803,-47.8015033227905)) ;
#54110 = CARTESIAN_POINT('Ctrl Pts',(180.936829035483,584.414473067217,-47.7942525957142)) ;
#54111 = CARTESIAN_POINT('Ctrl Pts',(180.980454847296,584.451008046381,-47.7903530580458)) ;
#54112 = CARTESIAN_POINT('Ctrl Pts',(181.070826200184,584.534919374387,-47.7817126029434)) ;
#54113 = CARTESIAN_POINT('Ctrl Pts',(181.116774516141,584.583009897295,-47.7769475388171)) ;
#54114 = CARTESIAN_POINT('Ctrl Pts',(181.238074762311,584.72620151044,-47.7633355204528)) ;
#54115 = CARTESIAN_POINT('Ctrl Pts',(181.306100073429,584.826969848809,-47.7543788991492)) ;
#54116 = CARTESIAN_POINT('Ctrl Pts',(181.377146484779,584.961869234682,-47.7437545121612)) ;
#54117 = CARTESIAN_POINT('Ctrl Pts',(181.390923965474,584.989914359271,-47.7416162949122)) ;
#54118 = CARTESIAN_POINT('Ctrl Pts',(181.420005657885,585.053577939834,-47.7369392242399)) ;
#54119 = CARTESIAN_POINT('Ctrl Pts',(181.434871689442,585.089374517483,-47.7344235946812)) ;
#54120 = CARTESIAN_POINT('Ctrl Pts',(181.466728698429,585.174337636028,-47.7286427827358)) ;
#54121 = CARTESIAN_POINT('Ctrl Pts',(181.482693166675,585.223845970174,-47.7254179100826)) ;
#54122 = CARTESIAN_POINT('Ctrl Pts',(181.532240432319,585.406329071536,-47.7137859949888)) ;
#54123 = CARTESIAN_POINT('Ctrl Pts',(181.551693191161,585.542550455988,-47.7055347715064)) ;
#54124 = CARTESIAN_POINT('Ctrl Pts',(181.555202721283,585.731418582942,-47.6933935229849)) ;
#54125 = CARTESIAN_POINT('Ctrl Pts',(181.553747970288,585.783235432592,-47.6899969891168)) ;
#54126 = CARTESIAN_POINT('Ctrl Pts',(181.545521981611,585.893154069984,-47.6826029385961)) ;
#54127 = CARTESIAN_POINT('Ctrl Pts',(181.538101371667,585.951135292317,-47.6785887999446)) ;
#54128 = CARTESIAN_POINT('Ctrl Pts',(181.510468967264,586.103106613832,-47.667743150632)) ;
#54129 = CARTESIAN_POINT('Ctrl Pts',(181.485146513092,586.195937380314,-47.6607736436916)) ;
#54130 = CARTESIAN_POINT('Ctrl Pts',(181.451973977593,586.286057561759,-47.6537754297552)) ;
#54131 = CARTESIAN_POINT('Origin',(179.888527625416,585.710565160536,-48.5221601717598)) ;
#54132 = CARTESIAN_POINT('',(181.451958155526,586.286100543914,-49.0537403040459)) ;
#54133 = CARTESIAN_POINT('',(181.451958155603,586.286100543705,-48.8631342200737)) ;
#54134 = CARTESIAN_POINT('',(181.451958155526,586.286100543914,-48.5221601717599)) ;
#54135 = CARTESIAN_POINT('',(181.555012477675,585.711613030546,-49.0927992681987)) ;
#54136 = CARTESIAN_POINT('Ctrl Pts',(181.55452730859,585.71159261619,-49.0925209293698)) ;
#54137 = CARTESIAN_POINT('Ctrl Pts',(181.554499034075,585.757439200686,-49.0892076633268)) ;
#54138 = CARTESIAN_POINT('Ctrl Pts',(181.552578285604,585.80326867997,-49.0859220267552)) ;
#54139 = CARTESIAN_POINT('Ctrl Pts',(181.546213055913,585.879626570088,-49.0805462416942)) ;
#54140 = CARTESIAN_POINT('Ctrl Pts',(181.542807775801,585.910215500907,-49.0784194957207)) ;
#54141 = CARTESIAN_POINT('Ctrl Pts',(181.534158770185,585.972228788091,-49.0741854936695)) ;
#54142 = CARTESIAN_POINT('Ctrl Pts',(181.528857649455,586.003630462584,-49.0720857688122)) ;
#54143 = CARTESIAN_POINT('Ctrl Pts',(181.50569208945,586.120361536234,-49.0643871935001)) ;
#54144 = CARTESIAN_POINT('Ctrl Pts',(181.482047253509,586.204364102039,-49.0590539986409)) ;
#54145 = CARTESIAN_POINT('Ctrl Pts',(181.451958155526,586.286100543914,-49.0537403040458)) ;
#54146 = CARTESIAN_POINT('',(178.619456745563,586.789923813584,-49.5221601717597)) ;
#54147 = CARTESIAN_POINT('Ctrl Pts',(181.555012477675,585.711613030547,-49.0927992681987)) ;
#54148 = CARTESIAN_POINT('Ctrl Pts',(181.554916975438,585.651747730793,-49.0970476791215)) ;
#54149 = CARTESIAN_POINT('Ctrl Pts',(181.55156888472,585.591782420422,-49.1013352669896)) ;
#54150 = CARTESIAN_POINT('Ctrl Pts',(181.544993104438,585.532094412162,-49.1056020815615)) ;
#54151 = CARTESIAN_POINT('Ctrl Pts',(181.538424435453,585.472470952776,-49.1098642818385)) ;
#54152 = CARTESIAN_POINT('Ctrl Pts',(181.528635291814,585.413124159944,-49.1141054952774)) ;
#54153 = CARTESIAN_POINT('Ctrl Pts',(181.51568743049,585.354421552545,-49.1182862646058)) ;
#54154 = CARTESIAN_POINT('Ctrl Pts',(181.502748495606,585.295759415561,-49.1224641516522)) ;
#54155 = CARTESIAN_POINT('Ctrl Pts',(181.486655266837,585.23774059531,-49.1265815797148)) ;
#54156 = CARTESIAN_POINT('Ctrl Pts',(181.467504049314,585.180723452478,-49.1306220736233)) ;
#54157 = CARTESIAN_POINT('Ctrl Pts',(181.448358461983,585.123723071894,-49.1346613796828)) ;
#54158 = CARTESIAN_POINT('Ctrl Pts',(181.426156640988,585.067723872839,-49.1386238192241)) ;
#54159 = CARTESIAN_POINT('Ctrl Pts',(181.401029308306,585.01307466407,-49.1425163763437)) ;
#54160 = CARTESIAN_POINT('Ctrl Pts',(181.37588165729,584.95838126514,-49.1464120810427)) ;
#54161 = CARTESIAN_POINT('Ctrl Pts',(181.347803621948,584.905040214261,-49.1502379281539)) ;
#54162 = CARTESIAN_POINT('Ctrl Pts',(181.316962186217,584.853389923659,-49.1540232238451)) ;
#54163 = CARTESIAN_POINT('Ctrl Pts',(181.286109214421,584.801720313557,-49.1578099354048)) ;
#54164 = CARTESIAN_POINT('Ctrl Pts',(181.252490551254,584.751743010917,-49.1615563552486)) ;
#54165 = CARTESIAN_POINT('Ctrl Pts',(181.216312051274,584.703782191105,-49.1653109644898)) ;
#54166 = CARTESIAN_POINT('Ctrl Pts',(181.180066428381,584.655732388335,-49.1690725397553)) ;
#54167 = CARTESIAN_POINT('Ctrl Pts',(181.14125117188,584.609707030218,-49.1728428254195)) ;
#54168 = CARTESIAN_POINT('Ctrl Pts',(181.100116031628,584.566011852995,-49.1766839806197)) ;
#54169 = CARTESIAN_POINT('Ctrl Pts',(181.064117916884,584.527773403004,-49.1800454458973)) ;
#54170 = CARTESIAN_POINT('Ctrl Pts',(181.026343714903,584.491319509308,-49.1834617127504)) ;
#54171 = CARTESIAN_POINT('Ctrl Pts',(180.986990038803,584.456836965442,-49.1869773558899)) ;
#54172 = CARTESIAN_POINT('Ctrl Pts',(180.986964608508,584.456814682867,-49.1869796276939)) ;
#54173 = CARTESIAN_POINT('Ctrl Pts',(180.986939177554,584.456792401114,-49.1869818995395)) ;
#54174 = CARTESIAN_POINT('Ctrl Pts',(180.98691374594,584.456770120182,-49.1869841714265)) ;
#54175 = CARTESIAN_POINT('Ctrl Pts',(180.945140375073,584.420171985243,-49.1907159196502)) ;
#54176 = CARTESIAN_POINT('Ctrl Pts',(180.901419378894,584.385655591161,-49.1945700929975)) ;
#54177 = CARTESIAN_POINT('Ctrl Pts',(180.856000692707,584.35340379413,-49.1984832169383)) ;
#54178 = CARTESIAN_POINT('Ctrl Pts',(180.851869769652,584.350470426763,-49.1988391236204)) ;
#54179 = CARTESIAN_POINT('Ctrl Pts',(180.84772483842,584.347555794413,-49.199195517958)) ;
#54180 = CARTESIAN_POINT('Ctrl Pts',(180.843566108376,584.34466003511,-49.1995523521944)) ;
#54181 = CARTESIAN_POINT('Ctrl Pts',(180.793070642185,584.309499610057,-49.2038850477349)) ;
#54182 = CARTESIAN_POINT('Ctrl Pts',(180.740534887717,584.277120936133,-49.2082819349534)) ;
#54183 = CARTESIAN_POINT('Ctrl Pts',(180.686313313283,584.247724422448,-49.2126719944644)) ;
#54184 = CARTESIAN_POINT('Ctrl Pts',(180.632892815892,584.218762216924,-49.2169971946287)) ;
#54185 = CARTESIAN_POINT('Ctrl Pts',(180.577836064427,584.192694277852,-49.2213154880044)) ;
#54186 = CARTESIAN_POINT('Ctrl Pts',(180.521493140722,584.169674877758,-49.2255797075153)) ;
#54187 = CARTESIAN_POINT('Ctrl Pts',(180.465182943006,584.146668848155,-49.2298414502147)) ;
#54188 = CARTESIAN_POINT('Ctrl Pts',(180.407588084837,584.126707692432,-49.2340490505442)) ;
#54189 = CARTESIAN_POINT('Ctrl Pts',(180.349068314023,584.109911717571,-49.238179348656)) ;
#54190 = CARTESIAN_POINT('Ctrl Pts',(180.290560694548,584.093119230311,-49.2423087891319)) ;
#54191 = CARTESIAN_POINT('Ctrl Pts',(180.231128556488,584.079490647407,-49.2463609597265)) ;
#54192 = CARTESIAN_POINT('Ctrl Pts',(180.171141520504,584.069113116492,-49.2503375872865)) ;
#54193 = CARTESIAN_POINT('Ctrl Pts',(180.10951115719,584.05845129615,-49.2544231533971)) ;
#54194 = CARTESIAN_POINT('Ctrl Pts',(180.047295052453,584.051221453135,-49.2584289947099)) ;
#54195 = CARTESIAN_POINT('Ctrl Pts',(179.984904894767,584.047479937027,-49.2623833427958)) ;
#54196 = CARTESIAN_POINT('Ctrl Pts',(179.924095112789,584.043833195502,-49.2662375251522)) ;
#54197 = CARTESIAN_POINT('Ctrl Pts',(179.863120082857,584.043500462936,-49.2700431605542)) ;
#54198 = CARTESIAN_POINT('Ctrl Pts',(179.802370493183,584.046494749208,-49.2738478860765)) ;
#54199 = CARTESIAN_POINT('Ctrl Pts',(179.739252686439,584.049605762521,-49.2778009322042)) ;
#54200 = CARTESIAN_POINT('Ctrl Pts',(179.676378371499,584.056309132488,-49.2817534251688)) ;
#54201 = CARTESIAN_POINT('Ctrl Pts',(179.614194658282,584.066568113834,-49.2857766618069)) ;
#54202 = CARTESIAN_POINT('Ctrl Pts',(179.560517819468,584.075423643033,-49.2892495104576)) ;
#54203 = CARTESIAN_POINT('Ctrl Pts',(179.507354576915,584.086928478519,-49.292775733492)) ;
#54204 = CARTESIAN_POINT('Ctrl Pts',(179.454998848441,584.101020396693,-49.2964059494497)) ;
#54205 = CARTESIAN_POINT('Ctrl Pts',(179.44673574158,584.103244470908,-49.2969788927218)) ;
#54206 = CARTESIAN_POINT('Ctrl Pts',(179.438492652571,584.105532944415,-49.2975544263657)) ;
#54207 = CARTESIAN_POINT('Ctrl Pts',(179.430270626706,584.10788552758,-49.2981327493788)) ;
#54208 = CARTESIAN_POINT('Ctrl Pts',(179.430236403881,584.107895319819,-49.2981351565528)) ;
#54209 = CARTESIAN_POINT('Ctrl Pts',(179.430202181422,584.107905113168,-49.2981375637751)) ;
#54210 = CARTESIAN_POINT('Ctrl Pts',(179.430167959327,584.107914907628,-49.2981399710457)) ;
#54211 = CARTESIAN_POINT('Ctrl Pts',(179.377307486094,584.123043724261,-49.3018583134886)) ;
#54212 = CARTESIAN_POINT('Ctrl Pts',(179.325121598491,584.140887420871,-49.3057022622174)) ;
#54213 = CARTESIAN_POINT('Ctrl Pts',(179.273893181901,584.16133916302,-49.309609012445)) ;
#54214 = CARTESIAN_POINT('Ctrl Pts',(179.268892802009,584.163335447251,-49.3099903483632)) ;
#54215 = CARTESIAN_POINT('Ctrl Pts',(179.263901567599,584.165356546063,-49.3103722826299)) ;
#54216 = CARTESIAN_POINT('Ctrl Pts',(179.258919756129,584.167402337824,-49.3107547568374)) ;
#54217 = CARTESIAN_POINT('Ctrl Pts',(179.202005494062,584.190774303856,-49.3151242994051)) ;
#54218 = CARTESIAN_POINT('Ctrl Pts',(179.146317320101,584.217373982964,-49.3195636175663)) ;
#54219 = CARTESIAN_POINT('Ctrl Pts',(179.092218229118,584.247012036341,-49.3239994237309)) ;
#54220 = CARTESIAN_POINT('Ctrl Pts',(179.039121233796,584.276101094085,-49.3283530639657)) ;
#54221 = CARTESIAN_POINT('Ctrl Pts',(178.987554685352,584.308116639412,-49.3327030365493)) ;
#54222 = CARTESIAN_POINT('Ctrl Pts',(178.937836152509,584.34284975659,-49.3370002826777)) ;
#54223 = CARTESIAN_POINT('Ctrl Pts',(178.888149236528,584.377560786387,-49.3412947961141)) ;
#54224 = CARTESIAN_POINT('Ctrl Pts',(178.840307890223,584.414985838712,-49.3455365073293)) ;
#54225 = CARTESIAN_POINT('Ctrl Pts',(178.794606171649,584.454889421259,-49.3497000203128)) ;
#54226 = CARTESIAN_POINT('Ctrl Pts',(178.748916150452,584.494782790464,-49.3538624676431)) ;
#54227 = CARTESIAN_POINT('Ctrl Pts',(178.705364697062,584.537153420526,-49.3579467461379)) ;
#54228 = CARTESIAN_POINT('Ctrl Pts',(178.664223181621,584.581739687353,-49.3619521589631)) ;
#54229 = CARTESIAN_POINT('Ctrl Pts',(178.621669202069,584.62785668296,-49.3660950849987)) ;
#54230 = CARTESIAN_POINT('Ctrl Pts',(178.581693798529,584.676344295866,-49.3701536069118)) ;
#54231 = CARTESIAN_POINT('Ctrl Pts',(178.544570351805,584.726882868498,-49.37415392759)) ;
#54232 = CARTESIAN_POINT('Ctrl Pts',(178.50863255681,584.775807335993,-49.3780264856936)) ;
#54233 = CARTESIAN_POINT('Ctrl Pts',(178.475367605706,584.826653805537,-49.3818448801019)) ;
#54234 = CARTESIAN_POINT('Ctrl Pts',(178.444995694823,584.879103570419,-49.3856546815712)) ;
#54235 = CARTESIAN_POINT('Ctrl Pts',(178.41312074896,584.934148951743,-49.3896530212229)) ;
#54236 = CARTESIAN_POINT('Ctrl Pts',(178.384433144334,584.990960659604,-49.3936422722471)) ;
#54237 = CARTESIAN_POINT('Ctrl Pts',(178.359148090972,585.049134680607,-49.3976942933565)) ;
#54238 = CARTESIAN_POINT('Ctrl Pts',(178.337346035383,585.099295272383,-49.4011881514952)) ;
#54239 = CARTESIAN_POINT('Ctrl Pts',(178.318073160041,585.150469561677,-49.4047293400311)) ;
#54240 = CARTESIAN_POINT('Ctrl Pts',(178.301437748954,585.20237200772,-49.408369639193)) ;
#54241 = CARTESIAN_POINT('Ctrl Pts',(178.298785756976,585.210646216864,-49.4089499701583)) ;
#54242 = CARTESIAN_POINT('Ctrl Pts',(178.296200705478,585.218938992642,-49.4095328199461)) ;
#54243 = CARTESIAN_POINT('Ctrl Pts',(178.293682934059,585.227249250715,-49.410118398344)) ;
#54244 = CARTESIAN_POINT('Ctrl Pts',(178.293677611746,585.227266817759,-49.4101196361974)) ;
#54245 = CARTESIAN_POINT('Ctrl Pts',(178.293672289732,585.227284384881,-49.410120874063)) ;
#54246 = CARTESIAN_POINT('Ctrl Pts',(178.29366696802,585.227301952081,-49.4101221119408)) ;
#54247 = CARTESIAN_POINT('Ctrl Pts',(178.277369746688,585.281099775292,-49.4139129910346)) ;
#54248 = CARTESIAN_POINT('Ctrl Pts',(178.263842601223,585.335821009913,-49.41782811536)) ;
#54249 = CARTESIAN_POINT('Ctrl Pts',(178.253148005755,585.391158117052,-49.4218051187755)) ;
#54250 = CARTESIAN_POINT('Ctrl Pts',(178.252075075313,585.396709787236,-49.42220410984)) ;
#54251 = CARTESIAN_POINT('Ctrl Pts',(178.251030638063,585.402267616169,-49.4226037237184)) ;
#54252 = CARTESIAN_POINT('Ctrl Pts',(178.250014745413,585.407831266905,-49.4230038974354)) ;
#54253 = CARTESIAN_POINT('Ctrl Pts',(178.238896357501,585.468722372946,-49.4273835793025)) ;
#54254 = CARTESIAN_POINT('Ctrl Pts',(178.231198848605,585.530316549137,-49.4318296844121)) ;
#54255 = CARTESIAN_POINT('Ctrl Pts',(178.226957393479,585.592209679162,-49.4362730601451)) ;
#54256 = CARTESIAN_POINT('Ctrl Pts',(178.222721181383,585.65402630064,-49.4407109432454)) ;
#54257 = CARTESIAN_POINT('Ctrl Pts',(178.221932117161,585.716141233715,-49.4451457640036)) ;
#54258 = CARTESIAN_POINT('Ctrl Pts',(178.224586920693,585.77815744219,-49.4495292153227)) ;
#54259 = CARTESIAN_POINT('Ctrl Pts',(178.227239278417,585.84011651659,-49.4539086282713)) ;
#54260 = CARTESIAN_POINT('Ctrl Pts',(178.233329040899,585.901977131034,-49.458236630351)) ;
#54261 = CARTESIAN_POINT('Ctrl Pts',(178.242818227128,585.963347489938,-49.462489098499)) ;
#54262 = CARTESIAN_POINT('Ctrl Pts',(178.252301656368,586.024680616099,-49.46673898672)) ;
#54263 = CARTESIAN_POINT('Ctrl Pts',(178.265180439986,586.085524097166,-49.4709134398764)) ;
#54264 = CARTESIAN_POINT('Ctrl Pts',(178.281382420909,586.145490231204,-49.475013341583)) ;
#54265 = CARTESIAN_POINT('Ctrl Pts',(178.297585993295,586.205462255501,-49.4791136460083)) ;
#54266 = CARTESIAN_POINT('Ctrl Pts',(178.317113611036,586.264556692915,-49.4831395187431)) ;
#54267 = CARTESIAN_POINT('Ctrl Pts',(178.339856941589,586.32238948273,-49.4871157690085)) ;
#54268 = CARTESIAN_POINT('Ctrl Pts',(178.362599508045,586.380220329561,-49.4910918856856)) ;
#54269 = CARTESIAN_POINT('Ctrl Pts',(178.388557894661,586.436789430184,-49.4950186757842)) ;
#54270 = CARTESIAN_POINT('Ctrl Pts',(178.417583737016,586.491718346697,-49.4989417091056)) ;
#54271 = CARTESIAN_POINT('Ctrl Pts',(178.446638728903,586.546702426199,-49.5028686821778)) ;
#54272 = CARTESIAN_POINT('Ctrl Pts',(178.478767778577,586.600042640508,-49.5067923950255)) ;
#54273 = CARTESIAN_POINT('Ctrl Pts',(178.51377617567,586.65136916444,-49.5107734463125)) ;
#54274 = CARTESIAN_POINT('Ctrl Pts',(178.546547199693,586.69941543015,-49.514500070157)) ;
#54275 = CARTESIAN_POINT('Ctrl Pts',(178.581841161819,586.745696770216,-49.5182775936648)) ;
#54276 = CARTESIAN_POINT('Ctrl Pts',(178.619456745563,586.789923813584,-49.5221601717599)) ;
#54277 = CARTESIAN_POINT('',(181.142689770678,586.808573586438,-49.5221525629812)) ;
#54278 = CARTESIAN_POINT('Origin',(179.888527625416,585.710565160536,-49.5221601717598)) ;
#54279 = CARTESIAN_POINT('',(181.554057944425,585.711436268501,-48.8998676108129)) ;
#54280 = CARTESIAN_POINT('Ctrl Pts',(181.142689782808,586.808573597058,-49.5221525628444)) ;
#54281 = CARTESIAN_POINT('Ctrl Pts',(181.107984462542,586.848168254349,-49.5185580363667)) ;
#54282 = CARTESIAN_POINT('Ctrl Pts',(181.071300684857,586.886147988108,-49.5148671084872)) ;
#54283 = CARTESIAN_POINT('Ctrl Pts',(181.03282965584,586.922325429852,-49.5111334393229)) ;
#54284 = CARTESIAN_POINT('Ctrl Pts',(180.98877560723,586.963753039612,-49.5068579300094)) ;
#54285 = CARTESIAN_POINT('Ctrl Pts',(180.94237691035,587.002818089248,-49.5025269351851)) ;
#54286 = CARTESIAN_POINT('Ctrl Pts',(180.89393693784,587.039280186148,-49.4982065963733)) ;
#54287 = CARTESIAN_POINT('Ctrl Pts',(180.845546327173,587.075705127033,-49.4938906601216)) ;
#54288 = CARTESIAN_POINT('Ctrl Pts',(180.795118731165,587.10953269946,-49.4895856561117)) ;
#54289 = CARTESIAN_POINT('Ctrl Pts',(180.742973687493,587.140557484973,-49.4853367559894)) ;
#54290 = CARTESIAN_POINT('Ctrl Pts',(180.690861998196,587.171562425603,-49.4810905736596)) ;
#54291 = CARTESIAN_POINT('Ctrl Pts',(180.637035096445,587.199768259184,-49.4769005415144)) ;
#54292 = CARTESIAN_POINT('Ctrl Pts',(180.581827802258,587.225001374835,-49.4727879430955)) ;
#54293 = CARTESIAN_POINT('Ctrl Pts',(180.526634877501,587.250227922777,-49.4686764151093)) ;
#54294 = CARTESIAN_POINT('Ctrl Pts',(180.470062289381,587.27248324267,-49.4646422709636)) ;
#54295 = CARTESIAN_POINT('Ctrl Pts',(180.412460153598,587.291625017121,-49.4606821959048)) ;
#54296 = CARTESIAN_POINT('Ctrl Pts',(180.354809484317,587.310782919746,-49.4567187842284)) ;
#54297 = CARTESIAN_POINT('Ctrl Pts',(180.296127532896,587.326821832658,-49.4528294423666)) ;
#54298 = CARTESIAN_POINT('Ctrl Pts',(180.236780813647,587.339632199945,-49.4489872070466)) ;
#54299 = CARTESIAN_POINT('Ctrl Pts',(180.177411791505,587.352447381453,-49.4451435277889)) ;
#54300 = CARTESIAN_POINT('Ctrl Pts',(180.117377518728,587.362031250819,-49.441346717111)) ;
#54301 = CARTESIAN_POINT('Ctrl Pts',(180.057060338566,587.368311241818,-49.4375490757087)) ;
#54302 = CARTESIAN_POINT('Ctrl Pts',(179.996628619868,587.374603158125,-49.4337442228239)) ;
#54303 = CARTESIAN_POINT('Ctrl Pts',(179.935913016452,587.377578105159,-49.4299380617709)) ;
#54304 = CARTESIAN_POINT('Ctrl Pts',(179.875312773369,587.377206876537,-49.4260673862609)) ;
#54305 = CARTESIAN_POINT('Ctrl Pts',(179.820862517637,587.376873321877,-49.4225895244464)) ;
#54306 = CARTESIAN_POINT('Ctrl Pts',(179.766505007503,587.373838347776,-49.4190589885622)) ;
#54307 = CARTESIAN_POINT('Ctrl Pts',(179.712540166677,587.368117441668,-49.4154254390394)) ;
#54308 = CARTESIAN_POINT('Ctrl Pts',(179.707745453804,587.367609145864,-49.4151026024219)) ;
#54309 = CARTESIAN_POINT('Ctrl Pts',(179.702953812063,587.367079665455,-49.4147789526031)) ;
#54310 = CARTESIAN_POINT('Ctrl Pts',(179.698165434781,587.366529021736,-49.4144544542754)) ;
#54311 = CARTESIAN_POINT('Ctrl Pts',(179.698131755894,587.366525148802,-49.4144521719276)) ;
#54312 = CARTESIAN_POINT('Ctrl Pts',(179.698098077168,587.366521274822,-49.4144498895378)) ;
#54313 = CARTESIAN_POINT('Ctrl Pts',(179.698064398604,587.366517399794,-49.414447607106)) ;
#54314 = CARTESIAN_POINT('Ctrl Pts',(179.642896317683,587.360169806438,-49.4107088080871)) ;
#54315 = CARTESIAN_POINT('Ctrl Pts',(179.587963110748,587.350981727434,-49.4068474613973)) ;
#54316 = CARTESIAN_POINT('Ctrl Pts',(179.53356734119,587.33901541415,-49.4029266301077)) ;
#54317 = CARTESIAN_POINT('Ctrl Pts',(179.528499936043,587.337900655447,-49.4025613730148)) ;
#54318 = CARTESIAN_POINT('Ctrl Pts',(179.523437221136,587.336761812741,-49.4021955996892)) ;
#54319 = CARTESIAN_POINT('Ctrl Pts',(179.518379456723,587.335598953164,-49.4018293611151)) ;
#54320 = CARTESIAN_POINT('Ctrl Pts',(179.458430829169,587.32181582094,-49.3974884116204)) ;
#54321 = CARTESIAN_POINT('Ctrl Pts',(179.39917320668,587.304654617268,-49.3930827597336)) ;
#54322 = CARTESIAN_POINT('Ctrl Pts',(179.340991973531,587.284243100262,-49.3886832329072)) ;
#54323 = CARTESIAN_POINT('Ctrl Pts',(179.283548964587,587.264090571852,-49.384339528844)) ;
#54324 = CARTESIAN_POINT('Ctrl Pts',(179.227154971626,587.240770057717,-49.3800020875789)) ;
#54325 = CARTESIAN_POINT('Ctrl Pts',(179.172160543843,587.214437864316,-49.3757185289197)) ;
#54326 = CARTESIAN_POINT('Ctrl Pts',(179.117199455987,587.188121634594,-49.3714375671332)) ;
#54327 = CARTESIAN_POINT('Ctrl Pts',(179.063636152059,587.158797475377,-49.3672105577313)) ;
#54328 = CARTESIAN_POINT('Ctrl Pts',(179.011802420145,587.126651659001,-49.3630612214273)) ;
#54329 = CARTESIAN_POINT('Ctrl Pts',(178.959980983161,587.094513467592,-49.3589128693433)) ;
#54330 = CARTESIAN_POINT('Ctrl Pts',(178.909888329004,587.059554939623,-49.35484215551)) ;
#54331 = CARTESIAN_POINT('Ctrl Pts',(178.861838281852,587.021991904379,-49.3508479809358)) ;
#54332 = CARTESIAN_POINT('Ctrl Pts',(178.812648695837,586.98353803674,-49.3467590818521)) ;
#54333 = CARTESIAN_POINT('Ctrl Pts',(178.765599983442,586.942354422518,-49.342750368405)) ;
#54334 = CARTESIAN_POINT('Ctrl Pts',(178.721008159666,586.898705850122,-49.3387946729961)) ;
#54335 = CARTESIAN_POINT('Ctrl Pts',(178.677394024503,586.85601428528,-49.3349257073513)) ;
#54336 = CARTESIAN_POINT('Ctrl Pts',(178.636130423477,586.810964610041,-49.3311071067563)) ;
#54337 = CARTESIAN_POINT('Ctrl Pts',(178.597490526956,586.763837833895,-49.32729200388)) ;
#54338 = CARTESIAN_POINT('Ctrl Pts',(178.557551357159,586.715126411663,-49.3233486175025)) ;
#54339 = CARTESIAN_POINT('Ctrl Pts',(178.520416004959,586.664195401138,-49.3194085375781)) ;
#54340 = CARTESIAN_POINT('Ctrl Pts',(178.486354817132,586.611395428241,-49.315402397988)) ;
#54341 = CARTESIAN_POINT('Ctrl Pts',(178.456715576896,586.565450140332,-49.3119163500458)) ;
#54342 = CARTESIAN_POINT('Ctrl Pts',(178.429403520484,586.518088983246,-49.3083796318267)) ;
#54343 = CARTESIAN_POINT('Ctrl Pts',(178.404572302892,586.46957357431,-49.3047416214865)) ;
#54344 = CARTESIAN_POINT('Ctrl Pts',(178.400881920831,586.462363279681,-49.3042009452974)) ;
#54345 = CARTESIAN_POINT('Ctrl Pts',(178.397246248602,586.455127452085,-49.3036580318183)) ;
#54346 = CARTESIAN_POINT('Ctrl Pts',(178.393665701765,586.44786690752,-49.303112714877)) ;
#54347 = CARTESIAN_POINT('Ctrl Pts',(178.393651880362,586.447838880819,-49.3031106098786)) ;
#54348 = CARTESIAN_POINT('Ctrl Pts',(178.39363805978,586.447810853749,-49.3031085048444)) ;
#54349 = CARTESIAN_POINT('Ctrl Pts',(178.393624240019,586.447782826312,-49.3031063997743)) ;
#54350 = CARTESIAN_POINT('Ctrl Pts',(178.369108043619,586.398062271909,-49.2993720144895)) ;
#54351 = CARTESIAN_POINT('Ctrl Pts',(178.347096457758,586.347001046843,-49.2955151006196)) ;
#54352 = CARTESIAN_POINT('Ctrl Pts',(178.327701549311,586.29488609049,-49.2915988750396)) ;
#54353 = CARTESIAN_POINT('Ctrl Pts',(178.325903343545,586.290054233959,-49.2912357808058)) ;
#54354 = CARTESIAN_POINT('Ctrl Pts',(178.32412762298,586.285213355516,-49.2908721767205)) ;
#54355 = CARTESIAN_POINT('Ctrl Pts',(178.322374471421,586.280363705792,-49.2905081131671)) ;
#54356 = CARTESIAN_POINT('Ctrl Pts',(178.301455498579,586.22249666607,-49.2861640303352)) ;
#54357 = CARTESIAN_POINT('Ctrl Pts',(178.283750767876,586.163374848216,-49.2817551958583)) ;
#54358 = CARTESIAN_POINT('Ctrl Pts',(178.269362954821,586.103392394662,-49.2773529891969)) ;
#54359 = CARTESIAN_POINT('Ctrl Pts',(178.255191439883,586.04431168286,-49.2730169627817)) ;
#54360 = CARTESIAN_POINT('Ctrl Pts',(178.244237416278,585.984396026408,-49.2686876489745)) ;
#54361 = CARTESIAN_POINT('Ctrl Pts',(178.236559961635,585.924023222118,-49.2644127041021)) ;
#54362 = CARTESIAN_POINT('Ctrl Pts',(178.22888728024,585.863687952967,-49.2601404170599)) ;
#54363 = CARTESIAN_POINT('Ctrl Pts',(178.224486968306,585.80289609105,-49.2559225653516)) ;
#54364 = CARTESIAN_POINT('Ctrl Pts',(178.223382757553,585.74202602782,-49.2517829466959)) ;
#54365 = CARTESIAN_POINT('Ctrl Pts',(178.222278821394,585.681171101718,-49.2476443574778)) ;
#54366 = CARTESIAN_POINT('Ctrl Pts',(178.224469379528,585.620238034422,-49.2435839645257)) ;
#54367 = CARTESIAN_POINT('Ctrl Pts',(178.229943572563,585.559606195112,-49.2396007952297)) ;
#54368 = CARTESIAN_POINT('Ctrl Pts',(178.23557092052,585.49727802091,-49.235506186315)) ;
#54369 = CARTESIAN_POINT('Ctrl Pts',(178.244668567839,585.435268238171,-49.2314931739831)) ;
#54370 = CARTESIAN_POINT('Ctrl Pts',(178.257185002814,585.373989606572,-49.2275343780659)) ;
#54371 = CARTESIAN_POINT('Ctrl Pts',(178.269376243481,585.314303078659,-49.2236784371473)) ;
#54372 = CARTESIAN_POINT('Ctrl Pts',(178.284811055711,585.255310343257,-49.2198735637431)) ;
#54373 = CARTESIAN_POINT('Ctrl Pts',(178.303401637145,585.197391862252,-49.2160729854487)) ;
#54374 = CARTESIAN_POINT('Ctrl Pts',(178.322736058126,585.137155968165,-49.2121203398055)) ;
#54375 = CARTESIAN_POINT('Ctrl Pts',(178.345484658224,585.078082371193,-49.2081719214991)) ;
#54376 = CARTESIAN_POINT('Ctrl Pts',(178.371496808442,585.020594370926,-49.2041571171506)) ;
#54377 = CARTESIAN_POINT('Ctrl Pts',(178.393998334916,584.970865004106,-49.2006841544934)) ;
#54378 = CARTESIAN_POINT('Ctrl Pts',(178.418942193086,584.922321201104,-49.1971608572299)) ;
#54379 = CARTESIAN_POINT('Ctrl Pts',(178.446191760885,584.875233004446,-49.193536554343)) ;
#54380 = CARTESIAN_POINT('Ctrl Pts',(178.450428110662,584.86791244535,-49.192973102664)) ;
#54381 = CARTESIAN_POINT('Ctrl Pts',(178.454720172327,584.860626965898,-49.1924072097481)) ;
#54382 = CARTESIAN_POINT('Ctrl Pts',(178.459067418464,584.85337746811,-49.1918386852)) ;
#54383 = CARTESIAN_POINT('Ctrl Pts',(178.459082862209,584.853351714015,-49.1918366654966)) ;
#54384 = CARTESIAN_POINT('Ctrl Pts',(178.459098306649,584.853325960374,-49.19183464576)) ;
#54385 = CARTESIAN_POINT('Ctrl Pts',(178.459113751787,584.853300207187,-49.1918326259902)) ;
#54386 = CARTESIAN_POINT('Ctrl Pts',(178.487624142231,584.805762046414,-49.1881043051814)) ;
#54387 = CARTESIAN_POINT('Ctrl Pts',(178.518617592855,584.759603881883,-49.18425292184)) ;
#54388 = CARTESIAN_POINT('Ctrl Pts',(178.551913455752,584.715075054469,-49.1803416167241)) ;
#54389 = CARTESIAN_POINT('Ctrl Pts',(178.55502638043,584.710911928073,-49.179975937713)) ;
#54390 = CARTESIAN_POINT('Ctrl Pts',(178.558159394931,584.706763056428,-49.179609734931)) ;
#54391 = CARTESIAN_POINT('Ctrl Pts',(178.561312329619,584.702628650688,-49.1792430599776)) ;
#54392 = CARTESIAN_POINT('Ctrl Pts',(178.598625129582,584.65370082008,-49.1749037156707)) ;
#54393 = CARTESIAN_POINT('Ctrl Pts',(178.638733271553,584.606796511376,-49.1704989107955)) ;
#54394 = CARTESIAN_POINT('Ctrl Pts',(178.681360830051,584.562215154816,-49.1661000410291)) ;
#54395 = CARTESIAN_POINT('Ctrl Pts',(178.723373783523,584.518276573184,-49.1617645942586)) ;
#54396 = CARTESIAN_POINT('Ctrl Pts',(178.767833778899,584.476594070801,-49.1574351996113)) ;
#54397 = CARTESIAN_POINT('Ctrl Pts',(178.814454604535,584.437422014611,-49.1531596741286)) ;
#54398 = CARTESIAN_POINT('Ctrl Pts',(178.861046800754,584.398274013617,-49.1488867742064)) ;
#54399 = CARTESIAN_POINT('Ctrl Pts',(178.909797116817,584.361633259874,-49.144667812578)) ;
#54400 = CARTESIAN_POINT('Ctrl Pts',(178.960399765495,584.327724663864,-49.1405267321975)) ;
#54401 = CARTESIAN_POINT('Ctrl Pts',(179.010990156184,584.293824281874,-49.1363866549526)) ;
#54402 = CARTESIAN_POINT('Ctrl Pts',(179.06343198272,584.262654770551,-49.1323244239374)) ;
#54403 = CARTESIAN_POINT('Ctrl Pts',(179.117399960444,584.234412463701,-49.1283391819763)) ;
#54404 = CARTESIAN_POINT('Ctrl Pts',(179.172816837166,584.205411924806,-49.1242469466957)) ;
#54405 = CARTESIAN_POINT('Ctrl Pts',(179.229843040947,584.179498206949,-49.1202358771053)) ;
#54406 = CARTESIAN_POINT('Ctrl Pts',(179.288104459943,584.156850973599,-49.1162787826406)) ;
#54407 = CARTESIAN_POINT('Ctrl Pts',(179.344915081598,584.134767690571,-49.1124202258056)) ;
#54408 = CARTESIAN_POINT('Ctrl Pts',(179.402900122557,584.115790423885,-49.1086126257215)) ;
#54409 = CARTESIAN_POINT('Ctrl Pts',(179.461691796814,584.100051466002,-49.1048092711824)) ;
#54410 = CARTESIAN_POINT('Ctrl Pts',(179.522735553577,584.083709609288,-49.100860224786)) ;
#54411 = CARTESIAN_POINT('Ctrl Pts',(179.584649064956,584.07085977513,-49.096915335282)) ;
#54412 = CARTESIAN_POINT('Ctrl Pts',(179.646996633105,584.061604210247,-49.0929043640023)) ;
#54413 = CARTESIAN_POINT('Ctrl Pts',(179.701034699138,584.053582200069,-49.0894279632814)) ;
#54414 = CARTESIAN_POINT('Ctrl Pts',(179.755399729108,584.048259951212,-49.0859012657915)) ;
#54415 = CARTESIAN_POINT('Ctrl Pts',(179.809790218402,584.045669015311,-49.0822735343401)) ;
#54416 = CARTESIAN_POINT('Ctrl Pts',(179.818124300906,584.045272014404,-49.0817176685332)) ;
#54417 = CARTESIAN_POINT('Ctrl Pts',(179.826459055938,584.044939074602,-49.0811594306042)) ;
#54418 = CARTESIAN_POINT('Ctrl Pts',(179.834793482175,584.044670239962,-49.0805986380245)) ;
#54419 = CARTESIAN_POINT('Ctrl Pts',(179.834823095581,584.044669284754,-49.0805966454484)) ;
#54420 = CARTESIAN_POINT('Ctrl Pts',(179.834852708984,584.044668330355,-49.08059465284)) ;
#54421 = CARTESIAN_POINT('Ctrl Pts',(179.834882322383,584.044667376766,-49.0805926601994)) ;
#54422 = CARTESIAN_POINT('Ctrl Pts',(179.89031287822,584.042882441949,-49.0768628222176)) ;
#54423 = CARTESIAN_POINT('Ctrl Pts',(179.945928073396,584.043934871952,-49.0730101401795)) ;
#54424 = CARTESIAN_POINT('Ctrl Pts',(180.001420128914,584.047807748355,-49.0690977612818)) ;
#54425 = CARTESIAN_POINT('Ctrl Pts',(180.006592146767,584.048168711482,-49.0687331164094)) ;
#54426 = CARTESIAN_POINT('Ctrl Pts',(180.011763065144,584.048554152583,-49.0683679529639)) ;
#54427 = CARTESIAN_POINT('Ctrl Pts',(180.016932616892,584.048964043609,-49.0680023220714)) ;
#54428 = CARTESIAN_POINT('Ctrl Pts',(180.078269623518,584.053827422453,-49.0636640920727)) ;
#54429 = CARTESIAN_POINT('Ctrl Pts',(180.139419264204,584.062136143938,-49.0592607207662)) ;
#54430 = CARTESIAN_POINT('Ctrl Pts',(180.199980570948,584.073820390237,-49.0548634692596)) ;
#54431 = CARTESIAN_POINT('Ctrl Pts',(180.259684216819,584.085339165851,-49.0505284910224)) ;
#54432 = CARTESIAN_POINT('Ctrl Pts',(180.318816251292,584.100138128127,-49.0461997476564)) ;
#54433 = CARTESIAN_POINT('Ctrl Pts',(180.377007710914,584.118114368945,-49.0419249684783)) ;
#54434 = CARTESIAN_POINT('Ctrl Pts',(180.435163684631,584.136079647619,-49.0376527961159)) ;
#54435 = CARTESIAN_POINT('Ctrl Pts',(180.492380297348,584.157218219851,-49.033434657059)) ;
#54436 = CARTESIAN_POINT('Ctrl Pts',(180.548302743424,584.181394770773,-49.0292943989477)) ;
#54437 = CARTESIAN_POINT('Ctrl Pts',(180.60421185903,584.205565558629,-49.0251551277673)) ;
#54438 = CARTESIAN_POINT('Ctrl Pts',(180.658827394703,584.232772897588,-49.021093702746)) ;
#54439 = CARTESIAN_POINT('Ctrl Pts',(180.71180800419,584.262849602764,-49.017109168591)) ;
#54440 = CARTESIAN_POINT('Ctrl Pts',(180.766185932191,584.293719555458,-49.0130195457364)) ;
#54441 = CARTESIAN_POINT('Ctrl Pts',(180.818841350595,584.327612510181,-49.0090109078189)) ;
#54442 = CARTESIAN_POINT('Ctrl Pts',(180.869420955123,584.364311501216,-49.0050560054703)) ;
#54443 = CARTESIAN_POINT('Ctrl Pts',(180.918764119481,584.400113369644,-49.0011977824092)) ;
#54444 = CARTESIAN_POINT('Ctrl Pts',(180.966131535035,584.438585829195,-48.9973903373221)) ;
#54445 = CARTESIAN_POINT('Ctrl Pts',(181.011212654959,584.479491266715,-48.9935868859116)) ;
#54446 = CARTESIAN_POINT('Ctrl Pts',(181.057988237781,584.521934215867,-48.9896404742703)) ;
#54447 = CARTESIAN_POINT('Ctrl Pts',(181.102301774941,584.56699705875,-48.9856979397272)) ;
#54448 = CARTESIAN_POINT('Ctrl Pts',(181.143831842375,584.614369438218,-48.9816891407575)) ;
#54449 = CARTESIAN_POINT('Ctrl Pts',(181.179841353531,584.655444647874,-48.978213228)) ;
#54450 = CARTESIAN_POINT('Ctrl Pts',(181.213758940726,584.698256791488,-48.9746868419877)) ;
#54451 = CARTESIAN_POINT('Ctrl Pts',(181.245394843605,584.742569634588,-48.9710592886712)) ;
#54452 = CARTESIAN_POINT('Ctrl Pts',(181.250227492098,584.74933879162,-48.9705051495927)) ;
#54453 = CARTESIAN_POINT('Ctrl Pts',(181.255006992596,584.756142994574,-48.9699486497634)) ;
#54454 = CARTESIAN_POINT('Ctrl Pts',(181.259732771233,584.76298143342,-48.9693896084778)) ;
#54455 = CARTESIAN_POINT('Ctrl Pts',(181.259749783921,584.763006051632,-48.9693875959429)) ;
#54456 = CARTESIAN_POINT('Ctrl Pts',(181.259766795912,584.763030670289,-48.969385583375)) ;
#54457 = CARTESIAN_POINT('Ctrl Pts',(181.259783807207,584.763055289389,-48.9693835707741)) ;
#54458 = CARTESIAN_POINT('Ctrl Pts',(181.291520131742,584.808984757977,-48.9656288564589)) ;
#54459 = CARTESIAN_POINT('Ctrl Pts',(181.320938077529,584.856624312683,-48.9617498451787)) ;
#54460 = CARTESIAN_POINT('Ctrl Pts',(181.347885531636,584.905704447521,-48.9578107311307)) ;
#54461 = CARTESIAN_POINT('Ctrl Pts',(181.350579740329,584.910611483467,-48.957416898182)) ;
#54462 = CARTESIAN_POINT('Ctrl Pts',(181.353249255775,584.915532876534,-48.9570224644449)) ;
#54463 = CARTESIAN_POINT('Ctrl Pts',(181.35589392791,584.920468328871,-48.9566274940753)) ;
#54464 = CARTESIAN_POINT('Ctrl Pts',(181.38494191897,584.974677307554,-48.9522893019751)) ;
#54465 = CARTESIAN_POINT('Ctrl Pts',(181.41099312482,585.030588422366,-48.9478870035079)) ;
#54466 = CARTESIAN_POINT('Ctrl Pts',(181.43389140552,585.08783326796,-48.9434912449672)) ;
#54467 = CARTESIAN_POINT('Ctrl Pts',(181.45675452436,585.144990210221,-48.9391022364112)) ;
#54468 = CARTESIAN_POINT('Ctrl Pts',(181.476474770402,585.203476780266,-48.9347200839646)) ;
#54469 = CARTESIAN_POINT('Ctrl Pts',(181.492934154698,585.262919802661,-48.9303936265267)) ;
#54470 = CARTESIAN_POINT('Ctrl Pts',(181.509378746909,585.322309403482,-48.9260710572855)) ;
#54471 = CARTESIAN_POINT('Ctrl Pts',(181.522568473053,585.382653783217,-48.9218042230144)) ;
#54472 = CARTESIAN_POINT('Ctrl Pts',(181.532419267779,585.443573947974,-48.9176168821652)) ;
#54473 = CARTESIAN_POINT('Ctrl Pts',(181.542264969106,585.50446261368,-48.9134317063998)) ;
#54474 = CARTESIAN_POINT('Ctrl Pts',(181.548775146656,585.565926503788,-48.9093259471425)) ;
#54475 = CARTESIAN_POINT('Ctrl Pts',(181.551898804922,585.627579766142,-48.9052973376481)) ;
#54476 = CARTESIAN_POINT('Ctrl Pts',(181.553313650828,585.655505313185,-48.903472598459)) ;
#54477 = CARTESIAN_POINT('Ctrl Pts',(181.554034172762,585.683469607269,-48.9016633335739)) ;
#54478 = CARTESIAN_POINT('Ctrl Pts',(181.554057944425,585.711436268501,-48.8998676108129)) ;
#54479 = CARTESIAN_POINT('Ctrl Pts',(181.554527406634,585.711418964488,-48.8995973781893)) ;
#54480 = CARTESIAN_POINT('Ctrl Pts',(181.554489983662,585.784441188358,-48.8949679628962)) ;
#54481 = CARTESIAN_POINT('Ctrl Pts',(181.549651778247,585.857385731781,-48.8904707120407)) ;
#54482 = CARTESIAN_POINT('Ctrl Pts',(181.526228131845,586.033851596541,-48.8795849394622)) ;
#54483 = CARTESIAN_POINT('Ctrl Pts',(181.502610161245,586.136370402795,-48.8732596311718)) ;
#54484 = CARTESIAN_POINT('Ctrl Pts',(181.463924712828,586.252776874084,-48.8654287208587)) ;
#54485 = CARTESIAN_POINT('Ctrl Pts',(181.458073665102,586.269487882621,-48.8642879440639)) ;
#54486 = CARTESIAN_POINT('Ctrl Pts',(181.45195815568,586.286100543496,-48.8631342200737)) ;
#54487 = CARTESIAN_POINT('Origin',(179.888527625407,535.710565160536,-48.5221601717598)) ;
#54488 = CARTESIAN_POINT('',(181.45221818455,536.286166738762,-47.6539472813452)) ;
#54489 = CARTESIAN_POINT('',(181.451956083813,536.286106171625,-47.5221601717599)) ;
#54490 = CARTESIAN_POINT('',(181.451956083813,536.286106171625,-48.5221601717599)) ;
#54491 = CARTESIAN_POINT('',(179.964851548283,537.375708203335,-47.5221677607717)) ;
#54492 = CARTESIAN_POINT('Origin',(179.888527625407,535.710565160536,-47.5221601717598)) ;
#54493 = CARTESIAN_POINT('Ctrl Pts',(179.964851549022,537.375708219471,-47.5221677609092)) ;
#54494 = CARTESIAN_POINT('Ctrl Pts',(180.017493447496,537.373264646232,-47.5257656577699)) ;
#54495 = CARTESIAN_POINT('Ctrl Pts',(180.070106532583,537.368262770555,-47.5294601611829)) ;
#54496 = CARTESIAN_POINT('Ctrl Pts',(180.122424397359,537.360735327514,-47.5331974679367)) ;
#54497 = CARTESIAN_POINT('Ctrl Pts',(180.182280313502,537.35212331704,-47.5374732525202)) ;
#54498 = CARTESIAN_POINT('Ctrl Pts',(180.241751057591,537.340205240901,-47.541804502013)) ;
#54499 = CARTESIAN_POINT('Ctrl Pts',(180.300459543354,537.325068387249,-47.5461250770343)) ;
#54500 = CARTESIAN_POINT('Ctrl Pts',(180.359108191529,537.309946961567,-47.5504412483859)) ;
#54501 = CARTESIAN_POINT('Ctrl Pts',(180.416996272399,537.291613595545,-47.5547464690616)) ;
#54502 = CARTESIAN_POINT('Ctrl Pts',(180.473763962208,537.270190023334,-47.5589955665134)) ;
#54503 = CARTESIAN_POINT('Ctrl Pts',(180.530495330378,537.248780158556,-47.5632419452675)) ;
#54504 = CARTESIAN_POINT('Ctrl Pts',(180.586107791095,537.224284130594,-47.5674321545138)) ;
#54505 = CARTESIAN_POINT('Ctrl Pts',(180.640256859013,537.196855454874,-47.571544907143)) ;
#54506 = CARTESIAN_POINT('Ctrl Pts',(180.694391823976,537.169433922866,-47.5756565886187)) ;
#54507 = CARTESIAN_POINT('Ctrl Pts',(180.747064106785,537.139081243039,-47.5796908633611)) ;
#54508 = CARTESIAN_POINT('Ctrl Pts',(180.797944151154,537.105982401317,-47.5836510404053)) ;
#54509 = CARTESIAN_POINT('Ctrl Pts',(180.848867058718,537.07285567593,-47.5876145536463)) ;
#54510 = CARTESIAN_POINT('Ctrl Pts',(180.897994553398,537.036978038971,-47.5915039683802)) ;
#54511 = CARTESIAN_POINT('Ctrl Pts',(180.945012468566,536.998567723417,-47.595346240642)) ;
#54512 = CARTESIAN_POINT('Ctrl Pts',(180.992048047913,536.960142977477,-47.5991899564084)) ;
#54513 = CARTESIAN_POINT('Ctrl Pts',(181.036972186419,536.91918345128,-47.6029867675705)) ;
#54514 = CARTESIAN_POINT('Ctrl Pts',(181.079489768143,536.875942814335,-47.6067843656198)) ;
#54515 = CARTESIAN_POINT('Ctrl Pts',(181.122088091324,536.83262006284,-47.6105891753587)) ;
#54516 = CARTESIAN_POINT('Ctrl Pts',(181.162270232401,536.787007274233,-47.614395249141)) ;
#54517 = CARTESIAN_POINT('Ctrl Pts',(181.199764436783,536.739398363538,-47.6182657863322)) ;
#54518 = CARTESIAN_POINT('Ctrl Pts',(181.233454623253,536.696619669994,-47.6217436336917)) ;
#54519 = CARTESIAN_POINT('Ctrl Pts',(181.264974901598,536.652229070148,-47.6252741171322)) ;
#54520 = CARTESIAN_POINT('Ctrl Pts',(181.294150364587,536.606470722797,-47.6289075781151)) ;
#54521 = CARTESIAN_POINT('Ctrl Pts',(181.296749413567,536.602394414358,-47.6292312591159)) ;
#54522 = CARTESIAN_POINT('Ctrl Pts',(181.299329886898,536.598307240734,-47.629555757331)) ;
#54523 = CARTESIAN_POINT('Ctrl Pts',(181.301891679859,536.594209367662,-47.6298811083493)) ;
#54524 = CARTESIAN_POINT('Ctrl Pts',(181.301909469313,536.59418091145,-47.6298833676329)) ;
#54525 = CARTESIAN_POINT('Ctrl Pts',(181.301927257866,536.594152454722,-47.6298856269576)) ;
#54526 = CARTESIAN_POINT('Ctrl Pts',(181.301945045518,536.594123997479,-47.6298878863235)) ;
#54527 = CARTESIAN_POINT('Ctrl Pts',(181.331804988159,536.546353124972,-47.6336806598109)) ;
#54528 = CARTESIAN_POINT('Ctrl Pts',(181.359221289387,536.496961798078,-47.6375987039909)) ;
#54529 = CARTESIAN_POINT('Ctrl Pts',(181.384055566174,536.44622998794,-47.6415767454939)) ;
#54530 = CARTESIAN_POINT('Ctrl Pts',(181.386698090807,536.440831801428,-47.6420000343521)) ;
#54531 = CARTESIAN_POINT('Ctrl Pts',(181.389311383618,536.435418486105,-47.6424240025185)) ;
#54532 = CARTESIAN_POINT('Ctrl Pts',(181.391895280729,536.429990413812,-47.6428485713542)) ;
#54533 = CARTESIAN_POINT('Ctrl Pts',(181.414225124921,536.38308142195,-47.64651766325)) ;
#54534 = CARTESIAN_POINT('Ctrl Pts',(181.434360511508,536.335066076585,-47.6502315179149)) ;
#54535 = CARTESIAN_POINT('Ctrl Pts',(181.45221818455,536.286166738761,-47.6539472813452)) ;
#54536 = CARTESIAN_POINT('Origin',(179.888527625407,535.710565160536,-48.5221601717598)) ;
#54537 = CARTESIAN_POINT('',(181.451956081261,536.286106178557,-48.355715363061)) ;
#54538 = CARTESIAN_POINT('',(181.451936403117,536.286095981694,-48.1612817710483)) ;
#54539 = CARTESIAN_POINT('',(181.451956083813,536.286106171625,-48.5221601717599)) ;
#54540 = CARTESIAN_POINT('',(181.523656952658,535.391334705907,-47.5221601717599)) ;
#54541 = CARTESIAN_POINT('Ctrl Pts',(181.451936403117,536.286095981694,-48.1612817710483)) ;
#54542 = CARTESIAN_POINT('Ctrl Pts',(181.430786255221,536.3431128388,-48.1569560749123)) ;
#54543 = CARTESIAN_POINT('Ctrl Pts',(181.406503744676,536.39902563506,-48.1526530389213)) ;
#54544 = CARTESIAN_POINT('Ctrl Pts',(181.379248521711,536.453487888781,-48.1484135941381)) ;
#54545 = CARTESIAN_POINT('Ctrl Pts',(181.352007036685,536.507922690917,-48.1441762862382)) ;
#54546 = CARTESIAN_POINT('Ctrl Pts',(181.321795895814,536.560908459043,-48.140002597123)) ;
#54547 = CARTESIAN_POINT('Ctrl Pts',(181.288804681928,536.612116603094,-48.1359091023072)) ;
#54548 = CARTESIAN_POINT('Ctrl Pts',(181.255817829905,536.663317976772,-48.131816148704)) ;
#54549 = CARTESIAN_POINT('Ctrl Pts',(181.220051596958,536.71274213145,-48.1278033364018)) ;
#54550 = CARTESIAN_POINT('Ctrl Pts',(181.181725573904,536.760078123245,-48.1238625130584)) ;
#54551 = CARTESIAN_POINT('Ctrl Pts',(181.143362610377,536.807459739758,-48.1199178913588)) ;
#54552 = CARTESIAN_POINT('Ctrl Pts',(181.10243479128,536.852748988088,-48.1160452476124)) ;
#54553 = CARTESIAN_POINT('Ctrl Pts',(181.059193789639,536.89565339179,-48.1122129738959)) ;
#54554 = CARTESIAN_POINT('Ctrl Pts',(181.015932218975,536.9385782044,-48.1083788772308)) ;
#54555 = CARTESIAN_POINT('Ctrl Pts',(180.970355069448,536.9791155841,-48.1045848793185)) ;
#54556 = CARTESIAN_POINT('Ctrl Pts',(180.92274828037,537.016995687241,-48.1007792862713)) ;
#54557 = CARTESIAN_POINT('Ctrl Pts',(180.875051662244,537.054947266187,-48.0969665124669)) ;
#54558 = CARTESIAN_POINT('Ctrl Pts',(180.825317518399,537.090230986917,-48.0931415739393)) ;
#54559 = CARTESIAN_POINT('Ctrl Pts',(180.773870657243,537.122605010773,-48.089238577472)) ;
#54560 = CARTESIAN_POINT('Ctrl Pts',(180.732417795799,537.148690099253,-48.0860937719747)) ;
#54561 = CARTESIAN_POINT('Ctrl Pts',(180.689853713353,537.172886512724,-48.0828978288437)) ;
#54562 = CARTESIAN_POINT('Ctrl Pts',(180.646366990726,537.195086142804,-48.0796140404029)) ;
#54563 = CARTESIAN_POINT('Ctrl Pts',(180.646340288671,537.195099773994,-48.0796120240655)) ;
#54564 = CARTESIAN_POINT('Ctrl Pts',(180.646313586266,537.195113404431,-48.0796100076951)) ;
#54565 = CARTESIAN_POINT('Ctrl Pts',(180.646286883514,537.195127034117,-48.0796079912915)) ;
#54566 = CARTESIAN_POINT('Ctrl Pts',(180.596942026413,537.220313760083,-48.0758818156077)) ;
#54567 = CARTESIAN_POINT('Ctrl Pts',(180.546223913397,537.243017267462,-48.072032685545)) ;
#54568 = CARTESIAN_POINT('Ctrl Pts',(180.494417541183,537.2631218576,-48.0681237287464)) ;
#54569 = CARTESIAN_POINT('Ctrl Pts',(180.489575379792,537.265000963701,-48.0677583721526)) ;
#54570 = CARTESIAN_POINT('Ctrl Pts',(180.484723748153,537.266857373542,-48.067392492913)) ;
#54571 = CARTESIAN_POINT('Ctrl Pts',(180.479862901525,537.26869099806,-48.0670261425728)) ;
#54572 = CARTESIAN_POINT('Ctrl Pts',(180.42228599186,537.290410348894,-48.0626867091243)) ;
#54573 = CARTESIAN_POINT('Ctrl Pts',(180.363410209124,537.308931948238,-48.0582818477462)) ;
#54574 = CARTESIAN_POINT('Ctrl Pts',(180.303628548833,537.324147931288,-48.0538830980338)) ;
#54575 = CARTESIAN_POINT('Ctrl Pts',(180.244746808968,537.339134861248,-48.0495505646944)) ;
#54576 = CARTESIAN_POINT('Ctrl Pts',(180.184986275206,537.350915397909,-48.0452242453842)) ;
#54577 = CARTESIAN_POINT('Ctrl Pts',(180.124724061371,537.35942557223,-48.0409519905051)) ;
#54578 = CARTESIAN_POINT('Ctrl Pts',(180.064498653858,537.367930548796,-48.036682344989)) ;
#54579 = CARTESIAN_POINT('Ctrl Pts',(180.003772167374,537.373169285969,-48.032466833336)) ;
#54580 = CARTESIAN_POINT('Ctrl Pts',(179.942922703367,537.375113182866,-48.0283294649578)) ;
#54581 = CARTESIAN_POINT('Ctrl Pts',(179.882087705436,537.377056617629,-48.0241930801788)) ;
#54582 = CARTESIAN_POINT('Ctrl Pts',(179.821129808884,537.375706748115,-48.0201348046835)) ;
#54583 = CARTESIAN_POINT('Ctrl Pts',(179.760428479388,537.37106954864,-48.0161538758092)) ;
#54584 = CARTESIAN_POINT('Ctrl Pts',(179.69802854173,537.366302586194,-48.0120615484148)) ;
#54585 = CARTESIAN_POINT('Ctrl Pts',(179.63589979852,537.358061384484,-48.0080509496658)) ;
#54586 = CARTESIAN_POINT('Ctrl Pts',(179.574455561883,537.346392103887,-48.0040949077139)) ;
#54587 = CARTESIAN_POINT('Ctrl Pts',(179.514606435191,537.33502576115,-48.0002415657419)) ;
#54588 = CARTESIAN_POINT('Ctrl Pts',(179.45540687377,537.320406891227,-47.9964396179116)) ;
#54589 = CARTESIAN_POINT('Ctrl Pts',(179.397238341075,537.302618303786,-47.9926424434774)) ;
#54590 = CARTESIAN_POINT('Ctrl Pts',(179.336744330713,537.284118559282,-47.9886934645547)) ;
#54591 = CARTESIAN_POINT('Ctrl Pts',(179.277365778676,537.262189767387,-47.9847492329119)) ;
#54592 = CARTESIAN_POINT('Ctrl Pts',(179.219527711406,537.236976879441,-47.9807392359889)) ;
#54593 = CARTESIAN_POINT('Ctrl Pts',(179.169458944596,537.215150800756,-47.9772678959127)) ;
#54594 = CARTESIAN_POINT('Ctrl Pts',(179.120543672459,537.190863429084,-47.9737466152818)) ;
#54595 = CARTESIAN_POINT('Ctrl Pts',(179.073054148742,537.164247975577,-47.9701245983729)) ;
#54596 = CARTESIAN_POINT('Ctrl Pts',(179.06571208263,537.160133122364,-47.969564620392)) ;
#54597 = CARTESIAN_POINT('Ctrl Pts',(179.058403995181,537.155962638946,-47.9690022345754)) ;
#54598 = CARTESIAN_POINT('Ctrl Pts',(179.051130781925,537.151737032616,-47.9684372532125)) ;
#54599 = CARTESIAN_POINT('Ctrl Pts',(179.051104028684,537.151721489462,-47.9684351750275)) ;
#54600 = CARTESIAN_POINT('Ctrl Pts',(179.051077275914,537.151705945563,-47.9684330968074)) ;
#54601 = CARTESIAN_POINT('Ctrl Pts',(179.051050523616,537.151690400919,-47.9684310185521)) ;
#54602 = CARTESIAN_POINT('Ctrl Pts',(179.003049114866,537.123798784166,-47.9647020237161)) ;
#54603 = CARTESIAN_POINT('Ctrl Pts',(178.956398910279,537.093398984338,-47.9608501385307)) ;
#54604 = CARTESIAN_POINT('Ctrl Pts',(178.911352196445,537.060669048607,-47.9569384696096)) ;
#54605 = CARTESIAN_POINT('Ctrl Pts',(178.907144485097,537.057611819561,-47.9565730894896)) ;
#54606 = CARTESIAN_POINT('Ctrl Pts',(178.90295077754,537.054534295181,-47.9562071877562)) ;
#54607 = CARTESIAN_POINT('Ctrl Pts',(178.89877128705,537.051436642416,-47.9558408158403)) ;
#54608 = CARTESIAN_POINT('Ctrl Pts',(178.849353911677,537.014810678108,-47.9515089149689)) ;
#54609 = CARTESIAN_POINT('Ctrl Pts',(178.801921587587,536.97536529003,-47.9471119423943)) ;
#54610 = CARTESIAN_POINT('Ctrl Pts',(178.756776446934,536.933371843567,-47.9427208450714)) ;
#54611 = CARTESIAN_POINT('Ctrl Pts',(178.712204331618,536.891911418122,-47.9383854837588)) ;
#54612 = CARTESIAN_POINT('Ctrl Pts',(178.669861345495,536.847967454211,-47.9340561419435)) ;
#54613 = CARTESIAN_POINT('Ctrl Pts',(178.630006233896,536.80182351969,-47.9297805484483)) ;
#54614 = CARTESIAN_POINT('Ctrl Pts',(178.590175393923,536.755707686666,-47.9255075587749)) ;
#54615 = CARTESIAN_POINT('Ctrl Pts',(178.552829281113,536.707394618948,-47.921288386993)) ;
#54616 = CARTESIAN_POINT('Ctrl Pts',(178.518197433363,536.657187817612,-47.9171468560982)) ;
#54617 = CARTESIAN_POINT('Ctrl Pts',(178.483573895665,536.6069930636,-47.9130063189804)) ;
#54618 = CARTESIAN_POINT('Ctrl Pts',(178.451663355893,536.554905480944,-47.9089433872833)) ;
#54619 = CARTESIAN_POINT('Ctrl Pts',(178.422667046997,536.501248446199,-47.9049570602619)) ;
#54620 = CARTESIAN_POINT('Ctrl Pts',(178.392982608062,536.446318041885,-47.9008761311524)) ;
#54621 = CARTESIAN_POINT('Ctrl Pts',(178.366352670331,536.389742684962,-47.8968754586295)) ;
#54622 = CARTESIAN_POINT('Ctrl Pts',(178.342960883909,536.331891489663,-47.8929279781005)) ;
#54623 = CARTESIAN_POINT('Ctrl Pts',(178.32008248051,536.275309963171,-47.889067133515)) ;
#54624 = CARTESIAN_POINT('Ctrl Pts',(178.3003018577,536.217508013867,-47.8852568180468)) ;
#54625 = CARTESIAN_POINT('Ctrl Pts',(178.28375689859,536.158852427536,-47.8814502632968)) ;
#54626 = CARTESIAN_POINT('Ctrl Pts',(178.266655045212,536.098222526278,-47.8775155819976)) ;
#54627 = CARTESIAN_POINT('Ctrl Pts',(178.253011166435,536.036680420503,-47.8735844888598)) ;
#54628 = CARTESIAN_POINT('Ctrl Pts',(178.24293271949,535.97465557031,-47.8695877180918)) ;
#54629 = CARTESIAN_POINT('Ctrl Pts',(178.23416107659,535.920673062912,-47.8661091815555)) ;
#54630 = CARTESIAN_POINT('Ctrl Pts',(178.228089925971,535.866324024968,-47.8625802460645)) ;
#54631 = CARTESIAN_POINT('Ctrl Pts',(178.22475542632,535.811909811167,-47.8589503194738)) ;
#54632 = CARTESIAN_POINT('Ctrl Pts',(178.224260699275,535.803836581001,-47.8584117610567)) ;
#54633 = CARTESIAN_POINT('Ctrl Pts',(178.223826149891,535.795761846863,-47.85787097957)) ;
#54634 = CARTESIAN_POINT('Ctrl Pts',(178.223451832322,535.78768651858,-47.8573278097841)) ;
#54635 = CARTESIAN_POINT('Ctrl Pts',(178.223450282402,535.787653081413,-47.8573255607042)) ;
#54636 = CARTESIAN_POINT('Ctrl Pts',(178.223448733513,535.787619644236,-47.8573233115834)) ;
#54637 = CARTESIAN_POINT('Ctrl Pts',(178.223447185658,535.787586207049,-47.8573210624215)) ;
#54638 = CARTESIAN_POINT('Ctrl Pts',(178.220879007096,535.732107729501,-47.8535892869709)) ;
#54639 = CARTESIAN_POINT('Ctrl Pts',(178.221152741422,535.676404466823,-47.8497351147999)) ;
#54640 = CARTESIAN_POINT('Ctrl Pts',(178.224255523442,535.620785841418,-47.845822019635)) ;
#54641 = CARTESIAN_POINT('Ctrl Pts',(178.224537666018,535.615728321373,-47.845466193559)) ;
#54642 = CARTESIAN_POINT('Ctrl Pts',(178.224843180112,535.610671529998,-47.8451098802692)) ;
#54643 = CARTESIAN_POINT('Ctrl Pts',(178.225172043119,535.605615716879,-47.8447531274907)) ;
#54644 = CARTESIAN_POINT('Ctrl Pts',(178.2291660325,535.544213663552,-47.8404204212343)) ;
#54645 = CARTESIAN_POINT('Ctrl Pts',(178.236607089779,535.482950827978,-47.8360235538722)) ;
#54646 = CARTESIAN_POINT('Ctrl Pts',(178.247430894952,535.422229322234,-47.83163354596)) ;
#54647 = CARTESIAN_POINT('Ctrl Pts',(178.258094469473,535.362406709838,-47.8273085257134)) ;
#54648 = CARTESIAN_POINT('Ctrl Pts',(178.272040970573,535.303109346939,-47.822990442542)) ;
#54649 = CARTESIAN_POINT('Ctrl Pts',(178.2891727465,535.244707116931,-47.8187264598205)) ;
#54650 = CARTESIAN_POINT('Ctrl Pts',(178.306294572705,535.186338805529,-47.8144649535173)) ;
#54651 = CARTESIAN_POINT('Ctrl Pts',(178.326597866137,535.128864524065,-47.810257616129)) ;
#54652 = CARTESIAN_POINT('Ctrl Pts',(178.349952392273,535.072640536659,-47.8061276057299)) ;
#54653 = CARTESIAN_POINT('Ctrl Pts',(178.373302070798,535.016428219455,-47.8019984525815)) ;
#54654 = CARTESIAN_POINT('Ctrl Pts',(178.399701738795,534.961465708792,-47.7979465940857)) ;
#54655 = CARTESIAN_POINT('Ctrl Pts',(178.42898908063,534.90809631272,-47.7939703036623)) ;
#54656 = CARTESIAN_POINT('Ctrl Pts',(178.459080288826,534.853262056423,-47.7898848737299)) ;
#54657 = CARTESIAN_POINT('Ctrl Pts',(178.492220164428,534.800109776089,-47.7858792034445)) ;
#54658 = CARTESIAN_POINT('Ctrl Pts',(178.528196051012,534.74899651985,-47.7819250587245)) ;
#54659 = CARTESIAN_POINT('Ctrl Pts',(178.563258858755,534.699180533454,-47.7780712713889)) ;
#54660 = CARTESIAN_POINT('Ctrl Pts',(178.601015614503,534.651301563366,-47.774266056544)) ;
#54661 = CARTESIAN_POINT('Ctrl Pts',(178.641232903684,534.605673160823,-47.7704617801808)) ;
#54662 = CARTESIAN_POINT('Ctrl Pts',(178.683021154726,534.558262428303,-47.7665089017314)) ;
#54663 = CARTESIAN_POINT('Ctrl Pts',(178.727466530178,534.513282175998,-47.7625566076072)) ;
#54664 = CARTESIAN_POINT('Ctrl Pts',(178.774261469017,534.471059114624,-47.7585335895023)) ;
#54665 = CARTESIAN_POINT('Ctrl Pts',(178.814651902175,534.434614837092,-47.7550611745812)) ;
#54666 = CARTESIAN_POINT('Ctrl Pts',(178.856793369279,534.400223905242,-47.7515354072975)) ;
#54667 = CARTESIAN_POINT('Ctrl Pts',(178.900453967763,534.368077307673,-47.7479056720436)) ;
#54668 = CARTESIAN_POINT('Ctrl Pts',(178.907348500323,534.36300097406,-47.7473324932792)) ;
#54669 = CARTESIAN_POINT('Ctrl Pts',(178.914280941161,534.35798050338,-47.7467567219486)) ;
#54670 = CARTESIAN_POINT('Ctrl Pts',(178.921250410667,534.353016533284,-47.7461781587414)) ;
#54671 = CARTESIAN_POINT('Ctrl Pts',(178.92127922712,534.352996008908,-47.7461757665738)) ;
#54672 = CARTESIAN_POINT('Ctrl Pts',(178.921308044206,534.352975485499,-47.7461733743585)) ;
#54673 = CARTESIAN_POINT('Ctrl Pts',(178.921336861924,534.352954963055,-47.7461709820954)) ;
#54674 = CARTESIAN_POINT('Ctrl Pts',(178.966123819551,534.321060078073,-47.742453054699)) ;
#54675 = CARTESIAN_POINT('Ctrl Pts',(179.012612734901,534.291385373579,-47.7386095408294)) ;
#54676 = CARTESIAN_POINT('Ctrl Pts',(179.06054367861,534.264085405347,-47.7347032488684)) ;
#54677 = CARTESIAN_POINT('Ctrl Pts',(179.065219895963,534.261421978022,-47.7343221449544)) ;
#54678 = CARTESIAN_POINT('Ctrl Pts',(179.069909798089,534.258781150969,-47.7339404435024)) ;
#54679 = CARTESIAN_POINT('Ctrl Pts',(179.074613117271,534.256163065068,-47.7335582028372)) ;
#54680 = CARTESIAN_POINT('Ctrl Pts',(179.128372717476,534.226237974742,-47.7291891382377)) ;
#54681 = CARTESIAN_POINT('Ctrl Pts',(179.183891378524,534.19928405756,-47.7247503225493)) ;
#54682 = CARTESIAN_POINT('Ctrl Pts',(179.240794700056,534.175467057658,-47.7203150457455)) ;
#54683 = CARTESIAN_POINT('Ctrl Pts',(179.296641211464,534.152092387762,-47.7159621410302)) ;
#54684 = CARTESIAN_POINT('Ctrl Pts',(179.353821335501,534.131738726617,-47.7116129293004)) ;
#54685 = CARTESIAN_POINT('Ctrl Pts',(179.411973747117,534.114524071162,-47.7073164593425)) ;
#54686 = CARTESIAN_POINT('Ctrl Pts',(179.470089277145,534.097320333635,-47.703022714304)) ;
#54687 = CARTESIAN_POINT('Ctrl Pts',(179.529175848197,534.08325148744,-47.6987817869211)) ;
#54688 = CARTESIAN_POINT('Ctrl Pts',(179.588866018623,534.072400576345,-47.6946190627617)) ;
#54689 = CARTESIAN_POINT('Ctrl Pts',(179.648541017051,534.061552423325,-47.6904573966799)) ;
#54690 = CARTESIAN_POINT('Ctrl Pts',(179.708819285398,534.053920596761,-47.6863739046806)) ;
#54691 = CARTESIAN_POINT('Ctrl Pts',(179.769327101651,534.049554107817,-47.6823692729947)) ;
#54692 = CARTESIAN_POINT('Ctrl Pts',(179.831917325208,534.045037343932,-47.6782268198705)) ;
#54693 = CARTESIAN_POINT('Ctrl Pts',(179.894753151485,534.044014940913,-47.6741687791312)) ;
#54694 = CARTESIAN_POINT('Ctrl Pts',(179.957414141148,534.046501295686,-47.6701689286977)) ;
#54695 = CARTESIAN_POINT('Ctrl Pts',(180.018069251131,534.04890805822,-47.6662971199493)) ;
#54696 = CARTESIAN_POINT('Ctrl Pts',(180.078560412276,534.054602622417,-47.6624794560378)) ;
#54697 = CARTESIAN_POINT('Ctrl Pts',(180.138501190525,534.063558395427,-47.6586703531882)) ;
#54698 = CARTESIAN_POINT('Ctrl Pts',(180.2014153536,534.072958422923,-47.6546722983607)) ;
#54699 = CARTESIAN_POINT('Ctrl Pts',(180.263722955934,534.085952177943,-47.650683299333)) ;
#54700 = CARTESIAN_POINT('Ctrl Pts',(180.324973840245,534.102455945175,-47.6466314574514)) ;
#54701 = CARTESIAN_POINT('Ctrl Pts',(180.377779147805,534.116684090849,-47.643138303693)) ;
#54702 = CARTESIAN_POINT('Ctrl Pts',(180.429800058266,534.133521136602,-47.6395977799359)) ;
#54703 = CARTESIAN_POINT('Ctrl Pts',(180.4807458833,534.152873691095,-47.6359581034402)) ;
#54704 = CARTESIAN_POINT('Ctrl Pts',(180.488876769537,534.155962333174,-47.6353772158894)) ;
#54705 = CARTESIAN_POINT('Ctrl Pts',(180.496980374762,534.159115018295,-47.6347938027461)) ;
#54706 = CARTESIAN_POINT('Ctrl Pts',(180.505055636178,534.162331334421,-47.6342076535002)) ;
#54707 = CARTESIAN_POINT('Ctrl Pts',(180.50507280645,534.162338173211,-47.6342064071824)) ;
#54708 = CARTESIAN_POINT('Ctrl Pts',(180.505089976594,534.16234501229,-47.6342051608523)) ;
#54709 = CARTESIAN_POINT('Ctrl Pts',(180.505107146609,534.162351851656,-47.6342039145097)) ;
#54710 = CARTESIAN_POINT('Ctrl Pts',(180.55732647196,534.183152477957,-47.6304134015972)) ;
#54711 = CARTESIAN_POINT('Ctrl Pts',(180.608540633887,534.206694341041,-47.6264985681328)) ;
#54712 = CARTESIAN_POINT('Ctrl Pts',(180.658470286984,534.232834549517,-47.622521772505)) ;
#54713 = CARTESIAN_POINT('Ctrl Pts',(180.663485422641,534.235460177445,-47.622122327119)) ;
#54714 = CARTESIAN_POINT('Ctrl Pts',(180.668487577824,534.238111982171,-47.6217222565965)) ;
#54715 = CARTESIAN_POINT('Ctrl Pts',(180.673476456043,534.240789793202,-47.6213216241303)) ;
#54716 = CARTESIAN_POINT('Ctrl Pts',(180.728017873916,534.270065234301,-47.6169416689989)) ;
#54717 = CARTESIAN_POINT('Ctrl Pts',(180.780975776105,534.302453959571,-47.6124951845948)) ;
#54718 = CARTESIAN_POINT('Ctrl Pts',(180.832012241287,534.337731455741,-47.6080513472692)) ;
#54719 = CARTESIAN_POINT('Ctrl Pts',(180.882985559462,534.37296530335,-47.6036130082677)) ;
#54720 = CARTESIAN_POINT('Ctrl Pts',(180.932042496935,534.411080550936,-47.5991776497722)) ;
#54721 = CARTESIAN_POINT('Ctrl Pts',(180.978874654322,534.451827037993,-47.5947936045321)) ;
#54722 = CARTESIAN_POINT('Ctrl Pts',(181.025663601896,534.492535930195,-47.590413604243)) ;
#54723 = CARTESIAN_POINT('Ctrl Pts',(181.070232013022,534.53587116621,-47.5860849587363)) ;
#54724 = CARTESIAN_POINT('Ctrl Pts',(181.112297226174,534.581558727159,-47.5818318158203)) ;
#54725 = CARTESIAN_POINT('Ctrl Pts',(181.154336851441,534.627218496782,-47.5775812600521)) ;
#54726 = CARTESIAN_POINT('Ctrl Pts',(181.193876301892,534.675227782712,-47.5734061078654)) ;
#54727 = CARTESIAN_POINT('Ctrl Pts',(181.230657426143,534.725288401908,-47.5693054982439)) ;
#54728 = CARTESIAN_POINT('Ctrl Pts',(181.267442042625,534.775353774174,-47.5652044992848)) ;
#54729 = CARTESIAN_POINT('Ctrl Pts',(181.301467634746,534.827470979894,-47.561177922665)) ;
#54730 = CARTESIAN_POINT('Ctrl Pts',(181.332501452985,534.881315826386,-47.5572009793439)) ;
#54731 = CARTESIAN_POINT('Ctrl Pts',(181.363534173554,534.935158768377,-47.5532241766878)) ;
#54732 = CARTESIAN_POINT('Ctrl Pts',(181.391574986876,534.990729367568,-47.5492967112841)) ;
#54733 = CARTESIAN_POINT('Ctrl Pts',(181.416420496784,535.04767563909,-47.545373030922)) ;
#54734 = CARTESIAN_POINT('Ctrl Pts',(181.441290859478,535.104678873562,-47.5414454257303)) ;
#54735 = CARTESIAN_POINT('Ctrl Pts',(181.46295894898,535.16306063624,-47.537521109075)) ;
#54736 = CARTESIAN_POINT('Ctrl Pts',(181.48125699761,535.222438078838,-47.5335394975804)) ;
#54737 = CARTESIAN_POINT('Ctrl Pts',(181.49837261429,535.277978511998,-47.5298151804424)) ;
#54738 = CARTESIAN_POINT('Ctrl Pts',(181.512539443077,535.334389744362,-47.5260400792227)) ;
#54739 = CARTESIAN_POINT('Ctrl Pts',(181.523656952658,535.391334705907,-47.5221601717599)) ;
#54740 = CARTESIAN_POINT('Origin',(179.888527625407,535.710565160536,-47.5221601717598)) ;
#54741 = CARTESIAN_POINT('Ctrl Pts',(181.451956078709,536.28610618549,-48.355715363061)) ;
#54742 = CARTESIAN_POINT('Ctrl Pts',(181.443432156306,536.309260995037,-48.3540745386352)) ;
#54743 = CARTESIAN_POINT('Ctrl Pts',(181.434394207593,536.332225451491,-48.3524165071428)) ;
#54744 = CARTESIAN_POINT('Ctrl Pts',(181.397471519135,536.420250845626,-48.3459354847706)) ;
#54745 = CARTESIAN_POINT('Ctrl Pts',(181.365967014669,536.483698917522,-48.340990223511)) ;
#54746 = CARTESIAN_POINT('Ctrl Pts',(181.277601068931,536.636415683579,-48.3283947666615)) ;
#54747 = CARTESIAN_POINT('Ctrl Pts',(181.216091736306,536.722639766728,-48.3206303658353)) ;
#54748 = CARTESIAN_POINT('Ctrl Pts',(181.110468882847,536.844361891796,-48.3089844490963)) ;
#54749 = CARTESIAN_POINT('Ctrl Pts',(181.072023854145,536.884436283982,-48.3050211410803)) ;
#54750 = CARTESIAN_POINT('Ctrl Pts',(181.009770460592,536.943153818467,-48.2990986957174)) ;
#54751 = CARTESIAN_POINT('Ctrl Pts',(180.987338099798,536.96319295314,-48.2970563376968)) ;
#54752 = CARTESIAN_POINT('Ctrl Pts',(180.931618933764,537.010317618914,-48.2922127808431)) ;
#54753 = CARTESIAN_POINT('Ctrl Pts',(180.897806379057,537.036745051117,-48.2894535663643)) ;
#54754 = CARTESIAN_POINT('Ctrl Pts',(180.812623574893,537.098175148572,-48.2828255190749)) ;
#54755 = CARTESIAN_POINT('Ctrl Pts',(180.760243077164,537.131666138784,-48.279017615289)) ;
#54756 = CARTESIAN_POINT('Ctrl Pts',(180.601878725853,537.22086220908,-48.267912086069)) ;
#54757 = CARTESIAN_POINT('Ctrl Pts',(180.491638210104,537.26816620639,-48.2606540385479)) ;
#54758 = CARTESIAN_POINT('Ctrl Pts',(180.327909616524,537.318410706314,-48.249666551006)) ;
#54759 = CARTESIAN_POINT('Ctrl Pts',(180.277858489177,537.331257710468,-48.2462865682751)) ;
#54760 = CARTESIAN_POINT('Ctrl Pts',(180.171017288128,537.353446611314,-48.2389785635886)) ;
#54761 = CARTESIAN_POINT('Ctrl Pts',(180.114178534133,537.362212861074,-48.235036363122)) ;
#54762 = CARTESIAN_POINT('Ctrl Pts',(179.989684828334,537.374867477988,-48.22626691009)) ;
#54763 = CARTESIAN_POINT('Ctrl Pts',(179.922015858998,537.377602005444,-48.2214138178156)) ;
#54764 = CARTESIAN_POINT('Ctrl Pts',(179.738003164606,537.373828916416,-48.2080684094743)) ;
#54765 = CARTESIAN_POINT('Ctrl Pts',(179.622197594573,537.35925410166,-48.1994914040934)) ;
#54766 = CARTESIAN_POINT('Ctrl Pts',(179.47801536914,537.325507483639,-48.1891652565625)) ;
#54767 = CARTESIAN_POINT('Ctrl Pts',(179.447385903466,537.317411024265,-48.1869948434875)) ;
#54768 = CARTESIAN_POINT('Ctrl Pts',(179.381212312762,537.297883505801,-48.1823811388451)) ;
#54769 = CARTESIAN_POINT('Ctrl Pts',(179.345785026416,537.286122010407,-48.1799554593728)) ;
#54770 = CARTESIAN_POINT('Ctrl Pts',(179.210892862924,537.236248070254,-48.1707838500216)) ;
#54771 = CARTESIAN_POINT('Ctrl Pts',(179.114767732667,537.189820857744,-48.1643734454356)) ;
#54772 = CARTESIAN_POINT('Ctrl Pts',(178.945854579752,537.087236531047,-48.1522819882884)) ;
#54773 = CARTESIAN_POINT('Ctrl Pts',(178.872003144414,537.033641731672,-48.1466503524933)) ;
#54774 = CARTESIAN_POINT('Ctrl Pts',(178.764691293621,536.941453526979,-48.1375388800779)) ;
#54775 = CARTESIAN_POINT('Ctrl Pts',(178.727988158534,536.906910220609,-48.1342295303475)) ;
#54776 = CARTESIAN_POINT('Ctrl Pts',(178.651403205098,536.827986955213,-48.126841609869)) ;
#54777 = CARTESIAN_POINT('Ctrl Pts',(178.612227588258,536.783022596584,-48.1227379148407)) ;
#54778 = CARTESIAN_POINT('Ctrl Pts',(178.530771423917,536.678731357091,-48.1134273767143)) ;
#54779 = CARTESIAN_POINT('Ctrl Pts',(178.489801511131,536.618535994306,-48.1081852650483)) ;
#54780 = CARTESIAN_POINT('Ctrl Pts',(178.398398515099,536.463299758907,-48.0950919426553)) ;
#54781 = CARTESIAN_POINT('Ctrl Pts',(178.352973573254,536.365676904987,-48.0872091251478)) ;
#54782 = CARTESIAN_POINT('Ctrl Pts',(178.306927373818,536.235029980686,-48.0775709980731)) ;
#54783 = CARTESIAN_POINT('Ctrl Pts',(178.297413708337,536.205418509373,-48.0754457259631)) ;
#54784 = CARTESIAN_POINT('Ctrl Pts',(178.277924050782,536.138364102538,-48.070786331965)) ;
#54785 = CARTESIAN_POINT('Ctrl Pts',(178.268413962295,536.100806289195,-48.0682761758745)) ;
#54786 = CARTESIAN_POINT('Ctrl Pts',(178.249199603956,536.012019559273,-48.0624999914387)) ;
#54787 = CARTESIAN_POINT('Ctrl Pts',(178.240572828918,535.960598908355,-48.0592750798041)) ;
#54788 = CARTESIAN_POINT('Ctrl Pts',(178.217961590007,535.771973432546,-48.0476173435945)) ;
#54789 = CARTESIAN_POINT('Ctrl Pts',(178.218606939032,535.633597647715,-48.0393438108748)) ;
#54790 = CARTESIAN_POINT('Ctrl Pts',(178.242911202225,535.445670148723,-48.0271864231066)) ;
#54791 = CARTESIAN_POINT('Ctrl Pts',(178.25191156015,535.394796788973,-48.0238069394469)) ;
#54792 = CARTESIAN_POINT('Ctrl Pts',(178.275908015491,535.2882775437,-48.0164941350027)) ;
#54793 = CARTESIAN_POINT('Ctrl Pts',(178.291457127882,535.232827525934,-48.0125463568321)) ;
#54794 = CARTESIAN_POINT('Ctrl Pts',(178.331518686863,535.11400625026,-48.003758415065)) ;
#54795 = CARTESIAN_POINT('Ctrl Pts',(178.357100364966,535.051104601854,-47.9988921172518)) ;
#54796 = CARTESIAN_POINT('Ctrl Pts',(178.436497274949,534.885607409271,-47.98558304811)) ;
#54797 = CARTESIAN_POINT('Ctrl Pts',(178.497288605296,534.786766271574,-47.9770589579872)) ;
#54798 = CARTESIAN_POINT('Ctrl Pts',(178.58719448683,534.669845926503,-47.9667729997946)) ;
#54799 = CARTESIAN_POINT('Ctrl Pts',(178.607270803379,534.645226693984,-47.9645964878086)) ;
#54800 = CARTESIAN_POINT('Ctrl Pts',(178.652452763857,534.592947794466,-47.959975568195)) ;
#54801 = CARTESIAN_POINT('Ctrl Pts',(178.677808222789,534.565528598271,-47.9575485695418)) ;
#54802 = CARTESIAN_POINT('Ctrl Pts',(178.778991820137,534.463232767556,-47.9483717314691)) ;
#54803 = CARTESIAN_POINT('Ctrl Pts',(178.861018567761,534.394838172088,-47.9419572163795)) ;
#54804 = CARTESIAN_POINT('Ctrl Pts',(179.024024650514,534.283526679081,-47.9298769232956)) ;
#54805 = CARTESIAN_POINT('Ctrl Pts',(179.103078906543,534.23853538757,-47.9242612771831)) ;
#54806 = CARTESIAN_POINT('Ctrl Pts',(179.231051320197,534.178959242756,-47.9151685357388)) ;
#54807 = CARTESIAN_POINT('Ctrl Pts',(179.27763865699,534.15978937583,-47.9118603686894)) ;
#54808 = CARTESIAN_POINT('Ctrl Pts',(179.381121896328,534.1225948745,-47.9044721066949)) ;
#54809 = CARTESIAN_POINT('Ctrl Pts',(179.438260077722,534.105458380698,-47.9003667501405)) ;
#54810 = CARTESIAN_POINT('Ctrl Pts',(179.566900481831,534.074287106329,-47.8910524971581)) ;
#54811 = CARTESIAN_POINT('Ctrl Pts',(179.638652957529,534.061804830488,-47.8858082824234)) ;
#54812 = CARTESIAN_POINT('Ctrl Pts',(179.818048512989,534.042577439444,-47.8726917292847)) ;
#54813 = CARTESIAN_POINT('Ctrl Pts',(179.925980153421,534.04150818883,-47.8647871073748)) ;
#54814 = CARTESIAN_POINT('Ctrl Pts',(180.064207456186,534.053562677191,-47.8551317954482)) ;
#54815 = CARTESIAN_POINT('Ctrl Pts',(180.095071346719,534.057126031649,-47.8530085073833)) ;
#54816 = CARTESIAN_POINT('Ctrl Pts',(180.163990519883,534.06704360586,-47.8483618997925)) ;
#54817 = CARTESIAN_POINT('Ctrl Pts',(180.201959552842,534.073859952344,-47.845862099041)) ;
#54818 = CARTESIAN_POINT('Ctrl Pts',(180.290270657586,534.092900518838,-47.8401167796297)) ;
#54819 = CARTESIAN_POINT('Ctrl Pts',(180.340347455955,534.106166220435,-47.8369118277216)) ;
#54820 = CARTESIAN_POINT('Ctrl Pts',(180.521655255622,534.163360549852,-47.8252443631657)) ;
#54821 = CARTESIAN_POINT('Ctrl Pts',(180.647872931375,534.221241593517,-47.8169460691682)) ;
#54822 = CARTESIAN_POINT('Ctrl Pts',(180.809134566258,534.321078010433,-47.8047760670396)) ;
#54823 = CARTESIAN_POINT('Ctrl Pts',(180.851508281459,534.350102379805,-47.8014159854988)) ;
#54824 = CARTESIAN_POINT('Ctrl Pts',(180.938019581324,534.415428008747,-47.794154959863)) ;
#54825 = CARTESIAN_POINT('Ctrl Pts',(180.981764910245,534.452135800576,-47.7902400724785)) ;
#54826 = CARTESIAN_POINT('Ctrl Pts',(181.0725322574,534.536610784876,-47.7815491110741)) ;
#54827 = CARTESIAN_POINT('Ctrl Pts',(181.118730538064,534.585116370418,-47.7767480572676)) ;
#54828 = CARTESIAN_POINT('Ctrl Pts',(181.238930878224,534.72758825234,-47.7632241204118)) ;
#54829 = CARTESIAN_POINT('Ctrl Pts',(181.305934200094,534.826939569601,-47.7544008821308)) ;
#54830 = CARTESIAN_POINT('Ctrl Pts',(181.376393862534,534.960368147172,-47.7438801866571)) ;
#54831 = CARTESIAN_POINT('Ctrl Pts',(181.39026751837,534.988540619103,-47.7417297780651)) ;
#54832 = CARTESIAN_POINT('Ctrl Pts',(181.419293528156,535.051944717249,-47.7370674276954)) ;
#54833 = CARTESIAN_POINT('Ctrl Pts',(181.434042251425,535.087339462612,-47.7345768628677)) ;
#54834 = CARTESIAN_POINT('Ctrl Pts',(181.465561336422,535.171002010718,-47.7288768394179)) ;
#54835 = CARTESIAN_POINT('Ctrl Pts',(181.48135931127,535.219595024162,-47.7257060408905)) ;
#54836 = CARTESIAN_POINT('Ctrl Pts',(181.531985587087,535.403702080352,-47.7139540562249)) ;
#54837 = CARTESIAN_POINT('Ctrl Pts',(181.551937472757,535.542684100415,-47.7055471331473)) ;
#54838 = CARTESIAN_POINT('Ctrl Pts',(181.555161103611,535.734172452488,-47.6932298419796)) ;
#54839 = CARTESIAN_POINT('Ctrl Pts',(181.553627859236,535.785829342167,-47.6898413574438)) ;
#54840 = CARTESIAN_POINT('Ctrl Pts',(181.545222177744,535.895982631582,-47.6824263686904)) ;
#54841 = CARTESIAN_POINT('Ctrl Pts',(181.537643366721,535.954352460752,-47.6783814140527)) ;
#54842 = CARTESIAN_POINT('Ctrl Pts',(181.509825057427,536.105463556812,-47.6675847664843)) ;
#54843 = CARTESIAN_POINT('Ctrl Pts',(181.484724091722,536.197086192928,-47.6607031740783)) ;
#54844 = CARTESIAN_POINT('Ctrl Pts',(181.451971427951,536.286064488325,-47.6537940777375)) ;
#54845 = CARTESIAN_POINT('Origin',(179.888527625407,535.710565160536,-48.5221601717598)) ;
#54846 = CARTESIAN_POINT('',(181.45195607237,536.286106202709,-49.0537499395136)) ;
#54847 = CARTESIAN_POINT('',(181.451956083891,536.286106171415,-48.8631290382246)) ;
#54848 = CARTESIAN_POINT('',(181.451956083813,536.286106171625,-48.5221601717599)) ;
#54849 = CARTESIAN_POINT('',(181.555006899063,535.71162572618,-49.0928089386736)) ;
#54850 = CARTESIAN_POINT('Ctrl Pts',(181.55452730056,535.711605540458,-49.0925337921257)) ;
#54851 = CARTESIAN_POINT('Ctrl Pts',(181.554499745292,535.755730832439,-49.0893446356981)) ;
#54852 = CARTESIAN_POINT('Ctrl Pts',(181.552719153091,535.799840895829,-49.0861810648237)) ;
#54853 = CARTESIAN_POINT('Ctrl Pts',(181.546820044684,535.873351227504,-49.0809981568373)) ;
#54854 = CARTESIAN_POINT('Ctrl Pts',(181.543664179677,535.902805434826,-49.0789457219699)) ;
#54855 = CARTESIAN_POINT('Ctrl Pts',(181.535633050346,535.962648202419,-49.0748456738758)) ;
#54856 = CARTESIAN_POINT('Ctrl Pts',(181.530698975711,535.993010761211,-49.0728064240962)) ;
#54857 = CARTESIAN_POINT('Ctrl Pts',(181.507825788572,536.112724184301,-49.0648825240018)) ;
#54858 = CARTESIAN_POINT('Ctrl Pts',(181.483416661406,536.200645086575,-49.0593063227425)) ;
#54859 = CARTESIAN_POINT('Ctrl Pts',(181.451956072328,536.286106202824,-49.0537499415271)) ;
#54860 = CARTESIAN_POINT('',(178.619456745555,536.789923813584,-49.5221601717597)) ;
#54861 = CARTESIAN_POINT('Ctrl Pts',(181.555006899063,535.71162572618,-49.0928089386736)) ;
#54862 = CARTESIAN_POINT('Ctrl Pts',(181.554911677155,535.651761101128,-49.0970575997108)) ;
#54863 = CARTESIAN_POINT('Ctrl Pts',(181.551563926785,535.591796400194,-49.1013454409477)) ;
#54864 = CARTESIAN_POINT('Ctrl Pts',(181.544988530129,535.53210893011,-49.1056125097224)) ;
#54865 = CARTESIAN_POINT('Ctrl Pts',(181.538420248955,535.472486050069,-49.1098749609425)) ;
#54866 = CARTESIAN_POINT('Ctrl Pts',(181.528631540799,535.413139765124,-49.1141164261649)) ;
#54867 = CARTESIAN_POINT('Ctrl Pts',(181.51568414664,535.354437590846,-49.1182974440124)) ;
#54868 = CARTESIAN_POINT('Ctrl Pts',(181.502745687373,535.295775926463,-49.1224755765735)) ;
#54869 = CARTESIAN_POINT('Ctrl Pts',(181.486652970128,535.237757503309,-49.1265932469502)) ;
#54870 = CARTESIAN_POINT('Ctrl Pts',(181.467502284901,535.180740681,-49.1306339744544)) ;
#54871 = CARTESIAN_POINT('Ctrl Pts',(181.44835724259,535.123740659193,-49.134673511323)) ;
#54872 = CARTESIAN_POINT('Ctrl Pts',(181.426155991489,535.067741741072,-49.1386361730387)) ;
#54873 = CARTESIAN_POINT('Ctrl Pts',(181.401029239235,535.013092736096,-49.1425289370527)) ;
#54874 = CARTESIAN_POINT('Ctrl Pts',(181.375882194113,534.958399595491,-49.1464248449407)) ;
#54875 = CARTESIAN_POINT('Ctrl Pts',(181.347804781064,534.905058723015,-49.1502508800457)) ;
#54876 = CARTESIAN_POINT('Ctrl Pts',(181.316963969973,534.853408532587,-49.1540363410482)) ;
#54877 = CARTESIAN_POINT('Ctrl Pts',(181.286111640662,534.801739052193,-49.1578232158193)) ;
#54878 = CARTESIAN_POINT('Ctrl Pts',(181.252493625534,534.751761799062,-49.1615697761749)) ;
#54879 = CARTESIAN_POINT('Ctrl Pts',(181.216315764961,534.703800951296,-49.1653244954319)) ;
#54880 = CARTESIAN_POINT('Ctrl Pts',(181.180070812056,534.655751159489,-49.1690861778665)) ;
#54881 = CARTESIAN_POINT('Ctrl Pts',(181.141256221114,534.609725731287,-49.1728565400046)) ;
#54882 = CARTESIAN_POINT('Ctrl Pts',(181.100121726458,534.566030406421,-49.1766977336409)) ;
#54883 = CARTESIAN_POINT('Ctrl Pts',(181.064119275007,534.52778662039,-49.1800596902799)) ;
#54884 = CARTESIAN_POINT('Ctrl Pts',(181.026340236735,534.491327817788,-49.1834764342659)) ;
#54885 = CARTESIAN_POINT('Ctrl Pts',(180.986981295376,534.456840870487,-49.1869925547289)) ;
#54886 = CARTESIAN_POINT('Ctrl Pts',(180.986956119852,534.456818811282,-49.1869948037776)) ;
#54887 = CARTESIAN_POINT('Ctrl Pts',(180.986930943682,534.456796752882,-49.1869970528668)) ;
#54888 = CARTESIAN_POINT('Ctrl Pts',(180.986905766866,534.456774695288,-49.1869993019968)) ;
#54889 = CARTESIAN_POINT('Ctrl Pts',(180.945132179332,534.420176547417,-49.1907310774929)) ;
#54890 = CARTESIAN_POINT('Ctrl Pts',(180.901410943968,534.385660145286,-49.19458524967)) ;
#54891 = CARTESIAN_POINT('Ctrl Pts',(180.855991998272,534.353408352203,-49.1984983448031)) ;
#54892 = CARTESIAN_POINT('Ctrl Pts',(180.851861958098,534.350475628885,-49.1988541707664)) ;
#54893 = CARTESIAN_POINT('Ctrl Pts',(180.847717915726,534.347561632462,-49.1992104839429)) ;
#54894 = CARTESIAN_POINT('Ctrl Pts',(180.843560080384,534.344666500875,-49.1995672366075)) ;
#54895 = CARTESIAN_POINT('Ctrl Pts',(180.79306380925,534.309505572763,-49.2038999428835)) ;
#54896 = CARTESIAN_POINT('Ctrl Pts',(180.74052717115,534.277126471809,-49.208296810223)) ;
#54897 = CARTESIAN_POINT('Ctrl Pts',(180.686304652853,534.247729623411,-49.2126868180687)) ;
#54898 = CARTESIAN_POINT('Ctrl Pts',(180.632884822058,534.218767953672,-49.2170118380729)) ;
#54899 = CARTESIAN_POINT('Ctrl Pts',(180.577828776666,534.192700466876,-49.2213299209602)) ;
#54900 = CARTESIAN_POINT('Ctrl Pts',(180.521486588017,534.169681434335,-49.2255939033608)) ;
#54901 = CARTESIAN_POINT('Ctrl Pts',(180.465177121547,534.14667577069,-49.2298554093435)) ;
#54902 = CARTESIAN_POINT('Ctrl Pts',(180.407583023497,534.126714896719,-49.2340627463742)) ;
#54903 = CARTESIAN_POINT('Ctrl Pts',(180.349064032254,534.109919118014,-49.2381927563816)) ;
#54904 = CARTESIAN_POINT('Ctrl Pts',(180.290557187574,534.093126825545,-49.2423219091387)) ;
#54905 = CARTESIAN_POINT('Ctrl Pts',(180.231125843687,534.079498352383,-49.2463737672092)) ;
#54906 = CARTESIAN_POINT('Ctrl Pts',(180.171139611766,534.069120844121,-49.2503500571725)) ;
#54907 = CARTESIAN_POINT('Ctrl Pts',(180.109506899204,534.058458497724,-49.2544354869207)) ;
#54908 = CARTESIAN_POINT('Ctrl Pts',(180.047288395297,534.051228390706,-49.2584411569732)) ;
#54909 = CARTESIAN_POINT('Ctrl Pts',(179.984895840698,534.047486877455,-49.2623953014158)) ;
#54910 = CARTESIAN_POINT('Ctrl Pts',(179.924086832196,534.043840325193,-49.2662490882108)) ;
#54911 = CARTESIAN_POINT('Ctrl Pts',(179.863112594942,534.043507696091,-49.2700543024794)) ;
#54912 = CARTESIAN_POINT('Ctrl Pts',(179.802363804755,534.046501995282,-49.2738585782267)) ;
#54913 = CARTESIAN_POINT('Ctrl Pts',(179.739242047665,534.049613257672,-49.2778114564466)) ;
#54914 = CARTESIAN_POINT('Ctrl Pts',(179.676363826613,534.056317323824,-49.2817637502975)) ;
#54915 = CARTESIAN_POINT('Ctrl Pts',(179.614176335598,534.066577433623,-49.2857867681017)) ;
#54916 = CARTESIAN_POINT('Ctrl Pts',(179.560500029662,534.075433310964,-49.2892591824236)) ;
#54917 = CARTESIAN_POINT('Ctrl Pts',(179.507337342244,534.086938441788,-49.2927849490772)) ;
#54918 = CARTESIAN_POINT('Ctrl Pts',(179.45498218312,534.101030596804,-49.2964146836658)) ;
#54919 = CARTESIAN_POINT('Ctrl Pts',(179.446714668846,534.103255918906,-49.2969878627569)) ;
#54920 = CARTESIAN_POINT('Ctrl Pts',(179.438467194578,534.105545708956,-49.2975636344171)) ;
#54921 = CARTESIAN_POINT('Ctrl Pts',(179.430240807281,534.107899676818,-49.2981421979574)) ;
#54922 = CARTESIAN_POINT('Ctrl Pts',(179.430206794206,534.107909409606,-49.2981445901041)) ;
#54923 = CARTESIAN_POINT('Ctrl Pts',(179.430172781491,534.107919143492,-49.2981469822985)) ;
#54924 = CARTESIAN_POINT('Ctrl Pts',(179.430138769138,534.107928878474,-49.2981493745406)) ;
#54925 = CARTESIAN_POINT('Ctrl Pts',(179.377278132391,534.123058597679,-49.301867301362)) ;
#54926 = CARTESIAN_POINT('Ctrl Pts',(179.325092149455,534.140903220938,-49.3057108146284)) ;
#54927 = CARTESIAN_POINT('Ctrl Pts',(179.273863720226,534.161355891207,-49.3096171059527)) ;
#54928 = CARTESIAN_POINT('Ctrl Pts',(179.26886579857,534.163351284101,-49.3099982095371)) ;
#54929 = CARTESIAN_POINT('Ctrl Pts',(179.263877014189,534.165371467186,-49.3103799106584)) ;
#54930 = CARTESIAN_POINT('Ctrl Pts',(179.258897644146,534.16741631899,-49.3107621509917)) ;
#54931 = CARTESIAN_POINT('Ctrl Pts',(179.201982702947,534.19078927966,-49.3151312149316)) ;
#54932 = CARTESIAN_POINT('Ctrl Pts',(179.14629396211,534.217390025738,-49.3195700299251)) ;
#54933 = CARTESIAN_POINT('Ctrl Pts',(179.092194440457,534.247029178958,-49.3240053059955)) ;
#54934 = CARTESIAN_POINT('Ctrl Pts',(179.039099660485,534.276117870886,-49.3283582096791)) ;
#54935 = CARTESIAN_POINT('Ctrl Pts',(178.987535306352,534.308132790928,-49.3327074203407)) ;
#54936 = CARTESIAN_POINT('Ctrl Pts',(178.937818914218,534.342865013661,-49.337003889208)) ;
#54937 = CARTESIAN_POINT('Ctrl Pts',(178.888134053237,534.377575208508,-49.3412976331668)) ;
#54938 = CARTESIAN_POINT('Ctrl Pts',(178.840294714745,534.4149991662,-49.3455385594482)) ;
#54939 = CARTESIAN_POINT('Ctrl Pts',(178.794594921043,534.454901386224,-49.3497012824977)) ;
#54940 = CARTESIAN_POINT('Ctrl Pts',(178.748906743163,534.494793464034,-49.3538629474801)) ;
#54941 = CARTESIAN_POINT('Ctrl Pts',(178.705357057807,534.537162543635,-49.3579464383719)) ;
#54942 = CARTESIAN_POINT('Ctrl Pts',(178.664217195255,534.581746995344,-49.3619510689569)) ;
#54943 = CARTESIAN_POINT('Ctrl Pts',(178.621661478401,534.627865849061,-49.3660935214277)) ;
#54944 = CARTESIAN_POINT('Ctrl Pts',(178.581684632514,534.676355421234,-49.3701515615004)) ;
#54945 = CARTESIAN_POINT('Ctrl Pts',(178.544560053224,534.726895975379,-49.374151411281)) ;
#54946 = CARTESIAN_POINT('Ctrl Pts',(178.508623895755,534.775818639206,-49.3780232189706)) ;
#54947 = CARTESIAN_POINT('Ctrl Pts',(178.475360465389,534.826663033093,-49.3818408818493)) ;
#54948 = CARTESIAN_POINT('Ctrl Pts',(178.444989908625,534.879110450356,-49.3856499837092)) ;
#54949 = CARTESIAN_POINT('Ctrl Pts',(178.413112803794,534.934159550416,-49.3896480381486)) ;
#54950 = CARTESIAN_POINT('Ctrl Pts',(178.384423573488,534.990975074804,-49.3936370368329)) ;
#54951 = CARTESIAN_POINT('Ctrl Pts',(178.359137434927,535.049152880559,-49.3976888784728)) ;
#54952 = CARTESIAN_POINT('Ctrl Pts',(178.337337879878,535.099308829681,-49.4011820312397)) ;
#54953 = CARTESIAN_POINT('Ctrl Pts',(178.318067108084,535.15047813457,-49.4047225540605)) ;
#54954 = CARTESIAN_POINT('Ctrl Pts',(178.301433344379,535.202375297453,-49.4083622296786)) ;
#54955 = CARTESIAN_POINT('Ctrl Pts',(178.298778613439,535.210658029279,-49.4089431180239)) ;
#54956 = CARTESIAN_POINT('Ctrl Pts',(178.296190962998,535.218959362182,-49.4095265319714)) ;
#54957 = CARTESIAN_POINT('Ctrl Pts',(178.293670733555,535.22727820833,-49.4101126820322)) ;
#54958 = CARTESIAN_POINT('Ctrl Pts',(178.293665374797,535.227295896675,-49.4101139283618)) ;
#54959 = CARTESIAN_POINT('Ctrl Pts',(178.293660016343,535.227313585099,-49.4101151747038)) ;
#54960 = CARTESIAN_POINT('Ctrl Pts',(178.293654658194,535.227331273602,-49.4101164210582)) ;
#54961 = CARTESIAN_POINT('Ctrl Pts',(178.277359028103,535.281126961539,-49.413906933453)) ;
#54962 = CARTESIAN_POINT('Ctrl Pts',(178.263833292121,535.335845914037,-49.4178217665055)) ;
#54963 = CARTESIAN_POINT('Ctrl Pts',(178.253139902238,535.391180638803,-49.4217985618384)) ;
#54964 = CARTESIAN_POINT('Ctrl Pts',(178.25206581324,535.396738690994,-49.4221980078663)) ;
#54965 = CARTESIAN_POINT('Ctrl Pts',(178.251020283373,535.402302915627,-49.422598079034)) ;
#54966 = CARTESIAN_POINT('Ctrl Pts',(178.2500033642,535.407872974596,-49.4229987121484)) ;
#54967 = CARTESIAN_POINT('Ctrl Pts',(178.238885809053,535.468768116883,-49.4273786676646)) ;
#54968 = CARTESIAN_POINT('Ctrl Pts',(178.231189624062,535.530366317671,-49.4318251526027)) ;
#54969 = CARTESIAN_POINT('Ctrl Pts',(178.226949968159,535.592263397604,-49.4362689905779)) ;
#54970 = CARTESIAN_POINT('Ctrl Pts',(178.222715557955,535.65408389268,-49.4407073302212)) ;
#54971 = CARTESIAN_POINT('Ctrl Pts',(178.221928761452,535.716202624384,-49.4451426894742)) ;
#54972 = CARTESIAN_POINT('Ctrl Pts',(178.224586279133,535.77822250377,-49.4495267355503)) ;
#54973 = CARTESIAN_POINT('Ctrl Pts',(178.227241344843,535.840185160232,-49.4539067366662)) ;
#54974 = CARTESIAN_POINT('Ctrl Pts',(178.233334251276,535.902049229793,-49.4582353830793)) ;
#54975 = CARTESIAN_POINT('Ctrl Pts',(178.2428269984,535.963422870731,-49.4624885269454)) ;
#54976 = CARTESIAN_POINT('Ctrl Pts',(178.252313971153,536.024759178508,-49.4667390836535)) ;
#54977 = CARTESIAN_POINT('Ctrl Pts',(178.265196703797,536.085605670115,-49.4709142368251)) ;
#54978 = CARTESIAN_POINT('Ctrl Pts',(178.281403022177,536.145574600527,-49.4750148474439)) ;
#54979 = CARTESIAN_POINT('Ctrl Pts',(178.297610879212,536.20554922449,-49.4791158473816)) ;
#54980 = CARTESIAN_POINT('Ctrl Pts',(178.31714314831,536.264646053285,-49.4831424249934)) ;
#54981 = CARTESIAN_POINT('Ctrl Pts',(178.339891482358,536.322480985118,-49.4871193692917)) ;
#54982 = CARTESIAN_POINT('Ctrl Pts',(178.362639011737,536.380313871178,-49.4910961729149)) ;
#54983 = CARTESIAN_POINT('Ctrl Pts',(178.388602702046,536.436884766255,-49.4950236392707)) ;
#54984 = CARTESIAN_POINT('Ctrl Pts',(178.417634175849,536.491815189789,-49.4989473205462)) ;
#54985 = CARTESIAN_POINT('Ctrl Pts',(178.446694689467,536.546800559527,-49.5028749266301)) ;
#54986 = CARTESIAN_POINT('Ctrl Pts',(178.478829564945,536.600141789156,-49.5067992441383)) ;
#54987 = CARTESIAN_POINT('Ctrl Pts',(178.513844080861,536.651469010558,-49.5107808564248)) ;
#54988 = CARTESIAN_POINT('Ctrl Pts',(178.546595900434,536.699479381415,-49.514505170293)) ;
#54989 = CARTESIAN_POINT('Ctrl Pts',(178.581867072349,536.745727234891,-49.5182802680799)) ;
#54990 = CARTESIAN_POINT('Ctrl Pts',(178.619456745554,536.789923813584,-49.5221601717597)) ;
#54991 = CARTESIAN_POINT('',(181.142801535895,536.808437501682,-49.5221525827187)) ;
#54992 = CARTESIAN_POINT('Origin',(179.888527625407,535.710565160536,-49.5221601717598)) ;
#54993 = CARTESIAN_POINT('',(181.55405613246,535.711433585225,-48.8998644770965)) ;
#54994 = CARTESIAN_POINT('Ctrl Pts',(181.142801548039,536.808437512311,-49.5221525825813)) ;
#54995 = CARTESIAN_POINT('Ctrl Pts',(181.108069436076,536.848071008662,-49.5185546904077)) ;
#54996 = CARTESIAN_POINT('Ctrl Pts',(181.071355132789,536.886086906054,-49.5148601919674)) ;
#54997 = CARTESIAN_POINT('Ctrl Pts',(181.032850332806,536.92229732986,-49.5111228902725)) ;
#54998 = CARTESIAN_POINT('Ctrl Pts',(180.988797636745,536.963725068605,-49.5068471060657)) ;
#54999 = CARTESIAN_POINT('Ctrl Pts',(180.942400305294,537.002790369321,-49.5025158569213)) ;
#55000 = CARTESIAN_POINT('Ctrl Pts',(180.893961692549,537.039252837364,-49.4981952822219)) ;
#55001 = CARTESIAN_POINT('Ctrl Pts',(180.845572449992,537.075678141689,-49.4938791111909)) ;
#55002 = CARTESIAN_POINT('Ctrl Pts',(180.795146217323,537.10950619834,-49.48957389081)) ;
#55003 = CARTESIAN_POINT('Ctrl Pts',(180.743002516597,537.140531585784,-49.4853247936267)) ;
#55004 = CARTESIAN_POINT('Ctrl Pts',(180.690892178933,537.171537122278,-49.4810784151399)) ;
#55005 = CARTESIAN_POINT('Ctrl Pts',(180.637066609147,537.199743670267,-49.4768882061335)) ;
#55006 = CARTESIAN_POINT('Ctrl Pts',(180.581860613547,537.22497761557,-49.4727754537126)) ;
#55007 = CARTESIAN_POINT('Ctrl Pts',(180.526668996164,537.250204988777,-49.4686637724443)) ;
#55008 = CARTESIAN_POINT('Ctrl Pts',(180.470097682587,537.272461250094,-49.4646294978784)) ;
#55009 = CARTESIAN_POINT('Ctrl Pts',(180.412496775638,537.291604078887,-49.4606693209704)) ;
#55010 = CARTESIAN_POINT('Ctrl Pts',(180.354847343587,537.310763034296,-49.4567058078651)) ;
#55011 = CARTESIAN_POINT('Ctrl Pts',(180.296166583948,537.326803113922,-49.4528163932275)) ;
#55012 = CARTESIAN_POINT('Ctrl Pts',(180.236820997839,537.339614758446,-49.4489741210126)) ;
#55013 = CARTESIAN_POINT('Ctrl Pts',(180.177453116158,537.352431216184,-49.4451304052926)) ;
#55014 = CARTESIAN_POINT('Ctrl Pts',(180.11741992538,537.362016473207,-49.4413335941278)) ;
#55015 = CARTESIAN_POINT('Ctrl Pts',(180.057103754115,537.36829795894,-49.4375359960147)) ;
#55016 = CARTESIAN_POINT('Ctrl Pts',(179.996673041641,537.374591373298,-49.4337311862122)) ;
#55017 = CARTESIAN_POINT('Ctrl Pts',(179.935958371058,537.377567925487,-49.4299251123059)) ;
#55018 = CARTESIAN_POINT('Ctrl Pts',(179.875358970622,537.377198402245,-49.4260545749207)) ;
#55019 = CARTESIAN_POINT('Ctrl Pts',(179.820907754908,537.376866369425,-49.4225767275398)) ;
#55020 = CARTESIAN_POINT('Ctrl Pts',(179.76654921578,537.373832827106,-49.4190462440258)) ;
#55021 = CARTESIAN_POINT('Ctrl Pts',(179.712583297119,537.368113257836,-49.4154127829198)) ;
#55022 = CARTESIAN_POINT('Ctrl Pts',(179.707775847752,537.367603741083,-49.4150891030728)) ;
#55023 = CARTESIAN_POINT('Ctrl Pts',(179.702971485346,537.367072927124,-49.414764606017)) ;
#55024 = CARTESIAN_POINT('Ctrl Pts',(179.69817040477,537.366520837422,-49.4144392561638)) ;
#55025 = CARTESIAN_POINT('Ctrl Pts',(179.698137064797,537.366517003565,-49.4144369968484)) ;
#55026 = CARTESIAN_POINT('Ctrl Pts',(179.698103724982,537.366513168683,-49.4144347374918)) ;
#55027 = CARTESIAN_POINT('Ctrl Pts',(179.698070385326,537.366509332774,-49.4144324780942)) ;
#55028 = CARTESIAN_POINT('Ctrl Pts',(179.642901235647,537.360161822149,-49.4106937158674)) ;
#55029 = CARTESIAN_POINT('Ctrl Pts',(179.587966985924,537.350973719898,-49.4068324308234)) ;
#55030 = CARTESIAN_POINT('Ctrl Pts',(179.533570215717,537.339007287281,-49.4029116847749)) ;
#55031 = CARTESIAN_POINT('Ctrl Pts',(179.528503948941,537.337892788392,-49.4025465243919)) ;
#55032 = CARTESIAN_POINT('Ctrl Pts',(179.52344237049,537.336754216371,-49.4021808482317)) ;
#55033 = CARTESIAN_POINT('Ctrl Pts',(179.51838574044,537.335591638312,-49.4018147072405)) ;
#55034 = CARTESIAN_POINT('Ctrl Pts',(179.458436330543,537.32180857174,-49.3974738841729)) ;
#55035 = CARTESIAN_POINT('Ctrl Pts',(179.399177962373,537.304647354077,-49.3930683863622)) ;
#55036 = CARTESIAN_POINT('Ctrl Pts',(179.340996033269,537.284235756859,-49.3886690376785)) ;
#55037 = CARTESIAN_POINT('Ctrl Pts',(179.283553092056,537.264083414077,-49.3843255665749)) ;
#55038 = CARTESIAN_POINT('Ctrl Pts',(179.227159187739,537.240763104393,-49.3799883815136)) ;
#55039 = CARTESIAN_POINT('Ctrl Pts',(179.172164866101,537.214431142677,-49.3757050966475)) ;
#55040 = CARTESIAN_POINT('Ctrl Pts',(179.117203845471,537.188115125897,-49.3714244054619)) ;
#55041 = CARTESIAN_POINT('Ctrl Pts',(179.063640628265,537.158791202608,-49.3671976842975)) ;
#55042 = CARTESIAN_POINT('Ctrl Pts',(179.011806997811,537.126645653541,-49.3630486490804)) ;
#55043 = CARTESIAN_POINT('Ctrl Pts',(178.959985625649,537.094507706672,-49.3589005950812)) ;
#55044 = CARTESIAN_POINT('Ctrl Pts',(178.909893053504,537.059549450668,-49.3548301922803)) ;
#55045 = CARTESIAN_POINT('Ctrl Pts',(178.86184309899,537.021986722675,-49.3508363377649)) ;
#55046 = CARTESIAN_POINT('Ctrl Pts',(178.81265258268,536.983532368187,-49.3467476811228)) ;
#55047 = CARTESIAN_POINT('Ctrl Pts',(178.765603040442,536.942348190254,-49.3427392229935)) ;
#55048 = CARTESIAN_POINT('Ctrl Pts',(178.721010496985,536.898699000879,-49.3387837906119)) ;
#55049 = CARTESIAN_POINT('Ctrl Pts',(178.67739648949,536.856007646564,-49.3349151559892)) ;
#55050 = CARTESIAN_POINT('Ctrl Pts',(178.636133031795,536.810958220954,-49.3310968917719)) ;
#55051 = CARTESIAN_POINT('Ctrl Pts',(178.597493283621,536.763831739696,-49.3272821279936)) ;
#55052 = CARTESIAN_POINT('Ctrl Pts',(178.557553137294,536.715119244241,-49.3233389805688)) ;
#55053 = CARTESIAN_POINT('Ctrl Pts',(178.52041697272,536.664187083124,-49.3193991427361)) ;
#55054 = CARTESIAN_POINT('Ctrl Pts',(178.486355144813,536.611385916437,-49.315393240636)) ;
#55055 = CARTESIAN_POINT('Ctrl Pts',(178.456716512441,536.565441395415,-49.3119075363459)) ;
#55056 = CARTESIAN_POINT('Ctrl Pts',(178.429405010976,536.518081083629,-49.3083711621868)) ;
#55057 = CARTESIAN_POINT('Ctrl Pts',(178.404574279484,536.469566591476,-49.3047334976926)) ;
#55058 = CARTESIAN_POINT('Ctrl Pts',(178.40088276031,536.462354070246,-49.3041926957337)) ;
#55059 = CARTESIAN_POINT('Ctrl Pts',(178.39724598531,536.455116000895,-49.3036496550576)) ;
#55060 = CARTESIAN_POINT('Ctrl Pts',(178.393664370397,536.447853200198,-49.3031042093333)) ;
#55061 = CARTESIAN_POINT('Ctrl Pts',(178.393650634657,536.447825346857,-49.3031021175115)) ;
#55062 = CARTESIAN_POINT('Ctrl Pts',(178.393636899729,536.447797493154,-49.3031000256542)) ;
#55063 = CARTESIAN_POINT('Ctrl Pts',(178.393623165612,536.447769639086,-49.3030979337616)) ;
#55064 = CARTESIAN_POINT('Ctrl Pts',(178.369107074875,536.398048725274,-49.2993638000577)) ;
#55065 = CARTESIAN_POINT('Ctrl Pts',(178.347095644288,536.346987147412,-49.295507131558)) ;
#55066 = CARTESIAN_POINT('Ctrl Pts',(178.327700935934,536.294871854987,-49.2915911460869)) ;
#55067 = CARTESIAN_POINT('Ctrl Pts',(178.325902770388,536.290040025524,-49.2912280784902)) ;
#55068 = CARTESIAN_POINT('Ctrl Pts',(178.324127089886,536.28519917451,-49.2908645010089)) ;
#55069 = CARTESIAN_POINT('Ctrl Pts',(178.322373978227,536.280349552575,-49.2905004640256)) ;
#55070 = CARTESIAN_POINT('Ctrl Pts',(178.301455345353,536.222482467893,-49.2861566699679)) ;
#55071 = CARTESIAN_POINT('Ctrl Pts',(178.283750973025,536.163360640214,-49.2817481185811)) ;
#55072 = CARTESIAN_POINT('Ctrl Pts',(178.269363526799,536.103378216542,-49.2773461889775)) ;
#55073 = CARTESIAN_POINT('Ctrl Pts',(178.255192293743,536.044297203013,-49.2730104111523)) ;
#55074 = CARTESIAN_POINT('Ctrl Pts',(178.244238596283,535.984381273989,-49.26868134018)) ;
#55075 = CARTESIAN_POINT('Ctrl Pts',(178.236561503253,535.924008234376,-49.2644066324919)) ;
#55076 = CARTESIAN_POINT('Ctrl Pts',(178.228889180239,535.863672706402,-49.260134580812)) ;
#55077 = CARTESIAN_POINT('Ctrl Pts',(178.224489264639,535.802880622491,-49.2559169588637)) ;
#55078 = CARTESIAN_POINT('Ctrl Pts',(178.223385478994,535.742010380143,-49.2517775636806)) ;
#55079 = CARTESIAN_POINT('Ctrl Pts',(178.222281967414,535.681155251669,-49.2476391962954)) ;
#55080 = CARTESIAN_POINT('Ctrl Pts',(178.224472981386,535.620222024777,-49.2435790189435)) ;
#55081 = CARTESIAN_POINT('Ctrl Pts',(178.22994765229,535.559590072891,-49.2395960575722)) ;
#55082 = CARTESIAN_POINT('Ctrl Pts',(178.235575430961,535.497262453281,-49.235501706433)) ;
#55083 = CARTESIAN_POINT('Ctrl Pts',(178.244673457541,535.435253267959,-49.2314889419518)) ;
#55084 = CARTESIAN_POINT('Ctrl Pts',(178.257190212385,535.3739752658,-49.2275303827539)) ;
#55085 = CARTESIAN_POINT('Ctrl Pts',(178.269381906449,535.314288656574,-49.2236746275461)) ;
#55086 = CARTESIAN_POINT('Ctrl Pts',(178.284817191276,535.25529588635,-49.2198699305122)) ;
#55087 = CARTESIAN_POINT('Ctrl Pts',(178.303408255902,535.197377418763,-49.216069516945)) ;
#55088 = CARTESIAN_POINT('Ctrl Pts',(178.322742846318,535.137142576336,-49.2121171107105)) ;
#55089 = CARTESIAN_POINT('Ctrl Pts',(178.345491509524,535.078070043124,-49.2081689190033)) ;
#55090 = CARTESIAN_POINT('Ctrl Pts',(178.371503615203,535.020583097395,-49.2041543295508)) ;
#55091 = CARTESIAN_POINT('Ctrl Pts',(178.394005286313,534.970854238001,-49.2006815245187)) ;
#55092 = CARTESIAN_POINT('Ctrl Pts',(178.418949248333,534.9223109549,-49.1971583753286)) ;
#55093 = CARTESIAN_POINT('Ctrl Pts',(178.446198877628,534.875223282812,-49.1935342109913)) ;
#55094 = CARTESIAN_POINT('Ctrl Pts',(178.450435005529,534.867903205194,-49.1929708116328)) ;
#55095 = CARTESIAN_POINT('Ctrl Pts',(178.454726838208,534.860618203501,-49.192404971074)) ;
#55096 = CARTESIAN_POINT('Ctrl Pts',(178.459073848331,534.853369179574,-49.1918364989507)) ;
#55097 = CARTESIAN_POINT('Ctrl Pts',(178.459089266447,534.853343468501,-49.1918344826754)) ;
#55098 = CARTESIAN_POINT('Ctrl Pts',(178.459104685258,534.853317757881,-49.1918324663669)) ;
#55099 = CARTESIAN_POINT('Ctrl Pts',(178.459120104762,534.853292047713,-49.1918304500253)) ;
#55100 = CARTESIAN_POINT('Ctrl Pts',(178.487630711552,534.805754042735,-49.1881022419431)) ;
#55101 = CARTESIAN_POINT('Ctrl Pts',(178.518624376016,534.759596052204,-49.184250960234)) ;
#55102 = CARTESIAN_POINT('Ctrl Pts',(178.551920446847,534.715067415536,-49.1803397465476)) ;
#55103 = CARTESIAN_POINT('Ctrl Pts',(178.555033589349,534.710904041663,-49.1799740527808)) ;
#55104 = CARTESIAN_POINT('Ctrl Pts',(178.558166824182,534.706754924506,-49.1796078350872)) ;
#55105 = CARTESIAN_POINT('Ctrl Pts',(178.561319981677,534.702620275257,-49.1792411450768)) ;
#55106 = CARTESIAN_POINT('Ctrl Pts',(178.598632802673,534.653692992815,-49.1749019267721)) ;
#55107 = CARTESIAN_POINT('Ctrl Pts',(178.638740920888,534.606789228571,-49.1704972367949)) ;
#55108 = CARTESIAN_POINT('Ctrl Pts',(178.68136841272,534.562208404265,-49.1660984705568)) ;
#55109 = CARTESIAN_POINT('Ctrl Pts',(178.723381799334,534.518269825508,-49.1617630743457)) ;
#55110 = CARTESIAN_POINT('Ctrl Pts',(178.767842244335,534.476587367754,-49.1574337193977)) ;
#55111 = CARTESIAN_POINT('Ctrl Pts',(178.814463529465,534.437415399226,-49.153158224334)) ;
#55112 = CARTESIAN_POINT('Ctrl Pts',(178.861056184788,534.39826748593,-49.148885354822)) ;
#55113 = CARTESIAN_POINT('Ctrl Pts',(178.909806969818,534.361626862826,-49.1446664143369)) ;
#55114 = CARTESIAN_POINT('Ctrl Pts',(178.960410091427,534.327718441226,-49.1405253465973)) ;
#55115 = CARTESIAN_POINT('Ctrl Pts',(179.011000954244,534.293818234066,-49.1363852820466)) ;
#55116 = CARTESIAN_POINT('Ctrl Pts',(179.063443256845,534.262648941234,-49.1323230552208)) ;
#55117 = CARTESIAN_POINT('Ctrl Pts',(179.117411709091,534.234406897251,-49.1283378089247)) ;
#55118 = CARTESIAN_POINT('Ctrl Pts',(179.172827935434,534.205407223615,-49.1242456532007)) ;
#55119 = CARTESIAN_POINT('Ctrl Pts',(179.229853421087,534.179494290947,-49.1202346507528)) ;
#55120 = CARTESIAN_POINT('Ctrl Pts',(179.288114071575,534.15684775281,-49.1162776121979)) ;
#55121 = CARTESIAN_POINT('Ctrl Pts',(179.344925102912,534.134764697144,-49.1124190311579)) ;
#55122 = CARTESIAN_POINT('Ctrl Pts',(179.402910553671,534.115787699122,-49.1086113983487)) ;
#55123 = CARTESIAN_POINT('Ctrl Pts',(179.461702632577,534.100049052582,-49.1048080018268)) ;
#55124 = CARTESIAN_POINT('Ctrl Pts',(179.522744964334,534.083708013086,-49.1008590312068)) ;
#55125 = CARTESIAN_POINT('Ctrl Pts',(179.58465699248,534.070858830823,-49.0969142071573)) ;
#55126 = CARTESIAN_POINT('Ctrl Pts',(179.647003052361,534.06160374531,-49.092903296481)) ;
#55127 = CARTESIAN_POINT('Ctrl Pts',(179.701041313284,534.053581927623,-49.0894268516491)) ;
#55128 = CARTESIAN_POINT('Ctrl Pts',(179.755406537252,534.048259891954,-49.0859001036798)) ;
#55129 = CARTESIAN_POINT('Ctrl Pts',(179.809797218069,534.04566919133,-49.0822723152298)) ;
#55130 = CARTESIAN_POINT('Ctrl Pts',(179.818129605256,534.045272308622,-49.081716555722)) ;
#55131 = CARTESIAN_POINT('Ctrl Pts',(179.826462664638,534.044939461026,-49.0811584249208)) ;
#55132 = CARTESIAN_POINT('Ctrl Pts',(179.834795395502,534.04467069258,-49.0805977404102)) ;
#55133 = CARTESIAN_POINT('Ctrl Pts',(179.834824989246,534.044669738047,-49.0805957491358)) ;
#55134 = CARTESIAN_POINT('Ctrl Pts',(179.834854582986,534.044668784323,-49.0805937578292)) ;
#55135 = CARTESIAN_POINT('Ctrl Pts',(179.834884176722,534.044667831406,-49.0805917664903)) ;
#55136 = CARTESIAN_POINT('Ctrl Pts',(179.89031453931,534.042882977362,-49.0768619016354)) ;
#55137 = CARTESIAN_POINT('Ctrl Pts',(179.945929545374,534.043935471606,-49.0730091891776)) ;
#55138 = CARTESIAN_POINT('Ctrl Pts',(180.001421418037,534.047808397575,-49.0690967767647)) ;
#55139 = CARTESIAN_POINT('Ctrl Pts',(180.00659353029,534.0481693731,-49.0687321209113)) ;
#55140 = CARTESIAN_POINT('Ctrl Pts',(180.011764543074,534.048554827526,-49.0683669464357)) ;
#55141 = CARTESIAN_POINT('Ctrl Pts',(180.016934189219,534.048964732805,-49.0680013044676)) ;
#55142 = CARTESIAN_POINT('Ctrl Pts',(180.078270911918,534.053828169436,-49.0636630423553)) ;
#55143 = CARTESIAN_POINT('Ctrl Pts',(180.139420276285,534.062136921654,-49.0592596355204)) ;
#55144 = CARTESIAN_POINT('Ctrl Pts',(180.199981318123,534.073821174808,-49.0548623452926)) ;
#55145 = CARTESIAN_POINT('Ctrl Pts',(180.259684867654,534.085339988979,-49.0505273169154)) ;
#55146 = CARTESIAN_POINT('Ctrl Pts',(180.31881681372,534.100138984745,-49.0461985203468)) ;
#55147 = CARTESIAN_POINT('Ctrl Pts',(180.377008192716,534.118115256545,-49.0419236855484)) ;
#55148 = CARTESIAN_POINT('Ctrl Pts',(180.435164076688,534.136080563351,-49.037651458273)) ;
#55149 = CARTESIAN_POINT('Ctrl Pts',(180.49238060773,534.157219160222,-49.0334332618706)) ;
#55150 = CARTESIAN_POINT('Ctrl Pts',(180.54830297958,534.181395734778,-49.0292929444644)) ;
#55151 = CARTESIAN_POINT('Ctrl Pts',(180.604212012219,534.205566542475,-49.0251536146517)) ;
#55152 = CARTESIAN_POINT('Ctrl Pts',(180.658827472774,534.23277389933,-49.0210921290245)) ;
#55153 = CARTESIAN_POINT('Ctrl Pts',(180.711808013897,534.262850622761,-49.0171075326426)) ;
#55154 = CARTESIAN_POINT('Ctrl Pts',(180.766185635232,534.293720459932,-49.0130178637069)) ;
#55155 = CARTESIAN_POINT('Ctrl Pts',(180.818840769077,534.327613273201,-49.0090091772793)) ;
#55156 = CARTESIAN_POINT('Ctrl Pts',(180.869420113903,534.364312101834,-49.0050542246641)) ;
#55157 = CARTESIAN_POINT('Ctrl Pts',(180.918763220308,534.400113953606,-49.0011959372863)) ;
#55158 = CARTESIAN_POINT('Ctrl Pts',(180.966130585896,534.438586397744,-48.9973884266311)) ;
#55159 = CARTESIAN_POINT('Ctrl Pts',(181.01121166194,534.479491822943,-48.9935849087003)) ;
#55160 = CARTESIAN_POINT('Ctrl Pts',(181.057986924741,534.521934510243,-48.9896384511976)) ;
#55161 = CARTESIAN_POINT('Ctrl Pts',(181.102300177346,534.566997063816,-48.9856958697069)) ;
#55162 = CARTESIAN_POINT('Ctrl Pts',(181.143829998704,534.614369133583,-48.9816870242632)) ;
#55163 = CARTESIAN_POINT('Ctrl Pts',(181.179839562802,534.655444378478,-48.9782110455028)) ;
#55164 = CARTESIAN_POINT('Ctrl Pts',(181.213757200832,534.698256567649,-48.9746845931137)) ;
#55165 = CARTESIAN_POINT('Ctrl Pts',(181.245393149751,534.742569466473,-48.9710569730146)) ;
#55166 = CARTESIAN_POINT('Ctrl Pts',(181.250225564489,534.749338294742,-48.9705028513451)) ;
#55167 = CARTESIAN_POINT('Ctrl Pts',(181.255004836416,534.756142165679,-48.9699463691506)) ;
#55168 = CARTESIAN_POINT('Ctrl Pts',(181.259730391743,534.762980269371,-48.9693873457525)) ;
#55169 = CARTESIAN_POINT('Ctrl Pts',(181.259747376072,534.763004846505,-48.9693853365415)) ;
#55170 = CARTESIAN_POINT('Ctrl Pts',(181.259764359708,534.763029424081,-48.9693833272977)) ;
#55171 = CARTESIAN_POINT('Ctrl Pts',(181.25978134265,534.763054002099,-48.9693813180211)) ;
#55172 = CARTESIAN_POINT('Ctrl Pts',(181.291517598264,534.808983281234,-48.9656265552922)) ;
#55173 = CARTESIAN_POINT('Ctrl Pts',(181.320935495203,534.856622644612,-48.9617474963916)) ;
#55174 = CARTESIAN_POINT('Ctrl Pts',(181.347882919564,534.905702589268,-48.9578083354708)) ;
#55175 = CARTESIAN_POINT('Ctrl Pts',(181.350577125159,534.910609605973,-48.9574144978538)) ;
#55176 = CARTESIAN_POINT('Ctrl Pts',(181.353246637699,534.915530979809,-48.9570200594561)) ;
#55177 = CARTESIAN_POINT('Ctrl Pts',(181.355891307121,534.920466412928,-48.9566250844334)) ;
#55178 = CARTESIAN_POINT('Ctrl Pts',(181.384939266138,534.974675176342,-48.9522868415599)) ;
#55179 = CARTESIAN_POINT('Ctrl Pts',(181.410990463583,535.030586077216,-48.9478844932253)) ;
#55180 = CARTESIAN_POINT('Ctrl Pts',(181.433888757778,535.087830713585,-48.9434886857549)) ;
#55181 = CARTESIAN_POINT('Ctrl Pts',(181.456751886361,535.14498743761,-48.9390996290608)) ;
#55182 = CARTESIAN_POINT('Ctrl Pts',(181.476472164991,535.203473793683,-48.9347174294075)) ;
#55183 = CARTESIAN_POINT('Ctrl Pts',(181.492931602766,535.262916609204,-48.9303909258775)) ;
#55184 = CARTESIAN_POINT('Ctrl Pts',(181.509376246892,535.322305997857,-48.9260683109845)) ;
#55185 = CARTESIAN_POINT('Ctrl Pts',(181.522566046394,535.382650172329,-48.9218014321654)) ;
#55186 = CARTESIAN_POINT('Ctrl Pts',(181.532416933869,535.443570141042,-48.9176140482287)) ;
#55187 = CARTESIAN_POINT('Ctrl Pts',(181.542262726689,535.504458603335,-48.9134288299117)) ;
#55188 = CARTESIAN_POINT('Ctrl Pts',(181.548773015915,535.565922299089,-48.9093230295455)) ;
#55189 = CARTESIAN_POINT('Ctrl Pts',(181.551896803974,535.627575378101,-48.9052943808938)) ;
#55190 = CARTESIAN_POINT('Ctrl Pts',(181.553311741504,535.655501490141,-48.9034695816231)) ;
#55191 = CARTESIAN_POINT('Ctrl Pts',(181.554032326547,535.683466353274,-48.9016602577813)) ;
#55192 = CARTESIAN_POINT('Ctrl Pts',(181.55405613246,535.711433585225,-48.8998644770965)) ;
#55193 = CARTESIAN_POINT('Ctrl Pts',(181.554527408033,535.711416213393,-48.8995931994887)) ;
#55194 = CARTESIAN_POINT('Ctrl Pts',(181.554490128221,535.784394239434,-48.8949665191685)) ;
#55195 = CARTESIAN_POINT('Ctrl Pts',(181.549657875426,535.857294737052,-48.8904718398709)) ;
#55196 = CARTESIAN_POINT('Ctrl Pts',(181.526253544035,536.033724863836,-48.8795881565153)) ;
#55197 = CARTESIAN_POINT('Ctrl Pts',(181.502641909275,536.136251581272,-48.8732625061677)) ;
#55198 = CARTESIAN_POINT('Ctrl Pts',(181.463949750002,536.252705458684,-48.8654288299871)) ;
#55199 = CARTESIAN_POINT('Ctrl Pts',(181.458085759128,536.269455214264,-48.8642854378288)) ;
#55200 = CARTESIAN_POINT('Ctrl Pts',(181.451956083968,536.286106171205,-48.8631290382246)) ;
#55201 = CARTESIAN_POINT('Origin',(179.888527625402,502.164639879998,-37.0221601717597)) ;
#55202 = CARTESIAN_POINT('',(181.517728960952,505.503023000143,-38.2742386719919)) ;
#55203 = CARTESIAN_POINT('',(181.517728888183,505.561201209649,-38.2742387666786)) ;
#55204 = CARTESIAN_POINT('',(181.517728902316,502.164639879998,-38.2742387482878)) ;
#55205 = CARTESIAN_POINT('',(179.0652954453,505.710565160536,-38.9047876814237)) ;
#55206 = CARTESIAN_POINT('Ctrl Pts',(181.517728888183,505.561201209649,-38.2742387666786)) ;
#55207 = CARTESIAN_POINT('Ctrl Pts',(181.506945791598,505.562230187057,-38.2882697026309)) ;
#55208 = CARTESIAN_POINT('Ctrl Pts',(181.495980453669,505.563264428463,-38.302162624092)) ;
#55209 = CARTESIAN_POINT('Ctrl Pts',(181.398708147322,505.572330902422,-38.4221827887736)) ;
#55210 = CARTESIAN_POINT('Ctrl Pts',(181.302190203612,505.580630274102,-38.5195793218676)) ;
#55211 = CARTESIAN_POINT('Ctrl Pts',(181.157295447536,505.591637868681,-38.6392064954657)) ;
#55212 = CARTESIAN_POINT('Ctrl Pts',(181.116672538108,505.594585097538,-38.6702716511746)) ;
#55213 = CARTESIAN_POINT('Ctrl Pts',(181.050521260699,505.599116388462,-38.7170531278522)) ;
#55214 = CARTESIAN_POINT('Ctrl Pts',(181.025737466234,505.600756416772,-38.7337808892257)) ;
#55215 = CARTESIAN_POINT('Ctrl Pts',(180.965777197614,505.604581481536,-38.7723730801744)) ;
#55216 = CARTESIAN_POINT('Ctrl Pts',(180.930289321945,505.606736902647,-38.7937258388954)) ;
#55217 = CARTESIAN_POINT('Ctrl Pts',(180.798918856659,505.614413412551,-38.8674563566956)) ;
#55218 = CARTESIAN_POINT('Ctrl Pts',(180.699540091164,505.619658122738,-38.913242605739)) ;
#55219 = CARTESIAN_POINT('Ctrl Pts',(180.472699884994,505.631291927045,-38.9965642264894)) ;
#55220 = CARTESIAN_POINT('Ctrl Pts',(180.344303596121,505.637673696071,-39.0300927677737)) ;
#55221 = CARTESIAN_POINT('Ctrl Pts',(180.154882828558,505.647462318702,-39.0604403723471)) ;
#55222 = CARTESIAN_POINT('Ctrl Pts',(180.095810191248,505.650561966847,-39.0672920317259)) ;
#55223 = CARTESIAN_POINT('Ctrl Pts',(179.980836990606,505.656723534007,-39.0755948786593)) ;
#55224 = CARTESIAN_POINT('Ctrl Pts',(179.925010163103,505.659773616552,-39.0773446774586)) ;
#55225 = CARTESIAN_POINT('Ctrl Pts',(179.742716349138,505.669938782097,-39.075628525469)) ;
#55226 = CARTESIAN_POINT('Ctrl Pts',(179.616641991441,505.677310635259,-39.0627641504108)) ;
#55227 = CARTESIAN_POINT('Ctrl Pts',(179.386535557587,505.691124319092,-39.0175742582776)) ;
#55228 = CARTESIAN_POINT('Ctrl Pts',(179.282308570779,505.697517319274,-38.9884191047433)) ;
#55229 = CARTESIAN_POINT('Ctrl Pts',(179.159260972625,505.704950845021,-38.9432787890502)) ;
#55230 = CARTESIAN_POINT('Ctrl Pts',(179.137801261035,505.70624253918,-38.9349948726183)) ;
#55231 = CARTESIAN_POINT('Ctrl Pts',(179.099325627916,505.708544927455,-38.9193951581186)) ;
#55232 = CARTESIAN_POINT('Ctrl Pts',(179.082261060808,505.709561184396,-38.9122063771401)) ;
#55233 = CARTESIAN_POINT('Ctrl Pts',(179.0652954453,505.710565160536,-38.9047876814236)) ;
#55234 = CARTESIAN_POINT('',(178.234426126892,505.709295655298,-38.244821809929)) ;
#55235 = CARTESIAN_POINT('Origin',(179.888527625402,505.710565160536,-37.0221601717597)) ;
#55236 = CARTESIAN_POINT('Ctrl Pts',(178.236339423148,505.708026150059,-38.2437459062988)) ;
#55237 = CARTESIAN_POINT('Ctrl Pts',(178.246212321761,505.70712926237,-38.2570989491102)) ;
#55238 = CARTESIAN_POINT('Ctrl Pts',(178.256247088797,505.706243310869,-38.2703322870222)) ;
#55239 = CARTESIAN_POINT('Ctrl Pts',(178.280000811933,505.704201178492,-38.3008810138008)) ;
#55240 = CARTESIAN_POINT('Ctrl Pts',(178.293840894228,505.703052463216,-38.3180999086104)) ;
#55241 = CARTESIAN_POINT('Ctrl Pts',(178.386783981602,505.695578963799,-38.4299892423993)) ;
#55242 = CARTESIAN_POINT('Ctrl Pts',(178.474004687336,505.689671126553,-38.5176022345782)) ;
#55243 = CARTESIAN_POINT('Ctrl Pts',(178.659038150305,505.677961340228,-38.6727023863125)) ;
#55244 = CARTESIAN_POINT('Ctrl Pts',(178.755871947701,505.67218414584,-38.7405959966526)) ;
#55245 = CARTESIAN_POINT('Ctrl Pts',(178.903893650852,505.663356853194,-38.8264075768925)) ;
#55246 = CARTESIAN_POINT('Ctrl Pts',(178.950806700938,505.660562516286,-38.8512286646373)) ;
#55247 = CARTESIAN_POINT('Ctrl Pts',(179.046351159345,505.654848271938,-38.897137512791)) ;
#55248 = CARTESIAN_POINT('Ctrl Pts',(179.094942294336,505.651930805372,-38.9182147125759)) ;
#55249 = CARTESIAN_POINT('Ctrl Pts',(179.247425597898,505.642725165823,-38.9774680376964)) ;
#55250 = CARTESIAN_POINT('Ctrl Pts',(179.353616946369,505.636232474154,-39.0091442621736)) ;
#55251 = CARTESIAN_POINT('Ctrl Pts',(179.555318928392,505.62391815518,-39.0519640424075)) ;
#55252 = CARTESIAN_POINT('Ctrl Pts',(179.650079541876,505.618143888782,-39.0652643315994)) ;
#55253 = CARTESIAN_POINT('Ctrl Pts',(179.786761310523,505.610059059747,-39.0748068607388)) ;
#55254 = CARTESIAN_POINT('Ctrl Pts',(179.828180548463,505.607641981781,-39.0764418972258)) ;
#55255 = CARTESIAN_POINT('Ctrl Pts',(179.904055275859,505.603306143197,-39.0771400117366)) ;
#55256 = CARTESIAN_POINT('Ctrl Pts',(179.938492507703,505.601372943566,-39.076591254611)) ;
#55257 = CARTESIAN_POINT('Ctrl Pts',(180.003921401465,505.597786719259,-39.073902279837)) ;
#55258 = CARTESIAN_POINT('Ctrl Pts',(180.034908371763,505.596127113771,-39.0719245855875)) ;
#55259 = CARTESIAN_POINT('Ctrl Pts',(180.137752135288,505.590716041551,-39.0630165928796)) ;
#55260 = CARTESIAN_POINT('Ctrl Pts',(180.209293152321,505.58710800581,-39.0530021324179)) ;
#55261 = CARTESIAN_POINT('Ctrl Pts',(180.443789446986,505.575387287441,-39.0074723494109)) ;
#55262 = CARTESIAN_POINT('Ctrl Pts',(180.602935399332,505.567551403571,-38.9559137276696)) ;
#55263 = CARTESIAN_POINT('Ctrl Pts',(180.808399358356,505.556076568485,-38.8604792358664)) ;
#55264 = CARTESIAN_POINT('Ctrl Pts',(180.861558421441,505.552978927717,-38.8329034306958)) ;
#55265 = CARTESIAN_POINT('Ctrl Pts',(180.956628338775,505.547149905503,-38.7781903545838)) ;
#55266 = CARTESIAN_POINT('Ctrl Pts',(180.998900001781,505.544446254891,-38.7517710284809)) ;
#55267 = CARTESIAN_POINT('Ctrl Pts',(181.100521819816,505.537647960482,-38.6829969191819)) ;
#55268 = CARTESIAN_POINT('Ctrl Pts',(181.158654772859,505.533491702225,-38.6389730409796)) ;
#55269 = CARTESIAN_POINT('Ctrl Pts',(181.326530288598,505.520674159904,-38.497191454525)) ;
#55270 = CARTESIAN_POINT('Ctrl Pts',(181.428243787735,505.511729959464,-38.3906765500404)) ;
#55271 = CARTESIAN_POINT('Ctrl Pts',(181.517728960952,505.503023000143,-38.2742386719919)) ;
#55272 = CARTESIAN_POINT('Origin',(179.888527625402,502.164639879998,-37.0221601717597)) ;
#55273 = CARTESIAN_POINT('',(181.51772890232,504.803342258844,-38.274238748284)) ;
#55274 = CARTESIAN_POINT('',(181.517728902317,504.861481368308,-38.2742387482878)) ;
#55275 = CARTESIAN_POINT('',(181.517728902316,502.164639879998,-38.2742387482878)) ;
#55276 = CARTESIAN_POINT('',(179.887971218886,505.313227684039,-34.9674102470945)) ;
#55277 = CARTESIAN_POINT('Ctrl Pts',(181.517728902317,504.861481368308,-38.2742387482878)) ;
#55278 = CARTESIAN_POINT('Ctrl Pts',(181.50282363087,504.862713419422,-38.2936334474142)) ;
#55279 = CARTESIAN_POINT('Ctrl Pts',(181.487566558281,504.863956449484,-38.3127691192065)) ;
#55280 = CARTESIAN_POINT('Ctrl Pts',(181.437041422955,504.868022782347,-38.3738648120083)) ;
#55281 = CARTESIAN_POINT('Ctrl Pts',(181.400446089409,504.870893009831,-38.4146766830833)) ;
#55282 = CARTESIAN_POINT('Ctrl Pts',(181.326218546114,504.876610157377,-38.4910775843731)) ;
#55283 = CARTESIAN_POINT('Ctrl Pts',(181.288785863608,504.879447242012,-38.5268028955588)) ;
#55284 = CARTESIAN_POINT('Ctrl Pts',(181.178928258441,504.887664764052,-38.62399685699)) ;
#55285 = CARTESIAN_POINT('Ctrl Pts',(181.103541408712,504.893184704261,-38.681904829899)) ;
#55286 = CARTESIAN_POINT('Ctrl Pts',(180.910205101557,504.906968927363,-38.8101651976646)) ;
#55287 = CARTESIAN_POINT('Ctrl Pts',(180.788689014218,504.915343739997,-38.8743198567907)) ;
#55288 = CARTESIAN_POINT('Ctrl Pts',(180.617900324062,504.926134764785,-38.9436822371964)) ;
#55289 = CARTESIAN_POINT('Ctrl Pts',(180.573504544794,504.928853816136,-38.9599524418868)) ;
#55290 = CARTESIAN_POINT('Ctrl Pts',(180.500862519732,504.933121744483,-38.9837652791507)) ;
#55291 = CARTESIAN_POINT('Ctrl Pts',(180.472951274591,504.934717718867,-38.9922611562714)) ;
#55292 = CARTESIAN_POINT('Ctrl Pts',(180.403482470405,504.93858097189,-39.0118000715804)) ;
#55293 = CARTESIAN_POINT('Ctrl Pts',(180.361743305479,504.940811754778,-39.0221383886533)) ;
#55294 = CARTESIAN_POINT('Ctrl Pts',(180.262772521127,504.94595474411,-39.0433799164438)) ;
#55295 = CARTESIAN_POINT('Ctrl Pts',(180.205340497337,504.948826149853,-39.0531744030832)) ;
#55296 = CARTESIAN_POINT('Ctrl Pts',(179.972778671358,504.960259848407,-39.08272897806)) ;
#55297 = CARTESIAN_POINT('Ctrl Pts',(179.795872929643,504.968592730584,-39.0823677814946)) ;
#55298 = CARTESIAN_POINT('Ctrl Pts',(179.568754377692,504.980417511158,-39.0525637117123)) ;
#55299 = CARTESIAN_POINT('Ctrl Pts',(179.516616330564,504.983204364824,-39.043663269288)) ;
#55300 = CARTESIAN_POINT('Ctrl Pts',(179.412716238464,504.988933406861,-39.0217709373221)) ;
#55301 = CARTESIAN_POINT('Ctrl Pts',(179.361001525323,504.991874491635,-39.0087540280226)) ;
#55302 = CARTESIAN_POINT('Ctrl Pts',(179.192627011546,505.001764611085,-38.9593349294167)) ;
#55303 = CARTESIAN_POINT('Ctrl Pts',(179.07871718205,505.008980873443,-38.9145458267304)) ;
#55304 = CARTESIAN_POINT('Ctrl Pts',(178.852478096477,505.024159551189,-38.8014044454432)) ;
#55305 = CARTESIAN_POINT('Ctrl Pts',(178.741331359726,505.03210293927,-38.7318540881188)) ;
#55306 = CARTESIAN_POINT('Ctrl Pts',(178.610969676867,505.041478563465,-38.6318078637487)) ;
#55307 = CARTESIAN_POINT('Ctrl Pts',(178.584892698132,505.043356010995,-38.6107621604143)) ;
#55308 = CARTESIAN_POINT('Ctrl Pts',(178.534889910419,505.046940292589,-38.5683459656992)) ;
#55309 = CARTESIAN_POINT('Ctrl Pts',(178.510927173022,505.048649644795,-38.5470348358357)) ;
#55310 = CARTESIAN_POINT('Ctrl Pts',(178.425797979676,505.054732640259,-38.4676802790939)) ;
#55311 = CARTESIAN_POINT('Ctrl Pts',(178.367715003357,505.058905309628,-38.4064426497816)) ;
#55312 = CARTESIAN_POINT('Ctrl Pts',(178.200174680065,505.071625779624,-38.2064861184753)) ;
#55313 = CARTESIAN_POINT('Ctrl Pts',(178.104713582771,505.079982814636,-38.0571331416867)) ;
#55314 = CARTESIAN_POINT('Ctrl Pts',(178.007172384774,505.091822113924,-37.8499593367763)) ;
#55315 = CARTESIAN_POINT('Ctrl Pts',(177.98665561363,505.094590877831,-37.8016671839152)) ;
#55316 = CARTESIAN_POINT('Ctrl Pts',(177.948916516739,505.100325959965,-37.7024474158823)) ;
#55317 = CARTESIAN_POINT('Ctrl Pts',(177.931800044227,505.103293208672,-37.6515236510647)) ;
#55318 = CARTESIAN_POINT('Ctrl Pts',(177.88195337532,505.113298788486,-37.4814235451365)) ;
#55319 = CARTESIAN_POINT('Ctrl Pts',(177.857977493662,505.120610343437,-37.359979317665)) ;
#55320 = CARTESIAN_POINT('Ctrl Pts',(177.831742032306,505.135670801813,-37.1105929793872)) ;
#55321 = CARTESIAN_POINT('Ctrl Pts',(177.830211815779,505.143391072684,-36.9830826193027)) ;
#55322 = CARTESIAN_POINT('Ctrl Pts',(177.843214108276,505.15258837476,-36.8225839898811)) ;
#55323 = CARTESIAN_POINT('Ctrl Pts',(177.846770636977,505.154482903932,-36.7889934075561)) ;
#55324 = CARTESIAN_POINT('Ctrl Pts',(177.855261939735,505.158063070187,-36.7241161014549)) ;
#55325 = CARTESIAN_POINT('Ctrl Pts',(177.860094924488,505.159752705507,-36.6928267068736)) ;
#55326 = CARTESIAN_POINT('Ctrl Pts',(177.879441866848,505.16552342851,-36.5842648942137)) ;
#55327 = CARTESIAN_POINT('Ctrl Pts',(177.897666316002,505.16943123101,-36.5077174405858)) ;
#55328 = CARTESIAN_POINT('Ctrl Pts',(177.973348629029,505.182320458574,-36.2551331059409)) ;
#55329 = CARTESIAN_POINT('Ctrl Pts',(178.050158718153,505.191034474329,-36.0858695805616)) ;
#55330 = CARTESIAN_POINT('Ctrl Pts',(178.176214430807,505.203300396884,-35.885200307277)) ;
#55331 = CARTESIAN_POINT('Ctrl Pts',(178.205492365261,505.206044401104,-35.8422932854756)) ;
#55332 = CARTESIAN_POINT('Ctrl Pts',(178.268306221195,505.211757672042,-35.7573412044155)) ;
#55333 = CARTESIAN_POINT('Ctrl Pts',(178.301929954114,505.214729261373,-35.7154117370569)) ;
#55334 = CARTESIAN_POINT('Ctrl Pts',(178.381136018215,505.221555419153,-35.6242092075448)) ;
#55335 = CARTESIAN_POINT('Ctrl Pts',(178.427565683494,505.225442493708,-35.5757559302762)) ;
#55336 = CARTESIAN_POINT('Ctrl Pts',(178.574219856507,505.237356109792,-35.4369869716062)) ;
#55337 = CARTESIAN_POINT('Ctrl Pts',(178.681038772688,505.245589361687,-35.3541834205342)) ;
#55338 = CARTESIAN_POINT('Ctrl Pts',(178.846459501428,505.257187660007,-35.2502240118311)) ;
#55339 = CARTESIAN_POINT('Ctrl Pts',(178.899128640742,505.260725524652,-35.2202848727496)) ;
#55340 = CARTESIAN_POINT('Ctrl Pts',(178.979904262458,505.265842752296,-35.1789805692709)) ;
#55341 = CARTESIAN_POINT('Ctrl Pts',(179.007062480536,505.267512411627,-35.1658393257151)) ;
#55342 = CARTESIAN_POINT('Ctrl Pts',(179.068368260311,505.271158027716,-35.1378241064699)) ;
#55343 = CARTESIAN_POINT('Ctrl Pts',(179.102648687739,505.273116927721,-35.1232714293314)) ;
#55344 = CARTESIAN_POINT('Ctrl Pts',(179.180511213483,505.277429531326,-35.0926874892022)) ;
#55345 = CARTESIAN_POINT('Ctrl Pts',(179.22427952349,505.279760331122,-35.0771853693676)) ;
#55346 = CARTESIAN_POINT('Ctrl Pts',(179.438002309131,505.290856676824,-35.0095451153084)) ;
#55347 = CARTESIAN_POINT('Ctrl Pts',(179.613705040265,505.299195207764,-34.9781278433698)) ;
#55348 = CARTESIAN_POINT('Ctrl Pts',(179.82347870271,505.309884020926,-34.9681868744578)) ;
#55349 = CARTESIAN_POINT('Ctrl Pts',(179.855723251356,505.311544657051,-34.9674189795339)) ;
#55350 = CARTESIAN_POINT('Ctrl Pts',(179.887971218886,505.313227684039,-34.9674102470945)) ;
#55351 = CARTESIAN_POINT('Ctrl Pts',(179.887972413115,505.313227746366,-34.9674102467714)) ;
#55352 = CARTESIAN_POINT('Ctrl Pts',(179.931624596704,505.315505962097,-34.9673984515508)) ;
#55353 = CARTESIAN_POINT('Ctrl Pts',(179.975264213753,505.317824392976,-34.9687777029824)) ;
#55354 = CARTESIAN_POINT('Ctrl Pts',(180.071034514204,505.323019000527,-34.9748630274251)) ;
#55355 = CARTESIAN_POINT('Ctrl Pts',(180.12309408548,505.325912770164,-34.9801728486144)) ;
#55356 = CARTESIAN_POINT('Ctrl Pts',(180.339374193126,505.338248025649,-35.0106121445431)) ;
#55357 = CARTESIAN_POINT('Ctrl Pts',(180.500421876701,505.348260125775,-35.0536184191277)) ;
#55358 = CARTESIAN_POINT('Ctrl Pts',(180.738149110347,505.36365468944,-35.1491235186524)) ;
#55359 = CARTESIAN_POINT('Ctrl Pts',(180.819498133654,505.369028756897,-35.1881973587433)) ;
#55360 = CARTESIAN_POINT('Ctrl Pts',(180.926256113304,505.376002474111,-35.2484161508916)) ;
#55361 = CARTESIAN_POINT('Ctrl Pts',(180.954110624124,505.377813697724,-35.2650086380489)) ;
#55362 = CARTESIAN_POINT('Ctrl Pts',(181.01002191576,505.38141385678,-35.3001329815278)) ;
#55363 = CARTESIAN_POINT('Ctrl Pts',(181.038039513195,505.383199869814,-35.3187078542507)) ;
#55364 = CARTESIAN_POINT('Ctrl Pts',(181.170976703106,505.39164948612,-35.4116158754433)) ;
#55365 = CARTESIAN_POINT('Ctrl Pts',(181.269228688345,505.397831670211,-35.4950058982537)) ;
#55366 = CARTESIAN_POINT('Ctrl Pts',(181.443401754122,505.409947652062,-35.6734754734415)) ;
#55367 = CARTESIAN_POINT('Ctrl Pts',(181.519965404593,505.41585405327,-35.767173573077)) ;
#55368 = CARTESIAN_POINT('Ctrl Pts',(181.618071696416,505.424860150587,-35.911500749566)) ;
#55369 = CARTESIAN_POINT('Ctrl Pts',(181.646532203332,505.427692129625,-35.957122028688)) ;
#55370 = CARTESIAN_POINT('Ctrl Pts',(181.699728654425,505.433482231359,-36.0503474094442)) ;
#55371 = CARTESIAN_POINT('Ctrl Pts',(181.724454417662,505.436437682742,-36.0979084387649)) ;
#55372 = CARTESIAN_POINT('Ctrl Pts',(181.795453102887,505.445823773504,-36.2485964610278)) ;
#55373 = CARTESIAN_POINT('Ctrl Pts',(181.835094616754,505.452470648951,-36.3545999288584)) ;
#55374 = CARTESIAN_POINT('Ctrl Pts',(181.891794920882,505.464954704331,-36.5552141626888)) ;
#55375 = CARTESIAN_POINT('Ctrl Pts',(181.911330962379,505.470739045616,-36.6488165827598)) ;
#55376 = CARTESIAN_POINT('Ctrl Pts',(181.931993385343,505.479746454951,-36.7997332961412)) ;
#55377 = CARTESIAN_POINT('Ctrl Pts',(181.937363084996,505.483052483556,-36.8563279573793)) ;
#55378 = CARTESIAN_POINT('Ctrl Pts',(181.941943114895,505.487906593332,-36.9424778543331)) ;
#55379 = CARTESIAN_POINT('Ctrl Pts',(181.942874221793,505.489533360928,-36.9719122135335)) ;
#55380 = CARTESIAN_POINT('Ctrl Pts',(181.943521358908,505.492982993229,-37.0358350683226)) ;
#55381 = CARTESIAN_POINT('Ctrl Pts',(181.943002633073,505.494792895322,-37.0703162863717)) ;
#55382 = CARTESIAN_POINT('Ctrl Pts',(181.937076119565,505.502368070327,-37.2176063008932)) ;
#55383 = CARTESIAN_POINT('Ctrl Pts',(181.92324108779,505.507758163467,-37.3298881288155)) ;
#55384 = CARTESIAN_POINT('Ctrl Pts',(181.872006909521,505.519758210943,-37.5762796076252)) ;
#55385 = CARTESIAN_POINT('Ctrl Pts',(181.830091785001,505.526352693664,-37.7088648575302)) ;
#55386 = CARTESIAN_POINT('Ctrl Pts',(181.753104771879,505.536221744344,-37.8872865964356)) ;
#55387 = CARTESIAN_POINT('Ctrl Pts',(181.729004159842,505.539110381616,-37.9374399116075)) ;
#55388 = CARTESIAN_POINT('Ctrl Pts',(181.679482633419,505.544731528113,-38.0306080534783)) ;
#55389 = CARTESIAN_POINT('Ctrl Pts',(181.654469790178,505.547447447767,-38.0737944312678)) ;
#55390 = CARTESIAN_POINT('Ctrl Pts',(181.59367203227,505.553795920953,-38.1704705610456)) ;
#55391 = CARTESIAN_POINT('Ctrl Pts',(181.556903044612,505.557463014257,-38.2232654608651)) ;
#55392 = CARTESIAN_POINT('Ctrl Pts',(181.517728888183,505.561201209649,-38.2742387666786)) ;
#55393 = CARTESIAN_POINT('Ctrl Pts',(181.517728960952,505.503023000143,-38.2742386719921)) ;
#55394 = CARTESIAN_POINT('Ctrl Pts',(181.554510770023,505.49944410876,-38.2263782762974)) ;
#55395 = CARTESIAN_POINT('Ctrl Pts',(181.589163153578,505.495917597715,-38.1769246559147)) ;
#55396 = CARTESIAN_POINT('Ctrl Pts',(181.635738170017,505.491018477495,-38.1038005625687)) ;
#55397 = CARTESIAN_POINT('Ctrl Pts',(181.649453667286,505.489553360676,-38.0813250528931)) ;
#55398 = CARTESIAN_POINT('Ctrl Pts',(181.67892390674,505.486364843897,-38.030876639769)) ;
#55399 = CARTESIAN_POINT('Ctrl Pts',(181.69446269358,505.48465660206,-38.0027857105539)) ;
#55400 = CARTESIAN_POINT('Ctrl Pts',(181.78637602339,505.474307774169,-37.8270242641324)) ;
#55401 = CARTESIAN_POINT('Ctrl Pts',(181.845261127654,505.466528423751,-37.6708843680565)) ;
#55402 = CARTESIAN_POINT('Ctrl Pts',(181.907842843034,505.453676279027,-37.4144626183609)) ;
#55403 = CARTESIAN_POINT('Ctrl Pts',(181.924202799645,505.448836792646,-37.3180640728702)) ;
#55404 = CARTESIAN_POINT('Ctrl Pts',(181.938627586626,505.441114805809,-37.1696078189518)) ;
#55405 = CARTESIAN_POINT('Ctrl Pts',(181.941679128983,505.438392589766,-37.118175395422)) ;
#55406 = CARTESIAN_POINT('Ctrl Pts',(181.943954873281,505.432713613478,-37.013179198085)) ;
#55407 = CARTESIAN_POINT('Ctrl Pts',(181.943023622886,505.429753999333,-36.9596520981478)) ;
#55408 = CARTESIAN_POINT('Ctrl Pts',(181.930436534106,505.417150816679,-36.7369218776964)) ;
#55409 = CARTESIAN_POINT('Ctrl Pts',(181.899947743615,505.406908163481,-36.5694745900173)) ;
#55410 = CARTESIAN_POINT('Ctrl Pts',(181.824023270054,505.391680435388,-36.3271975443084)) ;
#55411 = CARTESIAN_POINT('Ctrl Pts',(181.793854915335,505.386668174524,-36.2483082814553)) ;
#55412 = CARTESIAN_POINT('Ctrl Pts',(181.745708792909,505.380059492607,-36.1424478654832)) ;
#55413 = CARTESIAN_POINT('Ctrl Pts',(181.731823382325,505.378278524731,-36.1137127525355)) ;
#55414 = CARTESIAN_POINT('Ctrl Pts',(181.702253366721,505.374745292009,-36.0559916111054)) ;
#55415 = CARTESIAN_POINT('Ctrl Pts',(181.686529709557,505.372995763219,-36.0270362920814)) ;
#55416 = CARTESIAN_POINT('Ctrl Pts',(181.602523575396,505.364217038176,-35.8808355256149)) ;
#55417 = CARTESIAN_POINT('Ctrl Pts',(181.523439320893,505.357740639546,-35.77017131911)) ;
#55418 = CARTESIAN_POINT('Ctrl Pts',(181.355597259194,505.345408502778,-35.5786006272249)) ;
#55419 = CARTESIAN_POINT('Ctrl Pts',(181.269558985418,505.339596000749,-35.4960846905156)) ;
#55420 = CARTESIAN_POINT('Ctrl Pts',(181.135607706568,505.330733272368,-35.3882707736326)) ;
#55421 = CARTESIAN_POINT('Ctrl Pts',(181.093078107769,505.327945947911,-35.3566690283912)) ;
#55422 = CARTESIAN_POINT('Ctrl Pts',(181.006093460233,505.322266517321,-35.2971106039524)) ;
#55423 = CARTESIAN_POINT('Ctrl Pts',(180.961693510379,505.319377809688,-35.2691445782153)) ;
#55424 = CARTESIAN_POINT('Ctrl Pts',(180.761128228956,505.306349393143,-35.1532921951252)) ;
#55425 = CARTESIAN_POINT('Ctrl Pts',(180.594945730838,505.295515671179,-35.0843647071077)) ;
#55426 = CARTESIAN_POINT('Ctrl Pts',(180.367281162788,505.281395127858,-35.0231602897937)) ;
#55427 = CARTESIAN_POINT('Ctrl Pts',(180.311997303755,505.278027884774,-35.0107229876461)) ;
#55428 = CARTESIAN_POINT('Ctrl Pts',(180.214757553672,505.272283117937,-34.993034322229)) ;
#55429 = CARTESIAN_POINT('Ctrl Pts',(180.173021458832,505.26987377499,-34.9867630468717)) ;
#55430 = CARTESIAN_POINT('Ctrl Pts',(180.10227508799,505.265917412238,-34.9783516391548)) ;
#55431 = CARTESIAN_POINT('Ctrl Pts',(180.073364290604,505.264338521813,-34.9755344490615)) ;
#55432 = CARTESIAN_POINT('Ctrl Pts',(179.996946110786,505.260257859883,-34.9697207093969)) ;
#55433 = CARTESIAN_POINT('Ctrl Pts',(179.949379135104,505.257807667233,-34.9677599976293)) ;
#55434 = CARTESIAN_POINT('Ctrl Pts',(179.752988343518,505.247908929112,-34.9664929693984)) ;
#55435 = CARTESIAN_POINT('Ctrl Pts',(179.604521400592,505.240910782813,-34.9816982294533)) ;
#55436 = CARTESIAN_POINT('Ctrl Pts',(179.374574098227,505.229366836633,-35.0308537664649)) ;
#55437 = CARTESIAN_POINT('Ctrl Pts',(179.291385813054,505.225043858586,-35.0541995438076)) ;
#55438 = CARTESIAN_POINT('Ctrl Pts',(179.161903251777,505.217905790038,-35.0995052109148)) ;
#55439 = CARTESIAN_POINT('Ctrl Pts',(179.114533565336,505.215204220988,-35.1180809578454)) ;
#55440 = CARTESIAN_POINT('Ctrl Pts',(179.016880644929,505.20941899721,-35.1606214027236)) ;
#55441 = CARTESIAN_POINT('Ctrl Pts',(178.966785009288,505.206325608557,-35.1849109394923)) ;
#55442 = CARTESIAN_POINT('Ctrl Pts',(178.811604740099,505.196325638273,-35.268097333245)) ;
#55443 = CARTESIAN_POINT('Ctrl Pts',(178.710689149975,505.189174784485,-35.3342059919185)) ;
#55444 = CARTESIAN_POINT('Ctrl Pts',(178.529513132168,505.175308823821,-35.4770866111379)) ;
#55445 = CARTESIAN_POINT('Ctrl Pts',(178.448513295891,505.168634380227,-35.5522847288833)) ;
#55446 = CARTESIAN_POINT('Ctrl Pts',(178.347828681236,505.160026280009,-35.6621096346609)) ;
#55447 = CARTESIAN_POINT('Ctrl Pts',(178.322523015511,505.157833235595,-35.6913255909611)) ;
#55448 = CARTESIAN_POINT('Ctrl Pts',(178.279421935928,505.154071062762,-35.7440198991991)) ;
#55449 = CARTESIAN_POINT('Ctrl Pts',(178.261282946576,505.152480968429,-35.7671946376364)) ;
#55450 = CARTESIAN_POINT('Ctrl Pts',(178.211446768641,505.148076875168,-35.8337646388747)) ;
#55451 = CARTESIAN_POINT('Ctrl Pts',(178.180945123605,505.145335036363,-35.8780242378745)) ;
#55452 = CARTESIAN_POINT('Ctrl Pts',(178.076637222254,505.135588865683,-36.0428616130159)) ;
#55453 = CARTESIAN_POINT('Ctrl Pts',(178.013583893043,505.128924879494,-36.1697737966513)) ;
#55454 = CARTESIAN_POINT('Ctrl Pts',(177.940576001184,505.118684694105,-36.3649147307929)) ;
#55455 = CARTESIAN_POINT('Ctrl Pts',(177.920182288141,505.115339014052,-36.4287776684847)) ;
#55456 = CARTESIAN_POINT('Ctrl Pts',(177.888987183786,505.109114088239,-36.5459469176096)) ;
#55457 = CARTESIAN_POINT('Ctrl Pts',(177.877111785744,505.106270079784,-36.5989029907302)) ;
#55458 = CARTESIAN_POINT('Ctrl Pts',(177.858072068449,505.100590457945,-36.7029395308634)) ;
#55459 = CARTESIAN_POINT('Ctrl Pts',(177.850707694297,505.097763759575,-36.7539422858839)) ;
#55460 = CARTESIAN_POINT('Ctrl Pts',(177.835212219268,505.08954075187,-36.8998499542524)) ;
#55461 = CARTESIAN_POINT('Ctrl Pts',(177.831751415802,505.084003358379,-36.9951082483004)) ;
#55462 = CARTESIAN_POINT('Ctrl Pts',(177.83868017466,505.071577020968,-37.2040713634775)) ;
#55463 = CARTESIAN_POINT('Ctrl Pts',(177.851909360546,505.064653948259,-37.3173742040268)) ;
#55464 = CARTESIAN_POINT('Ctrl Pts',(177.886697652542,505.054223387855,-37.4895963906249)) ;
#55465 = CARTESIAN_POINT('Ctrl Pts',(177.901668740072,505.050609444951,-37.5496190689917)) ;
#55466 = CARTESIAN_POINT('Ctrl Pts',(177.927935476712,505.045420003552,-37.6377779449765)) ;
#55467 = CARTESIAN_POINT('Ctrl Pts',(177.937181561602,505.043749950309,-37.6664860034803)) ;
#55468 = CARTESIAN_POINT('Ctrl Pts',(177.95885781082,505.040168131594,-37.7290340023793)) ;
#55469 = CARTESIAN_POINT('Ctrl Pts',(177.971552469016,505.038270490356,-37.7627699197628)) ;
#55470 = CARTESIAN_POINT('Ctrl Pts',(178.047602738773,505.027853259488,-37.9497914493535)) ;
#55471 = CARTESIAN_POINT('Ctrl Pts',(178.128453652584,505.020097653723,-38.095312534693)) ;
#55472 = CARTESIAN_POINT('Ctrl Pts',(178.278953832286,505.007558116924,-38.3025556108408)) ;
#55473 = CARTESIAN_POINT('Ctrl Pts',(178.336724730834,505.003054955549,-38.3719919427473)) ;
#55474 = CARTESIAN_POINT('Ctrl Pts',(178.434107430826,504.995710555175,-38.4744952105936)) ;
#55475 = CARTESIAN_POINT('Ctrl Pts',(178.470717108393,504.992997867744,-38.5102555572575)) ;
#55476 = CARTESIAN_POINT('Ctrl Pts',(178.549338706159,504.987243354291,-38.5815159802886)) ;
#55477 = CARTESIAN_POINT('Ctrl Pts',(178.591517366953,504.984194287864,-38.6167701755253)) ;
#55478 = CARTESIAN_POINT('Ctrl Pts',(178.759603259324,504.97216850995,-38.7461769621864)) ;
#55479 = CARTESIAN_POINT('Ctrl Pts',(178.89472754835,504.962705481812,-38.8274445554859)) ;
#55480 = CARTESIAN_POINT('Ctrl Pts',(179.095257837632,504.949475272808,-38.9186595863778)) ;
#55481 = CARTESIAN_POINT('Ctrl Pts',(179.153929308183,504.945701104997,-38.9421479390222)) ;
#55482 = CARTESIAN_POINT('Ctrl Pts',(179.256223917001,504.939377492616,-38.9777232330315)) ;
#55483 = CARTESIAN_POINT('Ctrl Pts',(179.299336185575,504.936787934222,-38.9911418686249)) ;
#55484 = CARTESIAN_POINT('Ctrl Pts',(179.370769502948,504.932658847094,-39.0108185696902)) ;
#55485 = CARTESIAN_POINT('Ctrl Pts',(179.398838639979,504.931078355285,-39.017915823146)) ;
#55486 = CARTESIAN_POINT('Ctrl Pts',(179.470007068975,504.927175004462,-39.0343184980821)) ;
#55487 = CARTESIAN_POINT('Ctrl Pts',(179.513271321743,504.924892562287,-39.042834279208)) ;
#55488 = CARTESIAN_POINT('Ctrl Pts',(179.690575515069,504.915784628321,-39.0718414103903)) ;
#55489 = CARTESIAN_POINT('Ctrl Pts',(179.82621896306,504.909365180685,-39.0804364677486)) ;
#55490 = CARTESIAN_POINT('Ctrl Pts',(180.061658190465,504.89789044222,-39.0720435930674)) ;
#55491 = CARTESIAN_POINT('Ctrl Pts',(180.161187072156,504.892938588785,-39.061191888782)) ;
#55492 = CARTESIAN_POINT('Ctrl Pts',(180.310511694759,504.885077487925,-39.0337800158408)) ;
#55493 = CARTESIAN_POINT('Ctrl Pts',(180.361123731274,504.882337463574,-39.0224944500205)) ;
#55494 = CARTESIAN_POINT('Ctrl Pts',(180.463267303572,504.876625428776,-38.9956253111134)) ;
#55495 = CARTESIAN_POINT('Ctrl Pts',(180.514721208572,504.87365076055,-38.9799066252577)) ;
#55496 = CARTESIAN_POINT('Ctrl Pts',(180.725184840137,504.861055860518,-38.9064658240645)) ;
#55497 = CARTESIAN_POINT('Ctrl Pts',(180.877362673786,504.850843475642,-38.8312457951857)) ;
#55498 = CARTESIAN_POINT('Ctrl Pts',(181.089366082257,504.83561987089,-38.6916417816203)) ;
#55499 = CARTESIAN_POINT('Ctrl Pts',(181.157210572134,504.830584282341,-38.6406866091251)) ;
#55500 = CARTESIAN_POINT('Ctrl Pts',(181.246042418268,504.823950332707,-38.5649411098106)) ;
#55501 = CARTESIAN_POINT('Ctrl Pts',(181.269881555035,504.822166052496,-38.543633499697)) ;
#55502 = CARTESIAN_POINT('Ctrl Pts',(181.31731634043,504.818625242278,-38.499201421119)) ;
#55503 = CARTESIAN_POINT('Ctrl Pts',(181.340870923605,504.816871510371,-38.4760471234562)) ;
#55504 = CARTESIAN_POINT('Ctrl Pts',(181.418504873589,504.811064661938,-38.395961894576)) ;
#55505 = CARTESIAN_POINT('Ctrl Pts',(181.469879937113,504.807174807454,-38.3364996931447)) ;
#55506 = CARTESIAN_POINT('Ctrl Pts',(181.517728902323,504.803342258844,-38.2742387482803)) ;
#55507 = CARTESIAN_POINT('Origin',(179.888527625402,502.164639879998,-37.0221601717597)) ;
#55508 = CARTESIAN_POINT('',(181.517263155791,504.105570724017,-38.2738081386943)) ;
#55509 = CARTESIAN_POINT('',(181.517722816555,504.164527114775,-38.2742466670251)) ;
#55510 = CARTESIAN_POINT('',(181.517728902316,502.164639879998,-38.2742387482878)) ;
#55511 = CARTESIAN_POINT('',(179.888051515576,503.856489564609,-34.9674102269198)) ;
#55512 = CARTESIAN_POINT('Ctrl Pts',(179.888012689102,503.857432638953,-34.9679547929697)) ;
#55513 = CARTESIAN_POINT('Ctrl Pts',(179.958932145949,503.86150620242,-34.9680734899365)) ;
#55514 = CARTESIAN_POINT('Ctrl Pts',(180.029892959977,503.865524608869,-34.9718370771033)) ;
#55515 = CARTESIAN_POINT('Ctrl Pts',(180.100498384139,503.869458476652,-34.9792189466439)) ;
#55516 = CARTESIAN_POINT('Ctrl Pts',(180.171085622775,503.873391331207,-34.986598914869)) ;
#55517 = CARTESIAN_POINT('Ctrl Pts',(180.241317632988,503.877239660488,-34.9975952865709)) ;
#55518 = CARTESIAN_POINT('Ctrl Pts',(180.310802165125,503.880998694863,-35.0121470101295)) ;
#55519 = CARTESIAN_POINT('Ctrl Pts',(180.380292601802,503.884758048666,-35.0266999702401)) ;
#55520 = CARTESIAN_POINT('Ctrl Pts',(180.449035362884,503.888428164958,-35.0448089803899)) ;
#55521 = CARTESIAN_POINT('Ctrl Pts',(180.516642979013,503.892028550131,-35.0663778912399)) ;
#55522 = CARTESIAN_POINT('Ctrl Pts',(180.584328547214,503.895633086574,-35.0879716712008)) ;
#55523 = CARTESIAN_POINT('Ctrl Pts',(180.650876219736,503.899167916646,-35.1130335410347)) ;
#55524 = CARTESIAN_POINT('Ctrl Pts',(180.715903572164,503.902675042469,-35.1414296045501)) ;
#55525 = CARTESIAN_POINT('Ctrl Pts',(180.780971130696,503.906184336732,-35.169843225217)) ;
#55526 = CARTESIAN_POINT('Ctrl Pts',(180.844516253085,503.909666237896,-35.2015954784639)) ;
#55527 = CARTESIAN_POINT('Ctrl Pts',(180.90616488458,503.913181328988,-35.236510876872)) ;
#55528 = CARTESIAN_POINT('Ctrl Pts',(180.964246578652,503.916493039897,-35.2694061000028)) ;
#55529 = CARTESIAN_POINT('Ctrl Pts',(181.020645072211,503.919834702901,-35.305109425717)) ;
#55530 = CARTESIAN_POINT('Ctrl Pts',(181.075057591808,503.923266837811,-35.3434349028281)) ;
#55531 = CARTESIAN_POINT('Ctrl Pts',(181.078508092662,503.923484482289,-35.3458652643052)) ;
#55532 = CARTESIAN_POINT('Ctrl Pts',(181.081950624698,503.923702490582,-35.348306171434)) ;
#55533 = CARTESIAN_POINT('Ctrl Pts',(181.085385117762,503.923920878122,-35.3507575774486)) ;
#55534 = CARTESIAN_POINT('Ctrl Pts',(181.122127294371,503.926257186113,-35.3769826974451)) ;
#55535 = CARTESIAN_POINT('Ctrl Pts',(181.157947462091,503.928637131266,-35.4044082453032)) ;
#55536 = CARTESIAN_POINT('Ctrl Pts',(181.192756181077,503.931080249462,-35.4329650866252)) ;
#55537 = CARTESIAN_POINT('Ctrl Pts',(181.192783048711,503.93108213522,-35.432987128653)) ;
#55538 = CARTESIAN_POINT('Ctrl Pts',(181.192809915743,503.931084021015,-35.4330091713548)) ;
#55539 = CARTESIAN_POINT('Ctrl Pts',(181.192836782173,503.931085906848,-35.4330312147305)) ;
#55540 = CARTESIAN_POINT('Ctrl Pts',(181.242591194344,503.93457831371,-35.4738537282965)) ;
#55541 = CARTESIAN_POINT('Ctrl Pts',(181.290459790534,503.938209109013,-35.5171450374117)) ;
#55542 = CARTESIAN_POINT('Ctrl Pts',(181.336212786875,503.9419132054,-35.5626840657719)) ;
#55543 = CARTESIAN_POINT('Ctrl Pts',(181.340850913989,503.942288701461,-35.5673005022697)) ;
#55544 = CARTESIAN_POINT('Ctrl Pts',(181.345467291612,503.942664950802,-35.5719399941601)) ;
#55545 = CARTESIAN_POINT('Ctrl Pts',(181.350061675335,503.943041885617,-35.5766022817505)) ;
#55546 = CARTESIAN_POINT('Ctrl Pts',(181.399900926299,503.947130823329,-35.62717814465)) ;
#55547 = CARTESIAN_POINT('Ctrl Pts',(181.447153620298,503.95129980935,-35.6804422720945)) ;
#55548 = CARTESIAN_POINT('Ctrl Pts',(181.491555882654,503.955474476342,-35.7360751787159)) ;
#55549 = CARTESIAN_POINT('Ctrl Pts',(181.535903285675,503.959643985501,-35.7916393504567)) ;
#55550 = CARTESIAN_POINT('Ctrl Pts',(181.577407628645,503.963818808005,-35.8495662641025)) ;
#55551 = CARTESIAN_POINT('Ctrl Pts',(181.615842287979,503.967944206143,-35.909520218889)) ;
#55552 = CARTESIAN_POINT('Ctrl Pts',(181.654251266563,503.972066847829,-35.9694341144542)) ;
#55553 = CARTESIAN_POINT('Ctrl Pts',(181.689594824856,503.976139962293,-36.0313722785607)) ;
#55554 = CARTESIAN_POINT('Ctrl Pts',(181.72167934075,503.980132110577,-36.0949840814907)) ;
#55555 = CARTESIAN_POINT('Ctrl Pts',(181.753753201391,503.98412293307,-36.1585747589726)) ;
#55556 = CARTESIAN_POINT('Ctrl Pts',(181.782570198983,503.98803280281,-36.2238379456552)) ;
#55557 = CARTESIAN_POINT('Ctrl Pts',(181.807968141192,503.991855024412,-36.290408340099)) ;
#55558 = CARTESIAN_POINT('Ctrl Pts',(181.833366183934,503.995677261144,-36.3569789980492)) ;
#55559 = CARTESIAN_POINT('Ctrl Pts',(181.855345035104,503.999411913746,-36.4248568749306)) ;
#55560 = CARTESIAN_POINT('Ctrl Pts',(181.873774463563,504.003076816851,-36.493661757878)) ;
#55561 = CARTESIAN_POINT('Ctrl Pts',(181.892222348924,504.006745390323,-36.5625355482753)) ;
#55562 = CARTESIAN_POINT('Ctrl Pts',(181.907113458668,504.010344252824,-36.6323382123433)) ;
#55563 = CARTESIAN_POINT('Ctrl Pts',(181.918351807264,504.013914080483,-36.7026733581213)) ;
#55564 = CARTESIAN_POINT('Ctrl Pts',(181.929596207887,504.017485830549,-36.7730463804734)) ;
#55565 = CARTESIAN_POINT('Ctrl Pts',(181.937183521265,504.021028852069,-36.8439524401983)) ;
#55566 = CARTESIAN_POINT('Ctrl Pts',(181.941056960413,504.024602862834,-36.9149794679936)) ;
#55567 = CARTESIAN_POINT('Ctrl Pts',(181.944725011961,504.027987363073,-36.9822403153598)) ;
#55568 = CARTESIAN_POINT('Ctrl Pts',(181.945062320629,504.031400143998,-37.0496099794262)) ;
#55569 = CARTESIAN_POINT('Ctrl Pts',(181.942059490689,504.034902425056,-37.1167253075522)) ;
#55570 = CARTESIAN_POINT('Ctrl Pts',(181.941885895529,504.035104893745,-37.1206052795714)) ;
#55571 = CARTESIAN_POINT('Ctrl Pts',(181.941701144205,504.035307661548,-37.124484414397)) ;
#55572 = CARTESIAN_POINT('Ctrl Pts',(181.941505237282,504.035510740295,-37.1283626466467)) ;
#55573 = CARTESIAN_POINT('Ctrl Pts',(181.939333039661,504.037762458423,-37.1713641228339)) ;
#55574 = CARTESIAN_POINT('Ctrl Pts',(181.935789371233,504.040052623498,-37.2142525851414)) ;
#55575 = CARTESIAN_POINT('Ctrl Pts',(181.930881811781,504.042398035777,-37.2569307975213)) ;
#55576 = CARTESIAN_POINT('Ctrl Pts',(181.930878006913,504.042399854193,-37.2569638862606)) ;
#55577 = CARTESIAN_POINT('Ctrl Pts',(181.930874201226,504.042401672642,-37.256996974874)) ;
#55578 = CARTESIAN_POINT('Ctrl Pts',(181.930870394719,504.042403491124,-37.2570300633614)) ;
#55579 = CARTESIAN_POINT('Ctrl Pts',(181.923473697062,504.04593711499,-37.3213266881243)) ;
#55580 = CARTESIAN_POINT('Ctrl Pts',(181.912949276553,504.049604849235,-37.3853667088768)) ;
#55581 = CARTESIAN_POINT('Ctrl Pts',(181.899360286837,504.053341749049,-37.4488337623104)) ;
#55582 = CARTESIAN_POINT('Ctrl Pts',(181.898033000868,504.053706745623,-37.4550328198782)) ;
#55583 = CARTESIAN_POINT('Ctrl Pts',(181.896676507989,504.054072402047,-37.4612263827437)) ;
#55584 = CARTESIAN_POINT('Ctrl Pts',(181.895290886591,504.054438657802,-37.4674141381045)) ;
#55585 = CARTESIAN_POINT('Ctrl Pts',(181.879824271438,504.058526886249,-37.5364832438183)) ;
#55586 = CARTESIAN_POINT('Ctrl Pts',(181.860724512427,504.062689049994,-37.6048325829169)) ;
#55587 = CARTESIAN_POINT('Ctrl Pts',(181.838116440668,504.066853554458,-37.6720746691617)) ;
#55588 = CARTESIAN_POINT('Ctrl Pts',(181.836915879813,504.067074702953,-37.6756454388162)) ;
#55589 = CARTESIAN_POINT('Ctrl Pts',(181.8357054331,504.067295858049,-37.6792130763627)) ;
#55590 = CARTESIAN_POINT('Ctrl Pts',(181.834485121803,504.067517009024,-37.6827775205824)) ;
#55591 = CARTESIAN_POINT('Ctrl Pts',(181.811409853763,504.071698825614,-37.7501787697255)) ;
#55592 = CARTESIAN_POINT('Ctrl Pts',(181.784805036596,504.075878961822,-37.8164423868943)) ;
#55593 = CARTESIAN_POINT('Ctrl Pts',(181.75483274324,504.080004965875,-37.8811963347265)) ;
#55594 = CARTESIAN_POINT('Ctrl Pts',(181.724880324253,504.084128234011,-37.9459073447735)) ;
#55595 = CARTESIAN_POINT('Ctrl Pts',(181.691565026174,504.088197283791,-38.0091107813048)) ;
#55596 = CARTESIAN_POINT('Ctrl Pts',(181.655079203746,504.092183056001,-38.0704541533036)) ;
#55597 = CARTESIAN_POINT('Ctrl Pts',(181.618603297701,504.096167744928,-38.1317808529541)) ;
#55598 = CARTESIAN_POINT('Ctrl Pts',(181.578958606656,504.100069169259,-38.1912484957397)) ;
#55599 = CARTESIAN_POINT('Ctrl Pts',(181.53636686296,504.103882968901,-38.2485230005513)) ;
#55600 = CARTESIAN_POINT('Ctrl Pts',(181.530063203674,504.104447418521,-38.2569997364823)) ;
#55601 = CARTESIAN_POINT('Ctrl Pts',(181.523695043267,504.105009992972,-38.2654284654114)) ;
#55602 = CARTESIAN_POINT('Ctrl Pts',(181.517263155791,504.105570724017,-38.2738081386943)) ;
#55603 = CARTESIAN_POINT('',(177.903353299729,503.710565160536,-36.4919899545742)) ;
#55604 = CARTESIAN_POINT('Ctrl Pts',(177.90335329973,503.710565160536,-36.4919899545744)) ;
#55605 = CARTESIAN_POINT('Ctrl Pts',(177.922086669525,503.714501737535,-36.4218445492966)) ;
#55606 = CARTESIAN_POINT('Ctrl Pts',(177.944559935843,503.718438314534,-36.3526262888013)) ;
#55607 = CARTESIAN_POINT('Ctrl Pts',(177.970658359158,503.722374891533,-36.2847491329925)) ;
#55608 = CARTESIAN_POINT('Ctrl Pts',(177.996735874362,503.72630831484,-36.2169263553011)) ;
#55609 = CARTESIAN_POINT('Ctrl Pts',(178.026432607287,503.730241738147,-36.150442974721)) ;
#55610 = CARTESIAN_POINT('Ctrl Pts',(178.059584450202,503.734175161454,-36.0856963847457)) ;
#55611 = CARTESIAN_POINT('Ctrl Pts',(178.092726426208,503.738107414065,-36.0209690651541)) ;
#55612 = CARTESIAN_POINT('Ctrl Pts',(178.129321265059,503.742039666676,-35.957977921458)) ;
#55613 = CARTESIAN_POINT('Ctrl Pts',(178.169157796928,503.745971919287,-35.8970979710654)) ;
#55614 = CARTESIAN_POINT('Ctrl Pts',(178.20898983709,503.749903728523,-35.8362248850971)) ;
#55615 = CARTESIAN_POINT('Ctrl Pts',(178.25206259196,503.753835537759,-35.7774629049249)) ;
#55616 = CARTESIAN_POINT('Ctrl Pts',(178.298121045655,503.757767346995,-35.7211588367889)) ;
#55617 = CARTESIAN_POINT('Ctrl Pts',(178.344187323935,503.761699824182,-35.664845203504)) ;
#55618 = CARTESIAN_POINT('Ctrl Pts',(178.39324001716,503.765632301368,-35.610990668463)) ;
#55619 = CARTESIAN_POINT('Ctrl Pts',(178.444984140575,503.769564778555,-35.5599085621139)) ;
#55620 = CARTESIAN_POINT('Ctrl Pts',(178.496751681291,503.773499035422,-35.5088033380654)) ;
#55621 = CARTESIAN_POINT('Ctrl Pts',(178.551212744977,503.777433292289,-35.4604733594333)) ;
#55622 = CARTESIAN_POINT('Ctrl Pts',(178.608036897457,503.781367549156,-35.4151937570061)) ;
#55623 = CARTESIAN_POINT('Ctrl Pts',(178.664945234505,503.785307634596,-35.3698470731778)) ;
#55624 = CARTESIAN_POINT('Ctrl Pts',(178.724223287277,503.789247720036,-35.3275600731401)) ;
#55625 = CARTESIAN_POINT('Ctrl Pts',(178.785509441009,503.793187805476,-35.2885660879564)) ;
#55626 = CARTESIAN_POINT('Ctrl Pts',(178.846846634949,503.79713117229,-35.2495396278827)) ;
#55627 = CARTESIAN_POINT('Ctrl Pts',(178.910194859628,503.801074539104,-35.213811870712)) ;
#55628 = CARTESIAN_POINT('Ctrl Pts',(178.975167853069,503.805017905918,-35.1815701878734)) ;
#55629 = CARTESIAN_POINT('Ctrl Pts',(179.04026464019,503.808968786067,-35.1492670746407)) ;
#55630 = CARTESIAN_POINT('Ctrl Pts',(179.106991954837,503.812919666216,-35.1204634808391)) ;
#55631 = CARTESIAN_POINT('Ctrl Pts',(179.174943925636,503.816870546365,-35.0952985093853)) ;
#55632 = CARTESIAN_POINT('Ctrl Pts',(179.203132609039,503.818509499708,-35.0848592622994)) ;
#55633 = CARTESIAN_POINT('Ctrl Pts',(179.231531870175,503.820148453051,-35.0750455736566)) ;
#55634 = CARTESIAN_POINT('Ctrl Pts',(179.260112136805,503.821787406393,-35.0658648115978)) ;
#55635 = CARTESIAN_POINT('Ctrl Pts',(179.339468635472,503.826338154658,-35.0403733373046)) ;
#55636 = CARTESIAN_POINT('Ctrl Pts',(179.420464141971,503.830888902922,-35.0196867084889)) ;
#55637 = CARTESIAN_POINT('Ctrl Pts',(179.502557616501,503.835439651186,-35.0039865630905)) ;
#55638 = CARTESIAN_POINT('Ctrl Pts',(179.583771084385,503.839941617392,-34.9884547164807)) ;
#55639 = CARTESIAN_POINT('Ctrl Pts',(179.666058990972,503.844443583597,-34.9778031051609)) ;
#55640 = CARTESIAN_POINT('Ctrl Pts',(179.748876364633,503.848945549802,-34.9721613698416)) ;
#55641 = CARTESIAN_POINT('Ctrl Pts',(179.795135818443,503.851460221404,-34.969010055294)) ;
#55642 = CARTESIAN_POINT('Ctrl Pts',(179.841560097023,503.853974893007,-34.9674209995305)) ;
#55643 = CARTESIAN_POINT('Ctrl Pts',(179.888051515576,503.856489564609,-34.9674102269198)) ;
#55644 = CARTESIAN_POINT('',(177.901969296448,503.711777422211,-37.5551703732902)) ;
#55645 = CARTESIAN_POINT('Origin',(179.888527625402,503.710565160536,-37.0221601717597)) ;
#55646 = CARTESIAN_POINT('Ctrl Pts',(177.903947533684,503.712975317057,-37.5545504628579)) ;
#55647 = CARTESIAN_POINT('Ctrl Pts',(177.895757318976,503.714684508975,-37.5240199717342)) ;
#55648 = CARTESIAN_POINT('Ctrl Pts',(177.888272211867,503.716353732618,-37.4933026915394)) ;
#55649 = CARTESIAN_POINT('Ctrl Pts',(177.843255876735,503.727245875368,-37.2880864789864)) ;
#55650 = CARTESIAN_POINT('Ctrl Pts',(177.827886420719,503.735545865294,-37.1094919839223)) ;
#55651 = CARTESIAN_POINT('Ctrl Pts',(177.838765269825,503.747636894902,-36.8641427975573)) ;
#55652 = CARTESIAN_POINT('Ctrl Pts',(177.845014145554,503.750992058744,-36.7973337620819)) ;
#55653 = CARTESIAN_POINT('Ctrl Pts',(177.862161052059,503.757215308265,-36.6775667803755)) ;
#55654 = CARTESIAN_POINT('Ctrl Pts',(177.871902648708,503.760047275435,-36.6245056818421)) ;
#55655 = CARTESIAN_POINT('Ctrl Pts',(177.895145194004,503.765750615555,-36.5210187901725)) ;
#55656 = CARTESIAN_POINT('Ctrl Pts',(177.908502449703,503.768615418516,-36.4706025512604)) ;
#55657 = CARTESIAN_POINT('Ctrl Pts',(177.975574149277,503.781473142358,-36.2514832390895)) ;
#55658 = CARTESIAN_POINT('Ctrl Pts',(178.049037690473,503.792136946426,-36.0896420780475)) ;
#55659 = CARTESIAN_POINT('Ctrl Pts',(178.185397305171,503.807602824018,-35.8697578075168)) ;
#55660 = CARTESIAN_POINT('Ctrl Pts',(178.232606658886,503.812442541399,-35.8028931647587)) ;
#55661 = CARTESIAN_POINT('Ctrl Pts',(178.303541268729,503.818884373362,-35.7141741542682)) ;
#55662 = CARTESIAN_POINT('Ctrl Pts',(178.32397899941,503.820656440321,-35.6897949466128)) ;
#55663 = CARTESIAN_POINT('Ctrl Pts',(178.366968887714,503.824199102932,-35.6408684796157)) ;
#55664 = CARTESIAN_POINT('Ctrl Pts',(178.389568592076,503.825965686983,-35.6163757531014)) ;
#55665 = CARTESIAN_POINT('Ctrl Pts',(178.504372626142,503.834541364303,-35.4978736541451)) ;
#55666 = CARTESIAN_POINT('Ctrl Pts',(178.604877938666,503.840838577507,-35.4123199716945)) ;
#55667 = CARTESIAN_POINT('Ctrl Pts',(178.781952523299,503.85128445912,-35.28878769492)) ;
#55668 = CARTESIAN_POINT('Ctrl Pts',(178.853909444624,503.855376072505,-35.2449002551313)) ;
#55669 = CARTESIAN_POINT('Ctrl Pts',(178.987124614945,503.862923219619,-35.1744888603364)) ;
#55670 = CARTESIAN_POINT('Ctrl Pts',(179.047364616602,503.866325870217,-35.1462976245517)) ;
#55671 = CARTESIAN_POINT('Ctrl Pts',(179.154683211678,503.872440948625,-35.1022844643679)) ;
#55672 = CARTESIAN_POINT('Ctrl Pts',(179.201166385959,503.875105718216,-35.0851562241228)) ;
#55673 = CARTESIAN_POINT('Ctrl Pts',(179.308922577701,503.881338604638,-35.0498172445049)) ;
#55674 = CARTESIAN_POINT('Ctrl Pts',(179.370514853924,503.884941773821,-35.0327531875673)) ;
#55675 = CARTESIAN_POINT('Ctrl Pts',(179.575985296009,503.897092887691,-34.9860171575838)) ;
#55676 = CARTESIAN_POINT('Ctrl Pts',(179.722241991841,503.905985140548,-34.9688940738769)) ;
#55677 = CARTESIAN_POINT('Ctrl Pts',(179.945711503131,503.919331392535,-34.9667758221378)) ;
#55678 = CARTESIAN_POINT('Ctrl Pts',(180.022358683162,503.92385672602,-34.9703400004801)) ;
#55679 = CARTESIAN_POINT('Ctrl Pts',(180.129951961443,503.929985952611,-34.981399747356)) ;
#55680 = CARTESIAN_POINT('Ctrl Pts',(180.161195612573,503.931738654782,-34.985338797295)) ;
#55681 = CARTESIAN_POINT('Ctrl Pts',(180.225345320032,503.935264138454,-34.9949292578328)) ;
#55682 = CARTESIAN_POINT('Ctrl Pts',(180.258228797664,503.937031953938,-35.0006674890449)) ;
#55683 = CARTESIAN_POINT('Ctrl Pts',(180.398909995285,503.944480758777,-35.0287647137643)) ;
#55684 = CARTESIAN_POINT('Ctrl Pts',(180.504964254677,503.949812065802,-35.0589672768675)) ;
#55685 = CARTESIAN_POINT('Ctrl Pts',(180.734904791795,503.96167731295,-35.1449357705221)) ;
#55686 = CARTESIAN_POINT('Ctrl Pts',(180.856706846891,503.968192899056,-35.2047577744652)) ;
#55687 = CARTESIAN_POINT('Ctrl Pts',(181.018162071795,503.977916870129,-35.3049216227501)) ;
#55688 = CARTESIAN_POINT('Ctrl Pts',(181.063415632662,503.980771990906,-35.3355601434682)) ;
#55689 = CARTESIAN_POINT('Ctrl Pts',(181.14791631304,503.98639316946,-35.3978229287159)) ;
#55690 = CARTESIAN_POINT('Ctrl Pts',(181.187326581644,503.989146561038,-35.4291592364038)) ;
#55691 = CARTESIAN_POINT('Ctrl Pts',(181.290653110701,503.996747493691,-35.5177022235187)) ;
#55692 = CARTESIAN_POINT('Ctrl Pts',(181.352198477477,504.001701434117,-35.5775099068324)) ;
#55693 = CARTESIAN_POINT('Ctrl Pts',(181.50888619033,504.015475938451,-35.7500931092957)) ;
#55694 = CARTESIAN_POINT('Ctrl Pts',(181.595916942229,504.024501712009,-35.8695390577769)) ;
#55695 = CARTESIAN_POINT('Ctrl Pts',(181.693611264494,504.035990679966,-36.0392957004221)) ;
#55696 = CARTESIAN_POINT('Ctrl Pts',(181.716307480542,504.038786800327,-36.0821755785117)) ;
#55697 = CARTESIAN_POINT('Ctrl Pts',(181.750047002402,504.043112868775,-36.1517723911939)) ;
#55698 = CARTESIAN_POINT('Ctrl Pts',(181.762080021379,504.044694575938,-36.177985425348)) ;
#55699 = CARTESIAN_POINT('Ctrl Pts',(181.789687483722,504.048417407049,-36.2416275199888)) ;
#55700 = CARTESIAN_POINT('Ctrl Pts',(181.804713438876,504.05052876669,-36.2792790178148)) ;
#55701 = CARTESIAN_POINT('Ctrl Pts',(181.856432654011,504.058221709834,-36.4209101990515)) ;
#55702 = CARTESIAN_POINT('Ctrl Pts',(181.885855751607,504.063520368856,-36.527351265362)) ;
#55703 = CARTESIAN_POINT('Ctrl Pts',(181.930309792158,504.074954462313,-36.7594548453065)) ;
#55704 = CARTESIAN_POINT('Ctrl Pts',(181.942577323793,504.081086582172,-36.8851760842744)) ;
#55705 = CARTESIAN_POINT('Ctrl Pts',(181.943529751982,504.090301579191,-37.0640377043029)) ;
#55706 = CARTESIAN_POINT('Ctrl Pts',(181.94177426379,504.09307953441,-37.1168440458725)) ;
#55707 = CARTESIAN_POINT('Ctrl Pts',(181.93426333949,504.098718328245,-37.2213040161704)) ;
#55708 = CARTESIAN_POINT('Ctrl Pts',(181.928579104961,504.101574859447,-37.2729233005051)) ;
#55709 = CARTESIAN_POINT('Ctrl Pts',(181.905379487788,504.110441702532,-37.4289973928072)) ;
#55710 = CARTESIAN_POINT('Ctrl Pts',(181.881742716806,504.116639518345,-37.5323528521412)) ;
#55711 = CARTESIAN_POINT('Ctrl Pts',(181.805672544406,504.1319099548,-37.7764875068448)) ;
#55712 = CARTESIAN_POINT('Ctrl Pts',(181.745574868745,504.141078223086,-37.9142545955288)) ;
#55713 = CARTESIAN_POINT('Ctrl Pts',(181.654336389126,504.151553830523,-38.0733703472624)) ;
#55714 = CARTESIAN_POINT('Ctrl Pts',(181.636933944431,504.153436387901,-38.1020671416748)) ;
#55715 = CARTESIAN_POINT('Ctrl Pts',(181.604570192788,504.156721147625,-38.1526003889469)) ;
#55716 = CARTESIAN_POINT('Ctrl Pts',(181.58987603404,504.158139461567,-38.1745970845128)) ;
#55717 = CARTESIAN_POINT('Ctrl Pts',(181.556362419459,504.16123077008,-38.2227272559929)) ;
#55718 = CARTESIAN_POINT('Ctrl Pts',(181.537344535028,504.162891887699,-38.2487151965558)) ;
#55719 = CARTESIAN_POINT('Ctrl Pts',(181.517722816555,504.164527114775,-38.2742466670251)) ;
#55720 = CARTESIAN_POINT('Origin',(29.8885276254015,502.164639880024,-37.0221601717529)) ;
#55721 = CARTESIAN_POINT('',(31.5177152522353,505.503079332004,-38.2742565095294)) ;
#55722 = CARTESIAN_POINT('',(31.517715239327,505.561197820373,-38.2742565263254)) ;
#55723 = CARTESIAN_POINT('',(31.5177152522233,502.164639880024,-38.2742565095444)) ;
#55724 = CARTESIAN_POINT('',(29.0652954452959,505.710565160562,-38.9047876814153)) ;
#55725 = CARTESIAN_POINT('Ctrl Pts',(31.517715239327,505.561197820373,-38.2742565263254)) ;
#55726 = CARTESIAN_POINT('Ctrl Pts',(31.5075491635084,505.562168759122,-38.2874842980902)) ;
#55727 = CARTESIAN_POINT('Ctrl Pts',(31.4972210708087,505.563144379345,-38.3005894529987)) ;
#55728 = CARTESIAN_POINT('Ctrl Pts',(31.4015822254585,505.57207825581,-38.4189489716371)) ;
#55729 = CARTESIAN_POINT('Ctrl Pts',(31.3062234691222,505.580301471493,-38.5156423553119)) ;
#55730 = CARTESIAN_POINT('Ctrl Pts',(31.1611448810046,505.59137763975,-38.636245616164)) ;
#55731 = CARTESIAN_POINT('Ctrl Pts',(31.1189359034847,505.594450738869,-38.6686482014559)) ;
#55732 = CARTESIAN_POINT('Ctrl Pts',(31.0511435592626,505.599100143542,-38.7166256158861)) ;
#55733 = CARTESIAN_POINT('Ctrl Pts',(31.0263991082161,505.600739734931,-38.7333404097893)) ;
#55734 = CARTESIAN_POINT('Ctrl Pts',(30.9670432512362,505.604531093695,-38.7715776913673)) ;
#55735 = CARTESIAN_POINT('Ctrl Pts',(30.9321403781093,505.606655089118,-38.7926207042398)) ;
#55736 = CARTESIAN_POINT('Ctrl Pts',(30.8014997273251,505.614306047177,-38.866177211694)) ;
#55737 = CARTESIAN_POINT('Ctrl Pts',(30.7022411842305,505.61955169095,-38.9120784274336)) ;
#55738 = CARTESIAN_POINT('Ctrl Pts',(30.4737700196624,505.63127542291,-38.9963775917003)) ;
#55739 = CARTESIAN_POINT('Ctrl Pts',(30.3434963493631,505.637745073186,-39.0304039139251)) ;
#55740 = CARTESIAN_POINT('Ctrl Pts',(30.1521214543254,505.647634681118,-39.0607995658369)) ;
#55741 = CARTESIAN_POINT('Ctrl Pts',(30.0930310772155,505.650735445744,-39.0675720472511)) ;
#55742 = CARTESIAN_POINT('Ctrl Pts',(29.9778760565012,505.656907225942,-39.0757302690794)) ;
#55743 = CARTESIAN_POINT('Ctrl Pts',(29.9218840845969,505.659966780814,-39.0774022115405)) ;
#55744 = CARTESIAN_POINT('Ctrl Pts',(29.7389595994745,505.670169006103,-39.0753873946209)) ;
#55745 = CARTESIAN_POINT('Ctrl Pts',(29.6124387002168,505.677569456498,-39.0622289706628)) ;
#55746 = CARTESIAN_POINT('Ctrl Pts',(29.3834454037262,505.691317622877,-39.0167136061039)) ;
#55747 = CARTESIAN_POINT('Ctrl Pts',(29.2807041840142,505.697616119117,-38.987841832375)) ;
#55748 = CARTESIAN_POINT('Ctrl Pts',(29.159114743818,505.704960070217,-38.9432226974015)) ;
#55749 = CARTESIAN_POINT('Ctrl Pts',(29.1377005136105,505.706248825033,-38.9349547506654)) ;
#55750 = CARTESIAN_POINT('Ctrl Pts',(29.0992885979274,505.708547178493,-38.9193795582333)) ;
#55751 = CARTESIAN_POINT('Ctrl Pts',(29.0822426517464,505.709562273817,-38.9121983272501)) ;
#55752 = CARTESIAN_POINT('Ctrl Pts',(29.0652954452959,505.710565160562,-38.9047876814153)) ;
#55753 = CARTESIAN_POINT('',(28.2343942282376,505.709323904328,-38.2446969949844)) ;
#55754 = CARTESIAN_POINT('Origin',(29.8885276254021,505.710565160562,-37.0221601717529)) ;
#55755 = CARTESIAN_POINT('Ctrl Pts',(28.2362648420351,505.708082648095,-38.2436450292932)) ;
#55756 = CARTESIAN_POINT('Ctrl Pts',(28.2461072735545,505.707189028891,-38.2569585658441)) ;
#55757 = CARTESIAN_POINT('Ctrl Pts',(28.2561106100166,505.706306272621,-38.2701531255639)) ;
#55758 = CARTESIAN_POINT('Ctrl Pts',(28.2797687895217,505.704273173126,-38.3005873852562)) ;
#55759 = CARTESIAN_POINT('Ctrl Pts',(28.2935432205994,505.703130197476,-38.3177318410642)) ;
#55760 = CARTESIAN_POINT('Ctrl Pts',(28.3874565500433,505.695579706726,-38.4308533050305)) ;
#55761 = CARTESIAN_POINT('Ctrl Pts',(28.4759436690462,505.689601034009,-38.5195722420282)) ;
#55762 = CARTESIAN_POINT('Ctrl Pts',(28.6616888882861,505.677871318706,-38.6745901535631)) ;
#55763 = CARTESIAN_POINT('Ctrl Pts',(28.7576429151489,505.672149633239,-38.7416817700842)) ;
#55764 = CARTESIAN_POINT('Ctrl Pts',(28.9046092534273,505.663388774374,-38.8267953063175)) ;
#55765 = CARTESIAN_POINT('Ctrl Pts',(28.9514528702694,505.660599470974,-38.8515572194649)) ;
#55766 = CARTESIAN_POINT('Ctrl Pts',(29.046854653936,505.654895369001,-38.8973611838619)) ;
#55767 = CARTESIAN_POINT('Ctrl Pts',(29.0953728605494,505.651982990702,-38.9183924936482)) ;
#55768 = CARTESIAN_POINT('Ctrl Pts',(29.2471311335853,505.642823163637,-38.9773317225558)) ;
#55769 = CARTESIAN_POINT('Ctrl Pts',(29.3526338881399,505.636374314102,-39.0088402662777)) ;
#55770 = CARTESIAN_POINT('Ctrl Pts',(29.5540611870938,505.624077896448,-39.0517789010217)) ;
#55771 = CARTESIAN_POINT('Ctrl Pts',(29.6492724358515,505.618275709019,-39.0651915525782)) ;
#55772 = CARTESIAN_POINT('Ctrl Pts',(29.7864911376515,505.610158775639,-39.0747950590716)) ;
#55773 = CARTESIAN_POINT('Ctrl Pts',(29.827989899536,505.607736916038,-39.076437897636)) ;
#55774 = CARTESIAN_POINT('Ctrl Pts',(29.9039863067478,505.603393910383,-39.0771412359856)) ;
#55775 = CARTESIAN_POINT('Ctrl Pts',(29.9384655742036,505.601458246651,-39.0765926141257)) ;
#55776 = CARTESIAN_POINT('Ctrl Pts',(30.0039453381849,505.597869070187,-39.0739010684627)) ;
#55777 = CARTESIAN_POINT('Ctrl Pts',(30.0349411926149,505.596208888362,-39.0719223766892)) ;
#55778 = CARTESIAN_POINT('Ctrl Pts',(30.1377728071355,505.590798020501,-39.0630133279018)) ;
#55779 = CARTESIAN_POINT('Ctrl Pts',(30.2092929813512,505.587190485173,-39.0530014143618)) ;
#55780 = CARTESIAN_POINT('Ctrl Pts',(30.4436935426478,505.575472247853,-39.0074927039831)) ;
#55781 = CARTESIAN_POINT('Ctrl Pts',(30.6027687905733,505.567637529545,-38.9559686275298)) ;
#55782 = CARTESIAN_POINT('Ctrl Pts',(30.8080671253967,505.556169459069,-38.8606415929312)) ;
#55783 = CARTESIAN_POINT('Ctrl Pts',(30.8611267158057,505.55307722102,-38.8331314403171)) ;
#55784 = CARTESIAN_POINT('Ctrl Pts',(30.9560853312287,505.547254960259,-38.7785197094462)) ;
#55785 = CARTESIAN_POINT('Ctrl Pts',(30.9983410067869,505.544552403246,-38.7521289382581)) ;
#55786 = CARTESIAN_POINT('Ctrl Pts',(31.0999911331131,505.537752606351,-38.6833855875682)) ;
#55787 = CARTESIAN_POINT('Ctrl Pts',(31.1581656446523,505.533593522434,-38.6393587383011)) ;
#55788 = CARTESIAN_POINT('Ctrl Pts',(31.3262527658227,505.520759757052,-38.4974807879345)) ;
#55789 = CARTESIAN_POINT('Ctrl Pts',(31.4281137130496,505.511800710465,-38.3908431607179)) ;
#55790 = CARTESIAN_POINT('Ctrl Pts',(31.5177152522354,505.503079332004,-38.2742565095294)) ;
#55791 = CARTESIAN_POINT('Origin',(29.8885276254015,502.164639880024,-37.0221601717529)) ;
#55792 = CARTESIAN_POINT('',(31.5177152522275,504.803366924184,-38.2742565095395)) ;
#55793 = CARTESIAN_POINT('',(31.5177151883675,504.861461047188,-38.2742565926321)) ;
#55794 = CARTESIAN_POINT('',(31.5177152522233,502.164639880024,-38.2742565095444)) ;
#55795 = CARTESIAN_POINT('',(29.8879422111462,505.313162079696,-34.9674106910863)) ;
#55796 = CARTESIAN_POINT('Ctrl Pts',(31.5177151883675,504.861461047188,-38.2742565926321)) ;
#55797 = CARTESIAN_POINT('Ctrl Pts',(31.4981288392375,504.863080078642,-38.2997417197153)) ;
#55798 = CARTESIAN_POINT('Ctrl Pts',(31.4779403354198,504.864717676193,-38.3247726904712)) ;
#55799 = CARTESIAN_POINT('Ctrl Pts',(31.4229841836044,504.869108417019,-38.389727759927)) ;
#55800 = CARTESIAN_POINT('Ctrl Pts',(31.3872577899705,504.871896629293,-38.428789209312)) ;
#55801 = CARTESIAN_POINT('Ctrl Pts',(31.3127084554957,504.877617517573,-38.504230083968)) ;
#55802 = CARTESIAN_POINT('Ctrl Pts',(31.2739013978775,504.880548583038,-38.5405675691751)) ;
#55803 = CARTESIAN_POINT('Ctrl Pts',(31.1114993158224,504.892653281833,-38.6812218976206)) ;
#55804 = CARTESIAN_POINT('Ctrl Pts',(30.977213607994,504.902365127006,-38.7722722982688)) ;
#55805 = CARTESIAN_POINT('Ctrl Pts',(30.775739907595,504.915998408535,-38.8766437564329)) ;
#55806 = CARTESIAN_POINT('Ctrl Pts',(30.7164040375659,504.919902391153,-38.9038818298611)) ;
#55807 = CARTESIAN_POINT('Ctrl Pts',(30.6131208359359,504.926410452218,-38.9454609649906)) ;
#55808 = CARTESIAN_POINT('Ctrl Pts',(30.5698010780222,504.929057339692,-38.9612291199981)) ;
#55809 = CARTESIAN_POINT('Ctrl Pts',(30.4982885612648,504.93325235498,-38.9845663290332)) ;
#55810 = CARTESIAN_POINT('Ctrl Pts',(30.4704044295927,504.934843976556,-38.9930142893482)) ;
#55811 = CARTESIAN_POINT('Ctrl Pts',(30.4000362826776,504.938751291701,-39.0127095219153)) ;
#55812 = CARTESIAN_POINT('Ctrl Pts',(30.3573554881974,504.941027422794,-39.0231921079112)) ;
#55813 = CARTESIAN_POINT('Ctrl Pts',(30.174725418928,504.950495875648,-39.0618816537634)) ;
#55814 = CARTESIAN_POINT('Ctrl Pts',(30.0323705460408,504.957231637499,-39.0768349300546)) ;
#55815 = CARTESIAN_POINT('Ctrl Pts',(29.7942445336737,504.968856210848,-39.0769599584486)) ;
#55816 = CARTESIAN_POINT('Ctrl Pts',(29.6990022579582,504.973596036018,-39.070371367097)) ;
#55817 = CARTESIAN_POINT('Ctrl Pts',(29.5532879585618,504.98122573199,-39.0500390639636)) ;
#55818 = CARTESIAN_POINT('Ctrl Pts',(29.5022999535718,504.983966801187,-39.0409484153902)) ;
#55819 = CARTESIAN_POINT('Ctrl Pts',(29.3981895478093,504.989737809555,-39.0182980496468)) ;
#55820 = CARTESIAN_POINT('Ctrl Pts',(29.3451578055391,504.992773019505,-39.0045189385599)) ;
#55821 = CARTESIAN_POINT('Ctrl Pts',(29.2285873250816,504.999669504526,-38.9692015513979)) ;
#55822 = CARTESIAN_POINT('Ctrl Pts',(29.1654263786983,505.003560027214,-38.9466379259184)) ;
#55823 = CARTESIAN_POINT('Ctrl Pts',(28.9701919727207,505.016033904202,-38.8659229178025)) ;
#55824 = CARTESIAN_POINT('Ctrl Pts',(28.8430800448016,505.024855683166,-38.796938435276)) ;
#55825 = CARTESIAN_POINT('Ctrl Pts',(28.6823138706657,505.036331665862,-38.6863823069992)) ;
#55826 = CARTESIAN_POINT('Ctrl Pts',(28.6414674940954,505.039274614431,-38.6559988319908)) ;
#55827 = CARTESIAN_POINT('Ctrl Pts',(28.5788053219365,505.043780856716,-38.6056670649222)) ;
#55828 = CARTESIAN_POINT('Ctrl Pts',(28.5562210606389,505.045401832638,-38.5867131976417)) ;
#55829 = CARTESIAN_POINT('Ctrl Pts',(28.5040213635981,505.049134190153,-38.5409539373917)) ;
#55830 = CARTESIAN_POINT('Ctrl Pts',(28.4747655129482,505.051219069491,-38.5137597226582)) ;
#55831 = CARTESIAN_POINT('Ctrl Pts',(28.367434140807,505.058924077578,-38.4079947538045)) ;
#55832 = CARTESIAN_POINT('Ctrl Pts',(28.2949566488903,505.064252121472,-38.3240043771201)) ;
#55833 = CARTESIAN_POINT('Ctrl Pts',(28.1545170054817,505.075773328517,-38.1318429710699)) ;
#55834 = CARTESIAN_POINT('Ctrl Pts',(28.0891451551578,505.081962757305,-38.022364013775)) ;
#55835 = CARTESIAN_POINT('Ctrl Pts',(28.0113738670124,505.091266539733,-37.8594937474548)) ;
#55836 = CARTESIAN_POINT('Ctrl Pts',(27.9903045640372,505.094069474289,-37.8105650598151)) ;
#55837 = CARTESIAN_POINT('Ctrl Pts',(27.952160217412,505.099787195104,-37.7115598519733)) ;
#55838 = CARTESIAN_POINT('Ctrl Pts',(27.9350710232107,505.102698793676,-37.6615326971442)) ;
#55839 = CARTESIAN_POINT('Ctrl Pts',(27.8867640559,505.112187590116,-37.5000078895508)) ;
#55840 = CARTESIAN_POINT('Ctrl Pts',(27.8630323962951,505.118999437547,-37.3865206407382)) ;
#55841 = CARTESIAN_POINT('Ctrl Pts',(27.8326085890627,505.134013313537,-37.1378134512963)) ;
#55842 = CARTESIAN_POINT('Ctrl Pts',(27.8294495923459,505.142226304971,-37.0026827339092)) ;
#55843 = CARTESIAN_POINT('Ctrl Pts',(27.8421989123527,505.151984546786,-36.8329942994246)) ;
#55844 = CARTESIAN_POINT('Ctrl Pts',(27.8457528177593,505.153973832392,-36.7978471027659)) ;
#55845 = CARTESIAN_POINT('Ctrl Pts',(27.8540837367395,505.157597892617,-36.7323725571569)) ;
#55846 = CARTESIAN_POINT('Ctrl Pts',(27.8586372679264,505.159242400686,-36.7020289675269)) ;
#55847 = CARTESIAN_POINT('Ctrl Pts',(27.875234421428,505.164357693097,-36.6061180427956)) ;
#55848 = CARTESIAN_POINT('Ctrl Pts',(27.8897904153988,505.167707933541,-36.5410243868138)) ;
#55849 = CARTESIAN_POINT('Ctrl Pts',(27.9434616400019,505.177671969424,-36.3460800042188)) ;
#55850 = CARTESIAN_POINT('Ctrl Pts',(27.9922763839509,505.184077751913,-36.2192909156471)) ;
#55851 = CARTESIAN_POINT('Ctrl Pts',(28.0879134531826,505.194594048104,-36.0293164469265)) ;
#55852 = CARTESIAN_POINT('Ctrl Pts',(28.1264562467776,505.198490804028,-35.9624182742105)) ;
#55853 = CARTESIAN_POINT('Ctrl Pts',(28.1961091597132,505.205145417817,-35.8558700498401)) ;
#55854 = CARTESIAN_POINT('Ctrl Pts',(28.2250777124948,505.207821638959,-35.8149126029029)) ;
#55855 = CARTESIAN_POINT('Ctrl Pts',(28.2907357308412,505.213723078796,-35.7289369255706)) ;
#55856 = CARTESIAN_POINT('Ctrl Pts',(28.3278927579695,505.21696604294,-35.6843324016277)) ;
#55857 = CARTESIAN_POINT('Ctrl Pts',(28.4114477775995,505.224068857127,-35.5922545232644)) ;
#55858 = CARTESIAN_POINT('Ctrl Pts',(28.4583584232185,505.227946905042,-35.5453359090442)) ;
#55859 = CARTESIAN_POINT('Ctrl Pts',(28.6090525556392,505.2400312187,-35.4085399603043)) ;
#55860 = CARTESIAN_POINT('Ctrl Pts',(28.7196318187401,505.248423732633,-35.3267228092832)) ;
#55861 = CARTESIAN_POINT('Ctrl Pts',(28.8802171211402,505.259404735925,-35.2311341015567)) ;
#55862 = CARTESIAN_POINT('Ctrl Pts',(28.9238066828535,505.26227305394,-35.2072831153994)) ;
#55863 = CARTESIAN_POINT('Ctrl Pts',(28.9944447630443,505.266696358429,-35.1718970397575)) ;
#55864 = CARTESIAN_POINT('Ctrl Pts',(29.020946590006,505.268305835211,-35.1593232858362)) ;
#55865 = CARTESIAN_POINT('Ctrl Pts',(29.0857306034042,505.272117860183,-35.1302694469521)) ;
#55866 = CARTESIAN_POINT('Ctrl Pts',(29.1242604351063,505.274288569587,-35.1143788115343)) ;
#55867 = CARTESIAN_POINT('Ctrl Pts',(29.2674528017067,505.282097454294,-35.0603580956463)) ;
#55868 = CARTESIAN_POINT('Ctrl Pts',(29.3746877541625,505.287456545371,-35.0295805341481)) ;
#55869 = CARTESIAN_POINT('Ctrl Pts',(29.5710591498126,505.297175520829,-34.9901376900022)) ;
#55870 = CARTESIAN_POINT('Ctrl Pts',(29.6592638939451,505.301507515347,-34.9783063252283)) ;
#55871 = CARTESIAN_POINT('Ctrl Pts',(29.7945505680441,505.308336201423,-34.9690290583049)) ;
#55872 = CARTESIAN_POINT('Ctrl Pts',(29.841239982547,505.310725012016,-34.9674235888564)) ;
#55873 = CARTESIAN_POINT('Ctrl Pts',(29.8879409844869,505.313161259658,-34.9674102554973)) ;
#55874 = CARTESIAN_POINT('Ctrl Pts',(29.887942250361,505.313161325695,-34.9674102551363)) ;
#55875 = CARTESIAN_POINT('Ctrl Pts',(29.931406367057,505.315428715769,-34.9673978727004)) ;
#55876 = CARTESIAN_POINT('Ctrl Pts',(29.9748581011214,505.317735983423,-34.9687645769083)) ;
#55877 = CARTESIAN_POINT('Ctrl Pts',(30.0700919010336,505.322898407409,-34.9747881630337)) ;
#55878 = CARTESIAN_POINT('Ctrl Pts',(30.1218045219554,505.325770716653,-34.9800340927953)) ;
#55879 = CARTESIAN_POINT('Ctrl Pts',(30.334287187648,505.337878376111,-35.0097652070976)) ;
#55880 = CARTESIAN_POINT('Ctrl Pts',(30.4920496847355,505.34765765226,-35.0513278068641)) ;
#55881 = CARTESIAN_POINT('Ctrl Pts',(30.7304100775754,505.363062359331,-35.1454566553703)) ;
#55882 = CARTESIAN_POINT('Ctrl Pts',(30.8151350119253,505.368659702266,-35.1858094976814)) ;
#55883 = CARTESIAN_POINT('Ctrl Pts',(30.9251968312958,505.375848723428,-35.2477939194235)) ;
#55884 = CARTESIAN_POINT('Ctrl Pts',(30.9531977633756,505.377669473963,-35.2644524325701)) ;
#55885 = CARTESIAN_POINT('Ctrl Pts',(31.0091429552209,505.381271848921,-35.2995635466388)) ;
#55886 = CARTESIAN_POINT('Ctrl Pts',(31.0370557630183,505.383051193532,-35.3180471310376)) ;
#55887 = CARTESIAN_POINT('Ctrl Pts',(31.1712081834549,505.391577547857,-35.4116759925704)) ;
#55888 = CARTESIAN_POINT('Ctrl Pts',(31.2706067671416,505.397828971673,-35.4961217616894)) ;
#55889 = CARTESIAN_POINT('Ctrl Pts',(31.4448329300348,505.40997006538,-35.6752217409588)) ;
#55890 = CARTESIAN_POINT('Ctrl Pts',(31.5206448004573,505.415828566778,-35.7681587730373)) ;
#55891 = CARTESIAN_POINT('Ctrl Pts',(31.6180757464789,505.424775114195,-35.9115131174265)) ;
#55892 = CARTESIAN_POINT('Ctrl Pts',(31.6464709333382,505.427600924226,-35.9570272181227)) ;
#55893 = CARTESIAN_POINT('Ctrl Pts',(31.6995891429412,505.43338203227,-36.0500904320883)) ;
#55894 = CARTESIAN_POINT('Ctrl Pts',(31.7242972324535,505.43633484725,-36.0975994165408)) ;
#55895 = CARTESIAN_POINT('Ctrl Pts',(31.7950878352657,505.445690767992,-36.2477698231289)) ;
#55896 = CARTESIAN_POINT('Ctrl Pts',(31.8346116503925,505.452307999899,-36.3532779626431)) ;
#55897 = CARTESIAN_POINT('Ctrl Pts',(31.8915375668637,505.464802920524,-36.5539789154328)) ;
#55898 = CARTESIAN_POINT('Ctrl Pts',(31.9112492784356,505.470629418937,-36.6482083690304)) ;
#55899 = CARTESIAN_POINT('Ctrl Pts',(31.9320235603767,505.479690610628,-36.7999605742402)) ;
#55900 = CARTESIAN_POINT('Ctrl Pts',(31.937402730746,505.483009407519,-36.8567511403242)) ;
#55901 = CARTESIAN_POINT('Ctrl Pts',(31.9419669224967,505.487875768405,-36.943094869896)) ;
#55902 = CARTESIAN_POINT('Ctrl Pts',(31.9428891147143,505.489502817408,-36.9725265498881)) ;
#55903 = CARTESIAN_POINT('Ctrl Pts',(31.9435170542582,505.492952496085,-37.0364320994741)) ;
#55904 = CARTESIAN_POINT('Ctrl Pts',(31.9429886571748,505.49476227536,-37.0708985509635)) ;
#55905 = CARTESIAN_POINT('Ctrl Pts',(31.9370274694344,505.502333002227,-37.2180382696468)) ;
#55906 = CARTESIAN_POINT('Ctrl Pts',(31.9231889087325,505.507720579316,-37.3301837395203)) ;
#55907 = CARTESIAN_POINT('Ctrl Pts',(31.872100781106,505.519691521973,-37.5757734343199)) ;
#55908 = CARTESIAN_POINT('Ctrl Pts',(31.830444490881,505.526259986763,-37.7077295174122)) ;
#55909 = CARTESIAN_POINT('Ctrl Pts',(31.7539265691495,505.536093527371,-37.8855069550971)) ;
#55910 = CARTESIAN_POINT('Ctrl Pts',(31.7299169398524,505.538978067801,-37.9355962640774)) ;
#55911 = CARTESIAN_POINT('Ctrl Pts',(31.6805661196336,505.54459248417,-38.0286784891973)) ;
#55912 = CARTESIAN_POINT('Ctrl Pts',(31.6556299448185,505.547305891994,-38.0718410072548)) ;
#55913 = CARTESIAN_POINT('Ctrl Pts',(31.5945563448165,505.553696441116,-38.1692005939754)) ;
#55914 = CARTESIAN_POINT('Ctrl Pts',(31.5573682182337,505.557410654666,-38.2226613420936)) ;
#55915 = CARTESIAN_POINT('Ctrl Pts',(31.517715239327,505.561197820373,-38.2742565263254)) ;
#55916 = CARTESIAN_POINT('Ctrl Pts',(31.5177152522353,505.503079332004,-38.2742565095294)) ;
#55917 = CARTESIAN_POINT('Ctrl Pts',(31.5432594015477,505.500592988626,-38.241019281098)) ;
#55918 = CARTESIAN_POINT('Ctrl Pts',(31.5677759902234,505.498132158959,-38.2070146138837)) ;
#55919 = CARTESIAN_POINT('Ctrl Pts',(31.6077365179056,505.494018655011,-38.1478540702654)) ;
#55920 = CARTESIAN_POINT('Ctrl Pts',(31.6237048133343,505.492343866605,-38.1230808209613)) ;
#55921 = CARTESIAN_POINT('Ctrl Pts',(31.654357641665,505.489078477689,-38.0732011775607)) ;
#55922 = CARTESIAN_POINT('Ctrl Pts',(31.6690523403465,505.487489075299,-38.048110885117)) ;
#55923 = CARTESIAN_POINT('Ctrl Pts',(31.7041112169815,505.483637673754,-37.9852260120648)) ;
#55924 = CARTESIAN_POINT('Ctrl Pts',(31.7238322599976,505.48141223199,-37.9470909865917)) ;
#55925 = CARTESIAN_POINT('Ctrl Pts',(31.8051851392548,505.471837009847,-37.7769117488908)) ;
#55926 = CARTESIAN_POINT('Ctrl Pts',(31.8538695483115,505.46497816158,-37.6391398552467)) ;
#55927 = CARTESIAN_POINT('Ctrl Pts',(31.9094431812189,505.45325591178,-37.4053594828939)) ;
#55928 = CARTESIAN_POINT('Ctrl Pts',(31.9249351970208,505.448557249049,-37.3119586025348)) ;
#55929 = CARTESIAN_POINT('Ctrl Pts',(31.9388241458078,505.440997860556,-37.1667717136594)) ;
#55930 = CARTESIAN_POINT('Ctrl Pts',(31.941794673664,505.438284193569,-37.1155524345259)) ;
#55931 = CARTESIAN_POINT('Ctrl Pts',(31.9439502214248,505.432592308066,-37.0104156998921)) ;
#55932 = CARTESIAN_POINT('Ctrl Pts',(31.9429356820414,505.429609822057,-36.9565344427641)) ;
#55933 = CARTESIAN_POINT('Ctrl Pts',(31.9301488437827,505.417164331509,-36.7368609263858)) ;
#55934 = CARTESIAN_POINT('Ctrl Pts',(31.9004030573165,505.407133710477,-36.572767822369)) ;
#55935 = CARTESIAN_POINT('Ctrl Pts',(31.8334697505138,505.393559500329,-36.3567256915239)) ;
#55936 = CARTESIAN_POINT('Ctrl Pts',(31.8131938104639,505.38997828119,-36.3001742412565)) ;
#55937 = CARTESIAN_POINT('Ctrl Pts',(31.7739185188301,505.383928604321,-36.2041066614166)) ;
#55938 = CARTESIAN_POINT('Ctrl Pts',(31.7560782378548,505.381423891878,-36.1641592143029)) ;
#55939 = CARTESIAN_POINT('Ctrl Pts',(31.7243610022495,505.377381847522,-36.0988251011835)) ;
#55940 = CARTESIAN_POINT('Ctrl Pts',(31.7112012525127,505.375807563079,-36.073111764612)) ;
#55941 = CARTESIAN_POINT('Ctrl Pts',(31.6760828259188,505.371855363693,-36.0079197723625)) ;
#55942 = CARTESIAN_POINT('Ctrl Pts',(31.6533577202339,505.369521543204,-35.9688736446147)) ;
#55943 = CARTESIAN_POINT('Ctrl Pts',(31.5569927740764,505.360344610654,-35.8151887329742)) ;
#55944 = CARTESIAN_POINT('Ctrl Pts',(31.4733198468932,505.353900202707,-35.7072476536089)) ;
#55945 = CARTESIAN_POINT('Ctrl Pts',(31.3120446226615,505.342476280166,-35.5371587822526)) ;
#55946 = CARTESIAN_POINT('Ctrl Pts',(31.2395057059155,505.337609991647,-35.4708751030663)) ;
#55947 = CARTESIAN_POINT('Ctrl Pts',(31.1219360454515,505.329847836059,-35.3779655124312)) ;
#55948 = CARTESIAN_POINT('Ctrl Pts',(31.0801646953316,505.327113139803,-35.3474444174973)) ;
#55949 = CARTESIAN_POINT('Ctrl Pts',(30.9925627975267,505.321397130336,-35.2883741749554)) ;
#55950 = CARTESIAN_POINT('Ctrl Pts',(30.9466698406774,505.318412465061,-35.259990538721)) ;
#55951 = CARTESIAN_POINT('Ctrl Pts',(30.7478939960761,505.305505553309,-35.1476193254565)) ;
#55952 = CARTESIAN_POINT('Ctrl Pts',(30.58577954101,505.294947537872,-35.0814812310761)) ;
#55953 = CARTESIAN_POINT('Ctrl Pts',(30.3404172809854,505.279745486182,-35.0161382456613)) ;
#55954 = CARTESIAN_POINT('Ctrl Pts',(30.2624002655157,505.275034187498,-35.0001439488519)) ;
#55955 = CARTESIAN_POINT('Ctrl Pts',(30.1523268032647,505.268721449373,-34.9841687239715)) ;
#55956 = CARTESIAN_POINT('Ctrl Pts',(30.1209034492736,505.266957199868,-34.9803470099263)) ;
#55957 = CARTESIAN_POINT('Ctrl Pts',(30.0560717160086,505.263412270665,-34.9739785065418)) ;
#55958 = CARTESIAN_POINT('Ctrl Pts',(30.0226647066311,505.261636127242,-34.9715196161678)) ;
#55959 = CARTESIAN_POINT('Ctrl Pts',(29.8599061509482,505.253164541916,-34.9635348511347)) ;
#55960 = CARTESIAN_POINT('Ctrl Pts',(29.7302774337086,505.246961535828,-34.9694250504372)) ;
#55961 = CARTESIAN_POINT('Ctrl Pts',(29.4877074911626,505.235100694508,-35.0035776956375)) ;
#55962 = CARTESIAN_POINT('Ctrl Pts',(29.3749275155548,505.229475604998,-35.0292868657789)) ;
#55963 = CARTESIAN_POINT('Ctrl Pts',(29.2125147991268,505.220742448635,-35.0810192248685)) ;
#55964 = CARTESIAN_POINT('Ctrl Pts',(29.1608129479363,505.217865460563,-35.0998042935609)) ;
#55965 = CARTESIAN_POINT('Ctrl Pts',(29.0625858169282,505.212174789031,-35.14002444078)) ;
#55966 = CARTESIAN_POINT('Ctrl Pts',(29.0159860179916,505.209372764817,-35.1611697744908)) ;
#55967 = CARTESIAN_POINT('Ctrl Pts',(28.8896523223537,505.201472695054,-35.2242841378477)) ;
#55968 = CARTESIAN_POINT('Ctrl Pts',(28.811821334232,505.196253829399,-35.2697873726756)) ;
#55969 = CARTESIAN_POINT('Ctrl Pts',(28.6383150594367,505.183842710017,-35.3871591080225)) ;
#55970 = CARTESIAN_POINT('Ctrl Pts',(28.545423907068,505.176578538692,-35.4625670479707)) ;
#55971 = CARTESIAN_POINT('Ctrl Pts',(28.4269569699713,505.166783558656,-35.5772125941878)) ;
#55972 = CARTESIAN_POINT('Ctrl Pts',(28.3953596266303,505.164113058441,-35.609888224118)) ;
#55973 = CARTESIAN_POINT('Ctrl Pts',(28.3403197168179,505.1593935597,-35.6707206305667)) ;
#55974 = CARTESIAN_POINT('Ctrl Pts',(28.3164966479929,505.157325692856,-35.6985078248541)) ;
#55975 = CARTESIAN_POINT('Ctrl Pts',(28.2745393729093,505.153660272653,-35.7501785436828)) ;
#55976 = CARTESIAN_POINT('Ctrl Pts',(28.2561631940795,505.152048213576,-35.7738486152144)) ;
#55977 = CARTESIAN_POINT('Ctrl Pts',(28.2027390154522,505.147318538617,-35.8458614415899)) ;
#55978 = CARTESIAN_POINT('Ctrl Pts',(28.1692712221652,505.144294241577,-35.8953414156333)) ;
#55979 = CARTESIAN_POINT('Ctrl Pts',(28.0673887747061,505.134640099647,-36.0611000942924)) ;
#55980 = CARTESIAN_POINT('Ctrl Pts',(28.0082538770677,505.128266383487,-36.1826624000175)) ;
#55981 = CARTESIAN_POINT('Ctrl Pts',(27.9381615227228,505.118327366196,-36.3721019957412)) ;
#55982 = CARTESIAN_POINT('Ctrl Pts',(27.9179684468764,505.114969852566,-36.4361575043987)) ;
#55983 = CARTESIAN_POINT('Ctrl Pts',(27.88735574353,505.108760086949,-36.5529256348119)) ;
#55984 = CARTESIAN_POINT('Ctrl Pts',(27.8757988018647,505.10594521769,-36.6052765730506)) ;
#55985 = CARTESIAN_POINT('Ctrl Pts',(27.857097744626,505.100269343256,-36.7091305197846)) ;
#55986 = CARTESIAN_POINT('Ctrl Pts',(27.849835510262,505.09741457224,-36.7605713997011)) ;
#55987 = CARTESIAN_POINT('Ctrl Pts',(27.8257131609026,505.084158714168,-36.9954390527392)) ;
#55988 = CARTESIAN_POINT('Ctrl Pts',(27.8316177713847,505.073010012815,-37.1803234450564)) ;
#55989 = CARTESIAN_POINT('Ctrl Pts',(27.8751604348053,505.057240439044,-37.4400463182781)) ;
#55990 = CARTESIAN_POINT('Ctrl Pts',(27.8927726421801,505.052548364635,-37.5173777387894)) ;
#55991 = CARTESIAN_POINT('Ctrl Pts',(27.9235984391196,505.046255727532,-37.6238660426529)) ;
#55992 = CARTESIAN_POINT('Ctrl Pts',(27.9330877258813,505.044493493175,-37.6540239419565)) ;
#55993 = CARTESIAN_POINT('Ctrl Pts',(27.9540349362348,505.040954001598,-37.7155956044435)) ;
#55994 = CARTESIAN_POINT('Ctrl Pts',(27.9655709722411,505.039181211303,-37.7469723276986)) ;
#55995 = CARTESIAN_POINT('Ctrl Pts',(28.0257454140721,505.030676542357,-37.8990738843119)) ;
#55996 = CARTESIAN_POINT('Ctrl Pts',(28.0850173936249,505.024443865928,-38.015283221071)) ;
#55997 = CARTESIAN_POINT('Ctrl Pts',(28.2212010833597,505.012161033301,-38.2293385685761)) ;
#55998 = CARTESIAN_POINT('Ctrl Pts',(28.2967701320055,505.006137981683,-38.3273658581876)) ;
#55999 = CARTESIAN_POINT('Ctrl Pts',(28.4165817130021,504.997041877175,-38.4567911796279)) ;
#56000 = CARTESIAN_POINT('Ctrl Pts',(28.4539660250601,504.994259088158,-38.4941734989611)) ;
#56001 = CARTESIAN_POINT('Ctrl Pts',(28.5313488090397,504.988575411499,-38.5658019568158)) ;
#56002 = CARTESIAN_POINT('Ctrl Pts',(28.571304899042,504.985677285731,-38.600034648668)) ;
#56003 = CARTESIAN_POINT('Ctrl Pts',(28.7425712982585,504.973379570882,-38.7357261707658)) ;
#56004 = CARTESIAN_POINT('Ctrl Pts',(28.8845975969161,504.963404056848,-38.8226133190237)) ;
#56005 = CARTESIAN_POINT('Ctrl Pts',(29.0933743062256,504.949620468823,-38.9178862281061)) ;
#56006 = CARTESIAN_POINT('Ctrl Pts',(29.1524584016029,504.945817270856,-38.9415999111235)) ;
#56007 = CARTESIAN_POINT('Ctrl Pts',(29.2553632642701,504.939452978291,-38.9774493796882)) ;
#56008 = CARTESIAN_POINT('Ctrl Pts',(29.2986617632715,504.936851163619,-38.9909445365498)) ;
#56009 = CARTESIAN_POINT('Ctrl Pts',(29.370281174925,504.932710142485,-39.0106913320309)) ;
#56010 = CARTESIAN_POINT('Ctrl Pts',(29.3983463375474,504.931129353618,-39.0177949315178)) ;
#56011 = CARTESIAN_POINT('Ctrl Pts',(29.4693084782319,504.927236179828,-39.0341685816871)) ;
#56012 = CARTESIAN_POINT('Ctrl Pts',(29.5123678087349,504.924963566524,-39.0426618116219)) ;
#56013 = CARTESIAN_POINT('Ctrl Pts',(29.6893278364498,504.915869181874,-39.0717121081284)) ;
#56014 = CARTESIAN_POINT('Ctrl Pts',(29.8248377999944,504.909454863808,-39.0803858137404)) ;
#56015 = CARTESIAN_POINT('Ctrl Pts',(30.0605273344726,504.897970111336,-39.0721569499138)) ;
#56016 = CARTESIAN_POINT('Ctrl Pts',(30.1604321294592,504.893001244726,-39.0613109501082)) ;
#56017 = CARTESIAN_POINT('Ctrl Pts',(30.310144023599,504.885120863418,-39.0338575420454)) ;
#56018 = CARTESIAN_POINT('Ctrl Pts',(30.3607745174687,504.882380238046,-39.0225773586328)) ;
#56019 = CARTESIAN_POINT('Ctrl Pts',(30.4628939918487,504.876670346212,-38.9957327307716)) ;
#56020 = CARTESIAN_POINT('Ctrl Pts',(30.5143066547907,504.873698577772,-38.9800379010375)) ;
#56021 = CARTESIAN_POINT('Ctrl Pts',(30.725159134075,504.861082949099,-38.9065167783299)) ;
#56022 = CARTESIAN_POINT('Ctrl Pts',(30.8777293303398,504.850842812948,-38.8310864827132)) ;
#56023 = CARTESIAN_POINT('Ctrl Pts',(31.0898427805649,504.835608128116,-38.6912866238233)) ;
#56024 = CARTESIAN_POINT('Ctrl Pts',(31.1574830734569,504.830587488018,-38.6404604145834)) ;
#56025 = CARTESIAN_POINT('Ctrl Pts',(31.2461151503098,504.823968419732,-38.5648767573069)) ;
#56026 = CARTESIAN_POINT('Ctrl Pts',(31.269940717696,504.82218515875,-38.5435794273517)) ;
#56027 = CARTESIAN_POINT('Ctrl Pts',(31.317365891355,504.818645079631,-38.4991536137446)) ;
#56028 = CARTESIAN_POINT('Ctrl Pts',(31.3409237007241,504.816891108491,-38.4759945289144)) ;
#56029 = CARTESIAN_POINT('Ctrl Pts',(31.4185346947066,504.811085943858,-38.395926731457)) ;
#56030 = CARTESIAN_POINT('Ctrl Pts',(31.4698864950361,504.807197796271,-38.3364897555531)) ;
#56031 = CARTESIAN_POINT('Ctrl Pts',(31.5177152522312,504.803366924184,-38.2742565095347)) ;
#56032 = CARTESIAN_POINT('Origin',(29.8885276254015,502.164639880024,-37.0221601717529)) ;
#56033 = CARTESIAN_POINT('',(31.5172280011895,504.105620599056,-38.2738060481768)) ;
#56034 = CARTESIAN_POINT('',(31.5177152521424,504.164515898581,-38.2742565096501)) ;
#56035 = CARTESIAN_POINT('',(31.5177152522233,502.164639880024,-38.2742565095444)) ;
#56036 = CARTESIAN_POINT('',(29.8878696237816,503.856489559997,-34.9674102771103)) ;
#56037 = CARTESIAN_POINT('Ctrl Pts',(29.8878312245244,503.857426760662,-34.9679514454232)) ;
#56038 = CARTESIAN_POINT('Ctrl Pts',(29.9587306547387,503.861501994475,-34.968065421851)) ;
#56039 = CARTESIAN_POINT('Ctrl Pts',(30.0296724459679,503.865522183533,-34.9718222713218)) ;
#56040 = CARTESIAN_POINT('Ctrl Pts',(30.100260036513,503.869457885301,-34.9791956158892)) ;
#56041 = CARTESIAN_POINT('Ctrl Pts',(30.1708288602434,503.873392540701,-34.9865670001376)) ;
#56042 = CARTESIAN_POINT('Ctrl Pts',(30.2410436494645,503.877242723409,-34.9975529416747)) ;
#56043 = CARTESIAN_POINT('Ctrl Pts',(30.3105123120153,503.881003593668,-35.0120926107395)) ;
#56044 = CARTESIAN_POINT('Ctrl Pts',(30.3799863322682,503.88476475398,-35.0266334011618)) ;
#56045 = CARTESIAN_POINT('Ctrl Pts',(30.4487140397119,503.888436660364,-35.0447285611316)) ;
#56046 = CARTESIAN_POINT('Ctrl Pts',(30.5163081024759,503.892038742141,-35.0662821556403)) ;
#56047 = CARTESIAN_POINT('Ctrl Pts',(30.5839794203305,503.895644940836,-35.0878603843376)) ;
#56048 = CARTESIAN_POINT('Ctrl Pts',(30.6505143686305,503.89918134044,-35.112905163166)) ;
#56049 = CARTESIAN_POINT('Ctrl Pts',(30.7155306513185,503.902689862847,-35.1412828089591)) ;
#56050 = CARTESIAN_POINT('Ctrl Pts',(30.7805867418378,503.906200533434,-35.1696778296696)) ;
#56051 = CARTESIAN_POINT('Ctrl Pts',(30.8441220708106,503.909683637407,-35.2014101137795)) ;
#56052 = CARTESIAN_POINT('Ctrl Pts',(30.9057627031913,503.913199682518,-35.236304393048)) ;
#56053 = CARTESIAN_POINT('Ctrl Pts',(30.9638589191116,503.916513550467,-35.2691922059154)) ;
#56054 = CARTESIAN_POINT('Ctrl Pts',(31.0202722455625,503.919857171378,-35.3048892324424)) ;
#56055 = CARTESIAN_POINT('Ctrl Pts',(31.0746996633575,503.923291086605,-35.343209505544)) ;
#56056 = CARTESIAN_POINT('Ctrl Pts',(31.0781287493569,503.923507433276,-35.3456237944687)) ;
#56057 = CARTESIAN_POINT('Ctrl Pts',(31.0815499697125,503.923724138357,-35.3480484972001)) ;
#56058 = CARTESIAN_POINT('Ctrl Pts',(31.0849632555621,503.923941216991,-35.3504835678714)) ;
#56059 = CARTESIAN_POINT('Ctrl Pts',(31.121809935943,503.926284597351,-35.3767703409934)) ;
#56060 = CARTESIAN_POINT('Ctrl Pts',(31.157729995907,503.928671744451,-35.4042641881606)) ;
#56061 = CARTESIAN_POINT('Ctrl Pts',(31.1926332392124,503.931122357307,-35.4328954209148)) ;
#56062 = CARTESIAN_POINT('Ctrl Pts',(31.1926595354685,503.931124203609,-35.4329169918108)) ;
#56063 = CARTESIAN_POINT('Ctrl Pts',(31.1926858311482,503.931126049948,-35.4329385633523)) ;
#56064 = CARTESIAN_POINT('Ctrl Pts',(31.1927121262513,503.931127896322,-35.4329601355393)) ;
#56065 = CARTESIAN_POINT('Ctrl Pts',(31.2424669614003,503.934621552848,-35.4737784051372)) ;
#56066 = CARTESIAN_POINT('Ctrl Pts',(31.2903362767567,503.938253505451,-35.517065402354)) ;
#56067 = CARTESIAN_POINT('Ctrl Pts',(31.3360902907372,503.941958684045,-35.5626000995648)) ;
#56068 = CARTESIAN_POINT('Ctrl Pts',(31.3407283961832,503.942334279703,-35.567215972769)) ;
#56069 = CARTESIAN_POINT('Ctrl Pts',(31.3453447563855,503.94271062783,-35.5718548999249)) ;
#56070 = CARTESIAN_POINT('Ctrl Pts',(31.3499391269652,503.943087660642,-35.5765166214108)) ;
#56071 = CARTESIAN_POINT('Ctrl Pts',(31.3997794398737,503.947177760261,-35.6270875654645)) ;
#56072 = CARTESIAN_POINT('Ctrl Pts',(31.4470335721025,503.951347819346,-35.6803467425906)) ;
#56073 = CARTESIAN_POINT('Ctrl Pts',(31.491437646493,503.955523483257,-35.7359747223897)) ;
#56074 = CARTESIAN_POINT('Ctrl Pts',(31.5357868487461,503.95969398711,-35.7915339601601)) ;
#56075 = CARTESIAN_POINT('Ctrl Pts',(31.5772933649038,503.963869728294,-35.8494559619384)) ;
#56076 = CARTESIAN_POINT('Ctrl Pts',(31.6157305657986,503.967995970738,-35.909405072221)) ;
#56077 = CARTESIAN_POINT('Ctrl Pts',(31.6541420787343,503.972119455573,-35.969314117924)) ;
#56078 = CARTESIAN_POINT('Ctrl Pts',(31.6894885400054,503.976193338822,-36.0312474986286)) ;
#56079 = CARTESIAN_POINT('Ctrl Pts',(31.7215763217742,503.980186173349,-36.0948546235593)) ;
#56080 = CARTESIAN_POINT('Ctrl Pts',(31.7536534439539,503.984177681453,-36.1584406181473)) ;
#56081 = CARTESIAN_POINT('Ctrl Pts',(31.7824740663728,503.988088154215,-36.2236992266939)) ;
#56082 = CARTESIAN_POINT('Ctrl Pts',(31.8078759919812,503.991910879953,-36.2902651839037)) ;
#56083 = CARTESIAN_POINT('Ctrl Pts',(31.8332780166312,503.995733620596,-36.3568314006528)) ;
#56084 = CARTESIAN_POINT('Ctrl Pts',(31.8552612087533,503.999468678092,-36.4247049768362)) ;
#56085 = CARTESIAN_POINT('Ctrl Pts',(31.8736953332307,504.003133864588,-36.4935057365259)) ;
#56086 = CARTESIAN_POINT('Ctrl Pts',(31.8921479241621,504.006802722698,-36.5623754176373)) ;
#56087 = CARTESIAN_POINT('Ctrl Pts',(31.9070440935627,504.010401747856,-36.6321741504546)) ;
#56088 = CARTESIAN_POINT('Ctrl Pts',(31.9182878507565,504.013971589968,-36.7025055842154)) ;
#56089 = CARTESIAN_POINT('Ctrl Pts',(31.9295376629882,504.017543354527,-36.7728748931713)) ;
#56090 = CARTESIAN_POINT('Ctrl Pts',(31.9371307375621,504.021086241873,-36.8437774587815)) ;
#56091 = CARTESIAN_POINT('Ctrl Pts',(31.9410102774574,504.024659943532,-36.9148012608961)) ;
#56092 = CARTESIAN_POINT('Ctrl Pts',(31.9446846091069,504.028044614257,-36.9820682593097)) ;
#56093 = CARTESIAN_POINT('Ctrl Pts',(31.9450275903617,504.031457416092,-37.0494443437025)) ;
#56094 = CARTESIAN_POINT('Ctrl Pts',(31.9420298057886,504.034959576058,-37.1165662660705)) ;
#56095 = CARTESIAN_POINT('Ctrl Pts',(31.9418569339711,504.035161533451,-37.1204369540504)) ;
#56096 = CARTESIAN_POINT('Ctrl Pts',(31.9416729594104,504.035363787999,-37.124306809581)) ;
#56097 = CARTESIAN_POINT('Ctrl Pts',(31.941477882663,504.035566351442,-37.1281757677485)) ;
#56098 = CARTESIAN_POINT('Ctrl Pts',(31.939306877194,504.037820676204,-37.171233330753)) ;
#56099 = CARTESIAN_POINT('Ctrl Pts',(31.9357608346423,504.040113478892,-37.2141776975869)) ;
#56100 = CARTESIAN_POINT('Ctrl Pts',(31.9308473628059,504.04246162487,-37.2569112546444)) ;
#56101 = CARTESIAN_POINT('Ctrl Pts',(31.9308436908624,504.04246337969,-37.2569431903537)) ;
#56102 = CARTESIAN_POINT('Ctrl Pts',(31.9308400181555,504.042465134541,-37.2569751259456)) ;
#56103 = CARTESIAN_POINT('Ctrl Pts',(31.9308363446852,504.042466889423,-37.2570070614202)) ;
#56104 = CARTESIAN_POINT('Ctrl Pts',(31.9234398621271,504.046000320481,-37.3213087063446)) ;
#56105 = CARTESIAN_POINT('Ctrl Pts',(31.912915186025,504.049667772526,-37.3853536185928)) ;
#56106 = CARTESIAN_POINT('Ctrl Pts',(31.8993255122597,504.053404304604,-37.4488253707413)) ;
#56107 = CARTESIAN_POINT('Ctrl Pts',(31.8979992225737,504.053768972957,-37.4550199219631)) ;
#56108 = CARTESIAN_POINT('Ctrl Pts',(31.8966437686663,504.054134299289,-37.4612089854468)) ;
#56109 = CARTESIAN_POINT('Ctrl Pts',(31.8952592287782,504.05450022323,-37.4673922490841)) ;
#56110 = CARTESIAN_POINT('Ctrl Pts',(31.8797919975381,504.058588101277,-37.5364678815868)) ;
#56111 = CARTESIAN_POINT('Ctrl Pts',(31.8606909691678,504.062749822263,-37.6048235139712)) ;
#56112 = CARTESIAN_POINT('Ctrl Pts',(31.8380810444409,504.066913795307,-37.6720715610843)) ;
#56113 = CARTESIAN_POINT('Ctrl Pts',(31.8368818375184,504.067134648113,-37.6756383276524)) ;
#56114 = CARTESIAN_POINT('Ctrl Pts',(31.8356727670002,504.067355507253,-37.679201968751)) ;
#56115 = CARTESIAN_POINT('Ctrl Pts',(31.8344538540919,504.067576362047,-37.6827624233691)) ;
#56116 = CARTESIAN_POINT('Ctrl Pts',(31.8113790685836,504.071757281756,-37.7501640613874)) ;
#56117 = CARTESIAN_POINT('Ctrl Pts',(31.7847747385406,504.075936436921,-37.8164279458178)) ;
#56118 = CARTESIAN_POINT('Ctrl Pts',(31.7548029742689,504.080061397014,-37.8811820458108)) ;
#56119 = CARTESIAN_POINT('Ctrl Pts',(31.7248510222535,504.084183630383,-37.9458933413559)) ;
#56120 = CARTESIAN_POINT('Ctrl Pts',(31.69153621929,504.08825158237,-38.0090969421066)) ;
#56121 = CARTESIAN_POINT('Ctrl Pts',(31.6550509567708,504.092236212904,-38.0704403685554)) ;
#56122 = CARTESIAN_POINT('Ctrl Pts',(31.6185755072556,504.09621977174,-38.1317672961973)) ;
#56123 = CARTESIAN_POINT('Ctrl Pts',(31.5789313196791,504.100120021672,-38.1912350467056)) ;
#56124 = CARTESIAN_POINT('Ctrl Pts',(31.5363401614159,504.103932619486,-38.2485095559607)) ;
#56125 = CARTESIAN_POINT('Ctrl Pts',(31.5300337405706,504.104497146193,-38.2569901226744)) ;
#56126 = CARTESIAN_POINT('Ctrl Pts',(31.5236627620926,504.105059795431,-38.2654226367447)) ;
#56127 = CARTESIAN_POINT('Ctrl Pts',(31.5172280011895,504.105620599056,-38.2738060481768)) ;
#56128 = CARTESIAN_POINT('',(27.9033532997302,503.710565160562,-36.4919899545636)) ;
#56129 = CARTESIAN_POINT('Ctrl Pts',(27.9033532997302,503.710565160562,-36.4919899545636)) ;
#56130 = CARTESIAN_POINT('Ctrl Pts',(27.9220919685295,503.714502851079,-36.4218247076459)) ;
#56131 = CARTESIAN_POINT('Ctrl Pts',(27.9445724045105,503.718440541595,-36.3525880402978)) ;
#56132 = CARTESIAN_POINT('Ctrl Pts',(27.9706795420364,503.722378232112,-36.2846940426108)) ;
#56133 = CARTESIAN_POINT('Ctrl Pts',(27.9967660504768,503.726312811183,-36.2168536927464)) ;
#56134 = CARTESIAN_POINT('Ctrl Pts',(28.0264733976995,503.730247390253,-36.1503543313746)) ;
#56135 = CARTESIAN_POINT('Ctrl Pts',(28.0596371618002,503.734181969324,-36.0855934444734)) ;
#56136 = CARTESIAN_POINT('Ctrl Pts',(28.0927915167263,503.738115432081,-36.020850931436)) ;
#56137 = CARTESIAN_POINT('Ctrl Pts',(28.1294001364632,503.742048894839,-35.9578463250151)) ;
#56138 = CARTESIAN_POINT('Ctrl Pts',(28.1692515493607,503.745982357596,-35.8969547074697)) ;
#56139 = CARTESIAN_POINT('Ctrl Pts',(28.2090987948209,503.749915409014,-35.8360694576283)) ;
#56140 = CARTESIAN_POINT('Ctrl Pts',(28.2521879077288,503.753848460432,-35.7772971427937)) ;
#56141 = CARTESIAN_POINT('Ctrl Pts',(28.2982635873496,503.75778151185,-35.720984606436)) ;
#56142 = CARTESIAN_POINT('Ctrl Pts',(28.3443474330767,503.761715260333,-35.6646620896685)) ;
#56143 = CARTESIAN_POINT('Ctrl Pts',(28.3934186057526,503.765649008815,-35.6108005738718)) ;
#56144 = CARTESIAN_POINT('Ctrl Pts',(28.4451818536921,503.769582757297,-35.559713404931)) ;
#56145 = CARTESIAN_POINT('Ctrl Pts',(28.49696886516,503.773518311689,-35.508602782837)) ;
#56146 = CARTESIAN_POINT('Ctrl Pts',(28.5514500804081,503.777453866081,-35.4602693617864)) ;
#56147 = CARTESIAN_POINT('Ctrl Pts',(28.6082948160149,503.781389420473,-35.4149882717156)) ;
#56148 = CARTESIAN_POINT('Ctrl Pts',(28.6652241539097,503.785330832169,-35.3696397895851)) ;
#56149 = CARTESIAN_POINT('Ctrl Pts',(28.724523672739,503.789272243865,-35.3273529930464)) ;
#56150 = CARTESIAN_POINT('Ctrl Pts',(28.7858315231192,503.793213655561,-35.2883612017132)) ;
#56151 = CARTESIAN_POINT('Ctrl Pts',(28.8471906866653,503.797158366122,-35.2493367752077)) ;
#56152 = CARTESIAN_POINT('Ctrl Pts',(28.9105611288309,503.801103076683,-35.2136130723263)) ;
#56153 = CARTESIAN_POINT('Ctrl Pts',(28.9755563680077,503.805047787244,-35.181377445391)) ;
#56154 = CARTESIAN_POINT('Ctrl Pts',(29.0406755945526,503.809000022884,-35.1490803245588)) ;
#56155 = CARTESIAN_POINT('Ctrl Pts',(29.1074253848159,503.812952258523,-35.1202847483778)) ;
#56156 = CARTESIAN_POINT('Ctrl Pts',(29.1753996605939,503.816904494162,-35.0951297961986)) ;
#56157 = CARTESIAN_POINT('Ctrl Pts',(29.2033933039097,503.818532131581,-35.0847703072468)) ;
#56158 = CARTESIAN_POINT('Ctrl Pts',(29.2315944556788,503.820159769001,-35.0750276829276)) ;
#56159 = CARTESIAN_POINT('Ctrl Pts',(29.2599741689153,503.82178740642,-35.0659091360116)) ;
#56160 = CARTESIAN_POINT('Ctrl Pts',(29.3393312769002,503.826338706757,-35.0404112916096)) ;
#56161 = CARTESIAN_POINT('Ctrl Pts',(29.4203288439844,503.830890007094,-35.019718141297)) ;
#56162 = CARTESIAN_POINT('Ctrl Pts',(29.5024259274531,503.835441307431,-35.0040117526962)) ;
#56163 = CARTESIAN_POINT('Ctrl Pts',(29.5836359998494,503.839943433625,-34.9884750624574)) ;
#56164 = CARTESIAN_POINT('Ctrl Pts',(29.6659218421143,503.844445559818,-34.9778180432059)) ;
#56165 = CARTESIAN_POINT('Ctrl Pts',(29.7487386216568,503.848947686012,-34.9721707578944)) ;
#56166 = CARTESIAN_POINT('Ctrl Pts',(29.7949829729049,503.851461644007,-34.9690173504933)) ;
#56167 = CARTESIAN_POINT('Ctrl Pts',(29.8413925003401,503.853975602002,-34.9674251606845)) ;
#56168 = CARTESIAN_POINT('Ctrl Pts',(29.8878696237816,503.856489559997,-34.9674102771103)) ;
#56169 = CARTESIAN_POINT('',(27.9020254134846,503.711738695905,-37.5552366910798)) ;
#56170 = CARTESIAN_POINT('Origin',(29.8885276254018,503.710565160562,-37.0221601717529)) ;
#56171 = CARTESIAN_POINT('',(29.8898911409064,503.915940460665,-34.9674106241619)) ;
#56172 = CARTESIAN_POINT('Ctrl Pts',(27.9039683500008,503.712921345492,-37.5546280533383)) ;
#56173 = CARTESIAN_POINT('Ctrl Pts',(27.8995037155845,503.713852301909,-37.5379879292133)) ;
#56174 = CARTESIAN_POINT('Ctrl Pts',(27.8952483859091,503.714771424712,-37.5212917219665)) ;
#56175 = CARTESIAN_POINT('Ctrl Pts',(27.886036764227,503.716841188879,-37.4831506871666)) ;
#56176 = CARTESIAN_POINT('Ctrl Pts',(27.8812139526205,503.717985213449,-37.4616755791405)) ;
#56177 = CARTESIAN_POINT('Ctrl Pts',(27.8568247709929,503.724143278074,-37.3442834841899)) ;
#56178 = CARTESIAN_POINT('Ctrl Pts',(27.8437854282688,503.728897792319,-37.2471320603135)) ;
#56179 = CARTESIAN_POINT('Ctrl Pts',(27.8296332156294,503.739968633839,-37.0190582167473)) ;
#56180 = CARTESIAN_POINT('Ctrl Pts',(27.8339921163726,503.746265877539,-36.888231605803)) ;
#56181 = CARTESIAN_POINT('Ctrl Pts',(27.8579825952917,503.755817822207,-36.7026628037148)) ;
#56182 = CARTESIAN_POINT('Ctrl Pts',(27.8675376787861,503.758764102179,-36.6469395229417)) ;
#56183 = CARTESIAN_POINT('Ctrl Pts',(27.8898799130842,503.764464200626,-36.5426621624512)) ;
#56184 = CARTESIAN_POINT('Ctrl Pts',(27.9021730887732,503.767200103077,-36.4940446020989)) ;
#56185 = CARTESIAN_POINT('Ctrl Pts',(27.9394879791671,503.774613120687,-36.3663252054139)) ;
#56186 = CARTESIAN_POINT('Ctrl Pts',(27.9675402507877,503.779385189147,-36.2882119439521)) ;
#56187 = CARTESIAN_POINT('Ctrl Pts',(28.0495855302198,503.791628527376,-36.0969801900279)) ;
#56188 = CARTESIAN_POINT('Ctrl Pts',(28.1093470840185,503.799222721748,-35.9866988954612)) ;
#56189 = CARTESIAN_POINT('Ctrl Pts',(28.2043468026331,503.809383269486,-35.8441703913619)) ;
#56190 = CARTESIAN_POINT('Ctrl Pts',(28.231214526888,503.812090938927,-35.8066608073265)) ;
#56191 = CARTESIAN_POINT('Ctrl Pts',(28.2818373445074,503.816865971107,-35.7407901992321)) ;
#56192 = CARTESIAN_POINT('Ctrl Pts',(28.3051390535472,503.818952610576,-35.7121053384563)) ;
#56193 = CARTESIAN_POINT('Ctrl Pts',(28.3486802868947,503.822632837904,-35.6613654561645)) ;
#56194 = CARTESIAN_POINT('Ctrl Pts',(28.3686500757782,503.824241688844,-35.6390967753399)) ;
#56195 = CARTESIAN_POINT('Ctrl Pts',(28.4296630890996,503.828947793278,-35.5739780438843)) ;
#56196 = CARTESIAN_POINT('Ctrl Pts',(28.4720856913458,503.831953423431,-35.5324586622611)) ;
#56197 = CARTESIAN_POINT('Ctrl Pts',(28.5937487897015,503.840064678512,-35.4232894697111)) ;
#56198 = CARTESIAN_POINT('Ctrl Pts',(28.676425041411,503.845036795839,-35.3597376320947)) ;
#56199 = CARTESIAN_POINT('Ctrl Pts',(28.8506239461131,503.855149598635,-35.2457657528314)) ;
#56200 = CARTESIAN_POINT('Ctrl Pts',(28.9418766686474,503.860277451658,-35.1955046718228)) ;
#56201 = CARTESIAN_POINT('Ctrl Pts',(29.0844113825613,503.868361659425,-35.1305569912995)) ;
#56202 = CARTESIAN_POINT('Ctrl Pts',(29.1331037638954,503.871133589946,-35.1105902289528)) ;
#56203 = CARTESIAN_POINT('Ctrl Pts',(29.2320299767583,503.876814001513,-35.0743949495267)) ;
#56204 = CARTESIAN_POINT('Ctrl Pts',(29.2822295473098,503.87972065266,-35.0581895918306)) ;
#56205 = CARTESIAN_POINT('Ctrl Pts',(29.4512549976591,503.889603698697,-35.0107231550851)) ;
#56206 = CARTESIAN_POINT('Ctrl Pts',(29.5722404547271,503.896851265574,-34.9881883691788)) ;
#56207 = CARTESIAN_POINT('Ctrl Pts',(29.7594459305128,503.908121077591,-34.9704312157898)) ;
#56208 = CARTESIAN_POINT('Ctrl Pts',(29.8246508535686,503.912051762148,-34.9673673312246)) ;
#56209 = CARTESIAN_POINT('Ctrl Pts',(29.8898911409064,503.915940460665,-34.9674106241619)) ;
#56210 = CARTESIAN_POINT('Ctrl Pts',(29.8898907546911,503.915940437644,-34.9674106239056)) ;
#56211 = CARTESIAN_POINT('Ctrl Pts',(29.9412118975136,503.918999474773,-34.9674446705626)) ;
#56212 = CARTESIAN_POINT('Ctrl Pts',(29.9925166924859,503.922029783632,-34.9694014736775)) ;
#56213 = CARTESIAN_POINT('Ctrl Pts',(30.0772710138307,503.926938004848,-34.9758202236688)) ;
#56214 = CARTESIAN_POINT('Ctrl Pts',(30.110779615718,503.928852925703,-34.9791879325618)) ;
#56215 = CARTESIAN_POINT('Ctrl Pts',(30.1731762546706,503.932352264999,-34.9870125093617)) ;
#56216 = CARTESIAN_POINT('Ctrl Pts',(30.2020783033838,503.933944411954,-34.9912645428387)) ;
#56217 = CARTESIAN_POINT('Ctrl Pts',(30.275719399037,503.937928801769,-35.0037083854746)) ;
#56218 = CARTESIAN_POINT('Ctrl Pts',(30.3202933140566,503.940276653806,-35.0127711910703)) ;
#56219 = CARTESIAN_POINT('Ctrl Pts',(30.499928782168,503.949609406583,-35.0555494144053)) ;
#56220 = CARTESIAN_POINT('Ctrl Pts',(30.6317068364755,503.956177054412,-35.1014677215833)) ;
#56221 = CARTESIAN_POINT('Ctrl Pts',(30.8449847968994,503.967650789419,-35.2010512629974)) ;
#56222 = CARTESIAN_POINT('Ctrl Pts',(30.9291608931864,503.972423959962,-35.2478073802305)) ;
#56223 = CARTESIAN_POINT('Ctrl Pts',(31.0530156507559,503.980081622879,-35.3284567998562)) ;
#56224 = CARTESIAN_POINT('Ctrl Pts',(31.095203256516,503.982812703552,-35.3582500933929)) ;
#56225 = CARTESIAN_POINT('Ctrl Pts',(31.1792661583935,503.988538944048,-35.4224956388487)) ;
#56226 = CARTESIAN_POINT('Ctrl Pts',(31.2209892942773,503.991538273957,-35.4570794438543)) ;
#56227 = CARTESIAN_POINT('Ctrl Pts',(31.384374251533,504.003959453222,-35.6037802147022)) ;
#56228 = CARTESIAN_POINT('Ctrl Pts',(31.4936433169988,504.013941525847,-35.7287360089024)) ;
#56229 = CARTESIAN_POINT('Ctrl Pts',(31.6207528046515,504.027493959158,-35.9153429551586)) ;
#56230 = CARTESIAN_POINT('Ctrl Pts',(31.6525509761974,504.031098492875,-35.9667594242137)) ;
#56231 = CARTESIAN_POINT('Ctrl Pts',(31.7034883341003,504.037184023251,-36.0578741591218)) ;
#56232 = CARTESIAN_POINT('Ctrl Pts',(31.7237034616467,504.03970172154,-36.0969250055133)) ;
#56233 = CARTESIAN_POINT('Ctrl Pts',(31.7551791831204,504.043766137583,-36.1628264484052)) ;
#56234 = CARTESIAN_POINT('Ctrl Pts',(31.7671480753834,504.04535007867,-36.1893169209582)) ;
#56235 = CARTESIAN_POINT('Ctrl Pts',(31.7964942216375,504.049341231933,-36.2581232157323)) ;
#56236 = CARTESIAN_POINT('Ctrl Pts',(31.8130274850055,504.051702887088,-36.3007796192349)) ;
#56237 = CARTESIAN_POINT('Ctrl Pts',(31.8732001605406,504.060918625975,-36.4728673129829)) ;
#56238 = CARTESIAN_POINT('Ctrl Pts',(31.9053147636052,504.067376953104,-36.6059599726057)) ;
#56239 = CARTESIAN_POINT('Ctrl Pts',(31.9373099817429,504.078788352167,-36.8378057805151)) ;
#56240 = CARTESIAN_POINT('Ctrl Pts',(31.9437466642977,504.083623846665,-36.9351671541599)) ;
#56241 = CARTESIAN_POINT('Ctrl Pts',(31.9429870674464,504.09136281609,-37.0845125529047)) ;
#56242 = CARTESIAN_POINT('Ctrl Pts',(31.9407566908302,504.094108476059,-37.1363820140462)) ;
#56243 = CARTESIAN_POINT('Ctrl Pts',(31.9321639818676,504.09986743614,-37.2424281855392)) ;
#56244 = CARTESIAN_POINT('Ctrl Pts',(31.9256036212411,504.102885005581,-37.2965470116399)) ;
#56245 = CARTESIAN_POINT('Ctrl Pts',(31.8907667679561,504.115225099739,-37.5118637552816)) ;
#56246 = CARTESIAN_POINT('Ctrl Pts',(31.8454350063363,504.125089287533,-37.6696699718548)) ;
#56247 = CARTESIAN_POINT('Ctrl Pts',(31.7582035803814,504.138562293709,-37.8765757688344)) ;
#56248 = CARTESIAN_POINT('Ctrl Pts',(31.7320303805895,504.142198731399,-37.9316723938254)) ;
#56249 = CARTESIAN_POINT('Ctrl Pts',(31.6827119127414,504.148330635356,-38.0245851249103)) ;
#56250 = CARTESIAN_POINT('Ctrl Pts',(31.6607219471618,504.150863312766,-38.0629679880221)) ;
#56251 = CARTESIAN_POINT('Ctrl Pts',(31.622203027077,504.154947338704,-38.1254360075018)) ;
#56252 = CARTESIAN_POINT('Ctrl Pts',(31.6063716377376,504.156536360766,-38.1499279277824)) ;
#56253 = CARTESIAN_POINT('Ctrl Pts',(31.5669298128708,504.160289956304,-38.2081872630936)) ;
#56254 = CARTESIAN_POINT('Ctrl Pts',(31.5428169386247,504.162424078541,-38.2415949996772)) ;
#56255 = CARTESIAN_POINT('Ctrl Pts',(31.5177152521424,504.164515898581,-38.2742565096501)) ;
#56256 = CARTESIAN_POINT('Origin',(29.888527625402,504.710565160562,-37.0221601717529)) ;
#56257 = CARTESIAN_POINT('',(30.464143066922,505.578718967617,-35.4585122521231)) ;
#56258 = CARTESIAN_POINT('',(30.4640904799735,505.710565160562,-35.4587397547064)) ;
#56259 = CARTESIAN_POINT('',(30.4640904799733,504.710565160562,-35.4587397547064)) ;
#56260 = CARTESIAN_POINT('',(31.5536816258517,505.710557682283,-36.9466234719841)) ;
#56261 = CARTESIAN_POINT('Origin',(29.8885276254021,505.710565160562,-37.0221601717529)) ;
#56262 = CARTESIAN_POINT('Ctrl Pts',(31.5536816419713,505.710557682144,-36.9466234712529)) ;
#56263 = CARTESIAN_POINT('Ctrl Pts',(31.5512527851025,505.706944742544,-36.8937691566076)) ;
#56264 = CARTESIAN_POINT('Ctrl Pts',(31.5462448774997,505.70323427545,-36.8409426256499)) ;
#56265 = CARTESIAN_POINT('Ctrl Pts',(31.5386909643017,505.699480728201,-36.7884134558091)) ;
#56266 = CARTESIAN_POINT('Ctrl Pts',(31.5300837950213,505.695203816919,-36.7285600467054)) ;
#56267 = CARTESIAN_POINT('Ctrl Pts',(31.5181708641553,505.690871535778,-36.6690914842317)) ;
#56268 = CARTESIAN_POINT('Ctrl Pts',(31.5030394057526,505.686550012591,-36.6103848174665)) ;
#56269 = CARTESIAN_POINT('Ctrl Pts',(31.4879233747511,505.682232895447,-36.5517380055599)) ;
#56270 = CARTESIAN_POINT('Ctrl Pts',(31.4695956550047,505.677926812381,-36.4938513990106)) ;
#56271 = CARTESIAN_POINT('Ctrl Pts',(31.4481779335575,505.673676937873,-36.4370847936346)) ;
#56272 = CARTESIAN_POINT('Ctrl Pts',(31.426773921506,505.669429783692,-36.3803545243301)) ;
#56273 = CARTESIAN_POINT('Ctrl Pts',(31.4022839523053,505.665238884364,-36.3247427727838)) ;
#56274 = CARTESIAN_POINT('Ctrl Pts',(31.3748614996201,505.661125540527,-36.27059400033)) ;
#56275 = CARTESIAN_POINT('Ctrl Pts',(31.3474461947096,505.657013268851,-36.2164593419756)) ;
#56276 = CARTESIAN_POINT('Ctrl Pts',(31.3170999076325,505.652978502872,-36.1637869518671)) ;
#56277 = CARTESIAN_POINT('Ctrl Pts',(31.2840075847354,505.649017956302,-36.1129063626823)) ;
#56278 = CARTESIAN_POINT('Ctrl Pts',(31.2508873781163,505.645054072561,-36.0619829013119)) ;
#56279 = CARTESIAN_POINT('Ctrl Pts',(31.2150163856363,505.641164409488,-36.0128544152588)) ;
#56280 = CARTESIAN_POINT('Ctrl Pts',(31.1766127984997,505.637322040209,-35.965835046155)) ;
#56281 = CARTESIAN_POINT('Ctrl Pts',(31.1381947871522,505.633478227753,-35.9187980167923)) ;
#56282 = CARTESIAN_POINT('Ctrl Pts',(31.0972420804711,505.629681471652,-35.8738719648829)) ;
#56283 = CARTESIAN_POINT('Ctrl Pts',(31.0540082979801,505.62588411196,-35.8313519796076)) ;
#56284 = CARTESIAN_POINT('Ctrl Pts',(31.0106923755428,505.622079537657,-35.7887512105309)) ;
#56285 = CARTESIAN_POINT('Ctrl Pts',(30.9650864474462,505.618273883806,-35.7485661354866)) ;
#56286 = CARTESIAN_POINT('Ctrl Pts',(30.9174843642785,505.614403978776,-35.7110684842806)) ;
#56287 = CARTESIAN_POINT('Ctrl Pts',(30.8747062787521,505.610926250128,-35.6773708470431)) ;
#56288 = CARTESIAN_POINT('Ctrl Pts',(30.8303158357592,505.607396043612,-35.6458432612686)) ;
#56289 = CARTESIAN_POINT('Ctrl Pts',(30.7845572496917,505.603763009415,-35.6166606978547)) ;
#56290 = CARTESIAN_POINT('Ctrl Pts',(30.7804377721901,505.603435940685,-35.614033498814)) ;
#56291 = CARTESIAN_POINT('Ctrl Pts',(30.7763071950674,505.603108038564,-35.6114252724309)) ;
#56292 = CARTESIAN_POINT('Ctrl Pts',(30.7721656894153,505.602779266313,-35.6088361268173)) ;
#56293 = CARTESIAN_POINT('Ctrl Pts',(30.7721384702333,505.602777105526,-35.6088191101978)) ;
#56294 = CARTESIAN_POINT('Ctrl Pts',(30.7721112505793,505.602774944701,-35.6088020944026)) ;
#56295 = CARTESIAN_POINT('Ctrl Pts',(30.7720840304533,505.602772783839,-35.6087850794315)) ;
#56296 = CARTESIAN_POINT('Ctrl Pts',(30.7243106697558,505.598980308744,-35.5789225302735)) ;
#56297 = CARTESIAN_POINT('Ctrl Pts',(30.6749166898039,505.595062673764,-35.5515039524481)) ;
#56298 = CARTESIAN_POINT('Ctrl Pts',(30.6241821421764,505.591085141819,-35.526667745808)) ;
#56299 = CARTESIAN_POINT('Ctrl Pts',(30.6187902896983,505.590662426598,-35.5240282591351)) ;
#56300 = CARTESIAN_POINT('Ctrl Pts',(30.6133833445669,505.59023903487,-35.521417936482)) ;
#56301 = CARTESIAN_POINT('Ctrl Pts',(30.6079616773488,505.58981504497,-35.5188369411351)) ;
#56302 = CARTESIAN_POINT('Ctrl Pts',(30.5610542874591,505.586146752775,-35.4965065858826)) ;
#56303 = CARTESIAN_POINT('Ctrl Pts',(30.5130406271979,505.58243378182,-35.476370609909)) ;
#56304 = CARTESIAN_POINT('Ctrl Pts',(30.464143066922,505.578718967617,-35.4585122521231)) ;
#56305 = CARTESIAN_POINT('Origin',(29.888527625402,504.710565160562,-37.0221601717529)) ;
#56306 = CARTESIAN_POINT('',(30.464090486888,504.876987562729,-35.458739757252)) ;
#56307 = CARTESIAN_POINT('',(30.4640782702768,505.071453548379,-35.4587633355736)) ;
#56308 = CARTESIAN_POINT('',(30.4640904799733,504.710565160562,-35.4587397547064)) ;
#56309 = CARTESIAN_POINT('',(29.5692971707754,505.710565160562,-35.3870308445011)) ;
#56310 = CARTESIAN_POINT('Ctrl Pts',(30.4640782702767,505.071453548379,-35.4587633355736)) ;
#56311 = CARTESIAN_POINT('Ctrl Pts',(30.521095886814,505.075779371587,-35.4799146325238)) ;
#56312 = CARTESIAN_POINT('Ctrl Pts',(30.5770093172339,505.080082548189,-35.5041983938192)) ;
#56313 = CARTESIAN_POINT('Ctrl Pts',(30.6314720687145,505.084322153635,-35.5314549496953)) ;
#56314 = CARTESIAN_POINT('Ctrl Pts',(30.6859073887704,505.088559623705,-35.5586977771765)) ;
#56315 = CARTESIAN_POINT('Ctrl Pts',(30.7388935375263,505.092733495002,-35.5889103448657)) ;
#56316 = CARTESIAN_POINT('Ctrl Pts',(30.7901019141151,505.09682720154,-35.6219030512834)) ;
#56317 = CARTESIAN_POINT('Ctrl Pts',(30.841303537339,505.1009203682,-35.6548914066203)) ;
#56318 = CARTESIAN_POINT('Ctrl Pts',(30.8907277923682,505.104933423079,-35.6906592105178)) ;
#56319 = CARTESIAN_POINT('Ctrl Pts',(30.9380637241444,505.108874530588,-35.7289868532582)) ;
#56320 = CARTESIAN_POINT('Ctrl Pts',(30.9854452919855,505.112819437677,-35.7673514472685)) ;
#56321 = CARTESIAN_POINT('Ctrl Pts',(31.0307343299584,505.116692408518,-35.8082809470378)) ;
#56322 = CARTESIAN_POINT('Ctrl Pts',(31.0736383498221,505.120525064871,-35.8515236587419)) ;
#56323 = CARTESIAN_POINT('Ctrl Pts',(31.1165627879252,505.124359545204,-35.8947869498706)) ;
#56324 = CARTESIAN_POINT('Ctrl Pts',(31.157099618341,505.128153982491,-35.9403658504486)) ;
#56325 = CARTESIAN_POINT('Ctrl Pts',(31.1949789855704,505.131960084758,-35.9879743964208)) ;
#56326 = CARTESIAN_POINT('Ctrl Pts',(31.232929820935,505.135773368113,-36.0356727668608)) ;
#56327 = CARTESIAN_POINT('Ctrl Pts',(31.2682126114471,505.139598886506,-36.0854086683138)) ;
#56328 = CARTESIAN_POINT('Ctrl Pts',(31.3005855087351,505.143502545096,-36.136857261922)) ;
#56329 = CARTESIAN_POINT('Ctrl Pts',(31.3266547494785,505.146646082564,-36.1782877758715)) ;
#56330 = CARTESIAN_POINT('Ctrl Pts',(31.3508373525747,505.149840752387,-36.2208282201655)) ;
#56331 = CARTESIAN_POINT('Ctrl Pts',(31.373025387342,505.153123202999,-36.264290323874)) ;
#56332 = CARTESIAN_POINT('Ctrl Pts',(31.3730389005797,505.153125202119,-36.2643167937142)) ;
#56333 = CARTESIAN_POINT('Ctrl Pts',(31.3730524130785,505.153127201271,-36.2643432638968)) ;
#56334 = CARTESIAN_POINT('Ctrl Pts',(31.3730659248384,505.153129200455,-36.2643697344215)) ;
#56335 = CARTESIAN_POINT('Ctrl Pts',(31.3982528864256,505.156855834804,-36.3137128318952)) ;
#56336 = CARTESIAN_POINT('Ctrl Pts',(31.420956765697,505.16070546399,-36.3644292075354)) ;
#56337 = CARTESIAN_POINT('Ctrl Pts',(31.4410618580961,505.164614959203,-36.4162338892592)) ;
#56338 = CARTESIAN_POINT('Ctrl Pts',(31.4429416870201,505.164980497547,-36.4210776341757)) ;
#56339 = CARTESIAN_POINT('Ctrl Pts',(31.4447988044912,505.165346559256,-36.4259308565645)) ;
#56340 = CARTESIAN_POINT('Ctrl Pts',(31.4466331213465,505.165713092729,-36.4307933009082)) ;
#56341 = CARTESIAN_POINT('Ctrl Pts',(31.4683528422139,505.170053130654,-36.488368377742)) ;
#56342 = CARTESIAN_POINT('Ctrl Pts',(31.4868749718261,505.174458641855,-36.547242373152)) ;
#56343 = CARTESIAN_POINT('Ctrl Pts',(31.5020916321177,505.178858084683,-36.6070223227843)) ;
#56344 = CARTESIAN_POINT('Ctrl Pts',(31.5170796559837,505.183191424117,-36.6659040546905)) ;
#56345 = CARTESIAN_POINT('Ctrl Pts',(31.5288612462848,505.187518591047,-36.7256647050432)) ;
#56346 = CARTESIAN_POINT('Ctrl Pts',(31.5373724102927,505.191791728717,-36.785927153992)) ;
#56347 = CARTESIAN_POINT('Ctrl Pts',(31.5458783654769,505.196062251232,-36.8461527223839)) ;
#56348 = CARTESIAN_POINT('Ctrl Pts',(31.5511180254007,505.200278675115,-36.9068794869961)) ;
#56349 = CARTESIAN_POINT('Ctrl Pts',(31.5530627641506,505.20441698709,-36.9677293364333)) ;
#56350 = CARTESIAN_POINT('Ctrl Pts',(31.5550070381138,505.20855431002,-37.0285646429413)) ;
#56351 = CARTESIAN_POINT('Ctrl Pts',(31.5536579351739,505.2126135552,-37.0895229550957)) ;
#56352 = CARTESIAN_POINT('Ctrl Pts',(31.5490214038572,505.216595484114,-37.1502247919745)) ;
#56353 = CARTESIAN_POINT('Ctrl Pts',(31.5442553468897,505.220688651775,-37.2126223889773)) ;
#56354 = CARTESIAN_POINT('Ctrl Pts',(31.5360152655613,505.224700130541,-37.2747489134894)) ;
#56355 = CARTESIAN_POINT('Ctrl Pts',(31.5243472856465,505.228657089693,-37.3361910850951)) ;
#56356 = CARTESIAN_POINT('Ctrl Pts',(31.5129817265898,505.232511488934,-37.3960407450232)) ;
#56357 = CARTESIAN_POINT('Ctrl Pts',(31.498363534411,505.236314524773,-37.4552409302377)) ;
#56358 = CARTESIAN_POINT('Ctrl Pts',(31.4805754935564,505.24011282074,-37.5134101492967)) ;
#56359 = CARTESIAN_POINT('Ctrl Pts',(31.4620774821819,505.244062717335,-37.5739010647714)) ;
#56360 = CARTESIAN_POINT('Ctrl Pts',(31.4401507137193,505.248007903713,-37.6332767301028)) ;
#56361 = CARTESIAN_POINT('Ctrl Pts',(31.4149400872327,505.252018883781,-37.6911121580904)) ;
#56362 = CARTESIAN_POINT('Ctrl Pts',(31.3931146376458,505.255491286314,-37.7411816880382)) ;
#56363 = CARTESIAN_POINT('Ctrl Pts',(31.368827773735,505.259013656685,-37.7900977673775)) ;
#56364 = CARTESIAN_POINT('Ctrl Pts',(31.3422126922891,505.262636793551,-37.8375881137863)) ;
#56365 = CARTESIAN_POINT('Ctrl Pts',(31.3380993813103,505.263196742567,-37.844927657859)) ;
#56366 = CARTESIAN_POINT('Ctrl Pts',(31.3339304770256,505.263759098402,-37.852233248156)) ;
#56367 = CARTESIAN_POINT('Ctrl Pts',(31.3297064861299,505.264324048576,-37.8595039900052)) ;
#56368 = CARTESIAN_POINT('Ctrl Pts',(31.3296913405529,505.264326074266,-37.859530060038)) ;
#56369 = CARTESIAN_POINT('Ctrl Pts',(31.3296761942676,505.26432809999,-37.8595561296227)) ;
#56370 = CARTESIAN_POINT('Ctrl Pts',(31.3296610472742,505.264330125747,-37.8595821987594)) ;
#56371 = CARTESIAN_POINT('Ctrl Pts',(31.3017728603314,505.268059887965,-37.907579906101)) ;
#56372 = CARTESIAN_POINT('Ctrl Pts',(31.2713767813286,505.271912555743,-37.9542267962505)) ;
#56373 = CARTESIAN_POINT('Ctrl Pts',(31.2386507747087,505.275825029993,-37.9992706142958)) ;
#56374 = CARTESIAN_POINT('Ctrl Pts',(31.2355914882052,505.276190775188,-38.0034813921709)) ;
#56375 = CARTESIAN_POINT('Ctrl Pts',(31.2325118759833,505.276557043023,-38.007678147697)) ;
#56376 = CARTESIAN_POINT('Ctrl Pts',(31.2294121053228,505.27692378195,-38.0118606671151)) ;
#56377 = CARTESIAN_POINT('Ctrl Pts',(31.1927870786063,505.281256948653,-38.0612788022653)) ;
#56378 = CARTESIAN_POINT('Ctrl Pts',(31.1533424184425,505.285655220766,-38.1087120445306)) ;
#56379 = CARTESIAN_POINT('Ctrl Pts',(31.1113494546076,505.290047632902,-38.1538582110569)) ;
#56380 = CARTESIAN_POINT('Ctrl Pts',(31.0698905146768,505.294384186797,-38.1984302544467)) ;
#56381 = CARTESIAN_POINT('Ctrl Pts',(31.0259479181896,505.298714736299,-38.2407733821669)) ;
#56382 = CARTESIAN_POINT('Ctrl Pts',(30.9798051895301,505.302991533763,-38.2806288131767)) ;
#56383 = CARTESIAN_POINT('Ctrl Pts',(30.9336907071007,505.307265713189,-38.32045984672)) ;
#56384 = CARTESIAN_POINT('Ctrl Pts',(30.8853788424685,505.311486071251,-38.3578063463012)) ;
#56385 = CARTESIAN_POINT('Ctrl Pts',(30.8351730602288,505.315628761888,-38.3924387332868)) ;
#56386 = CARTESIAN_POINT('Ctrl Pts',(30.784979484531,505.319770445312,-38.4270627000931)) ;
#56387 = CARTESIAN_POINT('Ctrl Pts',(30.7328929083336,505.323834497195,-38.4589738385256)) ;
#56388 = CARTESIAN_POINT('Ctrl Pts',(30.6792366782967,505.327821892011,-38.4879708705226)) ;
#56389 = CARTESIAN_POINT('Ctrl Pts',(30.6243043061247,505.331904121714,-38.5176575583956)) ;
#56390 = CARTESIAN_POINT('Ctrl Pts',(30.5677266025114,505.335906031441,-38.5442895646531)) ;
#56391 = CARTESIAN_POINT('Ctrl Pts',(30.5098727161521,505.339854660265,-38.5676831579019)) ;
#56392 = CARTESIAN_POINT('Ctrl Pts',(30.4532918764318,505.343716401431,-38.5905619865059)) ;
#56393 = CARTESIAN_POINT('Ctrl Pts',(30.3954904280474,505.347527534501,-38.6103431478182)) ;
#56394 = CARTESIAN_POINT('Ctrl Pts',(30.3368351358503,505.35133479927,-38.6268887086384)) ;
#56395 = CARTESIAN_POINT('Ctrl Pts',(30.2762002621473,505.35527055698,-38.6439926723747)) ;
#56396 = CARTESIAN_POINT('Ctrl Pts',(30.2146528039645,505.359202610514,-38.657638126504)) ;
#56397 = CARTESIAN_POINT('Ctrl Pts',(30.1526223166261,505.363200214559,-38.6677175266866)) ;
#56398 = CARTESIAN_POINT('Ctrl Pts',(30.0986341516869,505.366679524746,-38.6764901213073)) ;
#56399 = CARTESIAN_POINT('Ctrl Pts',(30.0442792308175,505.370209139025,-38.6825616770159)) ;
#56400 = CARTESIAN_POINT('Ctrl Pts',(29.989858990173,505.373839649464,-38.6858959847392)) ;
#56401 = CARTESIAN_POINT('Ctrl Pts',(29.9817842858887,505.374378333194,-38.6863907188407)) ;
#56402 = CARTESIAN_POINT('Ctrl Pts',(29.9737080742526,505.374919238222,-38.6868252534974)) ;
#56403 = CARTESIAN_POINT('Ctrl Pts',(29.9656312655556,505.375462529814,-38.6871995343826)) ;
#56404 = CARTESIAN_POINT('Ctrl Pts',(29.9655992751451,505.375464681669,-38.6872010168245)) ;
#56405 = CARTESIAN_POINT('Ctrl Pts',(29.9655672847251,505.375466833562,-38.6872024983211)) ;
#56406 = CARTESIAN_POINT('Ctrl Pts',(29.9655352942958,505.375468985492,-38.6872039788726)) ;
#56407 = CARTESIAN_POINT('Ctrl Pts',(29.910055865614,505.379200971678,-38.6897716264538)) ;
#56408 = CARTESIAN_POINT('Ctrl Pts',(29.8543515765862,505.383055234418,-38.689497265412)) ;
#56409 = CARTESIAN_POINT('Ctrl Pts',(29.7987318761332,505.386968302999,-38.6863937388079)) ;
#56410 = CARTESIAN_POINT('Ctrl Pts',(29.7936788099732,505.387323806432,-38.6861117825022)) ;
#56411 = CARTESIAN_POINT('Ctrl Pts',(29.7886264707689,505.387679795235,-38.6858064957554)) ;
#56412 = CARTESIAN_POINT('Ctrl Pts',(29.7835751074526,505.388036221814,-38.6854779010942)) ;
#56413 = CARTESIAN_POINT('Ctrl Pts',(29.722169189496,505.39236905236,-38.6814834038582)) ;
#56414 = CARTESIAN_POINT('Ctrl Pts',(29.6609024128934,505.396765913205,-38.6740413916708)) ;
#56415 = CARTESIAN_POINT('Ctrl Pts',(29.6001769888483,505.401155779833,-38.6632161713429)) ;
#56416 = CARTESIAN_POINT('Ctrl Pts',(29.5403576390167,505.405480145972,-38.6525524723736)) ;
#56417 = CARTESIAN_POINT('Ctrl Pts',(29.4810634358088,505.409797446368,-38.6386061825611)) ;
#56418 = CARTESIAN_POINT('Ctrl Pts',(29.4226642303696,505.414060532842,-38.6214749234021)) ;
#56419 = CARTESIAN_POINT('Ctrl Pts',(29.3642989539147,505.418321142533,-38.6043536172249)) ;
#56420 = CARTESIAN_POINT('Ctrl Pts',(29.3068275724457,505.422527470063,-38.5840511502648)) ;
#56421 = CARTESIAN_POINT('Ctrl Pts',(29.250606322394,505.426656364448,-38.5606977303438)) ;
#56422 = CARTESIAN_POINT('Ctrl Pts',(29.1943967501594,505.430784401213,-38.5373491612037)) ;
#56423 = CARTESIAN_POINT('Ctrl Pts',(29.1394368218155,505.434835037256,-38.5109508832397)) ;
#56424 = CARTESIAN_POINT('Ctrl Pts',(29.0860698172838,505.438809997494,-38.4816651878905)) ;
#56425 = CARTESIAN_POINT('Ctrl Pts',(29.0312266948075,505.442894904134,-38.4515694575618)) ;
#56426 = CARTESIAN_POINT('Ctrl Pts',(28.978066042403,505.44689990356,-38.4184240703072)) ;
#56427 = CARTESIAN_POINT('Ctrl Pts',(28.926945092787,505.4508532385,-38.3824417917118)) ;
#56428 = CARTESIAN_POINT('Ctrl Pts',(28.8771318783715,505.454705442391,-38.3473799829564)) ;
#56429 = CARTESIAN_POINT('Ctrl Pts',(28.8292555258394,505.458508962815,-38.3096245023365)) ;
#56430 = CARTESIAN_POINT('Ctrl Pts',(28.7836295441577,505.462311419072,-38.2694087431619)) ;
#56431 = CARTESIAN_POINT('Ctrl Pts',(28.7362068494048,505.466263612882,-38.2276093209621)) ;
#56432 = CARTESIAN_POINT('Ctrl Pts',(28.6912159086222,505.470215085446,-38.1831514246148)) ;
#56433 = CARTESIAN_POINT('Ctrl Pts',(28.6489836710172,505.474237187497,-38.1363428692093)) ;
#56434 = CARTESIAN_POINT('Ctrl Pts',(28.6125417380707,505.47770783413,-38.0959520603359)) ;
#56435 = CARTESIAN_POINT('Ctrl Pts',(28.5781531172907,505.481231733459,-38.0538103871801)) ;
#56436 = CARTESIAN_POINT('Ctrl Pts',(28.5460087664382,505.484859486374,-38.0101497501515)) ;
#56437 = CARTESIAN_POINT('Ctrl Pts',(28.540921715463,505.485433601685,-38.0032401725653)) ;
#56438 = CARTESIAN_POINT('Ctrl Pts',(28.5358907697851,505.486010318021,-37.9962925253697)) ;
#56439 = CARTESIAN_POINT('Ctrl Pts',(28.5309165710722,505.486589835939,-37.9893076939497)) ;
#56440 = CARTESIAN_POINT('Ctrl Pts',(28.5308966183035,505.486592160532,-37.9892796760247)) ;
#56441 = CARTESIAN_POINT('Ctrl Pts',(28.5308766664477,505.48659448517,-37.9892516575015)) ;
#56442 = CARTESIAN_POINT('Ctrl Pts',(28.530856715505,505.486596809853,-37.98922363838)) ;
#56443 = CARTESIAN_POINT('Ctrl Pts',(28.4989644475012,505.49031289568,-37.9444341092091)) ;
#56444 = CARTESIAN_POINT('Ctrl Pts',(28.4692925350709,505.494154464843,-37.8979427697449)) ;
#56445 = CARTESIAN_POINT('Ctrl Pts',(28.4419955250567,505.498058691952,-37.8500096556061)) ;
#56446 = CARTESIAN_POINT('Ctrl Pts',(28.4393387204183,505.498438688468,-37.8453443490429)) ;
#56447 = CARTESIAN_POINT('Ctrl Pts',(28.43670441025,505.498819278544,-37.8406654251301)) ;
#56448 = CARTESIAN_POINT('Ctrl Pts',(28.4340927344234,505.499200404256,-37.8359731497715)) ;
#56449 = CARTESIAN_POINT('Ctrl Pts',(28.4041673982211,505.50356745278,-37.7822077029919)) ;
#56450 = CARTESIAN_POINT('Ctrl Pts',(28.3772138650138,505.508004129347,-37.7266831668167)) ;
#56451 = CARTESIAN_POINT('Ctrl Pts',(28.3533978736318,505.512437125704,-37.6697741685417)) ;
#56452 = CARTESIAN_POINT('Ctrl Pts',(28.3300305247356,505.516786613864,-37.6139372144259)) ;
#56453 = CARTESIAN_POINT('Ctrl Pts',(28.3096831476368,505.521132276051,-37.5567675619365)) ;
#56454 = CARTESIAN_POINT('Ctrl Pts',(28.2924735956573,505.525425110746,-37.4986264512002)) ;
#56455 = CARTESIAN_POINT('Ctrl Pts',(28.2752748252914,505.529715256021,-37.4405217652929)) ;
#56456 = CARTESIAN_POINT('Ctrl Pts',(28.261209815786,505.533952497417,-37.3814468522232)) ;
#56457 = CARTESIAN_POINT('Ctrl Pts',(28.2503614602831,505.538111497103,-37.3217690562125)) ;
#56458 = CARTESIAN_POINT('Ctrl Pts',(28.2395157738388,505.542269473536,-37.2621059429372)) ;
#56459 = CARTESIAN_POINT('Ctrl Pts',(28.2318851855977,505.546349236226,-37.2018402665271)) ;
#56460 = CARTESIAN_POINT('Ctrl Pts',(28.2275185485494,505.55035014595,-37.14134563109)) ;
#56461 = CARTESIAN_POINT('Ctrl Pts',(28.2229996175459,505.554490594263,-37.078741141502)) ;
#56462 = CARTESIAN_POINT('Ctrl Pts',(28.2219766819324,505.558546560858,-37.0158914609938)) ;
#56463 = CARTESIAN_POINT('Ctrl Pts',(28.2244639682465,505.562544359745,-36.9532174210266)) ;
#56464 = CARTESIAN_POINT('Ctrl Pts',(28.226870615007,505.566412547209,-36.8925753170618)) ;
#56465 = CARTESIAN_POINT('Ctrl Pts',(28.2325636526095,505.570226658843,-36.8320977765136)) ;
#56466 = CARTESIAN_POINT('Ctrl Pts',(28.2415163079168,505.574032336457,-36.7721710651033)) ;
#56467 = CARTESIAN_POINT('Ctrl Pts',(28.250918928383,505.578029289427,-36.7092324056952)) ;
#56468 = CARTESIAN_POINT('Ctrl Pts',(28.2639180144742,505.582017313911,-36.6469015568741)) ;
#56469 = CARTESIAN_POINT('Ctrl Pts',(28.2804294752268,505.586068514865,-36.5856292757383)) ;
#56470 = CARTESIAN_POINT('Ctrl Pts',(28.2946525214386,505.589558237503,-36.5328490584605)) ;
#56471 = CARTESIAN_POINT('Ctrl Pts',(28.3114819201761,505.593095501817,-36.4808533077519)) ;
#56472 = CARTESIAN_POINT('Ctrl Pts',(28.3308241855398,505.596732103637,-36.4299323744501)) ;
#56473 = CARTESIAN_POINT('Ctrl Pts',(28.3339294830955,505.597315940666,-36.4217572901598)) ;
#56474 = CARTESIAN_POINT('Ctrl Pts',(28.3370995170736,505.597902338079,-36.4136098043667)) ;
#56475 = CARTESIAN_POINT('Ctrl Pts',(28.3403338676742,505.598491510205,-36.4054909973772)) ;
#56476 = CARTESIAN_POINT('Ctrl Pts',(28.3403409220056,505.598492795228,-36.4054732897251)) ;
#56477 = CARTESIAN_POINT('Ctrl Pts',(28.340347976643,505.598494080264,-36.4054555822094)) ;
#56478 = CARTESIAN_POINT('Ctrl Pts',(28.3403550315863,505.598495365314,-36.4054378748302)) ;
#56479 = CARTESIAN_POINT('Ctrl Pts',(28.361155477361,505.602284141862,-36.353230313964)) ;
#56480 = CARTESIAN_POINT('Ctrl Pts',(28.3846961235323,505.606197592738,-36.3020279818582)) ;
#56481 = CARTESIAN_POINT('Ctrl Pts',(28.4108341231365,505.610173397742,-36.2521099908632)) ;
#56482 = CARTESIAN_POINT('Ctrl Pts',(28.4134743662545,505.610575000465,-36.2470676909862)) ;
#56483 = CARTESIAN_POINT('Ctrl Pts',(28.4161410727314,505.610977239409,-36.2420385169523)) ;
#56484 = CARTESIAN_POINT('Ctrl Pts',(28.4188340691836,505.611380050343,-36.2370227700409)) ;
#56485 = CARTESIAN_POINT('Ctrl Pts',(28.4481249715863,505.615761302224,-36.1824680181646)) ;
#56486 = CARTESIAN_POINT('Ctrl Pts',(28.480531020835,505.620209584656,-36.1294983574458)) ;
#56487 = CARTESIAN_POINT('Ctrl Pts',(28.5158274435636,505.624655609921,-36.078451901193)) ;
#56488 = CARTESIAN_POINT('Ctrl Pts',(28.5510800142243,505.629096111471,-36.0274688647571)) ;
#56489 = CARTESIAN_POINT('Ctrl Pts',(28.5892155533788,505.633534020205,-35.9784039506105)) ;
#56490 = CARTESIAN_POINT('Ctrl Pts',(28.6299836584483,505.63792088294,-35.9315656998075)) ;
#56491 = CARTESIAN_POINT('Ctrl Pts',(28.6707138952097,505.642303670845,-35.8847709556944)) ;
#56492 = CARTESIAN_POINT('Ctrl Pts',(28.714071767279,505.64663537072,-35.8401985986474)) ;
#56493 = CARTESIAN_POINT('Ctrl Pts',(28.7597830356109,505.650891718927,-35.798131407424)) ;
#56494 = CARTESIAN_POINT('Ctrl Pts',(28.8054661625882,505.655145446786,-35.7560901141419)) ;
#56495 = CARTESIAN_POINT('Ctrl Pts',(28.853499841945,505.659323922623,-35.7165509234305)) ;
#56496 = CARTESIAN_POINT('Ctrl Pts',(28.9035856874473,505.663427902196,-35.6797720977196)) ;
#56497 = CARTESIAN_POINT('Ctrl Pts',(28.9536755208936,505.667532208537,-35.6429903435986)) ;
#56498 = CARTESIAN_POINT('Ctrl Pts',(29.0058179585603,505.671562141034,-35.6089695679321)) ;
#56499 = CARTESIAN_POINT('Ctrl Pts',(29.0596886201874,505.675542395257,-35.577942630958)) ;
#56500 = CARTESIAN_POINT('Ctrl Pts',(29.1135569296164,505.679522475687,-35.546917048738)) ;
#56501 = CARTESIAN_POINT('Ctrl Pts',(29.1691534513111,505.683453174641,-35.5188853886785)) ;
#56502 = CARTESIAN_POINT('Ctrl Pts',(29.2261260138388,505.687379963192,-35.4940511678207)) ;
#56503 = CARTESIAN_POINT('Ctrl Pts',(29.2831544935491,505.69131060579,-35.4691925727801)) ;
#56504 = CARTESIAN_POINT('Ctrl Pts',(29.3415618192553,505.695237834327,-35.4475382706051)) ;
#56505 = CARTESIAN_POINT('Ctrl Pts',(29.4009649620739,505.69922216151,-35.4292561559619)) ;
#56506 = CARTESIAN_POINT('Ctrl Pts',(29.4563224157855,505.702935133537,-35.4122191564516)) ;
#56507 = CARTESIAN_POINT('Ctrl Pts',(29.5125442978946,505.706698340933,-35.3981108521241)) ;
#56508 = CARTESIAN_POINT('Ctrl Pts',(29.5692971707753,505.710565160562,-35.3870308445009)) ;
#56509 = CARTESIAN_POINT('Origin',(29.8885276254021,505.710565160562,-37.0221601717529)) ;
#56510 = CARTESIAN_POINT('Ctrl Pts',(30.4640904938027,504.876987562729,-35.4587397597976)) ;
#56511 = CARTESIAN_POINT('Ctrl Pts',(30.4869337999252,504.878606326814,-35.4671493716302)) ;
#56512 = CARTESIAN_POINT('Ctrl Pts',(30.5095919064472,504.880241842228,-35.4760593026279)) ;
#56513 = CARTESIAN_POINT('Ctrl Pts',(30.5969398749291,504.886669676781,-35.5126379224649)) ;
#56514 = CARTESIAN_POINT('Ctrl Pts',(30.6600356443181,504.891583087799,-35.5438915012115)) ;
#56515 = CARTESIAN_POINT('Ctrl Pts',(30.8112018494661,504.904035861512,-35.631088162206)) ;
#56516 = CARTESIAN_POINT('Ctrl Pts',(30.8963581682533,504.91168516546,-35.6914896998207)) ;
#56517 = CARTESIAN_POINT('Ctrl Pts',(31.0183684306797,504.923328324557,-35.7964997827966)) ;
#56518 = CARTESIAN_POINT('Ctrl Pts',(31.0595092459496,504.927391497997,-35.8357424522067)) ;
#56519 = CARTESIAN_POINT('Ctrl Pts',(31.1193420758518,504.933422332971,-35.8989659670094)) ;
#56520 = CARTESIAN_POINT('Ctrl Pts',(31.139517178829,504.935477752932,-35.9214807707376)) ;
#56521 = CARTESIAN_POINT('Ctrl Pts',(31.1861826459071,504.94027152647,-35.9765005393346)) ;
#56522 = CARTESIAN_POINT('Ctrl Pts',(31.2120797784735,504.942972035025,-36.0094790518896)) ;
#56523 = CARTESIAN_POINT('Ctrl Pts',(31.2717458874835,504.949392045973,-36.0916655653749)) ;
#56524 = CARTESIAN_POINT('Ctrl Pts',(31.3041695307979,504.953055753782,-36.1417784788156)) ;
#56525 = CARTESIAN_POINT('Ctrl Pts',(31.3963108705091,504.964382928952,-36.3024919662609)) ;
#56526 = CARTESIAN_POINT('Ctrl Pts',(31.4462548894849,504.971984508305,-36.4181612414627)) ;
#56527 = CARTESIAN_POINT('Ctrl Pts',(31.4976383669698,504.983351232614,-36.5874707561682)) ;
#56528 = CARTESIAN_POINT('Ctrl Pts',(31.5102685142421,504.986715794551,-36.6372604475614)) ;
#56529 = CARTESIAN_POINT('Ctrl Pts',(31.5322736830597,504.994062191278,-36.7445899001118)) ;
#56530 = CARTESIAN_POINT('Ctrl Pts',(31.5409685806546,504.998061606725,-36.8021970301492)) ;
#56531 = CARTESIAN_POINT('Ctrl Pts',(31.5533834565238,505.00702110329,-36.9292462563812)) ;
#56532 = CARTESIAN_POINT('Ctrl Pts',(31.5558086545656,505.012010252248,-36.9987050410494)) ;
#56533 = CARTESIAN_POINT('Ctrl Pts',(31.5506638408612,505.025550526036,-37.1851850933535)) ;
#56534 = CARTESIAN_POINT('Ctrl Pts',(31.5350964495807,505.034174280405,-37.3016039753621)) ;
#56535 = CARTESIAN_POINT('Ctrl Pts',(31.5003271382971,505.04439270362,-37.4447325775823)) ;
#56536 = CARTESIAN_POINT('Ctrl Pts',(31.4924147812081,505.046447069871,-37.4738366955062)) ;
#56537 = CARTESIAN_POINT('Ctrl Pts',(31.4720493303971,505.051146763743,-37.5414390832326)) ;
#56538 = CARTESIAN_POINT('Ctrl Pts',(31.458976426799,505.053759286329,-37.5797288360284)) ;
#56539 = CARTESIAN_POINT('Ctrl Pts',(31.4244820998282,505.059876520636,-37.6698827050114)) ;
#56540 = CARTESIAN_POINT('Ctrl Pts',(31.4018098630181,505.063332533912,-37.7212155100859)) ;
#56541 = CARTESIAN_POINT('Ctrl Pts',(31.3158637014097,505.075034591258,-37.8919333679364)) ;
#56542 = CARTESIAN_POINT('Ctrl Pts',(31.2407040325545,505.083174245486,-38.0047123934386)) ;
#56543 = CARTESIAN_POINT('Ctrl Pts',(31.1199440684997,505.095114223618,-38.145418171556)) ;
#56544 = CARTESIAN_POINT('Ctrl Pts',(31.085413035751,505.098423444659,-38.1821426676398)) ;
#56545 = CARTESIAN_POINT('Ctrl Pts',(31.0066437838756,505.105799002943,-38.2586487533931)) ;
#56546 = CARTESIAN_POINT('Ctrl Pts',(30.9618338916185,505.109889866297,-38.2977384194287)) ;
#56547 = CARTESIAN_POINT('Ctrl Pts',(30.8580579644143,505.119157797996,-38.3789211309444)) ;
#56548 = CARTESIAN_POINT('Ctrl Pts',(30.7982420997301,505.124369394691,-38.4197320168323)) ;
#56549 = CARTESIAN_POINT('Ctrl Pts',(30.6425261494663,505.137513556364,-38.5117311762407)) ;
#56550 = CARTESIAN_POINT('Ctrl Pts',(30.5439051631561,505.145481882937,-38.5576794254582)) ;
#56551 = CARTESIAN_POINT('Ctrl Pts',(30.4122557784069,505.155189801372,-38.6040029390564)) ;
#56552 = CARTESIAN_POINT('Ctrl Pts',(30.3827166441987,505.157308963363,-38.6134789835817)) ;
#56553 = CARTESIAN_POINT('Ctrl Pts',(30.3155720821077,505.161973058499,-38.6329679746827)) ;
#56554 = CARTESIAN_POINT('Ctrl Pts',(30.2778475830031,505.164493237266,-38.6424994365393)) ;
#56555 = CARTESIAN_POINT('Ctrl Pts',(30.1885140705319,505.170302414477,-38.6617695595558)) ;
#56556 = CARTESIAN_POINT('Ctrl Pts',(30.1367097335577,505.173549603447,-38.6704068862994)) ;
#56557 = CARTESIAN_POINT('Ctrl Pts',(29.9488542251005,505.185155725715,-38.6926682035512)) ;
#56558 = CARTESIAN_POINT('Ctrl Pts',(29.8116775425696,505.193362887803,-38.6919888024947)) ;
#56559 = CARTESIAN_POINT('Ctrl Pts',(29.624855350619,505.205444366386,-38.6679745984017)) ;
#56560 = CARTESIAN_POINT('Ctrl Pts',(29.5739237617302,505.208826330338,-38.6590021411539)) ;
#56561 = CARTESIAN_POINT('Ctrl Pts',(29.4675277637266,505.216127724888,-38.6351094876978)) ;
#56562 = CARTESIAN_POINT('Ctrl Pts',(29.41225300412,505.22006081354,-38.6196605510268)) ;
#56563 = CARTESIAN_POINT('Ctrl Pts',(29.2939961228177,505.228801051977,-38.5799251294602)) ;
#56564 = CARTESIAN_POINT('Ctrl Pts',(29.2314701995677,505.233633562076,-38.554600462466)) ;
#56565 = CARTESIAN_POINT('Ctrl Pts',(29.064866655393,505.247017025115,-38.4750474777764)) ;
#56566 = CARTESIAN_POINT('Ctrl Pts',(28.9647006331844,505.255656762407,-38.4135068552996)) ;
#56567 = CARTESIAN_POINT('Ctrl Pts',(28.8467901819903,505.266031924647,-38.3226744868733)) ;
#56568 = CARTESIAN_POINT('Ctrl Pts',(28.8223090351299,505.2681963671,-38.3026807437247)) ;
#56569 = CARTESIAN_POINT('Ctrl Pts',(28.7699718567068,505.272822773724,-38.2573941485137)) ;
#56570 = CARTESIAN_POINT('Ctrl Pts',(28.7423745303495,505.275265998877,-38.2318310516059)) ;
#56571 = CARTESIAN_POINT('Ctrl Pts',(28.6804139252238,505.280827135552,-38.1704113439542)) ;
#56572 = CARTESIAN_POINT('Ctrl Pts',(28.6467408006178,505.283908462598,-38.1339090892676)) ;
#56573 = CARTESIAN_POINT('Ctrl Pts',(28.5177073059866,505.296218322076,-37.9808440181915)) ;
#56574 = CARTESIAN_POINT('Ctrl Pts',(28.436728725186,505.305222181149,-37.853123558032)) ;
#56575 = CARTESIAN_POINT('Ctrl Pts',(28.3529740128628,505.318205848838,-37.6703728001715)) ;
#56576 = CARTESIAN_POINT('Ctrl Pts',(28.334040353043,505.321532015094,-37.6235526394832)) ;
#56577 = CARTESIAN_POINT('Ctrl Pts',(28.2966593623614,505.329109436808,-37.5174915946331)) ;
#56578 = CARTESIAN_POINT('Ctrl Pts',(28.2793370467759,505.333393656728,-37.4579373245657)) ;
#56579 = CARTESIAN_POINT('Ctrl Pts',(28.2288907648697,505.349207042725,-37.2398193604818)) ;
#56580 = CARTESIAN_POINT('Ctrl Pts',(28.2156013177303,505.361293063839,-37.0776284436838)) ;
#56581 = CARTESIAN_POINT('Ctrl Pts',(28.228191571231,505.375231915385,-36.8802928531777)) ;
#56582 = CARTESIAN_POINT('Ctrl Pts',(28.2316303213961,505.377718228363,-36.8445820480625)) ;
#56583 = CARTESIAN_POINT('Ctrl Pts',(28.2403577626611,505.382325518337,-36.7769292816497)) ;
#56584 = CARTESIAN_POINT('Ctrl Pts',(28.2454292806503,505.384455016644,-36.7449776845084)) ;
#56585 = CARTESIAN_POINT('Ctrl Pts',(28.2586443512131,505.389058212253,-36.674956229427)) ;
#56586 = CARTESIAN_POINT('Ctrl Pts',(28.2671984852559,505.39151304728,-36.6369818548884)) ;
#56587 = CARTESIAN_POINT('Ctrl Pts',(28.301076026269,505.399822747872,-36.5078679897967)) ;
#56588 = CARTESIAN_POINT('Ctrl Pts',(28.3328221189001,505.405512572982,-36.4186033051751)) ;
#56589 = CARTESIAN_POINT('Ctrl Pts',(28.4059772909885,505.41637075183,-36.2577331543419)) ;
#56590 = CARTESIAN_POINT('Ctrl Pts',(28.4454622972825,505.421493596654,-36.1855813807272)) ;
#56591 = CARTESIAN_POINT('Ctrl Pts',(28.5172672186643,505.430045411399,-36.0746905944075)) ;
#56592 = CARTESIAN_POINT('Ctrl Pts',(28.5463022170203,505.433346024103,-36.0339882514493)) ;
#56593 = CARTESIAN_POINT('Ctrl Pts',(28.6163113509271,505.441011148693,-35.9446353501423)) ;
#56594 = CARTESIAN_POINT('Ctrl Pts',(28.6583272987636,505.445415879141,-35.8969049674629)) ;
#56595 = CARTESIAN_POINT('Ctrl Pts',(28.7613552212687,505.455804280732,-35.7925477787027)) ;
#56596 = CARTESIAN_POINT('Ctrl Pts',(28.8240886310708,505.461845247271,-35.7378582062474)) ;
#56597 = CARTESIAN_POINT('Ctrl Pts',(28.9576212240075,505.473996343706,-35.6379754768635)) ;
#56598 = CARTESIAN_POINT('Ctrl Pts',(29.0282934864003,505.4800887769,-35.5929807957488)) ;
#56599 = CARTESIAN_POINT('Ctrl Pts',(29.1305594213015,505.488201968313,-35.53821748958)) ;
#56600 = CARTESIAN_POINT('Ctrl Pts',(29.159508920795,505.490424919367,-35.5237830352619)) ;
#56601 = CARTESIAN_POINT('Ctrl Pts',(29.2218806074471,505.495033449199,-35.4949204369125)) ;
#56602 = CARTESIAN_POINT('Ctrl Pts',(29.2553911764646,505.497406626614,-35.4807263531862)) ;
#56603 = CARTESIAN_POINT('Ctrl Pts',(29.3876437604648,505.506478834398,-35.4297500362299)) ;
#56604 = CARTESIAN_POINT('Ctrl Pts',(29.4893271533635,505.512841545071,-35.4012658788438)) ;
#56605 = CARTESIAN_POINT('Ctrl Pts',(29.6850219576468,505.525024427307,-35.3659962036172)) ;
#56606 = CARTESIAN_POINT('Ctrl Pts',(29.7782362896289,505.530803751587,-35.3571897627624)) ;
#56607 = CARTESIAN_POINT('Ctrl Pts',(29.9228101220036,505.540125589335,-35.3557286069205)) ;
#56608 = CARTESIAN_POINT('Ctrl Pts',(29.9739208018959,505.543487594534,-35.3575651743944)) ;
#56609 = CARTESIAN_POINT('Ctrl Pts',(30.0852175886486,505.550999961024,-35.3667036136506)) ;
#56610 = CARTESIAN_POINT('Ctrl Pts',(30.1452504613554,505.555176250007,-35.3749458216379)) ;
#56611 = CARTESIAN_POINT('Ctrl Pts',(30.2929665423896,505.56577908599,-35.4034977446196)) ;
#56612 = CARTESIAN_POINT('Ctrl Pts',(30.3797023347075,505.572304017086,-35.4276750353455)) ;
#56613 = CARTESIAN_POINT('Ctrl Pts',(30.4640543092331,505.578851962161,-35.4587264391634)) ;
#56614 = CARTESIAN_POINT('Origin',(29.888527625402,504.710565160562,-37.0221601717529)) ;
#56615 = CARTESIAN_POINT('',(30.4640904799732,504.178934308784,-35.4587397547064)) ;
#56616 = CARTESIAN_POINT('',(30.4640904797602,504.369620557053,-35.458739754628)) ;
#56617 = CARTESIAN_POINT('',(30.4640904799733,504.710565160562,-35.4587397547064)) ;
#56618 = CARTESIAN_POINT('',(29.8896377004414,504.139875734639,-35.3557043533874)) ;
#56619 = CARTESIAN_POINT('Ctrl Pts',(29.8896184786969,504.140137457474,-35.3561605288841)) ;
#56620 = CARTESIAN_POINT('Ctrl Pts',(29.9354901762523,504.143454067397,-35.3561905644802)) ;
#56621 = CARTESIAN_POINT('Ctrl Pts',(29.9813446690112,504.146743004584,-35.3581151472982)) ;
#56622 = CARTESIAN_POINT('Ctrl Pts',(30.0577028173439,504.152121209803,-35.3644868009658)) ;
#56623 = CARTESIAN_POINT('Ctrl Pts',(30.0882673386681,504.154247226243,-35.3678912625542)) ;
#56624 = CARTESIAN_POINT('Ctrl Pts',(30.1501713170452,504.158475770452,-35.3765275127624)) ;
#56625 = CARTESIAN_POINT('Ctrl Pts',(30.1814886437172,504.160570984008,-35.3818131807617)) ;
#56626 = CARTESIAN_POINT('Ctrl Pts',(30.2982115134967,504.168273320549,-35.4049631832909)) ;
#56627 = CARTESIAN_POINT('Ctrl Pts',(30.3822863928015,504.173613655647,-35.4286241227147)) ;
#56628 = CARTESIAN_POINT('Ctrl Pts',(30.4640904799732,504.178934308784,-35.4587397547064)) ;
#56629 = CARTESIAN_POINT('',(30.967886278449,503.710565160562,-38.2912310516064)) ;
#56630 = CARTESIAN_POINT('Ctrl Pts',(29.8896377004414,504.13987573464,-35.3557043533874)) ;
#56631 = CARTESIAN_POINT('Ctrl Pts',(29.8297753933383,504.135625997494,-35.3557985198437)) ;
#56632 = CARTESIAN_POINT('Ctrl Pts',(29.7698127451484,504.131337054551,-35.3591450254465)) ;
#56633 = CARTESIAN_POINT('Ctrl Pts',(29.7101270449706,504.127068870349,-35.3657190559218)) ;
#56634 = CARTESIAN_POINT('Ctrl Pts',(29.6505061160716,504.122805318007,-35.3722859522198)) ;
#56635 = CARTESIAN_POINT('Ctrl Pts',(29.5911614984541,504.118562737948,-35.3820731346348)) ;
#56636 = CARTESIAN_POINT('Ctrl Pts',(29.5324607005304,504.114380610146,-35.3950189269347)) ;
#56637 = CARTESIAN_POINT('Ctrl Pts',(29.4738005852685,504.110201380773,-35.4079557471369)) ;
#56638 = CARTESIAN_POINT('Ctrl Pts',(29.4157834169584,504.106082618206,-35.4240467306655)) ;
#56639 = CARTESIAN_POINT('Ctrl Pts',(29.3587675571641,504.102040827175,-35.4431956488098)) ;
#56640 = CARTESIAN_POINT('Ctrl Pts',(29.3017686658876,504.098000239025,-35.4623388680352)) ;
#56641 = CARTESIAN_POINT('Ctrl Pts',(29.2457705803453,504.094036554324,-35.4845382446598)) ;
#56642 = CARTESIAN_POINT('Ctrl Pts',(29.1911221195583,504.090142823904,-35.5096631290411)) ;
#56643 = CARTESIAN_POINT('Ctrl Pts',(29.1364297668549,504.086245966163,-35.5348081929353)) ;
#56644 = CARTESIAN_POINT('Ctrl Pts',(29.0830893815187,504.082419037368,-35.5628836052255)) ;
#56645 = CARTESIAN_POINT('Ctrl Pts',(29.0314393914955,504.078632770265,-35.5937224525954)) ;
#56646 = CARTESIAN_POINT('Ctrl Pts',(28.9797702420691,504.074845098657,-35.6245727395399)) ;
#56647 = CARTESIAN_POINT('Ctrl Pts',(28.9297930245083,504.071097829093,-35.6581887352351)) ;
#56648 = CARTESIAN_POINT('Ctrl Pts',(28.8818319358433,504.067342520788,-35.6943646557727)) ;
#56649 = CARTESIAN_POINT('Ctrl Pts',(28.8337820826919,504.063580262306,-35.7306075292737)) ;
#56650 = CARTESIAN_POINT('Ctrl Pts',(28.7877563004684,504.059809445068,-35.7694201009957)) ;
#56651 = CARTESIAN_POINT('Ctrl Pts',(28.7440603511994,504.055967948101,-35.8105526977708)) ;
#56652 = CARTESIAN_POINT('Ctrl Pts',(28.705798343014,504.052604172034,-35.8465701268648)) ;
#56653 = CARTESIAN_POINT('Ctrl Pts',(28.6693227631056,504.049185674405,-35.884365880256)) ;
#56654 = CARTESIAN_POINT('Ctrl Pts',(28.6348207573405,504.045667820509,-35.923743040089)) ;
#56655 = CARTESIAN_POINT('Ctrl Pts',(28.6347996521938,504.04566566861,-35.9237671274057)) ;
#56656 = CARTESIAN_POINT('Ctrl Pts',(28.634778547784,504.045663516674,-35.9237912153142)) ;
#56657 = CARTESIAN_POINT('Ctrl Pts',(28.6347574441113,504.045661364701,-35.9238153038146)) ;
#56658 = CARTESIAN_POINT('Ctrl Pts',(28.5981591185791,504.041929378649,-35.9655899651101)) ;
#56659 = CARTESIAN_POINT('Ctrl Pts',(28.5636425667076,504.038075115991,-36.0093123926301)) ;
#56660 = CARTESIAN_POINT('Ctrl Pts',(28.5313906856171,504.034162047438,-36.0547326419516)) ;
#56661 = CARTESIAN_POINT('Ctrl Pts',(28.5284605915725,504.033806543868,-36.0588590865973)) ;
#56662 = CARTESIAN_POINT('Ctrl Pts',(28.5255491912652,504.033450554927,-36.0629995091889)) ;
#56663 = CARTESIAN_POINT('Ctrl Pts',(28.5226566222899,504.033094128209,-36.0671537010576)) ;
#56664 = CARTESIAN_POINT('Ctrl Pts',(28.4874936832043,504.028761297747,-36.1176533077655)) ;
#56665 = CARTESIAN_POINT('Ctrl Pts',(28.4551128729339,504.024364436927,-36.1701936196456)) ;
#56666 = CARTESIAN_POINT('Ctrl Pts',(28.4257146889389,504.019974570264,-36.2244200807017)) ;
#56667 = CARTESIAN_POINT('Ctrl Pts',(28.3967551490687,504.015650203879,-36.2778374401289)) ;
#56668 = CARTESIAN_POINT('Ctrl Pts',(28.3706894657574,504.011332903179,-36.3328908853468)) ;
#56669 = CARTESIAN_POINT('Ctrl Pts',(28.347671913857,504.007069816351,-36.3892303890599)) ;
#56670 = CARTESIAN_POINT('Ctrl Pts',(28.3246677347717,504.002809206305,-36.4455371604577)) ;
#56671 = CARTESIAN_POINT('Ctrl Pts',(28.3047080218695,503.99860287837,-36.503128477941)) ;
#56672 = CARTESIAN_POINT('Ctrl Pts',(28.2879130843532,503.994473983533,-36.561644641388)) ;
#56673 = CARTESIAN_POINT('Ctrl Pts',(28.2711216353392,503.990345946314,-36.6201486503526)) ;
#56674 = CARTESIAN_POINT('Ctrl Pts',(28.2574936850388,503.98629530977,-36.6795771107382)) ;
#56675 = CARTESIAN_POINT('Ctrl Pts',(28.2471163804212,503.982320348983,-36.7395604484235)) ;
#56676 = CARTESIAN_POINT('Ctrl Pts',(28.2364520430735,503.978235442128,-36.8012029049085)) ;
#56677 = CARTESIAN_POINT('Ctrl Pts',(28.2292210259891,503.974230442421,-36.8634313832066)) ;
#56678 = CARTESIAN_POINT('Ctrl Pts',(28.2254797132738,503.970277107139,-36.9258339304508)) ;
#56679 = CARTESIAN_POINT('Ctrl Pts',(28.2218341075122,503.966424902584,-36.9866401509081)) ;
#56680 = CARTESIAN_POINT('Ctrl Pts',(28.221502112962,503.962621381447,-37.0476115487152)) ;
#56681 = CARTESIAN_POINT('Ctrl Pts',(28.2244967250289,503.95881892442,-37.1083574943258)) ;
#56682 = CARTESIAN_POINT('Ctrl Pts',(28.227609262024,503.95486673031,-37.1714955565514)) ;
#56683 = CARTESIAN_POINT('Ctrl Pts',(28.2343164508115,503.950915257385,-37.2343899285392)) ;
#56684 = CARTESIAN_POINT('Ctrl Pts',(28.2445814813765,503.946893154926,-37.2965930716829)) ;
#56685 = CARTESIAN_POINT('Ctrl Pts',(28.253439112898,503.943422507539,-37.3502677800003)) ;
#56686 = CARTESIAN_POINT('Ctrl Pts',(28.2649458444713,503.939898607407,-37.4034287902758)) ;
#56687 = CARTESIAN_POINT('Ctrl Pts',(28.2790394292767,503.936270853637,-37.4557822181718)) ;
#56688 = CARTESIAN_POINT('Ctrl Pts',(28.2812698280105,503.93569673871,-37.4640674785155)) ;
#56689 = CARTESIAN_POINT('Ctrl Pts',(28.283564971728,503.935120022762,-37.4723326100216)) ;
#56690 = CARTESIAN_POINT('Ctrl Pts',(28.2859245682816,503.934540505235,-37.4805765589885)) ;
#56691 = CARTESIAN_POINT('Ctrl Pts',(28.2859340333552,503.93453818061,-37.4806096280249)) ;
#56692 = CARTESIAN_POINT('Ctrl Pts',(28.285943499466,503.934535855941,-37.4806426967205)) ;
#56693 = CARTESIAN_POINT('Ctrl Pts',(28.2859529666137,503.934533531226,-37.4806757650752)) ;
#56694 = CARTESIAN_POINT('Ctrl Pts',(28.3010863252409,503.930817444538,-37.5335359597196)) ;
#56695 = CARTESIAN_POINT('Ctrl Pts',(28.3189345818505,503.92697587446,-37.5857212719082)) ;
#56696 = CARTESIAN_POINT('Ctrl Pts',(28.3393907908243,503.923071646374,-37.6369487425217)) ;
#56697 = CARTESIAN_POINT('Ctrl Pts',(28.3413817859688,503.92269164932,-37.6419346930168)) ;
#56698 = CARTESIAN_POINT('Ctrl Pts',(28.3433974527172,503.922311058702,-37.6469115468851)) ;
#56699 = CARTESIAN_POINT('Ctrl Pts',(28.3454376703857,503.921929932447,-37.6518790289816)) ;
#56700 = CARTESIAN_POINT('Ctrl Pts',(28.3688150453601,503.917562883034,-37.7087978045812)) ;
#56701 = CARTESIAN_POINT('Ctrl Pts',(28.3954206204328,503.913126205515,-37.7644899055475)) ;
#56702 = CARTESIAN_POINT('Ctrl Pts',(28.4250648367456,503.908693208131,-37.818592175824)) ;
#56703 = CARTESIAN_POINT('Ctrl Pts',(28.4541506235245,503.904343718324,-37.8716752825222)) ;
#56704 = CARTESIAN_POINT('Ctrl Pts',(28.4861612781874,503.89999805442,-37.9232282038626)) ;
#56705 = CARTESIAN_POINT('Ctrl Pts',(28.5208878521764,503.895705217961,-37.9729335687876)) ;
#56706 = CARTESIAN_POINT('Ctrl Pts',(28.5555926701839,503.891415070938,-38.0226077936124)) ;
#56707 = CARTESIAN_POINT('Ctrl Pts',(28.5930099109725,503.887177827747,-38.070436872033)) ;
#56708 = CARTESIAN_POINT('Ctrl Pts',(28.632904056294,503.883018826242,-38.1161269601138)) ;
#56709 = CARTESIAN_POINT('Ctrl Pts',(28.6727883861652,503.878860848006,-38.1618058067258)) ;
#56710 = CARTESIAN_POINT('Ctrl Pts',(28.7151484004903,503.874781083488,-38.2053466799925)) ;
#56711 = CARTESIAN_POINT('Ctrl Pts',(28.7597224631518,503.870780171933,-38.2464784466566)) ;
#56712 = CARTESIAN_POINT('Ctrl Pts',(28.8058511114513,503.866639722734,-38.2890447438503)) ;
#56713 = CARTESIAN_POINT('Ctrl Pts',(28.8543511747747,503.862583755205,-38.3290306366314)) ;
#56714 = CARTESIAN_POINT('Ctrl Pts',(28.904902504156,503.858585955385,-38.366162618192)) ;
#56715 = CARTESIAN_POINT('Ctrl Pts',(28.9538149356172,503.854717766119,-38.4020907634124)) ;
#56716 = CARTESIAN_POINT('Ctrl Pts',(29.0046477380894,503.850903652708,-38.435346900776)) ;
#56717 = CARTESIAN_POINT('Ctrl Pts',(29.0570822240754,503.847097973371,-38.4657111295024)) ;
#56718 = CARTESIAN_POINT('Ctrl Pts',(29.1121520759834,503.843101019962,-38.4976014693774)) ;
#56719 = CARTESIAN_POINT('Ctrl Pts',(29.1689890816134,503.839112995089,-38.5263010170895)) ;
#56720 = CARTESIAN_POINT('Ctrl Pts',(29.2271883953978,503.835061793906,-38.5515944752049)) ;
#56721 = CARTESIAN_POINT('Ctrl Pts',(29.2773215666856,503.83157206955,-38.573382382754)) ;
#56722 = CARTESIAN_POINT('Ctrl Pts',(29.3284664523474,503.828034803596,-38.5926434539553)) ;
#56723 = CARTESIAN_POINT('Ctrl Pts',(29.3803377593518,503.82439820022,-38.609269748101)) ;
#56724 = CARTESIAN_POINT('Ctrl Pts',(29.3886653951022,503.823814364762,-38.6119390026372)) ;
#56725 = CARTESIAN_POINT('Ctrl Pts',(29.397011815879,503.823227968938,-38.6145404372129)) ;
#56726 = CARTESIAN_POINT('Ctrl Pts',(29.4053759153336,503.822638798422,-38.6170737064832)) ;
#56727 = CARTESIAN_POINT('Ctrl Pts',(29.4053941577726,503.822637513417,-38.6170792316459)) ;
#56728 = CARTESIAN_POINT('Ctrl Pts',(29.4054124002957,503.822636228399,-38.6170847564843)) ;
#56729 = CARTESIAN_POINT('Ctrl Pts',(29.4054306429029,503.822634943368,-38.6170902809985)) ;
#56730 = CARTESIAN_POINT('Ctrl Pts',(29.4592170276719,503.81884616597,-38.6333787228135)) ;
#56731 = CARTESIAN_POINT('Ctrl Pts',(29.5139259802935,503.814932714415,-38.6468980394685)) ;
#56732 = CARTESIAN_POINT('Ctrl Pts',(29.5692502182216,503.810956908925,-38.6575858894562)) ;
#56733 = CARTESIAN_POINT('Ctrl Pts',(29.5748385967441,503.810555307261,-38.6586654841069)) ;
#56734 = CARTESIAN_POINT('Ctrl Pts',(29.5804332126718,503.81015306938,-38.6597162051964)) ;
#56735 = CARTESIAN_POINT('Ctrl Pts',(29.5860337223545,503.809750259515,-38.660738000437)) ;
#56736 = CARTESIAN_POINT('Ctrl Pts',(29.6469489136165,503.80536900827,-38.67185178401)) ;
#56737 = CARTESIAN_POINT('Ctrl Pts',(29.7085670930393,503.800920726721,-38.6795417607742)) ;
#56738 = CARTESIAN_POINT('Ctrl Pts',(29.7704837692506,503.796474702529,-38.6837728553795)) ;
#56739 = CARTESIAN_POINT('Ctrl Pts',(29.8323235206938,503.792034202041,-38.6879986933076)) ;
#56740 = CARTESIAN_POINT('Ctrl Pts',(29.8944611253984,503.787596294557,-38.6887746071938)) ;
#56741 = CARTESIAN_POINT('Ctrl Pts',(29.9564992329331,503.783209433205,-38.6861039974028)) ;
#56742 = CARTESIAN_POINT('Ctrl Pts',(30.0184797152543,503.778826646668,-38.6834358682558)) ;
#56743 = CARTESIAN_POINT('Ctrl Pts',(30.0803609695488,503.774494948293,-38.6773277365287)) ;
#56744 = CARTESIAN_POINT('Ctrl Pts',(30.1417509253501,503.770238601661,-38.6678177012168)) ;
#56745 = CARTESIAN_POINT('Ctrl Pts',(30.2031030876977,503.76598487536,-38.658313520561)) ;
#56746 = CARTESIAN_POINT('Ctrl Pts',(30.2639645733628,503.761806401157,-38.6454115696398)) ;
#56747 = CARTESIAN_POINT('Ctrl Pts',(30.3239474239815,503.757702423242,-38.6291841121664)) ;
#56748 = CARTESIAN_POINT('Ctrl Pts',(30.3839350510104,503.753598118529,-38.6129553625071)) ;
#56749 = CARTESIAN_POINT('Ctrl Pts',(30.443043836497,503.749568187684,-38.5934003812633)) ;
#56750 = CARTESIAN_POINT('Ctrl Pts',(30.5008894752955,503.745587935094,-38.5706275931094)) ;
#56751 = CARTESIAN_POINT('Ctrl Pts',(30.5587325885659,503.741607856281,-38.5478557992106)) ;
#56752 = CARTESIAN_POINT('Ctrl Pts',(30.6153124825885,503.737677158926,-38.521866155478)) ;
#56753 = CARTESIAN_POINT('Ctrl Pts',(30.6702504661428,503.733750371915,-38.4928071097867)) ;
#56754 = CARTESIAN_POINT('Ctrl Pts',(30.7252423704966,503.729819730822,-38.4637195430818)) ;
#56755 = CARTESIAN_POINT('Ctrl Pts',(30.7785887549332,503.725892503731,-38.4315561080091)) ;
#56756 = CARTESIAN_POINT('Ctrl Pts',(30.8299195396226,503.721908177903,-38.3965115879629)) ;
#56757 = CARTESIAN_POINT('Ctrl Pts',(30.8777544982746,503.718195200156,-38.3638537360025)) ;
#56758 = CARTESIAN_POINT('Ctrl Pts',(30.9238386672376,503.714431986771,-38.3286940263402)) ;
#56759 = CARTESIAN_POINT('Ctrl Pts',(30.9678862784492,503.710565160562,-38.2912310516066)) ;
#56760 = CARTESIAN_POINT('',(30.9857908490243,503.71057263878,-35.7673864800448)) ;
#56761 = CARTESIAN_POINT('Origin',(29.8885276254018,503.710565160562,-37.0221601717529)) ;
#56762 = CARTESIAN_POINT('',(29.8893873868701,504.332876521313,-35.3566407257823)) ;
#56763 = CARTESIAN_POINT('Ctrl Pts',(30.9857908596378,503.710572638919,-35.7673864679078)) ;
#56764 = CARTESIAN_POINT('Ctrl Pts',(31.025599741794,503.714185585541,-35.8022396077763)) ;
#56765 = CARTESIAN_POINT('Ctrl Pts',(31.0637788842238,503.717896060089,-35.8390918157986)) ;
#56766 = CARTESIAN_POINT('Ctrl Pts',(31.1001381250373,503.721649614921,-35.8777491764167)) ;
#56767 = CARTESIAN_POINT('Ctrl Pts',(31.1415669230504,503.725926526691,-35.9217965203363)) ;
#56768 = CARTESIAN_POINT('Ctrl Pts',(31.1806337273785,503.730258808275,-35.9681884647833)) ;
#56769 = CARTESIAN_POINT('Ctrl Pts',(31.2170981387204,503.734580331867,-36.0166217211997)) ;
#56770 = CARTESIAN_POINT('Ctrl Pts',(31.2535253724787,503.738897449415,-36.0650055971003)) ;
#56771 = CARTESIAN_POINT('Ctrl Pts',(31.287355798737,503.743203532846,-36.1154264921043)) ;
#56772 = CARTESIAN_POINT('Ctrl Pts',(31.3183839884289,503.74745340768,-36.1675649384462)) ;
#56773 = CARTESIAN_POINT('Ctrl Pts',(31.3493923171067,503.751700562187,-36.2196700111873)) ;
#56774 = CARTESIAN_POINT('Ctrl Pts',(31.3776020907355,503.755891461803,-36.2734903980026)) ;
#56775 = CARTESIAN_POINT('Ctrl Pts',(31.4028396878627,503.760004805882,-36.3286913402369)) ;
#56776 = CARTESIAN_POINT('Ctrl Pts',(31.4280707067097,503.764117077802,-36.3838778941257)) ;
#56777 = CARTESIAN_POINT('Ctrl Pts',(31.4503310408738,503.76815184398,-36.4404442728615)) ;
#56778 = CARTESIAN_POINT('Ctrl Pts',(31.4694783634939,503.772112390693,-36.4980404193198)) ;
#56779 = CARTESIAN_POINT('Ctrl Pts',(31.4886418197309,503.77607627458,-36.55568509654)) ;
#56780 = CARTESIAN_POINT('Ctrl Pts',(31.5046868209787,503.779965937745,-36.6143612760132)) ;
#56781 = CARTESIAN_POINT('Ctrl Pts',(31.5175038014117,503.783808307049,-36.6737025049001)) ;
#56782 = CARTESIAN_POINT('Ctrl Pts',(31.5303255958451,503.78765211953,-36.7330660220873)) ;
#56783 = CARTESIAN_POINT('Ctrl Pts',(31.5399166051113,503.791448875589,-36.7930950710586)) ;
#56784 = CARTESIAN_POINT('Ctrl Pts',(31.5462042483842,503.795246235159,-36.8534073790127)) ;
#56785 = CARTESIAN_POINT('Ctrl Pts',(31.5525038375664,503.799050809343,-36.9138342744737)) ;
#56786 = CARTESIAN_POINT('Ctrl Pts',(31.5554869660787,503.802856462993,-36.9745454079707)) ;
#56787 = CARTESIAN_POINT('Ctrl Pts',(31.5551243998437,503.80672636773,-37.0351416171265)) ;
#56788 = CARTESIAN_POINT('Ctrl Pts',(31.5547985760722,503.810204096306,-37.0895970062231)) ;
#56789 = CARTESIAN_POINT('Ctrl Pts',(31.5517708491299,503.813734302681,-37.1439599822949)) ;
#56790 = CARTESIAN_POINT('Ctrl Pts',(31.5460566864391,503.817367336672,-37.1979305182359)) ;
#56791 = CARTESIAN_POINT('Ctrl Pts',(31.5455422591127,503.817694406807,-37.202789308581)) ;
#56792 = CARTESIAN_POINT('Ctrl Pts',(31.5450060776737,503.818022310341,-37.2076449476738)) ;
#56793 = CARTESIAN_POINT('Ctrl Pts',(31.5444481642713,503.81835108401,-37.2124972343404)) ;
#56794 = CARTESIAN_POINT('Ctrl Pts',(31.5444444975928,503.818353244753,-37.2125291241909)) ;
#56795 = CARTESIAN_POINT('Ctrl Pts',(31.5444408299757,503.818355405533,-37.2125610138967)) ;
#56796 = CARTESIAN_POINT('Ctrl Pts',(31.54443716142,503.818357566351,-37.2125929034576)) ;
#56797 = CARTESIAN_POINT('Ctrl Pts',(31.5380899299618,503.822096152456,-37.2677673207176)) ;
#56798 = CARTESIAN_POINT('Ctrl Pts',(31.5289015841708,503.825957158538,-37.3227066992381)) ;
#56799 = CARTESIAN_POINT('Ctrl Pts',(31.5169344347899,503.829877527874,-37.3771083831853)) ;
#56800 = CARTESIAN_POINT('Ctrl Pts',(31.515821033412,503.830242271764,-37.3821698149383)) ;
#56801 = CARTESIAN_POINT('Ctrl Pts',(31.5146836050773,503.830607529508,-37.3872265662973)) ;
#56802 = CARTESIAN_POINT('Ctrl Pts',(31.5135222167086,503.830973250324,-37.3922783779415)) ;
#56803 = CARTESIAN_POINT('Ctrl Pts',(31.49973941815,503.835313449062,-37.45223084873)) ;
#56804 = CARTESIAN_POINT('Ctrl Pts',(31.4825781631431,503.839718206081,-37.5114921005573)) ;
#56805 = CARTESIAN_POINT('Ctrl Pts',(31.4621662833962,503.844116716503,-37.5696766912456)) ;
#56806 = CARTESIAN_POINT('Ctrl Pts',(31.4420144640731,503.848459187085,-37.6271199729757)) ;
#56807 = CARTESIAN_POINT('Ctrl Pts',(31.4186946915218,503.852795277295,-37.6835140848051)) ;
#56808 = CARTESIAN_POINT('Ctrl Pts',(31.3923633244276,503.857077398012,-37.7385084890886)) ;
#56809 = CARTESIAN_POINT('Ctrl Pts',(31.3660478185768,503.861356939305,-37.7934697663558)) ;
#56810 = CARTESIAN_POINT('Ctrl Pts',(31.3367244447431,503.865582441056,-37.8470331064885)) ;
#56811 = CARTESIAN_POINT('Ctrl Pts',(31.3045795269098,503.869730209488,-37.898866740617)) ;
#56812 = CARTESIAN_POINT('Ctrl Pts',(31.2724421101615,503.873877010031,-37.9506882792568)) ;
#56813 = CARTESIAN_POINT('Ctrl Pts',(31.2374844484629,503.877946111568,-38.0007808877875)) ;
#56814 = CARTESIAN_POINT('Ctrl Pts',(31.1999224196693,503.881938636219,-38.048830770933)) ;
#56815 = CARTESIAN_POINT('Ctrl Pts',(31.1614664592841,503.886026178206,-38.0980241841244)) ;
#56816 = CARTESIAN_POINT('Ctrl Pts',(31.1202804556097,503.890033481837,-38.1450762515352)) ;
#56817 = CARTESIAN_POINT('Ctrl Pts',(31.0766293059828,503.893987742501,-38.18967092766)) ;
#56818 = CARTESIAN_POINT('Ctrl Pts',(31.0339382825784,503.897855027463,-38.2332847242824)) ;
#56819 = CARTESIAN_POINT('Ctrl Pts',(30.9888893079486,503.901671931168,-38.2745478434933)) ;
#56820 = CARTESIAN_POINT('Ctrl Pts',(30.9417634312189,503.905485337521,-38.3131871643293)) ;
#56821 = CARTESIAN_POINT('Ctrl Pts',(30.8930477545831,503.909427389822,-38.3531299895858)) ;
#56822 = CARTESIAN_POINT('Ctrl Pts',(30.8421122291399,503.913366135261,-38.3902682995096)) ;
#56823 = CARTESIAN_POINT('Ctrl Pts',(30.7893076246311,503.917370974311,-38.4243317308909)) ;
#56824 = CARTESIAN_POINT('Ctrl Pts',(30.7433662941329,503.920855284745,-38.4539677706559)) ;
#56825 = CARTESIAN_POINT('Ctrl Pts',(30.6960094976692,503.92439027392,-38.4812768971128)) ;
#56826 = CARTESIAN_POINT('Ctrl Pts',(30.6474988141172,503.928026555932,-38.506105537957)) ;
#56827 = CARTESIAN_POINT('Ctrl Pts',(30.6402786321784,503.928567769038,-38.5098009570083)) ;
#56828 = CARTESIAN_POINT('Ctrl Pts',(30.6330328503057,503.929111226026,-38.5134415132153)) ;
#56829 = CARTESIAN_POINT('Ctrl Pts',(30.6257622879721,503.929657093778,-38.5170267894782)) ;
#56830 = CARTESIAN_POINT('Ctrl Pts',(30.625735166798,503.929659130013,-38.5170401635333)) ;
#56831 = CARTESIAN_POINT('Ctrl Pts',(30.6257080452791,503.929661166282,-38.5170535368193)) ;
#56832 = CARTESIAN_POINT('Ctrl Pts',(30.6256809234154,503.929663202584,-38.5170669093361)) ;
#56833 = CARTESIAN_POINT('Ctrl Pts',(30.5759590614946,503.933396306572,-38.5415824235088)) ;
#56834 = CARTESIAN_POINT('Ctrl Pts',(30.5248965668603,503.937251977912,-38.563593125864)) ;
#56835 = CARTESIAN_POINT('Ctrl Pts',(30.4727804230394,503.941166994424,-38.5829869725566)) ;
#56836 = CARTESIAN_POINT('Ctrl Pts',(30.467948435261,503.941529978148,-38.5847850877533)) ;
#56837 = CARTESIAN_POINT('Ctrl Pts',(30.4631074261961,503.941893472015,-38.586560716022)) ;
#56838 = CARTESIAN_POINT('Ctrl Pts',(30.458257646515,503.942257425637,-38.5883137735758)) ;
#56839 = CARTESIAN_POINT('Ctrl Pts',(30.400390604308,503.946600080566,-38.6092310651075)) ;
#56840 = CARTESIAN_POINT('Ctrl Pts',(30.3412689458996,503.951007524468,-38.6269340433287)) ;
#56841 = CARTESIAN_POINT('Ctrl Pts',(30.2812868347915,503.955408377488,-38.6413200789142)) ;
#56842 = CARTESIAN_POINT('Ctrl Pts',(30.2222048256791,503.959743190542,-38.6554902351465)) ;
#56843 = CARTESIAN_POINT('Ctrl Pts',(30.162288003225,503.96407132633,-38.6664426977938)) ;
#56844 = CARTESIAN_POINT('Ctrl Pts',(30.1019142031018,503.968345126172,-38.674118429795)) ;
#56845 = CARTESIAN_POINT('Ctrl Pts',(30.0415778315493,503.972616276483,-38.6817894032474)) ;
#56846 = CARTESIAN_POINT('Ctrl Pts',(29.9807850354928,503.976833024217,-38.6861878342942)) ;
#56847 = CARTESIAN_POINT('Ctrl Pts',(29.9199142353892,503.980971573472,-38.6872900336216)) ;
#56848 = CARTESIAN_POINT('Ctrl Pts',(29.8590584670246,503.985109100733,-38.6883919607665)) ;
#56849 = CARTESIAN_POINT('Ctrl Pts',(29.7981247542624,503.989168466053,-38.6861992518199)) ;
#56850 = CARTESIAN_POINT('Ctrl Pts',(29.7374924867608,503.993150647898,-38.6807228087513)) ;
#56851 = CARTESIAN_POINT('Ctrl Pts',(29.675167154414,503.99724402618,-38.6750934442497)) ;
#56852 = CARTESIAN_POINT('Ctrl Pts',(29.6131604094991,504.001255859216,-38.6659940414399)) ;
#56853 = CARTESIAN_POINT('Ctrl Pts',(29.5518849590064,504.005213532141,-38.6534761480589)) ;
#56854 = CARTESIAN_POINT('Ctrl Pts',(29.492198149365,504.009068597565,-38.6412827963442)) ;
#56855 = CARTESIAN_POINT('Ctrl Pts',(29.4332053466138,504.012872642956,-38.6258457871656)) ;
#56856 = CARTESIAN_POINT('Ctrl Pts',(29.375287021516,504.016672451451,-38.6072529623585)) ;
#56857 = CARTESIAN_POINT('Ctrl Pts',(29.3150563408614,504.020623965097,-38.5879178297986)) ;
#56858 = CARTESIAN_POINT('Ctrl Pts',(29.2559880036878,504.02457131541,-38.5651690412425)) ;
#56859 = CARTESIAN_POINT('Ctrl Pts',(29.1985052067541,504.028585110261,-38.5391572294889)) ;
#56860 = CARTESIAN_POINT('Ctrl Pts',(29.1487782751464,504.032057343915,-38.5166550609609)) ;
#56861 = CARTESIAN_POINT('Ctrl Pts',(29.1002369640037,504.035579960012,-38.4917107520701)) ;
#56862 = CARTESIAN_POINT('Ctrl Pts',(29.053151280261,504.039203629908,-38.4644609317492)) ;
#56863 = CARTESIAN_POINT('Ctrl Pts',(29.04583309661,504.039766830432,-38.4602256913595)) ;
#56864 = CARTESIAN_POINT('Ctrl Pts',(29.0385499740892,504.040332472034,-38.4559347740699)) ;
#56865 = CARTESIAN_POINT('Ctrl Pts',(29.0313028138539,504.040900744955,-38.4515887068868)) ;
#56866 = CARTESIAN_POINT('Ctrl Pts',(29.0312773349585,504.040902742836,-38.4515734273859)) ;
#56867 = CARTESIAN_POINT('Ctrl Pts',(29.0312518565074,504.04090474075,-38.4515581472033)) ;
#56868 = CARTESIAN_POINT('Ctrl Pts',(29.0312263785009,504.040906738696,-38.4515428663391)) ;
#56869 = CARTESIAN_POINT('Ctrl Pts',(28.9836891917994,504.044634532379,-38.4230316367382)) ;
#56870 = CARTESIAN_POINT('Ctrl Pts',(28.937532068309,504.04848544368,-38.3920373753948)) ;
#56871 = CARTESIAN_POINT('Ctrl Pts',(28.8930043403531,504.052396327771,-38.3587407430544)) ;
#56872 = CARTESIAN_POINT('Ctrl Pts',(28.8888399002697,504.052762091829,-38.3556266872351)) ;
#56873 = CARTESIAN_POINT('Ctrl Pts',(28.8846897251509,504.053128380461,-38.3524925282806)) ;
#56874 = CARTESIAN_POINT('Ctrl Pts',(28.8805540263586,504.05349514201,-38.3493384360104)) ;
#56875 = CARTESIAN_POINT('Ctrl Pts',(28.8316288596092,504.057833917845,-38.3120256388237)) ;
#56876 = CARTESIAN_POINT('Ctrl Pts',(28.7847271856301,504.062238210287,-38.2719177104918)) ;
#56877 = CARTESIAN_POINT('Ctrl Pts',(28.7401483956201,504.066636623972,-38.2292905661611)) ;
#56878 = CARTESIAN_POINT('Ctrl Pts',(28.6962098818012,504.070971864126,-38.1872756669273)) ;
#56879 = CARTESIAN_POINT('Ctrl Pts',(28.6545276339809,504.075301106021,-38.1428136461075)) ;
#56880 = CARTESIAN_POINT('Ctrl Pts',(28.6153560262653,504.079576524087,-38.0961907454377)) ;
#56881 = CARTESIAN_POINT('Ctrl Pts',(28.5762084777309,504.083849316194,-38.0495964805294)) ;
#56882 = CARTESIAN_POINT('Ctrl Pts',(28.5395683694364,504.088068215286,-38.0008440466416)) ;
#56883 = CARTESIAN_POINT('Ctrl Pts',(28.505660616964,504.092209273672,-37.9502392578844)) ;
#56884 = CARTESIAN_POINT('Ctrl Pts',(28.4717610838035,504.096349328258,-37.8996467358365)) ;
#56885 = CARTESIAN_POINT('Ctrl Pts',(28.4405926183445,504.100411577183,-37.847202756189)) ;
#56886 = CARTESIAN_POINT('Ctrl Pts',(28.4123515590043,504.104396876594,-37.7932326286487)) ;
#56887 = CARTESIAN_POINT('Ctrl Pts',(28.3833551024332,504.108488775552,-37.7378188978635)) ;
#56888 = CARTESIAN_POINT('Ctrl Pts',(28.3574450825579,504.112499566624,-37.6807961546299)) ;
#56889 = CARTESIAN_POINT('Ctrl Pts',(28.3348011177148,504.116456433674,-37.6225384285027)) ;
#56890 = CARTESIAN_POINT('Ctrl Pts',(28.3127189071721,504.120315138274,-37.5657259673018)) ;
#56891 = CARTESIAN_POINT('Ctrl Pts',(28.2937429000415,504.124122924579,-37.5077390823149)) ;
#56892 = CARTESIAN_POINT('Ctrl Pts',(28.2780053966865,504.127926506306,-37.4489455837021)) ;
#56893 = CARTESIAN_POINT('Ctrl Pts',(28.2616673685219,504.131875228284,-37.387908593618)) ;
#56894 = CARTESIAN_POINT('Ctrl Pts',(28.2488205811515,504.135819839118,-37.3260021173562)) ;
#56895 = CARTESIAN_POINT('Ctrl Pts',(28.2395672492876,504.139830550969,-37.2636616964272)) ;
#56896 = CARTESIAN_POINT('Ctrl Pts',(28.2315460959638,504.143307194318,-37.2096225587529)) ;
#56897 = CARTESIAN_POINT('Ctrl Pts',(28.2262248196662,504.146834162073,-37.1552564547135)) ;
#56898 = CARTESIAN_POINT('Ctrl Pts',(28.2236349801933,504.150462192433,-37.1008648994454)) ;
#56899 = CARTESIAN_POINT('Ctrl Pts',(28.2232385397136,504.151017554304,-37.0925388952725)) ;
#56900 = CARTESIAN_POINT('Ctrl Pts',(28.2229060366054,504.15157528428,-37.0842122200828)) ;
#56901 = CARTESIAN_POINT('Ctrl Pts',(28.2226375148372,504.15213556435,-37.0758858722792)) ;
#56902 = CARTESIAN_POINT('Ctrl Pts',(28.222636566139,504.152137543842,-37.075856454956)) ;
#56903 = CARTESIAN_POINT('Ctrl Pts',(28.2226356182393,504.152139523366,-37.0758270376369)) ;
#56904 = CARTESIAN_POINT('Ctrl Pts',(28.2226346711383,504.152141502922,-37.075797620322)) ;
#56905 = CARTESIAN_POINT('Ctrl Pts',(28.2208500943408,504.155871484354,-37.0203679936469)) ;
#56906 = CARTESIAN_POINT('Ctrl Pts',(28.2219028062132,504.159724323723,-36.9647537042311)) ;
#56907 = CARTESIAN_POINT('Ctrl Pts',(28.2257758975944,504.163636871801,-36.9092625220861)) ;
#56908 = CARTESIAN_POINT('Ctrl Pts',(28.2261369073593,504.164001559314,-36.9040902045117)) ;
#56909 = CARTESIAN_POINT('Ctrl Pts',(28.2265223981255,504.164366765579,-36.8989189862949)) ;
#56910 = CARTESIAN_POINT('Ctrl Pts',(28.2269323418467,504.164732439457,-36.8937491346411)) ;
#56911 = CARTESIAN_POINT('Ctrl Pts',(28.2317959566801,504.169070832282,-36.8324134783378)) ;
#56912 = CARTESIAN_POINT('Ctrl Pts',(28.2401047895027,504.173474379365,-36.7712651476695)) ;
#56913 = CARTESIAN_POINT('Ctrl Pts',(28.2517890378207,504.177871818711,-36.7107050943761)) ;
#56914 = CARTESIAN_POINT('Ctrl Pts',(28.2633079385338,504.182207028459,-36.6510020461283)) ;
#56915 = CARTESIAN_POINT('Ctrl Pts',(28.2781069899057,504.186536014908,-36.591870566549)) ;
#56916 = CARTESIAN_POINT('Ctrl Pts',(28.296083296526,504.190811046205,-36.5336796190072)) ;
#56917 = CARTESIAN_POINT('Ctrl Pts',(28.3140486279441,504.195083467438,-36.4755241991982)) ;
#56918 = CARTESIAN_POINT('Ctrl Pts',(28.3351872250997,504.199301864474,-36.4183080962711)) ;
#56919 = CARTESIAN_POINT('Ctrl Pts',(28.3593637853539,504.203442387736,-36.362386118099)) ;
#56920 = CARTESIAN_POINT('Ctrl Pts',(28.3835345651836,504.207581921032,-36.3064775104298)) ;
#56921 = CARTESIAN_POINT('Ctrl Pts',(28.410741876212,504.211643615454,-36.2518624389859)) ;
#56922 = CARTESIAN_POINT('Ctrl Pts',(28.440818544815,504.215628424807,-36.1988822544473)) ;
#56923 = CARTESIAN_POINT('Ctrl Pts',(28.4716879497097,504.219718262513,-36.1445056614308)) ;
#56924 = CARTESIAN_POINT('Ctrl Pts',(28.505580247537,504.223727124136,-36.0918514796608)) ;
#56925 = CARTESIAN_POINT('Ctrl Pts',(28.5422784938317,504.22768225627,-36.0412730036637)) ;
#56926 = CARTESIAN_POINT('Ctrl Pts',(28.5780801642525,504.23154076046,-35.9919302118176)) ;
#56927 = CARTESIAN_POINT('Ctrl Pts',(28.6165524211438,504.235348490898,-35.9445631243113)) ;
#56928 = CARTESIAN_POINT('Ctrl Pts',(28.6574576603838,504.239152230433,-35.8994822958023)) ;
#56929 = CARTESIAN_POINT('Ctrl Pts',(28.6998994752998,504.243098854689,-35.8527080386316)) ;
#56930 = CARTESIAN_POINT('Ctrl Pts',(28.744961073878,504.247041605063,-35.8083956799027)) ;
#56931 = CARTESIAN_POINT('Ctrl Pts',(28.7923321274247,504.251050616792,-35.7668666333778)) ;
#56932 = CARTESIAN_POINT('Ctrl Pts',(28.8334073936705,504.254526816113,-35.7308569499269)) ;
#56933 = CARTESIAN_POINT('Ctrl Pts',(28.8762196343179,504.25805348928,-35.6969391952642)) ;
#56934 = CARTESIAN_POINT('Ctrl Pts',(28.9205326144722,504.261681330358,-35.6653031412673)) ;
#56935 = CARTESIAN_POINT('Ctrl Pts',(28.9273005643906,504.262235412856,-35.6604713464225)) ;
#56936 = CARTESIAN_POINT('Ctrl Pts',(28.9341035484484,504.262791855262,-35.6556926806711)) ;
#56937 = CARTESIAN_POINT('Ctrl Pts',(28.9409407570499,504.263350838184,-35.6509677176084)) ;
#56938 = CARTESIAN_POINT('Ctrl Pts',(28.9409650997126,504.263352828343,-35.6509508952195)) ;
#56939 = CARTESIAN_POINT('Ctrl Pts',(28.9409894428091,504.263354818535,-35.6509340735113)) ;
#56940 = CARTESIAN_POINT('Ctrl Pts',(28.9410137863394,504.263356808758,-35.6509172524838)) ;
#56941 = CARTESIAN_POINT('Ctrl Pts',(28.9869423202729,504.267111730322,-35.6191812995285)) ;
#56942 = CARTESIAN_POINT('Ctrl Pts',(29.0345809314372,504.270990944817,-35.5897636294556)) ;
#56943 = CARTESIAN_POINT('Ctrl Pts',(29.0836601273048,504.274930258251,-35.562816359925)) ;
#56944 = CARTESIAN_POINT('Ctrl Pts',(29.0885670056895,504.275324106023,-35.5601222046511)) ;
#56945 = CARTESIAN_POINT('Ctrl Pts',(29.093488240868,504.275718554529,-35.5574527410732)) ;
#56946 = CARTESIAN_POINT('Ctrl Pts',(29.098423535015,504.276113539616,-35.5548081192529)) ;
#56947 = CARTESIAN_POINT('Ctrl Pts',(29.1526313881012,504.280451942346,-35.5257603529336)) ;
#56948 = CARTESIAN_POINT('Ctrl Pts',(29.2085413791482,504.284854446758,-35.499709252215)) ;
#56949 = CARTESIAN_POINT('Ctrl Pts',(29.2657851188358,504.289250406587,-35.4768109646585)) ;
#56950 = CARTESIAN_POINT('Ctrl Pts',(29.3229409176651,504.293639613111,-35.4539478546615)) ;
#56951 = CARTESIAN_POINT('Ctrl Pts',(29.3814263602263,504.298021958897,-35.4342275015703)) ;
#56952 = CARTESIAN_POINT('Ctrl Pts',(29.440868284465,504.302348604279,-35.4177679028226)) ;
#56953 = CARTESIAN_POINT('Ctrl Pts',(29.5002567651601,504.306671359625,-35.4013231027089)) ;
#56954 = CARTESIAN_POINT('Ctrl Pts',(29.5606000532667,504.310938374649,-35.3881330589776)) ;
#56955 = CARTESIAN_POINT('Ctrl Pts',(29.6215191659238,504.315125889259,-35.3782818457609)) ;
#56956 = CARTESIAN_POINT('Ctrl Pts',(29.6824067496338,504.319311236603,-35.3684357310817)) ;
#56957 = CARTESIAN_POINT('Ctrl Pts',(29.7438695966127,504.323417160521,-35.3619250360645)) ;
#56958 = CARTESIAN_POINT('Ctrl Pts',(29.8055218641932,504.327445925357,-35.3588007649088)) ;
#56959 = CARTESIAN_POINT('Ctrl Pts',(29.8334504027829,504.329270959839,-35.3573854669651)) ;
#56960 = CARTESIAN_POINT('Ctrl Pts',(29.8614177078716,504.331080514259,-35.3566646446211)) ;
#56961 = CARTESIAN_POINT('Ctrl Pts',(29.8893873868701,504.332876521313,-35.3566407257823)) ;
#56962 = CARTESIAN_POINT('Ctrl Pts',(29.8893696774914,504.333153023327,-35.3561603845536)) ;
#56963 = CARTESIAN_POINT('Ctrl Pts',(29.9621840579132,504.33776953377,-35.3561971873801)) ;
#56964 = CARTESIAN_POINT('Ctrl Pts',(30.0349214669345,504.342254646832,-35.3610074838177)) ;
#56965 = CARTESIAN_POINT('Ctrl Pts',(30.2112166298579,504.353130330676,-35.3843401317637)) ;
#56966 = CARTESIAN_POINT('Ctrl Pts',(30.3137700963673,504.359457033253,-35.4079275358013)) ;
#56967 = CARTESIAN_POINT('Ctrl Pts',(30.4303996283287,504.367300860559,-35.4466440056302)) ;
#56968 = CARTESIAN_POINT('Ctrl Pts',(30.4472953070465,504.368454090922,-35.4525567232203)) ;
#56969 = CARTESIAN_POINT('Ctrl Pts',(30.4640904795472,504.369620557053,-35.4587397545496)) ;
#56970 = CARTESIAN_POINT('Origin',(179.888527625402,504.710565160536,-37.0221601717597)) ;
#56971 = CARTESIAN_POINT('',(180.464132351894,505.578765842461,-35.4584785386352)) ;
#56972 = CARTESIAN_POINT('',(180.464073435736,505.710565160536,-35.4587334800957)) ;
#56973 = CARTESIAN_POINT('',(180.464073435736,504.710565160536,-35.4587334800957)) ;
#56974 = CARTESIAN_POINT('',(181.553672909139,505.710557590725,-36.9459937350495)) ;
#56975 = CARTESIAN_POINT('Origin',(179.888527625402,505.710565160536,-37.0221601717597)) ;
#56976 = CARTESIAN_POINT('Ctrl Pts',(181.553672925284,505.710557590587,-36.9459937343111)) ;
#56977 = CARTESIAN_POINT('Ctrl Pts',(181.551232283181,505.706956684071,-36.8933096088381)) ;
#56978 = CARTESIAN_POINT('Ctrl Pts',(181.546229220061,505.703258987467,-36.8406540870477)) ;
#56979 = CARTESIAN_POINT('Ctrl Pts',(181.538696531225,505.699518432147,-36.7882942048495)) ;
#56980 = CARTESIAN_POINT('Ctrl Pts',(181.53008552317,505.695242408978,-36.7284389025576)) ;
#56981 = CARTESIAN_POINT('Ctrl Pts',(181.518168521576,505.690910939552,-36.6689686983251)) ;
#56982 = CARTESIAN_POINT('Ctrl Pts',(181.503032801552,505.686590161194,-36.610260669948)) ;
#56983 = CARTESIAN_POINT('Ctrl Pts',(181.487912510483,505.682273787325,-36.5516124869901)) ;
#56984 = CARTESIAN_POINT('Ctrl Pts',(181.469580338947,505.677968380708,-36.4937247889096)) ;
#56985 = CARTESIAN_POINT('Ctrl Pts',(181.448158009494,505.673719114553,-36.4369573931851)) ;
#56986 = CARTESIAN_POINT('Ctrl Pts',(181.426749389391,505.669472567741,-36.380226326101)) ;
#56987 = CARTESIAN_POINT('Ctrl Pts',(181.402254655126,505.665282207666,-36.3246140776572)) ;
#56988 = CARTESIAN_POINT('Ctrl Pts',(181.374827311688,505.661169324461,-36.2704651280015)) ;
#56989 = CARTESIAN_POINT('Ctrl Pts',(181.347407114689,505.657057512904,-36.216330287334)) ;
#56990 = CARTESIAN_POINT('Ctrl Pts',(181.31705580914,505.653023128339,-36.1636580345744)) ;
#56991 = CARTESIAN_POINT('Ctrl Pts',(181.283958371087,505.649062866651,-36.1127779211213)) ;
#56992 = CARTESIAN_POINT('Ctrl Pts',(181.250833052662,505.645099268947,-36.0618549476582)) ;
#56993 = CARTESIAN_POINT('Ctrl Pts',(181.214956852527,505.641209795007,-36.0127272875708)) ;
#56994 = CARTESIAN_POINT('Ctrl Pts',(181.176547993421,505.63736749505,-35.9657091024632)) ;
#56995 = CARTESIAN_POINT('Ctrl Pts',(181.138124707358,505.633523751867,-35.9186732566059)) ;
#56996 = CARTESIAN_POINT('Ctrl Pts',(181.097166661149,505.629726944885,-35.8737487466492)) ;
#56997 = CARTESIAN_POINT('Ctrl Pts',(181.053927512491,505.625929389367,-35.8312306832966)) ;
#56998 = CARTESIAN_POINT('Ctrl Pts',(181.010606247503,505.622124621837,-35.7886318730427)) ;
#56999 = CARTESIAN_POINT('Ctrl Pts',(180.964994953339,505.618318628867,-35.7484491347412)) ;
#57000 = CARTESIAN_POINT('Ctrl Pts',(180.917387530296,505.614448217065,-35.7109542182485)) ;
#57001 = CARTESIAN_POINT('Ctrl Pts',(180.874609000482,505.610970387011,-35.6772624680851)) ;
#57002 = CARTESIAN_POINT('Ctrl Pts',(180.830218468774,505.607439954069,-35.6457406515821)) ;
#57003 = CARTESIAN_POINT('Ctrl Pts',(180.784460105248,505.603806575094,-35.6165636899711)) ;
#57004 = CARTESIAN_POINT('Ctrl Pts',(180.780374495576,505.603482162962,-35.6139585776513)) ;
#57005 = CARTESIAN_POINT('Ctrl Pts',(180.776277970414,505.603156930133,-35.6113721261506)) ;
#57006 = CARTESIAN_POINT('Ctrl Pts',(180.772170696643,505.602830840774,-35.6088044409151)) ;
#57007 = CARTESIAN_POINT('Ctrl Pts',(180.772142495247,505.602828601777,-35.6087868106542)) ;
#57008 = CARTESIAN_POINT('Ctrl Pts',(180.772114293344,505.602826362739,-35.6087691812779)) ;
#57009 = CARTESIAN_POINT('Ctrl Pts',(180.772086090935,505.602824123661,-35.6087515527864)) ;
#57010 = CARTESIAN_POINT('Ctrl Pts',(180.724314775962,505.599031408457,-35.5788911175874)) ;
#57011 = CARTESIAN_POINT('Ctrl Pts',(180.674922975228,505.595113445829,-35.5514743831438)) ;
#57012 = CARTESIAN_POINT('Ctrl Pts',(180.62419067516,505.591135506992,-35.5266397360626)) ;
#57013 = CARTESIAN_POINT('Ctrl Pts',(180.618793793035,505.590712335423,-35.5239978360755)) ;
#57014 = CARTESIAN_POINT('Ctrl Pts',(180.613381789521,505.590288485126,-35.521385153931)) ;
#57015 = CARTESIAN_POINT('Ctrl Pts',(180.607955036194,505.589864034679,-35.5188018533853)) ;
#57016 = CARTESIAN_POINT('Ctrl Pts',(180.561046359589,505.586195099023,-35.4964718887473)) ;
#57017 = CARTESIAN_POINT('Ctrl Pts',(180.51303134374,505.582481418132,-35.4763363661572)) ;
#57018 = CARTESIAN_POINT('Ctrl Pts',(180.464132351894,505.578765842461,-35.4584785386352)) ;
#57019 = CARTESIAN_POINT('Origin',(179.888527625402,504.710565160536,-37.0221601717597)) ;
#57020 = CARTESIAN_POINT('',(180.464073442659,504.877005588434,-35.4587334826444)) ;
#57021 = CARTESIAN_POINT('',(180.464062970719,505.071445141582,-35.4587536919275)) ;
#57022 = CARTESIAN_POINT('',(180.464073435736,504.710565160536,-35.4587334800957)) ;
#57023 = CARTESIAN_POINT('',(179.569297170772,505.710565160536,-35.3870308445086)) ;
#57024 = CARTESIAN_POINT('Ctrl Pts',(180.464062970719,505.071445141582,-35.4587536919275)) ;
#57025 = CARTESIAN_POINT('Ctrl Pts',(180.521080010244,505.075770871481,-35.4799041023179)) ;
#57026 = CARTESIAN_POINT('Ctrl Pts',(180.576992960962,505.080073944616,-35.5041868991519)) ;
#57027 = CARTESIAN_POINT('Ctrl Pts',(180.631455338622,505.084313431263,-35.5314424279691)) ;
#57028 = CARTESIAN_POINT('Ctrl Pts',(180.685890268488,505.088550781305,-35.5586842206219)) ;
#57029 = CARTESIAN_POINT('Ctrl Pts',(180.738876133664,505.092724517274,-35.588895689098)) ;
#57030 = CARTESIAN_POINT('Ctrl Pts',(180.790084341574,505.096818065672,-35.6218872465369)) ;
#57031 = CARTESIAN_POINT('Ctrl Pts',(180.841285782239,505.1009110731,-35.6548744440893)) ;
#57032 = CARTESIAN_POINT('Ctrl Pts',(180.890709970514,505.104923945953,-35.690641038872)) ;
#57033 = CARTESIAN_POINT('Ctrl Pts',(180.938045959887,505.108864839164,-35.7289674359767)) ;
#57034 = CARTESIAN_POINT('Ctrl Pts',(180.985427575524,505.112809530928,-35.7673307751703)) ;
#57035 = CARTESIAN_POINT('Ctrl Pts',(181.030716786754,505.116682254085,-35.8082589823685)) ;
#57036 = CARTESIAN_POINT('Ctrl Pts',(181.073621114329,505.120514619554,-35.8515003800246)) ;
#57037 = CARTESIAN_POINT('Ctrl Pts',(181.116545852412,505.124348808161,-35.8947623485404)) ;
#57038 = CARTESIAN_POINT('Ctrl Pts',(181.157083118322,505.128142910395,-35.9403399040468)) ;
#57039 = CARTESIAN_POINT('Ctrl Pts',(181.19496306555,505.131948623222,-35.9879471018041)) ;
#57040 = CARTESIAN_POINT('Ctrl Pts',(181.232914486131,505.135761516816,-36.035644126667)) ;
#57041 = CARTESIAN_POINT('Ctrl Pts',(181.268198006477,505.139586590695,-36.0853786797498)) ;
#57042 = CARTESIAN_POINT('Ctrl Pts',(181.300571785506,505.143489740683,-36.1368259459113)) ;
#57043 = CARTESIAN_POINT('Ctrl Pts',(181.326653284119,505.146634260849,-36.1782737422847)) ;
#57044 = CARTESIAN_POINT('Ctrl Pts',(181.350846570535,505.149829917129,-36.2208324674788)) ;
#57045 = CARTESIAN_POINT('Ctrl Pts',(181.373043576586,505.15311340371,-36.2643136111372)) ;
#57046 = CARTESIAN_POINT('Ctrl Pts',(181.373057187027,505.153115417031,-36.2643402722792)) ;
#57047 = CARTESIAN_POINT('Ctrl Pts',(181.373070796718,505.153117430385,-36.2643669337685)) ;
#57048 = CARTESIAN_POINT('Ctrl Pts',(181.37308440566,505.153119443772,-36.264393595605)) ;
#57049 = CARTESIAN_POINT('Ctrl Pts',(181.398271192042,505.156845725506,-36.3137380628099)) ;
#57050 = CARTESIAN_POINT('Ctrl Pts',(181.420974790708,505.160694970282,-36.3644557912384)) ;
#57051 = CARTESIAN_POINT('Ctrl Pts',(181.441079501555,505.164604050267,-36.4162617899537)) ;
#57052 = CARTESIAN_POINT('Ctrl Pts',(181.442958774348,505.164969448592,-36.4211043168937)) ;
#57053 = CARTESIAN_POINT('Ctrl Pts',(181.444815347382,505.165335369723,-36.425956315746)) ;
#57054 = CARTESIAN_POINT('Ctrl Pts',(181.446649131573,505.165701762102,-36.430817531191)) ;
#57055 = CARTESIAN_POINT('Ctrl Pts',(181.468368576099,505.170041334334,-36.4883940441226)) ;
#57056 = CARTESIAN_POINT('Ctrl Pts',(181.486890304425,505.174446344264,-36.5472694413303)) ;
#57057 = CARTESIAN_POINT('Ctrl Pts',(181.502106448514,505.178845251849,-36.6070507344203)) ;
#57058 = CARTESIAN_POINT('Ctrl Pts',(181.51709363293,505.183177968392,-36.6659324891493)) ;
#57059 = CARTESIAN_POINT('Ctrl Pts',(181.528874414093,505.187504479843,-36.7256930668193)) ;
#57060 = CARTESIAN_POINT('Ctrl Pts',(181.537384817382,505.191776934332,-36.7859553523217)) ;
#57061 = CARTESIAN_POINT('Ctrl Pts',(181.545890020311,505.196046778099,-36.8461808139944)) ;
#57062 = CARTESIAN_POINT('Ctrl Pts',(181.551128970221,505.200262495487,-36.9069073820963)) ;
#57063 = CARTESIAN_POINT('Ctrl Pts',(181.553073060345,505.20440007612,-36.96775695298)) ;
#57064 = CARTESIAN_POINT('Ctrl Pts',(181.555016687712,505.208536671873,-37.0285920396698)) ;
#57065 = CARTESIAN_POINT('Ctrl Pts',(181.553666993242,505.212595164903,-37.0895500501727)) ;
#57066 = CARTESIAN_POINT('Ctrl Pts',(181.549029945194,505.216576317454,-37.1502515153961)) ;
#57067 = CARTESIAN_POINT('Ctrl Pts',(181.544263187326,505.22066883279,-37.212650952271)) ;
#57068 = CARTESIAN_POINT('Ctrl Pts',(181.536022236578,505.224679627689,-37.2747792232977)) ;
#57069 = CARTESIAN_POINT('Ctrl Pts',(181.524353245269,505.228635873202,-37.3362230233926)) ;
#57070 = CARTESIAN_POINT('Ctrl Pts',(181.512987076644,505.232489449954,-37.3960722917928)) ;
#57071 = CARTESIAN_POINT('Ctrl Pts',(181.498368355485,505.236291638583,-37.455272016429)) ;
#57072 = CARTESIAN_POINT('Ctrl Pts',(181.480579885503,505.240089060205,-37.5134407275502)) ;
#57073 = CARTESIAN_POINT('Ctrl Pts',(181.462080522641,505.244038240803,-37.573934074945)) ;
#57074 = CARTESIAN_POINT('Ctrl Pts',(181.440152174811,505.247982681211,-37.633312011773)) ;
#57075 = CARTESIAN_POINT('Ctrl Pts',(181.4149397813,505.251992891751,-37.6911495202233)) ;
#57076 = CARTESIAN_POINT('Ctrl Pts',(181.393113818423,505.25546446641,-37.7412185194943)) ;
#57077 = CARTESIAN_POINT('Ctrl Pts',(181.368826529878,505.258985986666,-37.7901340331353)) ;
#57078 = CARTESIAN_POINT('Ctrl Pts',(181.342211123621,505.262608248821,-37.8376238003478)) ;
#57079 = CARTESIAN_POINT('Ctrl Pts',(181.338096637096,505.263168215807,-37.8449652628593)) ;
#57080 = CARTESIAN_POINT('Ctrl Pts',(181.333926529225,505.263730590343,-37.8522727526905)) ;
#57081 = CARTESIAN_POINT('Ctrl Pts',(181.32970130716,505.264295560091,-37.8595453745187)) ;
#57082 = CARTESIAN_POINT('Ctrl Pts',(181.329685846643,505.264297627373,-37.8595719857805)) ;
#57083 = CARTESIAN_POINT('Ctrl Pts',(181.329670385388,505.264299694689,-37.8595985965754)) ;
#57084 = CARTESIAN_POINT('Ctrl Pts',(181.329654923396,505.26430176204,-37.8596252069035)) ;
#57085 = CARTESIAN_POINT('Ctrl Pts',(181.301764050089,505.268030921166,-37.907625831437)) ;
#57086 = CARTESIAN_POINT('Ctrl Pts',(181.271365056046,505.271882972526,-37.9542753361818)) ;
#57087 = CARTESIAN_POINT('Ctrl Pts',(181.238635970714,505.275794811077,-37.9993214409816)) ;
#57088 = CARTESIAN_POINT('Ctrl Pts',(181.235578353838,505.276160262889,-38.0035297385506)) ;
#57089 = CARTESIAN_POINT('Ctrl Pts',(181.232500435814,505.276526236505,-38.0077240288423)) ;
#57090 = CARTESIAN_POINT('Ctrl Pts',(181.229402383651,505.276892680471,-38.0119040984859)) ;
#57091 = CARTESIAN_POINT('Ctrl Pts',(181.192776611733,505.281224851914,-38.0613216903563)) ;
#57092 = CARTESIAN_POINT('Ctrl Pts',(181.153331366697,505.285622100762,-38.1087542638443)) ;
#57093 = CARTESIAN_POINT('Ctrl Pts',(181.111338007007,505.290013476012,-38.1538996748488)) ;
#57094 = CARTESIAN_POINT('Ctrl Pts',(181.069877970916,505.294349079967,-38.1984717306076)) ;
#57095 = CARTESIAN_POINT('Ctrl Pts',(181.02593437793,505.298678666118,-38.2408147102694)) ;
#57096 = CARTESIAN_POINT('Ctrl Pts',(180.979790785691,505.302954501936,-38.2806698616093)) ;
#57097 = CARTESIAN_POINT('Ctrl Pts',(180.93367532461,505.307227731016,-38.3205007155007)) ;
#57098 = CARTESIAN_POINT('Ctrl Pts',(180.885362603077,505.311447140245,-38.3578468915722)) ;
#57099 = CARTESIAN_POINT('Ctrl Pts',(180.835156113497,505.315588901942,-38.3924788439465)) ;
#57100 = CARTESIAN_POINT('Ctrl Pts',(180.78496170375,505.319729667119,-38.427102463768)) ;
#57101 = CARTESIAN_POINT('Ctrl Pts',(180.732874433412,505.323792820316,-38.4590131305097)) ;
#57102 = CARTESIAN_POINT('Ctrl Pts',(180.679217671769,505.327779356826,-38.4880096023417)) ;
#57103 = CARTESIAN_POINT('Ctrl Pts',(180.624286752494,505.331860559427,-38.5176946374549)) ;
#57104 = CARTESIAN_POINT('Ctrl Pts',(180.567710791877,505.335861490449,-38.5443251205988)) ;
#57105 = CARTESIAN_POINT('Ctrl Pts',(180.509858914482,505.339809209461,-38.5677173832672)) ;
#57106 = CARTESIAN_POINT('Ctrl Pts',(180.453277628558,505.343670225356,-38.5905958854359)) ;
#57107 = CARTESIAN_POINT('Ctrl Pts',(180.395475884077,505.347480694652,-38.6103766403132)) ;
#57108 = CARTESIAN_POINT('Ctrl Pts',(180.336820461364,505.351287379752,-38.6269217550556)) ;
#57109 = CARTESIAN_POINT('Ctrl Pts',(180.276189286104,505.355222289445,-38.6440241763704)) ;
#57110 = CARTESIAN_POINT('Ctrl Pts',(180.21464581881,505.359153585616,-38.6576684834696)) ;
#57111 = CARTESIAN_POINT('Ctrl Pts',(180.152619545364,505.363150532887,-38.6677472000519)) ;
#57112 = CARTESIAN_POINT('Ctrl Pts',(180.098635944115,505.366629213707,-38.676519054088)) ;
#57113 = CARTESIAN_POINT('Ctrl Pts',(180.044285767577,505.370158273136,-38.6825903101323)) ;
#57114 = CARTESIAN_POINT('Ctrl Pts',(179.989870386624,505.373788303311,-38.6859247996509)) ;
#57115 = CARTESIAN_POINT('Ctrl Pts',(179.981796515883,505.374326908278,-38.6864195538341)) ;
#57116 = CARTESIAN_POINT('Ctrl Pts',(179.973721140369,505.374867736123,-38.6868541208458)) ;
#57117 = CARTESIAN_POINT('Ctrl Pts',(179.965645170118,505.375410952105,-38.6872284464903)) ;
#57118 = CARTESIAN_POINT('Ctrl Pts',(179.965612031944,505.375413181086,-38.6872299824628)) ;
#57119 = CARTESIAN_POINT('Ctrl Pts',(179.965578893759,505.375415410108,-38.6872315174211)) ;
#57120 = CARTESIAN_POINT('Ctrl Pts',(179.965545755565,505.375417639169,-38.6872330513651)) ;
#57121 = CARTESIAN_POINT('Ctrl Pts',(179.910067113818,505.379149445156,-38.6898011192401)) ;
#57122 = CARTESIAN_POINT('Ctrl Pts',(179.854363673121,505.383003622821,-38.689527257712)) ;
#57123 = CARTESIAN_POINT('Ctrl Pts',(179.798744861262,505.386916699123,-38.6864243279499)) ;
#57124 = CARTESIAN_POINT('Ctrl Pts',(179.793688291258,505.387272455451,-38.686142225887)) ;
#57125 = CARTESIAN_POINT('Ctrl Pts',(179.788632449574,505.387628698604,-38.6858367610734)) ;
#57126 = CARTESIAN_POINT('Ctrl Pts',(179.783577585658,505.387985380887,-38.6855079560975)) ;
#57127 = CARTESIAN_POINT('Ctrl Pts',(179.722174709537,505.392318102478,-38.6815138681186)) ;
#57128 = CARTESIAN_POINT('Ctrl Pts',(179.660911037464,505.396714958137,-38.6740726173969)) ;
#57129 = CARTESIAN_POINT('Ctrl Pts',(179.600188702896,505.401104926319,-38.663248522297)) ;
#57130 = CARTESIAN_POINT('Ctrl Pts',(179.540366824506,505.405429795324,-38.6525849385376)) ;
#57131 = CARTESIAN_POINT('Ctrl Pts',(179.481070175861,505.409747700509,-38.6386385048869)) ;
#57132 = CARTESIAN_POINT('Ctrl Pts',(179.42266863279,505.414011481721,-38.6215068676923)) ;
#57133 = CARTESIAN_POINT('Ctrl Pts',(179.364301006689,505.418272786722,-38.6043851797766)) ;
#57134 = CARTESIAN_POINT('Ctrl Pts',(179.306827383361,505.422479899325,-38.5840820957034)) ;
#57135 = CARTESIAN_POINT('Ctrl Pts',(179.250604020104,505.426609662978,-38.5607278453121)) ;
#57136 = CARTESIAN_POINT('Ctrl Pts',(179.194392324855,505.430738569583,-38.5373784416168)) ;
#57137 = CARTESIAN_POINT('Ctrl Pts',(179.139430402327,505.434790159582,-38.5109791146164)) ;
#57138 = CARTESIAN_POINT('Ctrl Pts',(179.086061553448,505.438766159265,-38.4816921757098)) ;
#57139 = CARTESIAN_POINT('Ctrl Pts',(179.031225404504,505.442851473366,-38.4516000343628)) ;
#57140 = CARTESIAN_POINT('Ctrl Pts',(178.978071339079,505.44685699701,-38.4184590177896)) ;
#57141 = CARTESIAN_POINT('Ctrl Pts',(178.926956443945,505.450810966356,-38.3824818069815)) ;
#57142 = CARTESIAN_POINT('Ctrl Pts',(178.87714107789,505.454664411224,-38.3474192695086)) ;
#57143 = CARTESIAN_POINT('Ctrl Pts',(178.829262694466,505.458469260829,-38.3096628501496)) ;
#57144 = CARTESIAN_POINT('Ctrl Pts',(178.783634834466,505.462273146348,-38.2694459596162)) ;
#57145 = CARTESIAN_POINT('Ctrl Pts',(178.736221539503,505.466225879307,-38.2276553673468)) ;
#57146 = CARTESIAN_POINT('Ctrl Pts',(178.691238997983,505.470178000043,-38.1832073670448)) ;
#57147 = CARTESIAN_POINT('Ctrl Pts',(178.64901397051,505.474200826604,-38.1364095751759)) ;
#57148 = CARTESIAN_POINT('Ctrl Pts',(178.612570228503,505.477672863499,-38.0960191537744)) ;
#57149 = CARTESIAN_POINT('Ctrl Pts',(178.578179820612,505.481198232857,-38.05387774283)) ;
#57150 = CARTESIAN_POINT('Ctrl Pts',(178.546033727488,505.484827547551,-38.0102172444428)) ;
#57151 = CARTESIAN_POINT('Ctrl Pts',(178.540955075824,505.485400930607,-38.003319471144)) ;
#57152 = CARTESIAN_POINT('Ctrl Pts',(178.535932339391,505.485976908114,-37.9963837548511)) ;
#57153 = CARTESIAN_POINT('Ctrl Pts',(178.530966156704,505.486555679654,-37.9894109764195)) ;
#57154 = CARTESIAN_POINT('Ctrl Pts',(178.530945746489,505.486558058313,-37.9893823194171)) ;
#57155 = CARTESIAN_POINT('Ctrl Pts',(178.530925337229,505.486560437018,-37.9893536617887)) ;
#57156 = CARTESIAN_POINT('Ctrl Pts',(178.530904928924,505.486562815771,-37.9893250035343)) ;
#57157 = CARTESIAN_POINT('Ctrl Pts',(178.49901047633,505.490280371737,-37.9445373870732)) ;
#57158 = CARTESIAN_POINT('Ctrl Pts',(178.469336257246,505.494123495406,-37.8980478367498)) ;
#57159 = CARTESIAN_POINT('Ctrl Pts',(178.442036825202,505.498029375113,-37.8501163050674)) ;
#57160 = CARTESIAN_POINT('Ctrl Pts',(178.4393746574,505.498410266084,-37.8454421499372)) ;
#57161 = CARTESIAN_POINT('Ctrl Pts',(178.43673506987,505.498791753843,-37.8407543228835)) ;
#57162 = CARTESIAN_POINT('Ctrl Pts',(178.434118203299,505.499173780139,-37.8360530912797)) ;
#57163 = CARTESIAN_POINT('Ctrl Pts',(178.404193150937,505.503542423556,-37.7822923824075)) ;
#57164 = CARTESIAN_POINT('Ctrl Pts',(178.377239393279,505.507980795142,-37.7267726190367)) ;
#57165 = CARTESIAN_POINT('Ctrl Pts',(178.353422670534,505.512415602303,-37.6698682440388)) ;
#57166 = CARTESIAN_POINT('Ctrl Pts',(178.330049388099,505.516767838394,-37.6140233638335)) ;
#57167 = CARTESIAN_POINT('Ctrl Pts',(178.309696939059,505.521116357443,-37.5568450454947)) ;
#57168 = CARTESIAN_POINT('Ctrl Pts',(178.292483291909,505.525412119828,-37.4986946008478)) ;
#57169 = CARTESIAN_POINT('Ctrl Pts',(178.275280535674,505.529705164323,-37.440580947449)) ;
#57170 = CARTESIAN_POINT('Ctrl Pts',(178.261212476853,505.533945376166,-37.3814964112241)) ;
#57171 = CARTESIAN_POINT('Ctrl Pts',(178.250362129364,505.53810737924,-37.3218084178744)) ;
#57172 = CARTESIAN_POINT('Ctrl Pts',(178.239514522384,505.542268331102,-37.2621355001256)) ;
#57173 = CARTESIAN_POINT('Ctrl Pts',(178.231883028496,505.546351103104,-37.2018594527911)) ;
#57174 = CARTESIAN_POINT('Ctrl Pts',(178.227516627559,505.550355018515,-37.1413539778099)) ;
#57175 = CARTESIAN_POINT('Ctrl Pts',(178.222999602097,505.554497054055,-37.0787612899084)) ;
#57176 = CARTESIAN_POINT('Ctrl Pts',(178.221977221747,505.558554667682,-37.0159230896694)) ;
#57177 = CARTESIAN_POINT('Ctrl Pts',(178.224463849545,505.562554099107,-36.9532598849088)) ;
#57178 = CARTESIAN_POINT('Ctrl Pts',(178.226870699266,505.566425217422,-36.8926070936028)) ;
#57179 = CARTESIAN_POINT('Ctrl Pts',(178.232565100846,505.570242206833,-36.8321183759182)) ;
#57180 = CARTESIAN_POINT('Ctrl Pts',(178.241520426093,505.574050662793,-36.7721801361307)) ;
#57181 = CARTESIAN_POINT('Ctrl Pts',(178.250921004708,505.578048472886,-36.7092618032315)) ;
#57182 = CARTESIAN_POINT('Ctrl Pts',(178.263915778421,505.582037255386,-36.6469502675765)) ;
#57183 = CARTESIAN_POINT('Ctrl Pts',(178.280420961934,505.586088946602,-36.5856957895303)) ;
#57184 = CARTESIAN_POINT('Ctrl Pts',(178.294648206635,505.589581449568,-36.5328952588654)) ;
#57185 = CARTESIAN_POINT('Ctrl Pts',(178.311483868444,505.593121357734,-36.4808791417708)) ;
#57186 = CARTESIAN_POINT('Ctrl Pts',(178.330834538074,505.596760456215,-36.4299380618792)) ;
#57187 = CARTESIAN_POINT('Ctrl Pts',(178.333926185787,505.597341873329,-36.4217992286427)) ;
#57188 = CARTESIAN_POINT('Ctrl Pts',(178.337082000965,505.597925822406,-36.413687733639)) ;
#57189 = CARTESIAN_POINT('Ctrl Pts',(178.340301570173,505.598512514642,-36.4056046427992)) ;
#57190 = CARTESIAN_POINT('Ctrl Pts',(178.340308451531,505.598513768611,-36.4055873663754)) ;
#57191 = CARTESIAN_POINT('Ctrl Pts',(178.340315333181,505.598515022592,-36.4055700900813)) ;
#57192 = CARTESIAN_POINT('Ctrl Pts',(178.340322215121,505.598516276586,-36.405552813917)) ;
#57193 = CARTESIAN_POINT('Ctrl Pts',(178.361122777435,505.602306454293,-36.3533358655596)) ;
#57194 = CARTESIAN_POINT('Ctrl Pts',(178.384664367637,505.606221021278,-36.3021240858524)) ;
#57195 = CARTESIAN_POINT('Ctrl Pts',(178.41080410433,505.610197626341,-36.2521967746116)) ;
#57196 = CARTESIAN_POINT('Ctrl Pts',(178.413432545432,505.61059748776,-36.2471764104621)) ;
#57197 = CARTESIAN_POINT('Ctrl Pts',(178.416087218387,505.610997976445,-36.2421690546694)) ;
#57198 = CARTESIAN_POINT('Ctrl Pts',(178.418767952148,505.611399029005,-36.2371750046425)) ;
#57199 = CARTESIAN_POINT('Ctrl Pts',(178.448046319473,505.615779234284,-36.1826311207183)) ;
#57200 = CARTESIAN_POINT('Ctrl Pts',(178.480438320548,505.620226065791,-36.1296710461462)) ;
#57201 = CARTESIAN_POINT('Ctrl Pts',(178.515719393852,505.62467032553,-36.0786327386408)) ;
#57202 = CARTESIAN_POINT('Ctrl Pts',(178.550956777783,505.62910908184,-36.0276576330572)) ;
#57203 = CARTESIAN_POINT('Ctrl Pts',(178.589075856204,505.633544932528,-35.9785992330982)) ;
#57204 = CARTESIAN_POINT('Ctrl Pts',(178.629826423725,505.637929521447,-35.9317659650367)) ;
#57205 = CARTESIAN_POINT('Ctrl Pts',(178.670539342107,505.642310059478,-35.8849759658764)) ;
#57206 = CARTESIAN_POINT('Ctrl Pts',(178.713878846991,505.64663929412,-35.8404068485302)) ;
#57207 = CARTESIAN_POINT('Ctrl Pts',(178.759570878723,505.650893055017,-35.7983412968363)) ;
#57208 = CARTESIAN_POINT('Ctrl Pts',(178.805235050172,505.655144222224,-35.7563013942139)) ;
#57209 = CARTESIAN_POINT('Ctrl Pts',(178.853248932888,505.659320014824,-35.7167620262066)) ;
#57210 = CARTESIAN_POINT('Ctrl Pts',(178.903314306228,505.663421273273,-35.6799813653945)) ;
#57211 = CARTESIAN_POINT('Ctrl Pts',(178.953384283495,505.667522908868,-35.6431973222944)) ;
#57212 = CARTESIAN_POINT('Ctrl Pts',(179.005506239459,505.671550130967,-35.6091726680432)) ;
#57213 = CARTESIAN_POINT('Ctrl Pts',(179.059355946802,505.675527710287,-35.5781401733316)) ;
#57214 = CARTESIAN_POINT('Ctrl Pts',(179.113203662447,505.679505142491,-35.5471088263952)) ;
#57215 = CARTESIAN_POINT('Ctrl Pts',(179.168779140413,505.683433228105,-35.5190697626465)) ;
#57216 = CARTESIAN_POINT('Ctrl Pts',(179.225730361398,505.687357503393,-35.4942264014249)) ;
#57217 = CARTESIAN_POINT('Ctrl Pts',(179.282738343372,505.691285689847,-35.4693582798255)) ;
#57218 = CARTESIAN_POINT('Ctrl Pts',(179.341124914445,505.69521056244,-35.4476928080947)) ;
#57219 = CARTESIAN_POINT('Ctrl Pts',(179.400507193109,505.699192690673,-35.4293977783462)) ;
#57220 = CARTESIAN_POINT('Ctrl Pts',(179.45601305068,505.7029148692,-35.4122970314849)) ;
#57221 = CARTESIAN_POINT('Ctrl Pts',(179.512388503592,505.706687725966,-35.398141268249)) ;
#57222 = CARTESIAN_POINT('Ctrl Pts',(179.569297170772,505.710565160536,-35.3870308445087)) ;
#57223 = CARTESIAN_POINT('Origin',(179.888527625402,505.710565160536,-37.0221601717597)) ;
#57224 = CARTESIAN_POINT('Ctrl Pts',(180.464073449582,504.877005588434,-35.458733485193)) ;
#57225 = CARTESIAN_POINT('Ctrl Pts',(180.486923937135,504.878624850681,-35.4671454579477)) ;
#57226 = CARTESIAN_POINT('Ctrl Pts',(180.509589115676,504.880260874332,-35.4760580625355)) ;
#57227 = CARTESIAN_POINT('Ctrl Pts',(180.596969805277,504.886691145551,-35.5126506627681)) ;
#57228 = CARTESIAN_POINT('Ctrl Pts',(180.660089881212,504.891606583489,-35.5439184757573)) ;
#57229 = CARTESIAN_POINT('Ctrl Pts',(180.811340399425,504.904066896042,-35.6311744752597)) ;
#57230 = CARTESIAN_POINT('Ctrl Pts',(180.896550775369,504.911721908279,-35.6916297508855)) ;
#57231 = CARTESIAN_POINT('Ctrl Pts',(181.018554427028,504.923365842585,-35.7966739263697)) ;
#57232 = CARTESIAN_POINT('Ctrl Pts',(181.059648271787,504.927424644711,-35.835882436113)) ;
#57233 = CARTESIAN_POINT('Ctrl Pts',(181.119436118134,504.93345114912,-35.8990690361585)) ;
#57234 = CARTESIAN_POINT('Ctrl Pts',(181.139609137954,504.935506399607,-35.9215853046345)) ;
#57235 = CARTESIAN_POINT('Ctrl Pts',(181.186316283446,504.940304605392,-35.9766635224297)) ;
#57236 = CARTESIAN_POINT('Ctrl Pts',(181.212252938322,504.943009445288,-36.009702430912)) ;
#57237 = CARTESIAN_POINT('Ctrl Pts',(181.272044681172,504.949444149712,-36.0920988537308)) ;
#57238 = CARTESIAN_POINT('Ctrl Pts',(181.304543412835,504.953117869027,-36.1423682932357)) ;
#57239 = CARTESIAN_POINT('Ctrl Pts',(181.396485733974,504.964430254262,-36.302928793793)) ;
#57240 = CARTESIAN_POINT('Ctrl Pts',(181.446249868579,504.972008724939,-36.4182320730915)) ;
#57241 = CARTESIAN_POINT('Ctrl Pts',(181.497560460995,504.983350705534,-36.587178359447)) ;
#57242 = CARTESIAN_POINT('Ctrl Pts',(181.510207705152,504.986717248839,-36.6369996831346)) ;
#57243 = CARTESIAN_POINT('Ctrl Pts',(181.532230036138,504.994063837716,-36.7443365911058)) ;
#57244 = CARTESIAN_POINT('Ctrl Pts',(181.540930631925,504.998061275522,-36.8019184880018)) ;
#57245 = CARTESIAN_POINT('Ctrl Pts',(181.553359292123,505.007013245318,-36.9288686931117)) ;
#57246 = CARTESIAN_POINT('Ctrl Pts',(181.555799197202,505.011996690765,-36.9982535435589)) ;
#57247 = CARTESIAN_POINT('Ctrl Pts',(181.55070834816,505.025548792702,-37.1849080138226)) ;
#57248 = CARTESIAN_POINT('Ctrl Pts',(181.53511901935,505.034191249214,-37.3015742218307)) ;
#57249 = CARTESIAN_POINT('Ctrl Pts',(181.500275399704,505.044425139138,-37.4449292715406)) ;
#57250 = CARTESIAN_POINT('Ctrl Pts',(181.492361784658,505.046478681483,-37.4740242787658)) ;
#57251 = CARTESIAN_POINT('Ctrl Pts',(181.471965229593,505.051183285923,-37.5417024901008)) ;
#57252 = CARTESIAN_POINT('Ctrl Pts',(181.458855805208,505.053801190539,-37.5800749980219)) ;
#57253 = CARTESIAN_POINT('Ctrl Pts',(181.424230357451,505.059936245267,-37.6704973274354)) ;
#57254 = CARTESIAN_POINT('Ctrl Pts',(181.401450364654,505.063404285732,-37.7220098758374)) ;
#57255 = CARTESIAN_POINT('Ctrl Pts',(181.315532245264,505.075086103401,-37.8923972549)) ;
#57256 = CARTESIAN_POINT('Ctrl Pts',(181.240640650181,505.083196344975,-38.0047289218465)) ;
#57257 = CARTESIAN_POINT('Ctrl Pts',(181.12022837144,505.095103941257,-38.1451082654634)) ;
#57258 = CARTESIAN_POINT('Ctrl Pts',(181.085677863873,505.098415370472,-38.1818711441832)) ;
#57259 = CARTESIAN_POINT('Ctrl Pts',(181.006937293535,505.105788735553,-38.2583804156556)) ;
#57260 = CARTESIAN_POINT('Ctrl Pts',(180.962182408179,505.109874869627,-38.2974423129976)) ;
#57261 = CARTESIAN_POINT('Ctrl Pts',(180.858604203979,505.119125960952,-38.3785221255862)) ;
#57262 = CARTESIAN_POINT('Ctrl Pts',(180.79893903227,505.12432511874,-38.4192698682888)) ;
#57263 = CARTESIAN_POINT('Ctrl Pts',(180.643044619778,505.137487624959,-38.5115000736188)) ;
#57264 = CARTESIAN_POINT('Ctrl Pts',(180.544040107551,505.145488389746,-38.5576523344385)) ;
#57265 = CARTESIAN_POINT('Ctrl Pts',(180.411996283235,505.155223222595,-38.6040884135458)) ;
#57266 = CARTESIAN_POINT('Ctrl Pts',(180.382475976189,505.157340538829,-38.6135532887174)) ;
#57267 = CARTESIAN_POINT('Ctrl Pts',(180.315245594623,505.162009624704,-38.6330571026779)) ;
#57268 = CARTESIAN_POINT('Ctrl Pts',(180.277414166837,505.164536198418,-38.642606105986)) ;
#57269 = CARTESIAN_POINT('Ctrl Pts',(180.18773445598,505.170366053779,-38.6619196979945)) ;
#57270 = CARTESIAN_POINT('Ctrl Pts',(180.135688521192,505.17362706911,-38.6705679818234)) ;
#57271 = CARTESIAN_POINT('Ctrl Pts',(179.948206921303,505.185206679317,-38.692639760043)) ;
#57272 = CARTESIAN_POINT('Ctrl Pts',(179.811670724101,505.193377618667,-38.6919367670938)) ;
#57273 = CARTESIAN_POINT('Ctrl Pts',(179.625414179962,505.205419327044,-38.6680657311009)) ;
#57274 = CARTESIAN_POINT('Ctrl Pts',(179.574426294266,505.208804115516,-38.6591003585801)) ;
#57275 = CARTESIAN_POINT('Ctrl Pts',(179.468049427096,505.216102419562,-38.6352426992973)) ;
#57276 = CARTESIAN_POINT('Ctrl Pts',(179.412846936446,505.220029163233,-38.619834619492)) ;
#57277 = CARTESIAN_POINT('Ctrl Pts',(179.294835284153,505.228748196148,-38.580236683263)) ;
#57278 = CARTESIAN_POINT('Ctrl Pts',(179.232476310779,505.23356548482,-38.5550228622864)) ;
#57279 = CARTESIAN_POINT('Ctrl Pts',(179.065399116446,505.246979858641,-38.4754019923391)) ;
#57280 = CARTESIAN_POINT('Ctrl Pts',(178.964661038147,505.25566904535,-38.4135356981219)) ;
#57281 = CARTESIAN_POINT('Ctrl Pts',(178.846316034503,505.266082739799,-38.3222931380907)) ;
#57282 = CARTESIAN_POINT('Ctrl Pts',(178.821886702845,505.268242531688,-38.3023275462298)) ;
#57283 = CARTESIAN_POINT('Ctrl Pts',(178.769472712104,505.272875614223,-38.2569473764955)) ;
#57284 = CARTESIAN_POINT('Ctrl Pts',(178.74175697741,505.275329412413,-38.2312511513939)) ;
#57285 = CARTESIAN_POINT('Ctrl Pts',(178.679437613317,505.280923981761,-38.1693998246943)) ;
#57286 = CARTESIAN_POINT('Ctrl Pts',(178.645540687169,505.284027484449,-38.1325842648028)) ;
#57287 = CARTESIAN_POINT('Ctrl Pts',(178.518133287261,505.296197058153,-37.9810484340822)) ;
#57288 = CARTESIAN_POINT('Ctrl Pts',(178.438435651292,505.305051170906,-37.8556334975304)) ;
#57289 = CARTESIAN_POINT('Ctrl Pts',(178.355075997403,505.317860434018,-37.6753450716706)) ;
#57290 = CARTESIAN_POINT('Ctrl Pts',(178.335919122793,505.321194422621,-37.6284029544816)) ;
#57291 = CARTESIAN_POINT('Ctrl Pts',(178.298555005547,505.328694032454,-37.5233966030894)) ;
#57292 = CARTESIAN_POINT('Ctrl Pts',(178.281329447934,505.332887893431,-37.4650633895282)) ;
#57293 = CARTESIAN_POINT('Ctrl Pts',(178.227850044723,505.349256782826,-37.2391424609511)) ;
#57294 = CARTESIAN_POINT('Ctrl Pts',(178.214347049073,505.362094189734,-37.0672986674056)) ;
#57295 = CARTESIAN_POINT('Ctrl Pts',(178.229778637586,505.376419274407,-36.8633981141818)) ;
#57296 = CARTESIAN_POINT('Ctrl Pts',(178.233263998269,505.378701134479,-36.830440431642)) ;
#57297 = CARTESIAN_POINT('Ctrl Pts',(178.242426744404,505.383266641816,-36.7630814145887)) ;
#57298 = CARTESIAN_POINT('Ctrl Pts',(178.248205197249,505.385544378412,-36.7287104772704)) ;
#57299 = CARTESIAN_POINT('Ctrl Pts',(178.275608284385,505.394482074718,-36.5920812460578)) ;
#57300 = CARTESIAN_POINT('Ctrl Pts',(178.3057558051,505.400790987909,-36.4917688232903)) ;
#57301 = CARTESIAN_POINT('Ctrl Pts',(178.381850620507,505.413139471535,-36.3045218641273)) ;
#57302 = CARTESIAN_POINT('Ctrl Pts',(178.426461340629,505.419147620642,-36.217524065389)) ;
#57303 = CARTESIAN_POINT('Ctrl Pts',(178.505172048478,505.428661250585,-36.0924258962436)) ;
#57304 = CARTESIAN_POINT('Ctrl Pts',(178.533824685386,505.431958307056,-36.0511516694038)) ;
#57305 = CARTESIAN_POINT('Ctrl Pts',(178.599904055385,505.43927009448,-35.9645926527049)) ;
#57306 = CARTESIAN_POINT('Ctrl Pts',(178.637948235698,505.443307499942,-35.9198673577203)) ;
#57307 = CARTESIAN_POINT('Ctrl Pts',(178.726853588352,505.452403122182,-35.8258877671727)) ;
#57308 = CARTESIAN_POINT('Ctrl Pts',(178.778654107249,505.457493181885,-35.7776790852677)) ;
#57309 = CARTESIAN_POINT('Ctrl Pts',(178.921445261153,505.470907251014,-35.6608131771621)) ;
#57310 = CARTESIAN_POINT('Ctrl Pts',(179.016698742053,505.479288438908,-35.5979298242953)) ;
#57311 = CARTESIAN_POINT('Ctrl Pts',(179.144581653435,505.489315980419,-35.5311789726886)) ;
#57312 = CARTESIAN_POINT('Ctrl Pts',(179.17192020229,505.491391850237,-35.517848055946)) ;
#57313 = CARTESIAN_POINT('Ctrl Pts',(179.236059184774,505.496089950105,-35.4887185677652)) ;
#57314 = CARTESIAN_POINT('Ctrl Pts',(179.27309282732,505.498681941617,-35.4734836777184)) ;
#57315 = CARTESIAN_POINT('Ctrl Pts',(179.362167115387,505.504716207531,-35.4405412402789)) ;
#57316 = CARTESIAN_POINT('Ctrl Pts',(179.414605851469,505.508112620284,-35.4240447770765)) ;
#57317 = CARTESIAN_POINT('Ctrl Pts',(179.600606287242,505.51991486733,-35.3754951136464)) ;
#57318 = CARTESIAN_POINT('Ctrl Pts',(179.737206831435,505.528200660572,-35.3573770654938)) ;
#57319 = CARTESIAN_POINT('Ctrl Pts',(179.925493396058,505.540354144688,-35.3557891850531)) ;
#57320 = CARTESIAN_POINT('Ctrl Pts',(179.976496111569,505.543712973918,-35.357702502675)) ;
#57321 = CARTESIAN_POINT('Ctrl Pts',(180.088440052483,505.55127769403,-35.3670613851399)) ;
#57322 = CARTESIAN_POINT('Ctrl Pts',(180.149217077004,505.555512452928,-35.3755405144951)) ;
#57323 = CARTESIAN_POINT('Ctrl Pts',(180.296031826649,505.566070634002,-35.4043549666717)) ;
#57324 = CARTESIAN_POINT('Ctrl Pts',(180.38118326896,505.572482028514,-35.4282214813861)) ;
#57325 = CARTESIAN_POINT('Ctrl Pts',(180.464032893301,505.578914864621,-35.458718555766)) ;
#57326 = CARTESIAN_POINT('Origin',(179.888527625402,504.710565160536,-37.0221601717597)) ;
#57327 = CARTESIAN_POINT('',(180.464073435742,504.178966917533,-35.4587334800982)) ;
#57328 = CARTESIAN_POINT('',(180.464073435525,504.369601015799,-35.4587334800181)) ;
#57329 = CARTESIAN_POINT('',(180.464073435736,504.710565160536,-35.4587334800957)) ;
#57330 = CARTESIAN_POINT('',(179.889599033433,504.139907930539,-35.3556857802299)) ;
#57331 = CARTESIAN_POINT('Ctrl Pts',(179.889579047996,504.140180283237,-35.3561605035393)) ;
#57332 = CARTESIAN_POINT('Ctrl Pts',(179.935879931379,504.143526942088,-35.3561897243104)) ;
#57333 = CARTESIAN_POINT('Ctrl Pts',(179.982163158329,504.146845416725,-35.3581491101495)) ;
#57334 = CARTESIAN_POINT('Ctrl Pts',(180.059263424997,504.152272397822,-35.3646408418133)) ;
#57335 = CARTESIAN_POINT('Ctrl Pts',(180.090142868883,504.154418486497,-35.3681128098242)) ;
#57336 = CARTESIAN_POINT('Ctrl Pts',(180.152752703499,504.158690116225,-35.376932162373)) ;
#57337 = CARTESIAN_POINT('Ctrl Pts',(180.184459988916,504.160808303287,-35.3823387500492)) ;
#57338 = CARTESIAN_POINT('Ctrl Pts',(180.300362090089,504.168446632402,-35.4055734397612)) ;
#57339 = CARTESIAN_POINT('Ctrl Pts',(180.383304656688,504.173715175109,-35.4289999897851)) ;
#57340 = CARTESIAN_POINT('Ctrl Pts',(180.464073435749,504.178966917533,-35.4587334801008)) ;
#57341 = CARTESIAN_POINT('',(180.967886278451,503.710565160535,-38.2912310516111)) ;
#57342 = CARTESIAN_POINT('Ctrl Pts',(179.889599033433,504.139907930539,-35.3556857802299)) ;
#57343 = CARTESIAN_POINT('Ctrl Pts',(179.829734963427,504.135659048629,-35.3557807655152)) ;
#57344 = CARTESIAN_POINT('Ctrl Pts',(179.769770760995,504.131370982823,-35.3591282310602)) ;
#57345 = CARTESIAN_POINT('Ctrl Pts',(179.710083728143,504.127103688023,-35.3657033091904)) ;
#57346 = CARTESIAN_POINT('Ctrl Pts',(179.650461321867,504.122841013668,-35.3722712681061)) ;
#57347 = CARTESIAN_POINT('Ctrl Pts',(179.591115449233,504.118599323853,-35.3820596163943)) ;
#57348 = CARTESIAN_POINT('Ctrl Pts',(179.532413623388,504.114418083644,-35.3950066269203)) ;
#57349 = CARTESIAN_POINT('Ctrl Pts',(179.473752342522,504.110239731391,-35.407944695028)) ;
#57350 = CARTESIAN_POINT('Ctrl Pts',(179.415734238346,504.106121843499,-35.4240369935909)) ;
#57351 = CARTESIAN_POINT('Ctrl Pts',(179.358717669987,504.102080905547,-35.4431872457158)) ;
#57352 = CARTESIAN_POINT('Ctrl Pts',(179.301717936172,504.09804116071,-35.4623318435938)) ;
#57353 = CARTESIAN_POINT('Ctrl Pts',(179.245719239883,504.09407829802,-35.4845326321906)) ;
#57354 = CARTESIAN_POINT('Ctrl Pts',(179.191070391662,504.090185345868,-35.5096589162831)) ;
#57355 = CARTESIAN_POINT('Ctrl Pts',(179.13637745663,504.086289253159,-35.5348054704776)) ;
#57356 = CARTESIAN_POINT('Ctrl Pts',(179.083036722165,504.082463045992,-35.5628823816942)) ;
#57357 = CARTESIAN_POINT('Ctrl Pts',(179.031386604159,504.078677432237,-35.5937226921901)) ;
#57358 = CARTESIAN_POINT('Ctrl Pts',(178.979717222524,504.074890406585,-35.6245745050081)) ;
#57359 = CARTESIAN_POINT('Ctrl Pts',(178.929740000811,504.071143714672,-35.6581920020274)) ;
#57360 = CARTESIAN_POINT('Ctrl Pts',(178.88177912004,504.067388889991,-35.6943693550852)) ;
#57361 = CARTESIAN_POINT('Ctrl Pts',(178.833729330466,504.063627104699,-35.7306137729074)) ;
#57362 = CARTESIAN_POINT('Ctrl Pts',(178.787703836856,504.059856666008,-35.7694278355667)) ;
#57363 = CARTESIAN_POINT('Ctrl Pts',(178.744008382537,504.056015428548,-35.810561822063)) ;
#57364 = CARTESIAN_POINT('Ctrl Pts',(178.705760217749,504.05265305858,-35.8465678441633)) ;
#57365 = CARTESIAN_POINT('Ctrl Pts',(178.669297385938,504.049235914134,-35.8843508652821)) ;
#57366 = CARTESIAN_POINT('Ctrl Pts',(178.634806823727,504.045719394504,-35.9237141442276)) ;
#57367 = CARTESIAN_POINT('Ctrl Pts',(178.634784961163,504.045717165485,-35.9237390954658)) ;
#57368 = CARTESIAN_POINT('Ctrl Pts',(178.634763099389,504.045714936425,-35.9237640473391)) ;
#57369 = CARTESIAN_POINT('Ctrl Pts',(178.634741238406,504.045712707326,-35.9237889998475)) ;
#57370 = CARTESIAN_POINT('Ctrl Pts',(178.598143074702,504.041980901396,-35.9655627841434)) ;
#57371 = CARTESIAN_POINT('Ctrl Pts',(178.563626661024,504.038126723739,-36.0092842373027)) ;
#57372 = CARTESIAN_POINT('Ctrl Pts',(178.531374867164,504.034213647399,-36.0547034201323)) ;
#57373 = CARTESIAN_POINT('Ctrl Pts',(178.528442702617,504.033857890948,-36.0588326948703)) ;
#57374 = CARTESIAN_POINT('Ctrl Pts',(178.525529257917,504.03350164767,-36.0629759666304)) ;
#57375 = CARTESIAN_POINT('Ctrl Pts',(178.522634670932,504.033144965263,-36.0671330263022)) ;
#57376 = CARTESIAN_POINT('Ctrl Pts',(178.487473308412,504.028812243707,-36.1176299997569)) ;
#57377 = CARTESIAN_POINT('Ctrl Pts',(178.455093838431,504.024415388031,-36.1701674097863)) ;
#57378 = CARTESIAN_POINT('Ctrl Pts',(178.425696700947,504.020025419779,-36.2243907539794)) ;
#57379 = CARTESIAN_POINT('Ctrl Pts',(178.396735494467,504.015700550493,-36.277810018629)) ;
#57380 = CARTESIAN_POINT('Ctrl Pts',(178.370668398909,504.011382644977,-36.3328654656163)) ;
#57381 = CARTESIAN_POINT('Ctrl Pts',(178.347649685094,504.00711886339,-36.3892070328538)) ;
#57382 = CARTESIAN_POINT('Ctrl Pts',(178.324644339505,504.002857558013,-36.4455158794604)) ;
#57383 = CARTESIAN_POINT('Ctrl Pts',(178.304683711337,503.99865044499,-36.5031093346559)) ;
#57384 = CARTESIAN_POINT('Ctrl Pts',(178.287888105595,503.994520680875,-36.5616276682746)) ;
#57385 = CARTESIAN_POINT('Ctrl Pts',(178.271095985438,503.990391773808,-36.62013385761)) ;
#57386 = CARTESIAN_POINT('Ctrl Pts',(178.257467612023,503.986340183306,-36.6795645313902)) ;
#57387 = CARTESIAN_POINT('Ctrl Pts',(178.247090129816,503.982364183077,-36.7395500866227)) ;
#57388 = CARTESIAN_POINT('Ctrl Pts',(178.236427334499,503.97827886876,-36.8011848535858)) ;
#57389 = CARTESIAN_POINT('Ctrl Pts',(178.229197007305,503.974273344842,-36.8634054572202)) ;
#57390 = CARTESIAN_POINT('Ctrl Pts',(178.225455507491,503.970319375166,-36.9258001115029)) ;
#57391 = CARTESIAN_POINT('Ctrl Pts',(178.221809130089,503.966465929654,-36.98660846875)) ;
#57392 = CARTESIAN_POINT('Ctrl Pts',(178.221476603408,503.96266107936,-37.0475820399051)) ;
#57393 = CARTESIAN_POINT('Ctrl Pts',(178.224470929098,503.958857193105,-37.1083301596863)) ;
#57394 = CARTESIAN_POINT('Ctrl Pts',(178.227582423468,503.954904459871,-37.1714553679145)) ;
#57395 = CARTESIAN_POINT('Ctrl Pts',(178.234287112341,503.950952338808,-37.2343370034491)) ;
#57396 = CARTESIAN_POINT('Ctrl Pts',(178.244548223404,503.946929511884,-37.2965277989752)) ;
#57397 = CARTESIAN_POINT('Ctrl Pts',(178.253404424326,503.943457474277,-37.3502036804004)) ;
#57398 = CARTESIAN_POINT('Ctrl Pts',(178.264909836953,503.939932104169,-37.403365924728)) ;
#57399 = CARTESIAN_POINT('Ctrl Pts',(178.279002227418,503.936302788681,-37.4557206286662)) ;
#57400 = CARTESIAN_POINT('Ctrl Pts',(178.281228634172,503.935729406008,-37.4639919625257)) ;
#57401 = CARTESIAN_POINT('Ctrl Pts',(178.283519568417,503.935153428887,-37.4722432372026)) ;
#57402 = CARTESIAN_POINT('Ctrl Pts',(178.285874739581,503.934574657738,-37.4804734042846)) ;
#57403 = CARTESIAN_POINT('Ctrl Pts',(178.285884419069,503.934572279054,-37.4805072293439)) ;
#57404 = CARTESIAN_POINT('Ctrl Pts',(178.285894099642,503.934569900322,-37.4805410540468)) ;
#57405 = CARTESIAN_POINT('Ctrl Pts',(178.2859037813,503.934567521544,-37.4805748783931)) ;
#57406 = CARTESIAN_POINT('Ctrl Pts',(178.301034282463,503.930849964868,-37.5334355875821)) ;
#57407 = CARTESIAN_POINT('Ctrl Pts',(178.318879702032,503.927006840452,-37.5856215868244)) ;
#57408 = CARTESIAN_POINT('Ctrl Pts',(178.339333163539,503.923100959956,-37.6368499635939)) ;
#57409 = CARTESIAN_POINT('Ctrl Pts',(178.341327732312,503.922720068571,-37.6418456226678)) ;
#57410 = CARTESIAN_POINT('Ctrl Pts',(178.343347068838,503.922338580399,-37.6468321520644)) ;
#57411 = CARTESIAN_POINT('Ctrl Pts',(178.345391051792,503.921956553687,-37.6518092750848)) ;
#57412 = CARTESIAN_POINT('Ctrl Pts',(178.368764899837,503.917587909471,-37.7087248755417)) ;
#57413 = CARTESIAN_POINT('Ctrl Pts',(178.395366603873,503.913149537041,-37.7644141769854)) ;
#57414 = CARTESIAN_POINT('Ctrl Pts',(178.425006750074,503.908714728987,-37.8185141372354)) ;
#57415 = CARTESIAN_POINT('Ctrl Pts',(178.454095033182,503.904362491608,-37.8716068227185)) ;
#57416 = CARTESIAN_POINT('Ctrl Pts',(178.4861092995,503.900013971222,-37.9231691105662)) ;
#57417 = CARTESIAN_POINT('Ctrl Pts',(178.520840616235,503.895718207472,-37.9728834949947)) ;
#57418 = CARTESIAN_POINT('Ctrl Pts',(178.555549958685,503.891425161625,-38.022566425446)) ;
#57419 = CARTESIAN_POINT('Ctrl Pts',(178.592972820244,503.887184948401,-38.0704038862008)) ;
#57420 = CARTESIAN_POINT('Ctrl Pts',(178.632873694272,503.883022943935,-38.1161018881213)) ;
#57421 = CARTESIAN_POINT('Ctrl Pts',(178.672764490276,503.878861990693,-38.1617883477998)) ;
#57422 = CARTESIAN_POINT('Ctrl Pts',(178.715132046167,503.874779217299,-38.2053363939955)) ;
#57423 = CARTESIAN_POINT('Ctrl Pts',(178.759714728454,503.870775300502,-38.2464747332912)) ;
#57424 = CARTESIAN_POINT('Ctrl Pts',(178.805835339648,503.866633264169,-38.289032185076)) ;
#57425 = CARTESIAN_POINT('Ctrl Pts',(178.854326775488,503.862575649729,-38.3290104882774)) ;
#57426 = CARTESIAN_POINT('Ctrl Pts',(178.904869225075,503.858576217504,-38.366136231121)) ;
#57427 = CARTESIAN_POINT('Ctrl Pts',(178.953790136573,503.854705097851,-38.4020708800111)) ;
#57428 = CARTESIAN_POINT('Ctrl Pts',(179.0046325257,503.850888107131,-38.4353329188909)) ;
#57429 = CARTESIAN_POINT('Ctrl Pts',(179.057077687018,503.847079649913,-38.4657022473033)) ;
#57430 = CARTESIAN_POINT('Ctrl Pts',(179.112130378247,503.843081839363,-38.497581513529)) ;
#57431 = CARTESIAN_POINT('Ctrl Pts',(179.168949600054,503.839093056456,-38.5262723939944)) ;
#57432 = CARTESIAN_POINT('Ctrl Pts',(179.227131085679,503.835041364962,-38.5515596619594)) ;
#57433 = CARTESIAN_POINT('Ctrl Pts',(179.277282753221,503.831548860729,-38.5733569509497)) ;
#57434 = CARTESIAN_POINT('Ctrl Pts',(179.328447463615,503.828008951363,-38.5926258227454)) ;
#57435 = CARTESIAN_POINT('Ctrl Pts',(179.38033975834,503.824369851754,-38.6092581066902)) ;
#57436 = CARTESIAN_POINT('Ctrl Pts',(179.388630549264,503.823788435685,-38.6119154335535)) ;
#57437 = CARTESIAN_POINT('Ctrl Pts',(179.396939973992,503.823204487666,-38.6145055474257)) ;
#57438 = CARTESIAN_POINT('Ctrl Pts',(179.40526694138,503.822617796502,-38.6170281069471)) ;
#57439 = CARTESIAN_POINT('Ctrl Pts',(179.405284738878,503.822616542548,-38.6170334984955)) ;
#57440 = CARTESIAN_POINT('Ctrl Pts',(179.405302536456,503.822615288581,-38.6170388897353)) ;
#57441 = CARTESIAN_POINT('Ctrl Pts',(179.405320334114,503.822614034602,-38.6170442806666)) ;
#57442 = CARTESIAN_POINT('Ctrl Pts',(179.459114130303,503.818823856251,-38.6333384837133)) ;
#57443 = CARTESIAN_POINT('Ctrl Pts',(179.51383105719,503.814909288754,-38.6468629521616)) ;
#57444 = CARTESIAN_POINT('Ctrl Pts',(179.569163664211,503.810932683327,-38.6575552545591)) ;
#57445 = CARTESIAN_POINT('Ctrl Pts',(179.574727537931,503.810532822709,-38.6586304003642)) ;
#57446 = CARTESIAN_POINT('Ctrl Pts',(179.580297596578,503.810132334828,-38.6596769268195)) ;
#57447 = CARTESIAN_POINT('Ctrl Pts',(179.585873500983,503.809731283076,-38.6606947822229)) ;
#57448 = CARTESIAN_POINT('Ctrl Pts',(179.646772382743,503.805351078281,-38.6718115897136)) ;
#57449 = CARTESIAN_POINT('Ctrl Pts',(179.708374311401,503.800904247445,-38.6795065722235)) ;
#57450 = CARTESIAN_POINT('Ctrl Pts',(179.770275049275,503.796459988522,-38.6837445858013)) ;
#57451 = CARTESIAN_POINT('Ctrl Pts',(179.832099134149,503.792021233019,-38.6879773513567)) ;
#57452 = CARTESIAN_POINT('Ctrl Pts',(179.894221385486,503.787585383282,-38.6887620718713)) ;
#57453 = CARTESIAN_POINT('Ctrl Pts',(179.956244665505,503.783200795414,-38.6861020651215)) ;
#57454 = CARTESIAN_POINT('Ctrl Pts',(180.018210642834,503.778820258423,-38.6834445159254)) ;
#57455 = CARTESIAN_POINT('Ctrl Pts',(180.080077914972,503.774491024919,-38.6773487223369)) ;
#57456 = CARTESIAN_POINT('Ctrl Pts',(180.141454597477,503.770237265217,-38.6678527022962)) ;
#57457 = CARTESIAN_POINT('Ctrl Pts',(180.202793856304,503.765986099193,-38.6583624723372)) ;
#57458 = CARTESIAN_POINT('Ctrl Pts',(180.263643139769,503.761810307832,-38.6454761070374)) ;
#57459 = CARTESIAN_POINT('Ctrl Pts',(180.323614662971,503.757709050637,-38.6292657966812)) ;
#57460 = CARTESIAN_POINT('Ctrl Pts',(180.383591701399,503.753607416273,-38.6130539955585)) ;
#57461 = CARTESIAN_POINT('Ctrl Pts',(180.442690750923,503.749580195423,-38.5935174427467)) ;
#57462 = CARTESIAN_POINT('Ctrl Pts',(180.500527671737,503.745602617334,-38.5707644991912)) ;
#57463 = CARTESIAN_POINT('Ctrl Pts',(180.558362453561,503.741625186349,-38.5480123971105)) ;
#57464 = CARTESIAN_POINT('Ctrl Pts',(180.614935016818,503.737697101935,-38.5220438186177)) ;
#57465 = CARTESIAN_POINT('Ctrl Pts',(180.669866841495,503.733772827799,-38.4930071535775)) ;
#57466 = CARTESIAN_POINT('Ctrl Pts',(180.724853414895,503.729844642471,-38.4639415486586)) ;
#57467 = CARTESIAN_POINT('Ctrl Pts',(180.778195592547,503.725919770956,-38.4318013003984)) ;
#57468 = CARTESIAN_POINT('Ctrl Pts',(180.829523466653,503.721937643725,-38.3967811409211)) ;
#57469 = CARTESIAN_POINT('Ctrl Pts',(180.877500769541,503.718215461039,-38.3640470207639)) ;
#57470 = CARTESIAN_POINT('Ctrl Pts',(180.923717771023,503.714442599911,-38.328796849899)) ;
#57471 = CARTESIAN_POINT('Ctrl Pts',(180.967886278451,503.710565160535,-38.2912310516112)) ;
#57472 = CARTESIAN_POINT('',(180.986277812533,503.710572730308,-35.767785970461)) ;
#57473 = CARTESIAN_POINT('Origin',(179.888527625402,503.710565160536,-37.0221601717597)) ;
#57474 = CARTESIAN_POINT('',(179.889393904536,504.332863786117,-35.3566333596088)) ;
#57475 = CARTESIAN_POINT('Ctrl Pts',(180.986277823167,503.710572730446,-35.7677859583096)) ;
#57476 = CARTESIAN_POINT('Ctrl Pts',(181.025946282702,503.714173642747,-35.80254219037)) ;
#57477 = CARTESIAN_POINT('Ctrl Pts',(181.063994730973,503.717871345489,-35.8392839762004)) ;
#57478 = CARTESIAN_POINT('Ctrl Pts',(181.100234837561,503.721611907053,-35.8778191803887)) ;
#57479 = CARTESIAN_POINT('Ctrl Pts',(181.141662721888,503.725887930674,-35.9218707059471)) ;
#57480 = CARTESIAN_POINT('Ctrl Pts',(181.180728271362,503.730219400517,-35.968266856604)) ;
#57481 = CARTESIAN_POINT('Ctrl Pts',(181.217191089831,503.734540179259,-36.0167042937996)) ;
#57482 = CARTESIAN_POINT('Ctrl Pts',(181.253616739054,503.738856553511,-36.0650923551351)) ;
#57483 = CARTESIAN_POINT('Ctrl Pts',(181.28744524273,503.743161960478,-36.1155174111814)) ;
#57484 = CARTESIAN_POINT('Ctrl Pts',(181.318471176994,503.747411226951,-36.1676599529123)) ;
#57485 = CARTESIAN_POINT('Ctrl Pts',(181.349477256015,503.75165777408,-36.2197691256952)) ;
#57486 = CARTESIAN_POINT('Ctrl Pts',(181.37768444688,503.755848134438,-36.2735935477084)) ;
#57487 = CARTESIAN_POINT('Ctrl Pts',(181.402919132954,503.759961017888,-36.3287984240804)) ;
#57488 = CARTESIAN_POINT('Ctrl Pts',(181.428147243903,503.764072829689,-36.3839889163229)) ;
#57489 = CARTESIAN_POINT('Ctrl Pts',(181.450404341474,503.768107214459,-36.4405591329151)) ;
#57490 = CARTESIAN_POINT('Ctrl Pts',(181.469548102683,503.772067476304,-36.4981589818455)) ;
#57491 = CARTESIAN_POINT('Ctrl Pts',(181.48870799007,503.776031074165,-36.5558073513022)) ;
#57492 = CARTESIAN_POINT('Ctrl Pts',(181.504749098426,503.779920548214,-36.6144870871759)) ;
#57493 = CARTESIAN_POINT('Ctrl Pts',(181.517561865967,503.783762848219,-36.6738316995243)) ;
#57494 = CARTESIAN_POINT('Ctrl Pts',(181.530379446178,503.78760659145,-36.7331986026101)) ;
#57495 = CARTESIAN_POINT('Ctrl Pts',(181.539965920586,503.791403398421,-36.7932308646697)) ;
#57496 = CARTESIAN_POINT('Ctrl Pts',(181.546248715336,503.795200953853,-36.8535461696402)) ;
#57497 = CARTESIAN_POINT('Ctrl Pts',(181.552543441867,503.7990057213,-36.9139760206226)) ;
#57498 = CARTESIAN_POINT('Ctrl Pts',(181.555521397616,503.802811714112,-36.9746898924054)) ;
#57499 = CARTESIAN_POINT('Ctrl Pts',(181.555153363817,503.806682125672,-37.0352885712453)) ;
#57500 = CARTESIAN_POINT('Ctrl Pts',(181.554822660227,503.810159955687,-37.0897406368495)) ;
#57501 = CARTESIAN_POINT('Ctrl Pts',(181.551790367297,503.813690388526,-37.1441000848864)) ;
#57502 = CARTESIAN_POINT('Ctrl Pts',(181.546071963646,503.817323767339,-37.1980669538674)) ;
#57503 = CARTESIAN_POINT('Ctrl Pts',(181.545561384502,503.817648180857,-37.2028854940467)) ;
#57504 = CARTESIAN_POINT('Ctrl Pts',(181.545029409859,503.817973415077,-37.2077009334435)) ;
#57505 = CARTESIAN_POINT('Ctrl Pts',(181.544476061327,503.818299505835,-37.2125130758366)) ;
#57506 = CARTESIAN_POINT('Ctrl Pts',(181.544472262003,503.818301744794,-37.2125461162941)) ;
#57507 = CARTESIAN_POINT('Ctrl Pts',(181.544468461671,503.818303983793,-37.2125791565962)) ;
#57508 = CARTESIAN_POINT('Ctrl Pts',(181.544464660332,503.818306222832,-37.2126121967428)) ;
#57509 = CARTESIAN_POINT('Ctrl Pts',(181.538117217828,503.822044950919,-37.2677823393863)) ;
#57510 = CARTESIAN_POINT('Ctrl Pts',(181.528929085212,503.825906180113,-37.322717557164)) ;
#57511 = CARTESIAN_POINT('Ctrl Pts',(181.516962532995,503.829826849693,-37.3771152557338)) ;
#57512 = CARTESIAN_POINT('Ctrl Pts',(181.515848262687,503.830191924413,-37.3821805192507)) ;
#57513 = CARTESIAN_POINT('Ctrl Pts',(181.514709928829,503.83055751451,-37.387241096116)) ;
#57514 = CARTESIAN_POINT('Ctrl Pts',(181.513547598479,503.830923569071,-37.3922967264089)) ;
#57515 = CARTESIAN_POINT('Ctrl Pts',(181.499764589189,503.835264274287,-37.4522468079656)) ;
#57516 = CARTESIAN_POINT('Ctrl Pts',(181.482603360873,503.839669629951,-37.5115058139305)) ;
#57517 = CARTESIAN_POINT('Ctrl Pts',(181.462191697142,503.844068815616,-37.5696883361893)) ;
#57518 = CARTESIAN_POINT('Ctrl Pts',(181.442039499626,503.848412080309,-37.627131261763)) ;
#57519 = CARTESIAN_POINT('Ctrl Pts',(181.418719347169,503.852749038788,-37.6835251288724)) ;
#57520 = CARTESIAN_POINT('Ctrl Pts',(181.392387562637,503.857032081953,-37.7385193943068)) ;
#57521 = CARTESIAN_POINT('Ctrl Pts',(181.366071706209,503.861312534304,-37.7934803936946)) ;
#57522 = CARTESIAN_POINT('Ctrl Pts',(181.336747959414,503.865539001473,-37.847043568874)) ;
#57523 = CARTESIAN_POINT('Ctrl Pts',(181.304602610932,503.86968777188,-37.8988771403132)) ;
#57524 = CARTESIAN_POINT('Ctrl Pts',(181.272464844239,503.873835563761,-37.9506984863057)) ;
#57525 = CARTESIAN_POINT('Ctrl Pts',(181.237506788954,503.87790569354,-38.0007910131001)) ;
#57526 = CARTESIAN_POINT('Ctrl Pts',(181.199944289675,503.881899267768,-38.048840908492)) ;
#57527 = CARTESIAN_POINT('Ctrl Pts',(181.161489538531,503.885987704534,-38.0980321711941)) ;
#57528 = CARTESIAN_POINT('Ctrl Pts',(181.120304903677,503.889995932486,-38.1450823750831)) ;
#57529 = CARTESIAN_POINT('Ctrl Pts',(181.076655216884,503.893951128991,-38.1896754883366)) ;
#57530 = CARTESIAN_POINT('Ctrl Pts',(181.033964008986,503.897819475564,-38.2332894065256)) ;
#57531 = CARTESIAN_POINT('Ctrl Pts',(180.988914761083,503.901637447854,-38.2745527568117)) ;
#57532 = CARTESIAN_POINT('Ctrl Pts',(180.94178849477,503.905451918346,-38.3131923884192)) ;
#57533 = CARTESIAN_POINT('Ctrl Pts',(180.893075149975,503.909394849345,-38.3531332928131)) ;
#57534 = CARTESIAN_POINT('Ctrl Pts',(180.842142081548,503.913334469124,-38.3902700821888)) ;
#57535 = CARTESIAN_POINT('Ctrl Pts',(180.789339977226,503.917340157934,-38.4243323963118)) ;
#57536 = CARTESIAN_POINT('Ctrl Pts',(180.743396128359,503.920825563746,-38.453970491843)) ;
#57537 = CARTESIAN_POINT('Ctrl Pts',(180.696036557341,503.924361639824,-38.4812815026592)) ;
#57538 = CARTESIAN_POINT('Ctrl Pts',(180.647522868314,503.927999005388,-38.5061118036851)) ;
#57539 = CARTESIAN_POINT('Ctrl Pts',(180.640308509786,503.928539909611,-38.5098042603412)) ;
#57540 = CARTESIAN_POINT('Ctrl Pts',(180.633068590654,503.929083053748,-38.5134419444454)) ;
#57541 = CARTESIAN_POINT('Ctrl Pts',(180.625803928338,503.92962860426,-38.5170244397967)) ;
#57542 = CARTESIAN_POINT('Ctrl Pts',(180.625776227412,503.929630684501,-38.5170381002305)) ;
#57543 = CARTESIAN_POINT('Ctrl Pts',(180.625748526126,503.929632764778,-38.5170517598619)) ;
#57544 = CARTESIAN_POINT('Ctrl Pts',(180.625720824481,503.92963484509,-38.5170654186909)) ;
#57545 = CARTESIAN_POINT('Ctrl Pts',(180.575999633131,503.933368759793,-38.5415814082224)) ;
#57546 = CARTESIAN_POINT('Ctrl Pts',(180.524937783754,503.937225215228,-38.563592697846)) ;
#57547 = CARTESIAN_POINT('Ctrl Pts',(180.472822234143,503.941140992713,-38.582987229563)) ;
#57548 = CARTESIAN_POINT('Ctrl Pts',(180.467990408081,503.941504038979,-38.5847853685928)) ;
#57549 = CARTESIAN_POINT('Ctrl Pts',(180.463149560691,503.941867595168,-38.586561022526)) ;
#57550 = CARTESIAN_POINT('Ctrl Pts',(180.458299942609,503.942231610897,-38.5883141075688)) ;
#57551 = CARTESIAN_POINT('Ctrl Pts',(180.40043283571,503.946575156459,-38.6092324474977)) ;
#57552 = CARTESIAN_POINT('Ctrl Pts',(180.341311015314,503.950983464914,-38.6269365125238)) ;
#57553 = CARTESIAN_POINT('Ctrl Pts',(180.281328632211,503.955385157311,-38.6413236454677)) ;
#57554 = CARTESIAN_POINT('Ctrl Pts',(180.222247370112,503.959720722668,-38.6554946391551)) ;
#57555 = CARTESIAN_POINT('Ctrl Pts',(180.162331216653,503.96404958664,-38.6664480600204)) ;
#57556 = CARTESIAN_POINT('Ctrl Pts',(180.101957983656,503.968324092576,-38.6741248465967)) ;
#57557 = CARTESIAN_POINT('Ctrl Pts',(180.041622242767,503.97259594402,-38.6817968658464)) ;
#57558 = CARTESIAN_POINT('Ctrl Pts',(179.980829976647,503.976813370938,-38.686196445756)) ;
#57559 = CARTESIAN_POINT('Ctrl Pts',(179.919959587964,503.980952576775,-38.6872998714748)) ;
#57560 = CARTESIAN_POINT('Ctrl Pts',(179.859104293839,503.985090756178,-38.6884030235676)) ;
#57561 = CARTESIAN_POINT('Ctrl Pts',(179.798170937088,503.989150751186,-38.6862116238091)) ;
#57562 = CARTESIAN_POINT('Ctrl Pts',(179.737538894785,503.993133537007,-38.6807365485424)) ;
#57563 = CARTESIAN_POINT('Ctrl Pts',(179.675211763591,503.997227669498,-38.6751084066972)) ;
#57564 = CARTESIAN_POINT('Ctrl Pts',(179.613203102409,504.001240224082,-38.6660100621272)) ;
#57565 = CARTESIAN_POINT('Ctrl Pts',(179.551925650776,504.005198583097,-38.6534930410653)) ;
#57566 = CARTESIAN_POINT('Ctrl Pts',(179.49223897753,504.009054182095,-38.6413009650862)) ;
#57567 = CARTESIAN_POINT('Ctrl Pts',(179.433246182249,504.012858731079,-38.6258652821553)) ;
#57568 = CARTESIAN_POINT('Ctrl Pts',(179.375327730127,504.016659006697,-38.6072738104232)) ;
#57569 = CARTESIAN_POINT('Ctrl Pts',(179.315093800773,504.02061121061,-38.5879390845484)) ;
#57570 = CARTESIAN_POINT('Ctrl Pts',(179.256022189819,504.024559211105,-38.5651903779576)) ;
#57571 = CARTESIAN_POINT('Ctrl Pts',(179.198536157218,504.02857361947,-38.5391783218387)) ;
#57572 = CARTESIAN_POINT('Ctrl Pts',(179.14880772746,504.032046293012,-38.5166765305859)) ;
#57573 = CARTESIAN_POINT('Ctrl Pts',(179.100264884407,504.035569318995,-38.4917324825779)) ;
#57574 = CARTESIAN_POINT('Ctrl Pts',(179.0531776563,504.039193368418,-38.4644828027308)) ;
#57575 = CARTESIAN_POINT('Ctrl Pts',(179.045858000477,504.039756722761,-38.4602468711253)) ;
#57576 = CARTESIAN_POINT('Ctrl Pts',(179.038573417292,504.04032251827,-38.4559552409651)) ;
#57577 = CARTESIAN_POINT('Ctrl Pts',(179.031324808433,504.040890945281,-38.4516084395122)) ;
#57578 = CARTESIAN_POINT('Ctrl Pts',(179.031299138759,504.040892958265,-38.451593046079)) ;
#57579 = CARTESIAN_POINT('Ctrl Pts',(179.031273469536,504.040894971282,-38.4515776519539)) ;
#57580 = CARTESIAN_POINT('Ctrl Pts',(179.031247800765,504.040896984333,-38.4515622571369)) ;
#57581 = CARTESIAN_POINT('Ctrl Pts',(178.983709945429,504.044625097892,-38.4230514819521)) ;
#57582 = CARTESIAN_POINT('Ctrl Pts',(178.937552118394,504.048476294638,-38.3920576524867)) ;
#57583 = CARTESIAN_POINT('Ctrl Pts',(178.893023657722,504.052387432178,-38.3587614226577)) ;
#57584 = CARTESIAN_POINT('Ctrl Pts',(178.888860064263,504.052753139558,-38.3556480887891)) ;
#57585 = CARTESIAN_POINT('Ctrl Pts',(178.884710729245,504.053119371001,-38.3525146603628)) ;
#57586 = CARTESIAN_POINT('Ctrl Pts',(178.880575863895,504.053486074888,-38.3493613070806)) ;
#57587 = CARTESIAN_POINT('Ctrl Pts',(178.831649049199,504.05782518913,-38.3120484761493)) ;
#57588 = CARTESIAN_POINT('Ctrl Pts',(178.784745748647,504.06222978468,-38.2719403856926)) ;
#57589 = CARTESIAN_POINT('Ctrl Pts',(178.740165376907,504.066628466276,-38.2293129576102)) ;
#57590 = CARTESIAN_POINT('Ctrl Pts',(178.696226804807,504.070963822419,-38.1872992136885)) ;
#57591 = CARTESIAN_POINT('Ctrl Pts',(178.654544388054,504.075293146648,-38.1428383973493)) ;
#57592 = CARTESIAN_POINT('Ctrl Pts',(178.615372496037,504.07956861893,-38.0962167323261)) ;
#57593 = CARTESIAN_POINT('Ctrl Pts',(178.576224659597,504.083841465632,-38.0496236978077)) ;
#57594 = CARTESIAN_POINT('Ctrl Pts',(178.539584148741,504.088060391233,-38.0008725250665)) ;
#57595 = CARTESIAN_POINT('Ctrl Pts',(178.50567587558,504.092201451286,-37.950269012115)) ;
#57596 = CARTESIAN_POINT('Ctrl Pts',(178.471775817483,504.096341508071,-37.8996777590359)) ;
#57597 = CARTESIAN_POINT('Ctrl Pts',(178.440606709769,504.100403734332,-37.8472350625964)) ;
#57598 = CARTESIAN_POINT('Ctrl Pts',(178.412364887662,504.104388987196,-37.7932662174788)) ;
#57599 = CARTESIAN_POINT('Ctrl Pts',(178.38336594261,504.108481079002,-37.7378505446471)) ;
#57600 = CARTESIAN_POINT('Ctrl Pts',(178.357453670579,504.112492027932,-37.6808256691424)) ;
#57601 = CARTESIAN_POINT('Ctrl Pts',(178.33480771692,504.116449022292,-37.622565670781)) ;
#57602 = CARTESIAN_POINT('Ctrl Pts',(178.312724852657,504.120307626379,-37.5657543015131)) ;
#57603 = CARTESIAN_POINT('Ctrl Pts',(178.293748080204,504.124115289283,-37.5077685123963)) ;
#57604 = CARTESIAN_POINT('Ctrl Pts',(178.27800969468,504.127918723497,-37.4489760990798)) ;
#57605 = CARTESIAN_POINT('Ctrl Pts',(178.261669341185,504.131867632962,-37.3879349703697)) ;
#57606 = CARTESIAN_POINT('Ctrl Pts',(178.248820705576,504.135812404332,-37.3260241937824)) ;
#57607 = CARTESIAN_POINT('Ctrl Pts',(178.23956602147,504.139823266144,-37.2636794060451)) ;
#57608 = CARTESIAN_POINT('Ctrl Pts',(178.231544361973,504.14329975085,-37.2096409696274)) ;
#57609 = CARTESIAN_POINT('Ctrl Pts',(178.22622250326,504.146826543878,-37.1552755703853)) ;
#57610 = CARTESIAN_POINT('Ctrl Pts',(178.223631999662,504.15045438272,-37.1008847160766)) ;
#57611 = CARTESIAN_POINT('Ctrl Pts',(178.223235216675,504.151010052563,-37.0925537623512)) ;
#57612 = CARTESIAN_POINT('Ctrl Pts',(178.222902446833,504.151568092995,-37.0842221367079)) ;
#57613 = CARTESIAN_POINT('Ctrl Pts',(178.222633734156,504.152128686334,-37.0758908393388)) ;
#57614 = CARTESIAN_POINT('Ctrl Pts',(178.222632780434,504.152130676006,-37.0758612696975)) ;
#57615 = CARTESIAN_POINT('Ctrl Pts',(178.22263182752,504.152132665709,-37.0758317000604)) ;
#57616 = CARTESIAN_POINT('Ctrl Pts',(178.222630875412,504.152134655445,-37.0758021304273)) ;
#57617 = CARTESIAN_POINT('Ctrl Pts',(178.220846087648,504.155864544243,-37.0203719331003)) ;
#57618 = CARTESIAN_POINT('Ctrl Pts',(178.221898634255,504.159717283414,-36.9647570884874)) ;
#57619 = CARTESIAN_POINT('Ctrl Pts',(178.225771600282,504.163629724937,-36.909265371742)) ;
#57620 = CARTESIAN_POINT('Ctrl Pts',(178.226132585354,504.163994389377,-36.9040931907217)) ;
#57621 = CARTESIAN_POINT('Ctrl Pts',(178.226518050009,504.164359572476,-36.8989221091583)) ;
#57622 = CARTESIAN_POINT('Ctrl Pts',(178.2269279662,504.164725223103,-36.893752394232)) ;
#57623 = CARTESIAN_POINT('Ctrl Pts',(178.231791448608,504.169063513302,-36.8324159108179)) ;
#57624 = CARTESIAN_POINT('Ctrl Pts',(178.240100224105,504.173466950864,-36.7712667789477)) ;
#57625 = CARTESIAN_POINT('Ctrl Pts',(178.251784480751,504.177864274275,-36.710705959758)) ;
#57626 = CARTESIAN_POINT('Ctrl Pts',(178.263303322816,504.182199344568,-36.6510025029893)) ;
#57627 = CARTESIAN_POINT('Ctrl Pts',(178.278102341194,504.18652818541,-36.5918706425448)) ;
#57628 = CARTESIAN_POINT('Ctrl Pts',(178.296078632547,504.190803066331,-36.5336793420849)) ;
#57629 = CARTESIAN_POINT('Ctrl Pts',(178.314043956525,504.195075339138,-36.4755235442623)) ;
#57630 = CARTESIAN_POINT('Ctrl Pts',(178.335182566682,504.199293582935,-36.4183070920453)) ;
#57631 = CARTESIAN_POINT('Ctrl Pts',(178.359359152784,504.203433949214,-36.3623847921564)) ;
#57632 = CARTESIAN_POINT('Ctrl Pts',(178.383529968864,504.207573327346,-36.3064758387721)) ;
#57633 = CARTESIAN_POINT('Ctrl Pts',(178.410737331575,504.211634862792,-36.2518604502738)) ;
#57634 = CARTESIAN_POINT('Ctrl Pts',(178.440814060322,504.215619510201,-36.1988799748682)) ;
#57635 = CARTESIAN_POINT('Ctrl Pts',(178.471683800588,504.219709217948,-36.1445026012948)) ;
#57636 = CARTESIAN_POINT('Ctrl Pts',(178.50557649632,504.223717945013,-36.0918476971024)) ;
#57637 = CARTESIAN_POINT('Ctrl Pts',(178.542275190797,504.227672939551,-36.041268561789)) ;
#57638 = CARTESIAN_POINT('Ctrl Pts',(178.578077018835,504.231531279374,-35.9919255121081)) ;
#57639 = CARTESIAN_POINT('Ctrl Pts',(178.616549439427,504.235338843381,-35.9445581959155)) ;
#57640 = CARTESIAN_POINT('Ctrl Pts',(178.65745484286,504.239142415311,-35.8994771634488)) ;
#57641 = CARTESIAN_POINT('Ctrl Pts',(178.69989731935,504.243088911341,-35.8527021533026)) ;
#57642 = CARTESIAN_POINT('Ctrl Pts',(178.744959640762,504.2470315321,-35.808389125236)) ;
#57643 = CARTESIAN_POINT('Ctrl Pts',(178.792331462551,504.251040416332,-35.7668594981143)) ;
#57644 = CARTESIAN_POINT('Ctrl Pts',(178.833406729212,504.254516448764,-35.7308498948544)) ;
#57645 = CARTESIAN_POINT('Ctrl Pts',(178.876218948242,504.258042955032,-35.696932219074)) ;
#57646 = CARTESIAN_POINT('Ctrl Pts',(178.92053188491,504.261670629236,-35.6652962359978)) ;
#57647 = CARTESIAN_POINT('Ctrl Pts',(178.927300464559,504.262224738344,-35.6604639976644)) ;
#57648 = CARTESIAN_POINT('Ctrl Pts',(178.934104084428,504.262781207804,-35.6556848982313)) ;
#57649 = CARTESIAN_POINT('Ctrl Pts',(178.940941934694,504.263340218276,-35.6509595114309)) ;
#57650 = CARTESIAN_POINT('Ctrl Pts',(178.940966471226,504.263342224195,-35.6509425551364)) ;
#57651 = CARTESIAN_POINT('Ctrl Pts',(178.940991008198,504.263344230148,-35.6509255995334)) ;
#57652 = CARTESIAN_POINT('Ctrl Pts',(178.941015545612,504.263346236133,-35.650908644622)) ;
#57653 = CARTESIAN_POINT('Ctrl Pts',(178.986944662912,504.267101037983,-35.6191724502927)) ;
#57654 = CARTESIAN_POINT('Ctrl Pts',(179.034583862883,504.2709801353,-35.5897545977169)) ;
#57655 = CARTESIAN_POINT('Ctrl Pts',(179.083663645032,504.274919333971,-35.5628072016248)) ;
#57656 = CARTESIAN_POINT('Ctrl Pts',(179.088570639873,504.275313174911,-35.5601130019402)) ;
#57657 = CARTESIAN_POINT('Ctrl Pts',(179.09349199182,504.275707616624,-35.5574434950931)) ;
#57658 = CARTESIAN_POINT('Ctrl Pts',(179.098427403031,504.276102594954,-35.5547988311475)) ;
#57659 = CARTESIAN_POINT('Ctrl Pts',(179.152635977017,504.280440878255,-35.5257509048351)) ;
#57660 = CARTESIAN_POINT('Ctrl Pts',(179.208546689207,504.284843266207,-35.499699719582)) ;
#57661 = CARTESIAN_POINT('Ctrl Pts',(179.265791140492,504.289239112474,-35.4768014184793)) ;
#57662 = CARTESIAN_POINT('Ctrl Pts',(179.322947672265,504.293628207333,-35.4539382859812)) ;
#57663 = CARTESIAN_POINT('Ctrl Pts',(179.381433839323,504.298010444336,-35.4342179835861)) ;
#57664 = CARTESIAN_POINT('Ctrl Pts',(179.440876471456,504.302336984258,-35.4177585037803)) ;
#57665 = CARTESIAN_POINT('Ctrl Pts',(179.500265672515,504.306659635192,-35.4013138188721)) ;
#57666 = CARTESIAN_POINT('Ctrl Pts',(179.560609664863,504.310926549102,-35.388123959882)) ;
#57667 = CARTESIAN_POINT('Ctrl Pts',(179.621529458883,504.315113966885,-35.3782729958669)) ;
#57668 = CARTESIAN_POINT('Ctrl Pts',(179.682417740684,504.319299218626,-35.3684271274981)) ;
#57669 = CARTESIAN_POINT('Ctrl Pts',(179.743881263251,504.323405051185,-35.3619167450483)) ;
#57670 = CARTESIAN_POINT('Ctrl Pts',(179.805534178045,504.327433730372,-35.3587928477403)) ;
#57671 = CARTESIAN_POINT('Ctrl Pts',(179.833460793808,504.32925858125,-35.3573778314333)) ;
#57672 = CARTESIAN_POINT('Ctrl Pts',(179.861426164107,504.331067955713,-35.3566571930793)) ;
#57673 = CARTESIAN_POINT('Ctrl Pts',(179.889393904536,504.332863786117,-35.3566333596088)) ;
#57674 = CARTESIAN_POINT('Ctrl Pts',(179.889376469388,504.333136041102,-35.356160388007)) ;
#57675 = CARTESIAN_POINT('Ctrl Pts',(179.962317757491,504.3377604451,-35.3561975523419)) ;
#57676 = CARTESIAN_POINT('Ctrl Pts',(180.035181643089,504.342252983734,-35.3610248634196)) ;
#57677 = CARTESIAN_POINT('Ctrl Pts',(180.211581870764,504.353134911495,-35.3844131273454)) ;
#57678 = CARTESIAN_POINT('Ctrl Pts',(180.314114978436,504.359460830589,-35.4080194385543)) ;
#57679 = CARTESIAN_POINT('Ctrl Pts',(180.430608289387,504.367296800496,-35.4467171416852)) ;
#57680 = CARTESIAN_POINT('Ctrl Pts',(180.447390450651,504.36844237917,-35.4525919563438)) ;
#57681 = CARTESIAN_POINT('Ctrl Pts',(180.464073435314,504.369601015799,-35.4587334799406)) ;
#57682 = CARTESIAN_POINT('Origin',(179.888527625422,620.256490441073,-37.0221601717597)) ;
#57683 = CARTESIAN_POINT('',(181.517739097406,616.918146095397,-35.7700948611419)) ;
#57684 = CARTESIAN_POINT('',(181.517739074368,616.85992786049,-35.7700948311641)) ;
#57685 = CARTESIAN_POINT('',(181.517739089189,620.256490441073,-35.7700948504488)) ;
#57686 = CARTESIAN_POINT('',(179.065295445318,616.710565160536,-35.1395326620963)) ;
#57687 = CARTESIAN_POINT('Ctrl Pts',(181.517739074368,616.85992786049,-35.7700948311641)) ;
#57688 = CARTESIAN_POINT('Ctrl Pts',(181.506609107836,616.858866348378,-35.7556123051225)) ;
#57689 = CARTESIAN_POINT('Ctrl Pts',(181.495285009743,616.857799228944,-35.741276854028)) ;
#57690 = CARTESIAN_POINT('Ctrl Pts',(181.39714883938,616.848663946389,-35.6203944242632)) ;
#57691 = CARTESIAN_POINT('Ctrl Pts',(181.300047612677,616.840327777811,-35.5226622490848)) ;
#57692 = CARTESIAN_POINT('Ctrl Pts',(181.155040681315,616.829340879517,-35.4033714355429)) ;
#57693 = CARTESIAN_POINT('Ctrl Pts',(181.114994883078,616.826441830741,-35.3728236061938)) ;
#57694 = CARTESIAN_POINT('Ctrl Pts',(181.049444651431,616.82195796045,-35.3265296152158)) ;
#57695 = CARTESIAN_POINT('Ctrl Pts',(181.024650646624,616.820319711129,-35.3098178704186)) ;
#57696 = CARTESIAN_POINT('Ctrl Pts',(180.964094489759,616.816462006346,-35.270896475894)) ;
#57697 = CARTESIAN_POINT('Ctrl Pts',(180.927999232584,616.814274192439,-35.2492338086848)) ;
#57698 = CARTESIAN_POINT('Ctrl Pts',(180.794503903944,616.806491824449,-35.1745960578176)) ;
#57699 = CARTESIAN_POINT('Ctrl Pts',(180.693519165775,616.801177658522,-35.1284129259982)) ;
#57700 = CARTESIAN_POINT('Ctrl Pts',(180.468180350198,616.789637118546,-35.0466602879336)) ;
#57701 = CARTESIAN_POINT('Ctrl Pts',(180.343212053813,616.783417505349,-35.0142120406523)) ;
#57702 = CARTESIAN_POINT('Ctrl Pts',(180.157277050943,616.773810250216,-34.9841921653847)) ;
#57703 = CARTESIAN_POINT('Ctrl Pts',(180.098140669292,616.770707818637,-34.9772637601659)) ;
#57704 = CARTESIAN_POINT('Ctrl Pts',(179.983239558847,616.764551176367,-34.9688385471496)) ;
#57705 = CARTESIAN_POINT('Ctrl Pts',(179.92755007429,616.761509321861,-34.9670259885493)) ;
#57706 = CARTESIAN_POINT('Ctrl Pts',(179.813152576433,616.755131963,-34.9679540391312)) ;
#57707 = CARTESIAN_POINT('Ctrl Pts',(179.754497305784,616.751792334337,-34.9709460657023)) ;
#57708 = CARTESIAN_POINT('Ctrl Pts',(179.511442039914,616.737693994545,-34.9938142339676)) ;
#57709 = CARTESIAN_POINT('Ctrl Pts',(179.330042150489,616.726468516774,-35.0360909204514)) ;
#57710 = CARTESIAN_POINT('Ctrl Pts',(179.125992098987,616.714177429145,-35.1138565302351)) ;
#57711 = CARTESIAN_POINT('Ctrl Pts',(179.095487977552,616.712351867416,-35.1263301225568)) ;
#57712 = CARTESIAN_POINT('Ctrl Pts',(179.065295445318,616.710565160536,-35.1395326620961)) ;
#57713 = CARTESIAN_POINT('',(178.234449048513,616.711852647397,-35.799415550035)) ;
#57714 = CARTESIAN_POINT('Origin',(179.888527625422,616.710565160536,-37.0221601717597)) ;
#57715 = CARTESIAN_POINT('Ctrl Pts',(178.236389517568,616.713140134259,-35.8005066877149)) ;
#57716 = CARTESIAN_POINT('Ctrl Pts',(178.246281071676,616.714039061134,-35.7871295609758)) ;
#57717 = CARTESIAN_POINT('Ctrl Pts',(178.25633508351,616.714927007289,-35.773872585346)) ;
#57718 = CARTESIAN_POINT('Ctrl Pts',(178.280148287692,616.716974845351,-35.743252763817)) ;
#57719 = CARTESIAN_POINT('Ctrl Pts',(178.294029590926,616.718127209171,-35.7259872121017)) ;
#57720 = CARTESIAN_POINT('Ctrl Pts',(178.386281286779,616.725546033727,-35.6149700240209)) ;
#57721 = CARTESIAN_POINT('Ctrl Pts',(178.47260906756,616.731403820701,-35.5281360333275)) ;
#57722 = CARTESIAN_POINT('Ctrl Pts',(178.657151287698,616.743100547166,-35.3729644679706)) ;
#57723 = CARTESIAN_POINT('Ctrl Pts',(178.754617781303,616.748917689103,-35.3044933824928)) ;
#57724 = CARTESIAN_POINT('Ctrl Pts',(178.903393629093,616.757792529321,-35.2181840499202)) ;
#57725 = CARTESIAN_POINT('Ctrl Pts',(178.950350783986,616.760590155878,-35.1933238278685)) ;
#57726 = CARTESIAN_POINT('Ctrl Pts',(179.045990364134,616.766311283977,-35.1473432456521)) ;
#57727 = CARTESIAN_POINT('Ctrl Pts',(179.09463247113,616.76923234295,-35.1262336713056)) ;
#57728 = CARTESIAN_POINT('Ctrl Pts',(179.247680335172,616.778473618264,-35.0667373362296)) ;
#57729 = CARTESIAN_POINT('Ctrl Pts',(179.35441431837,616.785000864595,-35.0349306516471)) ;
#57730 = CARTESIAN_POINT('Ctrl Pts',(179.556339881529,616.797329737497,-34.9922056682046)) ;
#57731 = CARTESIAN_POINT('Ctrl Pts',(179.650752835576,616.803082489123,-34.9789941339355)) ;
#57732 = CARTESIAN_POINT('Ctrl Pts',(179.787019112059,616.811142508186,-34.9695019825114)) ;
#57733 = CARTESIAN_POINT('Ctrl Pts',(179.828375835261,616.813555838922,-34.9678739828228)) ;
#57734 = CARTESIAN_POINT('Ctrl Pts',(179.904154121519,616.817886019535,-34.967181646926)) ;
#57735 = CARTESIAN_POINT('Ctrl Pts',(179.938557529514,616.81981724856,-34.9677312374899)) ;
#57736 = CARTESIAN_POINT('Ctrl Pts',(180.003949330139,616.823401331865,-34.9704196844264)) ;
#57737 = CARTESIAN_POINT('Ctrl Pts',(180.034932991873,616.825060691311,-34.9723975660884)) ;
#57738 = CARTESIAN_POINT('Ctrl Pts',(180.137813650187,616.830473422,-34.9813098338369)) ;
#57739 = CARTESIAN_POINT('Ctrl Pts',(180.209394385912,616.83408306858,-34.9913327653996)) ;
#57740 = CARTESIAN_POINT('Ctrl Pts',(180.444109653757,616.845813294523,-35.0369219662064)) ;
#57741 = CARTESIAN_POINT('Ctrl Pts',(180.603423779144,616.853656347961,-35.0885710813705)) ;
#57742 = CARTESIAN_POINT('Ctrl Pts',(180.809038231136,616.865140915143,-35.1841604138706)) ;
#57743 = CARTESIAN_POINT('Ctrl Pts',(180.862201693352,616.868239308291,-35.2117622080527)) ;
#57744 = CARTESIAN_POINT('Ctrl Pts',(180.957293248508,616.874070777027,-35.2665336812578)) ;
#57745 = CARTESIAN_POINT('Ctrl Pts',(180.999581890234,616.876776150802,-35.2929863389798)) ;
#57746 = CARTESIAN_POINT('Ctrl Pts',(181.101309196086,616.883583339896,-35.36189261198)) ;
#57747 = CARTESIAN_POINT('Ctrl Pts',(181.159523288404,616.887747072433,-35.40602412492)) ;
#57748 = CARTESIAN_POINT('Ctrl Pts',(181.327103008902,616.900548417978,-35.5477277959752)) ;
#57749 = CARTESIAN_POINT('Ctrl Pts',(181.428501854798,616.909465413451,-35.6539776441301)) ;
#57750 = CARTESIAN_POINT('Ctrl Pts',(181.517739097406,616.918146095397,-35.7700948611417)) ;
#57751 = CARTESIAN_POINT('Origin',(179.888527625422,620.256490441073,-37.0221601717597)) ;
#57752 = CARTESIAN_POINT('',(181.517739089193,617.617803659368,-35.7700948504542)) ;
#57753 = CARTESIAN_POINT('',(181.517739089189,617.559637408341,-35.7700948504488)) ;
#57754 = CARTESIAN_POINT('',(181.517739089189,620.256490441073,-35.7700948504488)) ;
#57755 = CARTESIAN_POINT('',(179.887993154238,617.107857237813,-39.0769101022477)) ;
#57756 = CARTESIAN_POINT('Ctrl Pts',(181.517739089189,617.559637408341,-35.7700948504488)) ;
#57757 = CARTESIAN_POINT('Ctrl Pts',(181.502586585041,617.55838496062,-35.7503781207849)) ;
#57758 = CARTESIAN_POINT('Ctrl Pts',(181.48707049028,617.557121165613,-35.7309290693371)) ;
#57759 = CARTESIAN_POINT('Ctrl Pts',(181.436305398982,617.553037290777,-35.6696163119889)) ;
#57760 = CARTESIAN_POINT('Ctrl Pts',(181.399746698261,617.550170829413,-35.6288880856673)) ;
#57761 = CARTESIAN_POINT('Ctrl Pts',(181.325493689432,617.544453120502,-35.5525310944956)) ;
#57762 = CARTESIAN_POINT('Ctrl Pts',(181.287989926459,617.541611310833,-35.5167746163965)) ;
#57763 = CARTESIAN_POINT('Ctrl Pts',(181.177330663977,617.533335783561,-35.4189828374422)) ;
#57764 = CARTESIAN_POINT('Ctrl Pts',(181.101136387809,617.527758860662,-35.3606045772991)) ;
#57765 = CARTESIAN_POINT('Ctrl Pts',(180.906988104656,617.513927774877,-35.2323394139)) ;
#57766 = CARTESIAN_POINT('Ctrl Pts',(180.785577864741,617.505568757037,-35.1685096301611)) ;
#57767 = CARTESIAN_POINT('Ctrl Pts',(180.615481219117,617.494837194308,-35.0997367396894)) ;
#57768 = CARTESIAN_POINT('Ctrl Pts',(180.571650207537,617.492156157517,-35.0837284404162)) ;
#57769 = CARTESIAN_POINT('Ctrl Pts',(180.499593955378,617.487926256182,-35.0601597089916)) ;
#57770 = CARTESIAN_POINT('Ctrl Pts',(180.471689702302,617.486332214729,-35.0516855779554)) ;
#57771 = CARTESIAN_POINT('Ctrl Pts',(180.401718114024,617.482444319193,-35.0320531077093)) ;
#57772 = CARTESIAN_POINT('Ctrl Pts',(180.359460892321,617.480188632512,-35.021631990952)) ;
#57773 = CARTESIAN_POINT('Ctrl Pts',(180.258835714518,617.474966558407,-35.0001823398716)) ;
#57774 = CARTESIAN_POINT('Ctrl Pts',(180.200257315445,617.472042845602,-34.9903265749881)) ;
#57775 = CARTESIAN_POINT('Ctrl Pts',(179.973804732676,617.460923544124,-34.9622519189994)) ;
#57776 = CARTESIAN_POINT('Ctrl Pts',(179.804369589251,617.45292613096,-34.9622063400165)) ;
#57777 = CARTESIAN_POINT('Ctrl Pts',(179.583141569119,617.441467885864,-34.9895106669195)) ;
#57778 = CARTESIAN_POINT('Ctrl Pts',(179.529732889551,617.438628030699,-34.9982554623742)) ;
#57779 = CARTESIAN_POINT('Ctrl Pts',(179.425547790386,617.43291024879,-35.0195676161912)) ;
#57780 = CARTESIAN_POINT('Ctrl Pts',(179.374782905162,617.430039126328,-35.0319860777773)) ;
#57781 = CARTESIAN_POINT('Ctrl Pts',(179.225930602873,617.421349339453,-35.074474157384)) ;
#57782 = CARTESIAN_POINT('Ctrl Pts',(179.129569871467,617.415359318058,-35.1099640084541)) ;
#57783 = CARTESIAN_POINT('Ctrl Pts',(178.913668042379,617.401211382308,-35.208379310482)) ;
#57784 = CARTESIAN_POINT('Ctrl Pts',(178.796860832817,617.392988049764,-35.2761886918068)) ;
#57785 = CARTESIAN_POINT('Ctrl Pts',(178.652736433403,617.382655276666,-35.3800101413563)) ;
#57786 = CARTESIAN_POINT('Ctrl Pts',(178.618731176535,617.380204483273,-35.4061607562826)) ;
#57787 = CARTESIAN_POINT('Ctrl Pts',(178.562969642741,617.376198015675,-35.4518902364823)) ;
#57788 = CARTESIAN_POINT('Ctrl Pts',(178.540772050863,617.374608824275,-35.4709004560454)) ;
#57789 = CARTESIAN_POINT('Ctrl Pts',(178.48346343048,617.370514785968,-35.5221393584425)) ;
#57790 = CARTESIAN_POINT('Ctrl Pts',(178.449055899489,617.368061368419,-35.555125866284)) ;
#57791 = CARTESIAN_POINT('Ctrl Pts',(178.367703064376,617.362181236546,-35.6387397730613)) ;
#57792 = CARTESIAN_POINT('Ctrl Pts',(178.322101522062,617.358813994491,-35.6905935922773)) ;
#57793 = CARTESIAN_POINT('Ctrl Pts',(178.184923953435,617.348112886578,-35.863401454723)) ;
#57794 = CARTESIAN_POINT('Ctrl Pts',(178.104095651772,617.340851873848,-35.9922153202804)) ;
#57795 = CARTESIAN_POINT('Ctrl Pts',(178.014722026189,617.330280878681,-36.1773173992612)) ;
#57796 = CARTESIAN_POINT('Ctrl Pts',(177.993193309615,617.32744851166,-36.2267899102247)) ;
#57797 = CARTESIAN_POINT('Ctrl Pts',(177.954682671024,617.321736369837,-36.3257599657668)) ;
#57798 = CARTESIAN_POINT('Ctrl Pts',(177.937595561359,617.318862922739,-36.3751725948307)) ;
#57799 = CARTESIAN_POINT('Ctrl Pts',(177.89237840864,617.310122572018,-36.5240923650791)) ;
#57800 = CARTESIAN_POINT('Ctrl Pts',(177.869855803236,617.304080325146,-36.6251178418996)) ;
#57801 = CARTESIAN_POINT('Ctrl Pts',(177.835704709839,617.289874665742,-36.8607182836646)) ;
#57802 = CARTESIAN_POINT('Ctrl Pts',(177.829537230187,617.281649080268,-36.9956152099634)) ;
#57803 = CARTESIAN_POINT('Ctrl Pts',(177.83885503347,617.271335960438,-37.1726698259194)) ;
#57804 = CARTESIAN_POINT('Ctrl Pts',(177.842414513726,617.268902649459,-37.215117567384)) ;
#57805 = CARTESIAN_POINT('Ctrl Pts',(177.850628220982,617.264917443303,-37.2863818727768)) ;
#57806 = CARTESIAN_POINT('Ctrl Pts',(177.854580792064,617.263332645549,-37.3152600224801)) ;
#57807 = CARTESIAN_POINT('Ctrl Pts',(177.866599212484,617.259247174458,-37.3910312637793)) ;
#57808 = CARTESIAN_POINT('Ctrl Pts',(177.87568104503,617.256797951674,-37.4377437402562)) ;
#57809 = CARTESIAN_POINT('Ctrl Pts',(177.901856227057,617.250930052497,-37.5511923359043)) ;
#57810 = CARTESIAN_POINT('Ctrl Pts',(177.920698726028,617.247570693924,-37.6174656764953)) ;
#57811 = CARTESIAN_POINT('Ctrl Pts',(177.991623658939,617.236871778689,-37.8263922486861)) ;
#57812 = CARTESIAN_POINT('Ctrl Pts',(178.056181857435,617.229606466954,-37.9642533268478)) ;
#57813 = CARTESIAN_POINT('Ctrl Pts',(178.163348689015,617.21903941333,-38.1395864694115)) ;
#57814 = CARTESIAN_POINT('Ctrl Pts',(178.193152007248,617.216218448627,-38.1843067631357)) ;
#57815 = CARTESIAN_POINT('Ctrl Pts',(178.25514324928,617.210536265199,-38.2698580442139)) ;
#57816 = CARTESIAN_POINT('Ctrl Pts',(178.287195954441,617.207681646063,-38.3107371694879)) ;
#57817 = CARTESIAN_POINT('Ctrl Pts',(178.385731225683,617.199121661689,-38.4270455827215)) ;
#57818 = CARTESIAN_POINT('Ctrl Pts',(178.456233181178,617.193252179432,-38.4988552214778)) ;
#57819 = CARTESIAN_POINT('Ctrl Pts',(178.634009548446,617.17912993173,-38.6551768238592)) ;
#57820 = CARTESIAN_POINT('Ctrl Pts',(178.745013702691,617.170795664895,-38.7347415664399)) ;
#57821 = CARTESIAN_POINT('Ctrl Pts',(178.90137574635,617.160263973947,-38.8247921923812)) ;
#57822 = CARTESIAN_POINT('Ctrl Pts',(178.940380988712,617.157729746914,-38.8456100819122)) ;
#57823 = CARTESIAN_POINT('Ctrl Pts',(179.006275570121,617.153637511541,-38.8780925730419)) ;
#57824 = CARTESIAN_POINT('Ctrl Pts',(179.03279211868,617.152042008275,-38.8904670711412)) ;
#57825 = CARTESIAN_POINT('Ctrl Pts',(179.101975382736,617.148004095038,-38.9209706044151)) ;
#57826 = CARTESIAN_POINT('Ctrl Pts',(179.145005717671,617.145608388341,-38.9382293992682)) ;
#57827 = CARTESIAN_POINT('Ctrl Pts',(179.250361721806,617.139936310134,-38.976401472423)) ;
#57828 = CARTESIAN_POINT('Ctrl Pts',(179.313178811052,617.136712612141,-38.9958089206235)) ;
#57829 = CARTESIAN_POINT('Ctrl Pts',(179.4980724366,617.127415336166,-39.0433520007103)) ;
#57830 = CARTESIAN_POINT('Ctrl Pts',(179.621914097063,617.121407885486,-39.0633822627132)) ;
#57831 = CARTESIAN_POINT('Ctrl Pts',(179.79380202668,617.112726932359,-39.0752660378272)) ;
#57832 = CARTESIAN_POINT('Ctrl Pts',(179.84089165485,617.110316209617,-39.0768978504434)) ;
#57833 = CARTESIAN_POINT('Ctrl Pts',(179.887993154238,617.107857237813,-39.0769101022477)) ;
#57834 = CARTESIAN_POINT('Ctrl Pts',(179.887994300553,617.107857177969,-39.0769101025456)) ;
#57835 = CARTESIAN_POINT('Ctrl Pts',(179.931748483178,617.105572954829,-39.076921459253)) ;
#57836 = CARTESIAN_POINT('Ctrl Pts',(179.97548999554,617.10324833753,-39.075535261176)) ;
#57837 = CARTESIAN_POINT('Ctrl Pts',(180.071561238632,617.098035449014,-39.0694154273536)) ;
#57838 = CARTESIAN_POINT('Ctrl Pts',(180.12381888014,617.095129323125,-39.0640692522285)) ;
#57839 = CARTESIAN_POINT('Ctrl Pts',(180.342482870469,617.082651282919,-39.0331936076929)) ;
#57840 = CARTESIAN_POINT('Ctrl Pts',(180.505609754287,617.072491440771,-38.9892704948936)) ;
#57841 = CARTESIAN_POINT('Ctrl Pts',(180.742998106722,617.057100438195,-38.8928847970312)) ;
#57842 = CARTESIAN_POINT('Ctrl Pts',(180.822274454612,617.05186350609,-38.8546038648334)) ;
#57843 = CARTESIAN_POINT('Ctrl Pts',(180.926988113091,617.045023143873,-38.7954737114887)) ;
#57844 = CARTESIAN_POINT('Ctrl Pts',(180.954741046925,617.043218570973,-38.7789272071751)) ;
#57845 = CARTESIAN_POINT('Ctrl Pts',(181.010632278967,617.039619800362,-38.7437916482847)) ;
#57846 = CARTESIAN_POINT('Ctrl Pts',(181.038725918926,617.037828987409,-38.7251510622714)) ;
#57847 = CARTESIAN_POINT('Ctrl Pts',(181.170747514585,617.029437403796,-38.6327942940199)) ;
#57848 = CARTESIAN_POINT('Ctrl Pts',(181.268137532102,617.023307596862,-38.550202539998)) ;
#57849 = CARTESIAN_POINT('Ctrl Pts',(181.442290554182,617.011209674755,-38.3721984430523)) ;
#57850 = CARTESIAN_POINT('Ctrl Pts',(181.51943714825,617.005266341215,-38.2779122576196)) ;
#57851 = CARTESIAN_POINT('Ctrl Pts',(181.618062377617,616.996214627546,-38.1328384535756)) ;
#57852 = CARTESIAN_POINT('Ctrl Pts',(181.646569915149,616.993378284313,-38.0871405969377)) ;
#57853 = CARTESIAN_POINT('Ctrl Pts',(181.699819310156,616.987582234548,-37.9938057004965)) ;
#57854 = CARTESIAN_POINT('Ctrl Pts',(181.7245548971,616.984625351876,-37.9462141191694)) ;
#57855 = CARTESIAN_POINT('Ctrl Pts',(181.7956346867,616.975227139334,-37.7953057049953)) ;
#57856 = CARTESIAN_POINT('Ctrl Pts',(181.835318675884,616.968568838972,-37.6891010116894)) ;
#57857 = CARTESIAN_POINT('Ctrl Pts',(181.891898060409,616.95609510919,-37.488594272575)) ;
#57858 = CARTESIAN_POINT('Ctrl Pts',(181.911348701779,616.950333216952,-37.3953211495107)) ;
#57859 = CARTESIAN_POINT('Ctrl Pts',(181.931962597854,616.941354485208,-37.2448434608005)) ;
#57860 = CARTESIAN_POINT('Ctrl Pts',(181.937331067427,616.938055335606,-37.1883522907547)) ;
#57861 = CARTESIAN_POINT('Ctrl Pts',(181.941925447787,616.933207546444,-37.1022991223444)) ;
#57862 = CARTESIAN_POINT('Ctrl Pts',(181.942863276539,616.931580674787,-37.0728577866721)) ;
#57863 = CARTESIAN_POINT('Ctrl Pts',(181.94352433511,616.928130907502,-37.0089203794651)) ;
#57864 = CARTESIAN_POINT('Ctrl Pts',(181.943012734418,616.926321035078,-36.9744314866176)) ;
#57865 = CARTESIAN_POINT('Ctrl Pts',(181.937111839773,616.918742220634,-36.8270282926864)) ;
#57866 = CARTESIAN_POINT('Ctrl Pts',(181.923278371657,616.913349797256,-36.7146404094036)) ;
#57867 = CARTESIAN_POINT('Ctrl Pts',(181.87195147715,616.901331556798,-36.4677386305984)) ;
#57868 = CARTESIAN_POINT('Ctrl Pts',(181.829877489038,616.894721323105,-36.3347662570377)) ;
#57869 = CARTESIAN_POINT('Ctrl Pts',(181.752604770617,616.884830986749,-36.1559531550421)) ;
#57870 = CARTESIAN_POINT('Ctrl Pts',(181.728448913669,616.881939946307,-36.1057612086665)) ;
#57871 = CARTESIAN_POINT('Ctrl Pts',(181.678827079011,616.876315230185,-36.0125475253731)) ;
#57872 = CARTESIAN_POINT('Ctrl Pts',(181.653771474374,616.873598235882,-35.9693528025679)) ;
#57873 = CARTESIAN_POINT('Ctrl Pts',(181.593143507417,616.867275496381,-35.8730915803318)) ;
#57874 = CARTESIAN_POINT('Ctrl Pts',(181.556626176123,616.86363668831,-35.8206954742303)) ;
#57875 = CARTESIAN_POINT('Ctrl Pts',(181.517739074368,616.85992786049,-35.7700948311641)) ;
#57876 = CARTESIAN_POINT('Ctrl Pts',(181.517739097406,616.918146095397,-35.7700948611415)) ;
#57877 = CARTESIAN_POINT('Ctrl Pts',(181.550328721279,616.921316298233,-35.8125011067506)) ;
#57878 = CARTESIAN_POINT('Ctrl Pts',(181.581246855276,616.924445264569,-35.8561583268598)) ;
#57879 = CARTESIAN_POINT('Ctrl Pts',(181.625374003287,616.929048745201,-35.9239288915403)) ;
#57880 = CARTESIAN_POINT('Ctrl Pts',(181.639855178756,616.930584660759,-35.9471721511206)) ;
#57881 = CARTESIAN_POINT('Ctrl Pts',(181.669022937296,616.933721059168,-35.9961430811549)) ;
#57882 = CARTESIAN_POINT('Ctrl Pts',(181.683625433427,616.935313808053,-36.0219109388662)) ;
#57883 = CARTESIAN_POINT('Ctrl Pts',(181.725712386179,616.939994159661,-36.1000706894596)) ;
#57884 = CARTESIAN_POINT('Ctrl Pts',(181.751498255502,616.942989324102,-36.1533457943525)) ;
#57885 = CARTESIAN_POINT('Ctrl Pts',(181.828273701453,616.952592025105,-36.3311623217492)) ;
#57886 = CARTESIAN_POINT('Ctrl Pts',(181.869341509308,616.958937602289,-36.4596016858192)) ;
#57887 = CARTESIAN_POINT('Ctrl Pts',(181.911581610771,616.968819666931,-36.6564866040734)) ;
#57888 = CARTESIAN_POINT('Ctrl Pts',(181.922404077584,616.972152671785,-36.7224766318149)) ;
#57889 = CARTESIAN_POINT('Ctrl Pts',(181.936140540446,616.978357020819,-36.8426826702027)) ;
#57890 = CARTESIAN_POINT('Ctrl Pts',(181.940159278133,616.981193203918,-36.8967103196874)) ;
#57891 = CARTESIAN_POINT('Ctrl Pts',(181.943812903979,616.986839931187,-37.0018948196659)) ;
#57892 = CARTESIAN_POINT('Ctrl Pts',(181.943681213294,616.989640781737,-37.0530037165148)) ;
#57893 = CARTESIAN_POINT('Ctrl Pts',(181.937965970889,616.997669395724,-37.1962917900183)) ;
#57894 = CARTESIAN_POINT('Ctrl Pts',(181.928075488364,617.003027668162,-37.2881684388466)) ;
#57895 = CARTESIAN_POINT('Ctrl Pts',(181.891815335774,617.015414513837,-37.4937526547962)) ;
#57896 = CARTESIAN_POINT('Ctrl Pts',(181.861872978786,617.022495958312,-37.6065127691157)) ;
#57897 = CARTESIAN_POINT('Ctrl Pts',(181.807352682194,617.032082323236,-37.7584551703357)) ;
#57898 = CARTESIAN_POINT('Ctrl Pts',(181.790778012824,617.034723677821,-37.8002757302703)) ;
#57899 = CARTESIAN_POINT('Ctrl Pts',(181.75835588775,617.039398589554,-37.8748381738567)) ;
#57900 = CARTESIAN_POINT('Ctrl Pts',(181.74298624706,617.041450542541,-37.9077679224054)) ;
#57901 = CARTESIAN_POINT('Ctrl Pts',(181.713350732643,617.045101232571,-37.9671032943191)) ;
#57902 = CARTESIAN_POINT('Ctrl Pts',(181.699365616808,617.046713767382,-37.9936346613234)) ;
#57903 = CARTESIAN_POINT('Ctrl Pts',(181.655548903705,617.051471129102,-38.0725237332439)) ;
#57904 = CARTESIAN_POINT('Ctrl Pts',(181.623988462496,617.054520402284,-38.1238882091899)) ;
#57905 = CARTESIAN_POINT('Ctrl Pts',(181.514803487523,617.064177585205,-38.2852228144751)) ;
#57906 = CARTESIAN_POINT('Ctrl Pts',(181.428630086657,617.070534384318,-38.3889767072537)) ;
#57907 = CARTESIAN_POINT('Ctrl Pts',(181.285202348625,617.080453946922,-38.5307357513301)) ;
#57908 = CARTESIAN_POINT('Ctrl Pts',(181.235196313883,617.083809486818,-38.575538116578)) ;
#57909 = CARTESIAN_POINT('Ctrl Pts',(181.141472499279,617.090016628892,-38.6515769026892)) ;
#57910 = CARTESIAN_POINT('Ctrl Pts',(181.098552023683,617.092830864496,-38.6836986141816)) ;
#57911 = CARTESIAN_POINT('Ctrl Pts',(181.011669320262,617.098505144396,-38.7435685195111)) ;
#57912 = CARTESIAN_POINT('Ctrl Pts',(180.967812709095,617.101358936485,-38.7713991426981)) ;
#57913 = CARTESIAN_POINT('Ctrl Pts',(180.764235053408,617.114584965928,-38.8900137399832)) ;
#57914 = CARTESIAN_POINT('Ctrl Pts',(180.593854302493,617.12569994237,-38.9607759619112)) ;
#57915 = CARTESIAN_POINT('Ctrl Pts',(180.339716258798,617.141442511417,-39.0283307669638)) ;
#57916 = CARTESIAN_POINT('Ctrl Pts',(180.261920739583,617.146139457245,-39.0442559505548)) ;
#57917 = CARTESIAN_POINT('Ctrl Pts',(180.152085707938,617.152437967904,-39.0601826164286)) ;
#57918 = CARTESIAN_POINT('Ctrl Pts',(180.120674440741,617.154201376314,-39.06399918876)) ;
#57919 = CARTESIAN_POINT('Ctrl Pts',(180.055803867352,617.157748126157,-39.0703645630655)) ;
#57920 = CARTESIAN_POINT('Ctrl Pts',(180.022345689361,617.159526796168,-39.0728224026525)) ;
#57921 = CARTESIAN_POINT('Ctrl Pts',(179.860120920872,617.167969660526,-39.0807516487854)) ;
#57922 = CARTESIAN_POINT('Ctrl Pts',(179.731080963116,617.174146901798,-39.0749201346289)) ;
#57923 = CARTESIAN_POINT('Ctrl Pts',(179.488784219288,617.185993759301,-39.0409726421341)) ;
#57924 = CARTESIAN_POINT('Ctrl Pts',(179.375709988295,617.19163197621,-39.0152516759678)) ;
#57925 = CARTESIAN_POINT('Ctrl Pts',(179.212980670018,617.200381079083,-38.963464160089)) ;
#57926 = CARTESIAN_POINT('Ctrl Pts',(179.16124581863,617.203259535436,-38.9446807292251)) ;
#57927 = CARTESIAN_POINT('Ctrl Pts',(179.062983908672,617.208951568143,-38.9044704939683)) ;
#57928 = CARTESIAN_POINT('Ctrl Pts',(179.016381441385,617.211753400817,-38.8833358608337)) ;
#57929 = CARTESIAN_POINT('Ctrl Pts',(178.890154857852,617.219645758608,-38.8203086692027)) ;
#57930 = CARTESIAN_POINT('Ctrl Pts',(178.812424763463,617.224856612693,-38.7748967759229)) ;
#57931 = CARTESIAN_POINT('Ctrl Pts',(178.638774692763,617.237274261633,-38.6575307720814)) ;
#57932 = CARTESIAN_POINT('Ctrl Pts',(178.545672381528,617.244554470164,-38.581986293298)) ;
#57933 = CARTESIAN_POINT('Ctrl Pts',(178.42699329747,617.254367707815,-38.4671457367803)) ;
#57934 = CARTESIAN_POINT('Ctrl Pts',(178.39536794152,617.25704084133,-38.4344421826375)) ;
#57935 = CARTESIAN_POINT('Ctrl Pts',(178.340288451284,617.261764274289,-38.3735644535104)) ;
#57936 = CARTESIAN_POINT('Ctrl Pts',(178.316452712281,617.263833496823,-38.3457609079863)) ;
#57937 = CARTESIAN_POINT('Ctrl Pts',(178.274480773444,617.267500663887,-38.294067585386)) ;
#57938 = CARTESIAN_POINT('Ctrl Pts',(178.256101949607,617.269113165125,-38.2703917847557)) ;
#57939 = CARTESIAN_POINT('Ctrl Pts',(178.202693929471,617.27384209283,-38.198392916288)) ;
#57940 = CARTESIAN_POINT('Ctrl Pts',(178.16924287227,617.276865347643,-38.1489342417559)) ;
#57941 = CARTESIAN_POINT('Ctrl Pts',(178.067393037271,617.286517747301,-37.9832239347606)) ;
#57942 = CARTESIAN_POINT('Ctrl Pts',(178.00827069366,617.292890850926,-37.8616905795828)) ;
#57943 = CARTESIAN_POINT('Ctrl Pts',(177.938178140203,617.302830009259,-37.6722696361415)) ;
#57944 = CARTESIAN_POINT('Ctrl Pts',(177.917979420572,617.306188529697,-37.6082013287826)) ;
#57945 = CARTESIAN_POINT('Ctrl Pts',(177.887361106619,617.312399699006,-37.4914178531219)) ;
#57946 = CARTESIAN_POINT('Ctrl Pts',(177.875803074765,617.315214936164,-37.4390647065857)) ;
#57947 = CARTESIAN_POINT('Ctrl Pts',(177.85709408481,617.32089339154,-37.3351722068065)) ;
#57948 = CARTESIAN_POINT('Ctrl Pts',(177.849827592242,617.323750457439,-37.2836945667341)) ;
#57949 = CARTESIAN_POINT('Ctrl Pts',(177.825750344344,617.336988634995,-37.0491628894965)) ;
#57950 = CARTESIAN_POINT('Ctrl Pts',(177.831600636578,617.348113475758,-36.8646577856199)) ;
#57951 = CARTESIAN_POINT('Ctrl Pts',(177.875001283232,617.363881152821,-36.6049837039085)) ;
#57952 = CARTESIAN_POINT('Ctrl Pts',(177.892659450038,617.368592317796,-36.5273502126785)) ;
#57953 = CARTESIAN_POINT('Ctrl Pts',(177.923569987055,617.374904156855,-36.4205460128189)) ;
#57954 = CARTESIAN_POINT('Ctrl Pts',(177.933064938416,617.376667845483,-36.390365775814)) ;
#57955 = CARTESIAN_POINT('Ctrl Pts',(177.954013658771,617.380208142601,-36.3287847580082)) ;
#57956 = CARTESIAN_POINT('Ctrl Pts',(177.965543906333,617.381980372035,-36.2974204563991)) ;
#57957 = CARTESIAN_POINT('Ctrl Pts',(178.025788869192,617.390496766316,-36.1451209349666)) ;
#57958 = CARTESIAN_POINT('Ctrl Pts',(178.085176990798,617.396739705751,-36.0287180031394)) ;
#57959 = CARTESIAN_POINT('Ctrl Pts',(178.221447380879,617.409025717228,-35.8146595134732)) ;
#57960 = CARTESIAN_POINT('Ctrl Pts',(178.296924316347,617.415041127856,-35.716782978665)) ;
#57961 = CARTESIAN_POINT('Ctrl Pts',(178.416625919415,617.424129027223,-35.5874835335559)) ;
#57962 = CARTESIAN_POINT('Ctrl Pts',(178.454016748612,617.426912338358,-35.5500971448259)) ;
#57963 = CARTESIAN_POINT('Ctrl Pts',(178.5314303225,617.432598339232,-35.4784456753361)) ;
#57964 = CARTESIAN_POINT('Ctrl Pts',(178.571411863573,617.435498321972,-35.4441953811801)) ;
#57965 = CARTESIAN_POINT('Ctrl Pts',(178.742559221263,617.44778745189,-35.3086213109438)) ;
#57966 = CARTESIAN_POINT('Ctrl Pts',(178.884410445348,617.457750667779,-35.2218295169491)) ;
#57967 = CARTESIAN_POINT('Ctrl Pts',(179.093063813471,617.471527796875,-35.1265616067474)) ;
#57968 = CARTESIAN_POINT('Ctrl Pts',(179.152221259439,617.475336158369,-35.102808649532)) ;
#57969 = CARTESIAN_POINT('Ctrl Pts',(179.255237150789,617.481707829895,-35.0669109214474)) ;
#57970 = CARTESIAN_POINT('Ctrl Pts',(179.298571368106,617.484311967162,-35.0534020130791)) ;
#57971 = CARTESIAN_POINT('Ctrl Pts',(179.370234483952,617.488455684473,-35.0336410680502)) ;
#57972 = CARTESIAN_POINT('Ctrl Pts',(179.3983069954,617.490036948082,-35.0265349636113)) ;
#57973 = CARTESIAN_POINT('Ctrl Pts',(179.469271466407,617.493930359723,-35.010159584666)) ;
#57974 = CARTESIAN_POINT('Ctrl Pts',(179.51232564288,617.49620276916,-35.0016664927409)) ;
#57975 = CARTESIAN_POINT('Ctrl Pts',(179.689278683189,617.50529705332,-34.9726131001116)) ;
#57976 = CARTESIAN_POINT('Ctrl Pts',(179.824787120053,617.511711385577,-34.9639361846214)) ;
#57977 = CARTESIAN_POINT('Ctrl Pts',(180.060497655407,617.523197141869,-34.9721598209715)) ;
#57978 = CARTESIAN_POINT('Ctrl Pts',(180.160424619279,617.528167077317,-34.9830073038409)) ;
#57979 = CARTESIAN_POINT('Ctrl Pts',(180.310169803791,617.536049256118,-35.0104678971105)) ;
#57980 = CARTESIAN_POINT('Ctrl Pts',(180.360811777393,617.538790535241,-35.0217514721223)) ;
#57981 = CARTESIAN_POINT('Ctrl Pts',(180.462961472524,617.544502227499,-35.0486067082229)) ;
#57982 = CARTESIAN_POINT('Ctrl Pts',(180.51439266739,617.547475161923,-35.0643093872556)) ;
#57983 = CARTESIAN_POINT('Ctrl Pts',(180.725161334104,617.560086329988,-35.1378139503805)) ;
#57984 = CARTESIAN_POINT('Ctrl Pts',(180.877638419302,617.570319822621,-35.2131939400467)) ;
#57985 = CARTESIAN_POINT('Ctrl Pts',(181.089730278994,617.585552146686,-35.3529496062667)) ;
#57986 = CARTESIAN_POINT('Ctrl Pts',(181.157423117762,617.590576635154,-35.403809668987)) ;
#57987 = CARTESIAN_POINT('Ctrl Pts',(181.246109728965,617.597199768885,-35.4794386347682)) ;
#57988 = CARTESIAN_POINT('Ctrl Pts',(181.269941834904,617.598983521114,-35.5007417472021)) ;
#57989 = CARTESIAN_POINT('Ctrl Pts',(181.317382422261,617.602524754099,-35.5451824379964)) ;
#57990 = CARTESIAN_POINT('Ctrl Pts',(181.340948958807,617.604279378033,-35.568350759617)) ;
#57991 = CARTESIAN_POINT('Ctrl Pts',(181.418564822408,617.610084953589,-35.6484273383273)) ;
#57992 = CARTESIAN_POINT('Ctrl Pts',(181.469913375323,617.613972930346,-35.7078631122422)) ;
#57993 = CARTESIAN_POINT('Ctrl Pts',(181.517739089197,617.617803659368,-35.7700948504595)) ;
#57994 = CARTESIAN_POINT('Origin',(179.888527625422,620.256490441073,-37.0221601717597)) ;
#57995 = CARTESIAN_POINT('',(181.51728805297,618.315593727817,-35.7705118777721)) ;
#57996 = CARTESIAN_POINT('',(181.517739089185,618.256600448669,-35.770094850444)) ;
#57997 = CARTESIAN_POINT('',(181.517739089189,620.256490441073,-35.7700948504488)) ;
#57998 = CARTESIAN_POINT('',(179.888164616977,618.564640754081,-39.0769101396937)) ;
#57999 = CARTESIAN_POINT('Ctrl Pts',(179.888125504502,618.563693523877,-39.0763631698524)) ;
#58000 = CARTESIAN_POINT('Ctrl Pts',(179.959056146154,618.559621057654,-39.0762415227883)) ;
#58001 = CARTESIAN_POINT('Ctrl Pts',(180.030027539004,618.555603825935,-39.0724738662884)) ;
#58002 = CARTESIAN_POINT('Ctrl Pts',(180.100642834529,618.551671173244,-39.0650869459768)) ;
#58003 = CARTESIAN_POINT('Ctrl Pts',(180.171240300517,618.547739513502,-39.0577018907762)) ;
#58004 = CARTESIAN_POINT('Ctrl Pts',(180.241481827655,618.543892420134,-39.0466994145418)) ;
#58005 = CARTESIAN_POINT('Ctrl Pts',(180.310975081654,618.540134620763,-39.0321407020133)) ;
#58006 = CARTESIAN_POINT('Ctrl Pts',(180.380474576421,618.536376483926,-39.0175806820547)) ;
#58007 = CARTESIAN_POINT('Ctrl Pts',(180.449225593483,618.532707584397,-38.9994636931089)) ;
#58008 = CARTESIAN_POINT('Ctrl Pts',(180.516840591467,618.529108370222,-38.9778860130638)) ;
#58009 = CARTESIAN_POINT('Ctrl Pts',(180.584533976828,618.525504983408,-38.9562833175963)) ;
#58010 = CARTESIAN_POINT('Ctrl Pts',(180.651088576284,618.521971257736,-38.9312116960932)) ;
#58011 = CARTESIAN_POINT('Ctrl Pts',(180.71612189975,618.51846514406,-38.9028051720917)) ;
#58012 = CARTESIAN_POINT('Ctrl Pts',(180.781195676329,618.514956849453,-38.8743809781904)) ;
#58013 = CARTESIAN_POINT('Ctrl Pts',(180.844746048432,618.511475855401,-38.8426174166942)) ;
#58014 = CARTESIAN_POINT('Ctrl Pts',(180.90639890197,618.507961534938,-38.8076901049773)) ;
#58015 = CARTESIAN_POINT('Ctrl Pts',(180.964471862557,618.504651274634,-38.7747908589512)) ;
#58016 = CARTESIAN_POINT('Ctrl Pts',(181.020861449749,618.501310953758,-38.7390842018661)) ;
#58017 = CARTESIAN_POINT('Ctrl Pts',(181.075265040859,618.497880064485,-38.7007560774233)) ;
#58018 = CARTESIAN_POINT('Ctrl Pts',(181.078727888333,618.497661684668,-38.6983164508069)) ;
#58019 = CARTESIAN_POINT('Ctrl Pts',(181.082182707133,618.497442937917,-38.6958662022202)) ;
#58020 = CARTESIAN_POINT('Ctrl Pts',(181.085629426356,618.497223808628,-38.6934053789544)) ;
#58021 = CARTESIAN_POINT('Ctrl Pts',(181.122314421018,618.494891516302,-38.6672137217535)) ;
#58022 = CARTESIAN_POINT('Ctrl Pts',(181.158079903752,618.492515656591,-38.6398252694906)) ;
#58023 = CARTESIAN_POINT('Ctrl Pts',(181.192836848114,618.490076781835,-38.6113088574816)) ;
#58024 = CARTESIAN_POINT('Ctrl Pts',(181.192864076843,618.49007487121,-38.6112865176113)) ;
#58025 = CARTESIAN_POINT('Ctrl Pts',(181.192891304952,618.490072960548,-38.6112641770488)) ;
#58026 = CARTESIAN_POINT('Ctrl Pts',(181.192918532444,618.490071049846,-38.6112418357942)) ;
#58027 = CARTESIAN_POINT('Ctrl Pts',(181.242673139758,618.486579497818,-38.5704161744067)) ;
#58028 = CARTESIAN_POINT('Ctrl Pts',(181.290541683293,618.482949500952,-38.52712164623)) ;
#58029 = CARTESIAN_POINT('Ctrl Pts',(181.336294377515,618.47924615687,-38.4815793682111)) ;
#58030 = CARTESIAN_POINT('Ctrl Pts',(181.340932471314,618.47887073729,-38.4769626049605)) ;
#58031 = CARTESIAN_POINT('Ctrl Pts',(181.345548813078,618.478494563957,-38.4723227860285)) ;
#58032 = CARTESIAN_POINT('Ctrl Pts',(181.350143158393,618.478117704687,-38.4676601711489)) ;
#58033 = CARTESIAN_POINT('Ctrl Pts',(181.39998204525,618.47402958217,-38.4170807045429)) ;
#58034 = CARTESIAN_POINT('Ctrl Pts',(181.447234070826,618.4698613568,-38.3638129387118)) ;
#58035 = CARTESIAN_POINT('Ctrl Pts',(181.491635364602,618.465687402768,-38.3081764046326)) ;
#58036 = CARTESIAN_POINT('Ctrl Pts',(181.535981829134,618.461518602973,-38.252608573711)) ;
#58037 = CARTESIAN_POINT('Ctrl Pts',(181.577484930695,618.45734444223,-38.1946780085854)) ;
#58038 = CARTESIAN_POINT('Ctrl Pts',(181.615918052772,618.453219658054,-38.1347204485888)) ;
#58039 = CARTESIAN_POINT('Ctrl Pts',(181.654325510364,618.449097628284,-38.0748029264502)) ;
#58040 = CARTESIAN_POINT('Ctrl Pts',(181.689667249886,618.445025077976,-38.0128611802261)) ;
#58041 = CARTESIAN_POINT('Ctrl Pts',(181.721749657168,618.441033439463,-37.9492458730777)) ;
#58042 = CARTESIAN_POINT('Ctrl Pts',(181.753821421396,618.437043125141,-37.8856516697398)) ;
#58043 = CARTESIAN_POINT('Ctrl Pts',(181.78263603063,618.433133709202,-37.8203850336934)) ;
#58044 = CARTESIAN_POINT('Ctrl Pts',(181.80803130034,618.42931187499,-37.7538112969984)) ;
#58045 = CARTESIAN_POINT('Ctrl Pts',(181.833426678707,618.425490024426,-37.6872372754576)) ;
#58046 = CARTESIAN_POINT('Ctrl Pts',(181.85540257914,618.421755691541,-37.619356141093)) ;
#58047 = CARTESIAN_POINT('Ctrl Pts',(181.873828778154,618.418091025479,-37.550548137017)) ;
#58048 = CARTESIAN_POINT('Ctrl Pts',(181.892273434705,618.414422688518,-37.4816712079157)) ;
#58049 = CARTESIAN_POINT('Ctrl Pts',(181.907161034768,618.410823979583,-37.4118655412063)) ;
#58050 = CARTESIAN_POINT('Ctrl Pts',(181.91839560142,618.407254203748,-37.3415275613066)) ;
#58051 = CARTESIAN_POINT('Ctrl Pts',(181.929636220517,618.403682504752,-37.2711516879324)) ;
#58052 = CARTESIAN_POINT('Ctrl Pts',(181.937219477996,618.400139432256,-37.2002429455114)) ;
#58053 = CARTESIAN_POINT('Ctrl Pts',(181.941088598904,618.39656524962,-37.1292134404523)) ;
#58054 = CARTESIAN_POINT('Ctrl Pts',(181.944752203609,618.393180916943,-37.0619568116149)) ;
#58055 = CARTESIAN_POINT('Ctrl Pts',(181.94508548051,618.389768200429,-36.9945915705661)) ;
#58056 = CARTESIAN_POINT('Ctrl Pts',(181.942079051817,618.386265885841,-36.92748080267)) ;
#58057 = CARTESIAN_POINT('Ctrl Pts',(181.94190493884,618.386063054349,-36.9235941794562)) ;
#58058 = CARTESIAN_POINT('Ctrl Pts',(181.94171963135,618.385859922347,-36.9197083968835)) ;
#58059 = CARTESIAN_POINT('Ctrl Pts',(181.941523129918,618.385656477945,-36.915823520671)) ;
#58060 = CARTESIAN_POINT('Ctrl Pts',(181.93935010503,618.383406673734,-36.8728623442949)) ;
#58061 = CARTESIAN_POINT('Ctrl Pts',(181.935808169022,618.381118446845,-36.8300140550891)) ;
#58062 = CARTESIAN_POINT('Ctrl Pts',(181.930904882405,618.378775043707,-36.7873756177613)) ;
#58063 = CARTESIAN_POINT('Ctrl Pts',(181.930900988185,618.378773182562,-36.7873417540572)) ;
#58064 = CARTESIAN_POINT('Ctrl Pts',(181.930897093107,618.378771321383,-36.7873078904849)) ;
#58065 = CARTESIAN_POINT('Ctrl Pts',(181.93089319717,618.378769460168,-36.7872740270446)) ;
#58066 = CARTESIAN_POINT('Ctrl Pts',(181.923496304728,618.37523572605,-36.7229803128489)) ;
#58067 = CARTESIAN_POINT('Ctrl Pts',(181.912971962119,618.371567819245,-36.6589431336752)) ;
#58068 = CARTESIAN_POINT('Ctrl Pts',(181.899383298866,618.367830687328,-36.595478813972)) ;
#58069 = CARTESIAN_POINT('Ctrl Pts',(181.898055332695,618.367465472246,-36.5892766976896)) ;
#58070 = CARTESIAN_POINT('Ctrl Pts',(181.896698130639,618.367099596038,-36.5830800809786)) ;
#58071 = CARTESIAN_POINT('Ctrl Pts',(181.89531177119,618.366733119321,-36.5768892771111)) ;
#58072 = CARTESIAN_POINT('Ctrl Pts',(181.87984539817,618.362644666207,-36.5078240126944)) ;
#58073 = CARTESIAN_POINT('Ctrl Pts',(181.860746264821,618.358482213079,-36.4394783858795)) ;
#58074 = CARTESIAN_POINT('Ctrl Pts',(181.83813916127,618.35431735719,-36.3722398226686)) ;
#58075 = CARTESIAN_POINT('Ctrl Pts',(181.836937952426,618.354096061184,-36.3686671599152)) ;
#58076 = CARTESIAN_POINT('Ctrl Pts',(181.835726847168,618.353874758394,-36.3650976323868)) ;
#58077 = CARTESIAN_POINT('Ctrl Pts',(181.8345058668,618.353653459561,-36.3615313014004)) ;
#58078 = CARTESIAN_POINT('Ctrl Pts',(181.811430103808,618.349471050443,-36.2941298830263)) ;
#58079 = CARTESIAN_POINT('Ctrl Pts',(181.784824745324,618.345290261806,-36.2278660420256)) ;
#58080 = CARTESIAN_POINT('Ctrl Pts',(181.75485184391,618.341163559267,-36.1631118241443)) ;
#58081 = CARTESIAN_POINT('Ctrl Pts',(181.724898856605,618.337039598525,-36.0984006292118)) ;
#58082 = CARTESIAN_POINT('Ctrl Pts',(181.691582932313,618.332969810021,-36.0351969575839)) ;
#58083 = CARTESIAN_POINT('Ctrl Pts',(181.655096405581,618.328983264932,-35.9738533116335)) ;
#58084 = CARTESIAN_POINT('Ctrl Pts',(181.618619862224,618.324997810633,-35.9125264504166)) ;
#58085 = CARTESIAN_POINT('Ctrl Pts',(181.578974467337,618.321095586499,-35.853058600381)) ;
#58086 = CARTESIAN_POINT('Ctrl Pts',(181.536381933975,618.317280962604,-35.7957838575602)) ;
#58087 = CARTESIAN_POINT('Ctrl Pts',(181.53008148432,618.316716688918,-35.7873115595969)) ;
#58088 = CARTESIAN_POINT('Ctrl Pts',(181.523716599731,618.316154287881,-35.7788872173185)) ;
#58089 = CARTESIAN_POINT('Ctrl Pts',(181.51728805297,618.315593727817,-35.7705118777721)) ;
#58090 = CARTESIAN_POINT('',(177.90335329975,618.710565160536,-37.552330388949)) ;
#58091 = CARTESIAN_POINT('Ctrl Pts',(177.90335329975,618.710565160536,-37.552330388949)) ;
#58092 = CARTESIAN_POINT('Ctrl Pts',(177.922083606511,618.706629227194,-37.6224643249733)) ;
#58093 = CARTESIAN_POINT('Ctrl Pts',(177.944552733151,618.702693293853,-37.6916719620047)) ;
#58094 = CARTESIAN_POINT('Ctrl Pts',(177.970646133763,618.698757360511,-37.7595394137045)) ;
#58095 = CARTESIAN_POINT('Ctrl Pts',(177.996718458269,618.694824606293,-37.8273520476528)) ;
#58096 = CARTESIAN_POINT('Ctrl Pts',(178.026409071389,618.690891852074,-37.8938262197478)) ;
#58097 = CARTESIAN_POINT('Ctrl Pts',(178.059554051881,618.686959097856,-37.9585645874841)) ;
#58098 = CARTESIAN_POINT('Ctrl Pts',(178.092688887672,618.683027547338,-38.0232831407163)) ;
#58099 = CARTESIAN_POINT('Ctrl Pts',(178.129275785989,618.67909599682,-38.086266532727)) ;
#58100 = CARTESIAN_POINT('Ctrl Pts',(178.169103756104,618.675164446301,-38.1471397805177)) ;
#58101 = CARTESIAN_POINT('Ctrl Pts',(178.208927037003,618.671233358671,-38.2080058612881)) ;
#58102 = CARTESIAN_POINT('Ctrl Pts',(178.251990379354,618.667302271041,-38.2667619058341)) ;
#58103 = CARTESIAN_POINT('Ctrl Pts',(178.29803893613,618.663371183411,-38.3230611256129)) ;
#58104 = CARTESIAN_POINT('Ctrl Pts',(178.344095108192,618.659439445677,-38.3793696558808)) ;
#58105 = CARTESIAN_POINT('Ctrl Pts',(178.39313718377,618.655507707943,-38.4332201974016)) ;
#58106 = CARTESIAN_POINT('Ctrl Pts',(178.444870336052,618.651575970209,-38.484299424139)) ;
#58107 = CARTESIAN_POINT('Ctrl Pts',(178.496626691879,618.647642468997,-38.535401561121)) ;
#58108 = CARTESIAN_POINT('Ctrl Pts',(178.551076195138,618.643708967785,-38.5837295897)) ;
#58109 = CARTESIAN_POINT('Ctrl Pts',(178.607888558719,618.639775466573,-38.6290083734684)) ;
#58110 = CARTESIAN_POINT('Ctrl Pts',(178.664784842608,618.635836154995,-38.6743540407325)) ;
#58111 = CARTESIAN_POINT('Ctrl Pts',(178.724050592454,618.631896843418,-38.7166411852367)) ;
#58112 = CARTESIAN_POINT('Ctrl Pts',(178.785324331511,618.62795753184,-38.7556364637246)) ;
#58113 = CARTESIAN_POINT('Ctrl Pts',(178.846648938566,618.624014949939,-38.7946641151639)) ;
#58114 = CARTESIAN_POINT('Ctrl Pts',(178.909984453703,618.620072368038,-38.8303942316352)) ;
#58115 = CARTESIAN_POINT('Ctrl Pts',(178.974944743423,618.616129786138,-38.8626394246227)) ;
#58116 = CARTESIAN_POINT('Ctrl Pts',(179.040028692326,618.612179699091,-38.8949459999443)) ;
#58117 = CARTESIAN_POINT('Ctrl Pts',(179.106743168932,618.608229612045,-38.9237542227441)) ;
#58118 = CARTESIAN_POINT('Ctrl Pts',(179.174682422129,618.604279524998,-38.948924970129)) ;
#58119 = CARTESIAN_POINT('Ctrl Pts',(179.202984719819,618.602633988225,-38.9594106606842)) ;
#58120 = CARTESIAN_POINT('Ctrl Pts',(179.231499396579,618.600988451452,-38.9692657018397)) ;
#58121 = CARTESIAN_POINT('Ctrl Pts',(179.26019651201,618.599342914678,-38.9784826335278)) ;
#58122 = CARTESIAN_POINT('Ctrl Pts',(179.339550661574,618.594792625589,-39.0039695775893)) ;
#58123 = CARTESIAN_POINT('Ctrl Pts',(179.420542892379,618.5902423365,-39.024651836472)) ;
#58124 = CARTESIAN_POINT('Ctrl Pts',(179.50263213996,618.585692047411,-39.0403480314002)) ;
#58125 = CARTESIAN_POINT('Ctrl Pts',(179.583845704284,618.581190298321,-39.0558767878938)) ;
#58126 = CARTESIAN_POINT('Ctrl Pts',(179.666132889144,618.576688549231,-39.0665252057191)) ;
#58127 = CARTESIAN_POINT('Ctrl Pts',(179.748948669339,618.572186800141,-39.0721638979804)) ;
#58128 = CARTESIAN_POINT('Ctrl Pts',(179.795221919972,618.569671451454,-39.0753145127502)) ;
#58129 = CARTESIAN_POINT('Ctrl Pts',(179.841659828985,618.567156102768,-39.0769019237886)) ;
#58130 = CARTESIAN_POINT('Ctrl Pts',(179.888164616977,618.564640754081,-39.0769101396937)) ;
#58131 = CARTESIAN_POINT('',(177.901919214914,618.709347838499,-36.4891859383096)) ;
#58132 = CARTESIAN_POINT('Origin',(179.888527625422,618.710565160536,-37.0221601717597)) ;
#58133 = CARTESIAN_POINT('Ctrl Pts',(177.903934811095,618.708121040096,-36.4898173087268)) ;
#58134 = CARTESIAN_POINT('Ctrl Pts',(177.89961331501,618.70721870862,-36.5059279972954)) ;
#58135 = CARTESIAN_POINT('Ctrl Pts',(177.895488008535,618.706327482754,-36.522091261017)) ;
#58136 = CARTESIAN_POINT('Ctrl Pts',(177.886633355003,618.704340332833,-36.558636087596)) ;
#58137 = CARTESIAN_POINT('Ctrl Pts',(177.882017504782,618.70325007211,-36.5790434341295)) ;
#58138 = CARTESIAN_POINT('Ctrl Pts',(177.847956110036,618.694720105473,-36.7410982126199)) ;
#58139 = CARTESIAN_POINT('Ctrl Pts',(177.833231202522,618.687867576172,-36.8854382773337)) ;
#58140 = CARTESIAN_POINT('Ctrl Pts',(177.834192659606,618.67580505919,-37.1330268029234)) ;
#58141 = CARTESIAN_POINT('Ctrl Pts',(177.842319395807,618.67071454387,-37.2357312845398)) ;
#58142 = CARTESIAN_POINT('Ctrl Pts',(177.866104838432,618.662686387422,-37.3889365830538)) ;
#58143 = CARTESIAN_POINT('Ctrl Pts',(177.876067460293,618.659929360742,-37.4401581341412)) ;
#58144 = CARTESIAN_POINT('Ctrl Pts',(177.900297135361,618.654186813558,-37.5435599297601)) ;
#58145 = CARTESIAN_POINT('Ctrl Pts',(177.914696888043,618.651198863856,-37.5956666098326)) ;
#58146 = CARTESIAN_POINT('Ctrl Pts',(177.981046279874,618.638880335466,-37.8034677918017)) ;
#58147 = CARTESIAN_POINT('Ctrl Pts',(178.049501899252,618.629007724035,-37.9532323266272)) ;
#58148 = CARTESIAN_POINT('Ctrl Pts',(178.17967765215,618.614064101347,-38.1663497344923)) ;
#58149 = CARTESIAN_POINT('Ctrl Pts',(178.228871061269,618.608981376482,-38.2366067359811)) ;
#58150 = CARTESIAN_POINT('Ctrl Pts',(178.302289575914,618.602299660776,-38.328633536338)) ;
#58151 = CARTESIAN_POINT('Ctrl Pts',(178.322852354449,618.600513368516,-38.3532067691423)) ;
#58152 = CARTESIAN_POINT('Ctrl Pts',(178.36575584161,618.596972252822,-38.4021071171549)) ;
#58153 = CARTESIAN_POINT('Ctrl Pts',(178.388125183866,618.595220293271,-38.4263967150322)) ;
#58154 = CARTESIAN_POINT('Ctrl Pts',(178.505050836438,618.58646734713,-38.5473737279596)) ;
#58155 = CARTESIAN_POINT('Ctrl Pts',(178.608410297247,618.580012766468,-38.6351053656314)) ;
#58156 = CARTESIAN_POINT('Ctrl Pts',(178.787843049251,618.569455660769,-38.7592168399994)) ;
#58157 = CARTESIAN_POINT('Ctrl Pts',(178.858824452271,618.565422800512,-38.8022115113597)) ;
#58158 = CARTESIAN_POINT('Ctrl Pts',(178.990564734723,618.55796187353,-38.871486449181)) ;
#58159 = CARTESIAN_POINT('Ctrl Pts',(179.050362128865,618.554584290457,-38.8993448978869)) ;
#58160 = CARTESIAN_POINT('Ctrl Pts',(179.157258933908,618.54849327467,-38.9430190012259)) ;
#58161 = CARTESIAN_POINT('Ctrl Pts',(179.20378586791,618.545825814901,-38.9600922339088)) ;
#58162 = CARTESIAN_POINT('Ctrl Pts',(179.312169929997,618.539556043029,-38.9954736023798)) ;
#58163 = CARTESIAN_POINT('Ctrl Pts',(179.374360329489,618.535917063841,-39.0125834421195)) ;
#58164 = CARTESIAN_POINT('Ctrl Pts',(179.5802153312,618.523740225149,-39.0589264262495)) ;
#58165 = CARTESIAN_POINT('Ctrl Pts',(179.726206525767,618.514864335276,-39.0757221602284)) ;
#58166 = CARTESIAN_POINT('Ctrl Pts',(179.948302534723,618.501608568692,-39.0774308612065)) ;
#58167 = CARTESIAN_POINT('Ctrl Pts',(180.023866402557,618.497150861992,-39.0738414215875)) ;
#58168 = CARTESIAN_POINT('Ctrl Pts',(180.130322055668,618.491088932512,-39.0628758123629)) ;
#58169 = CARTESIAN_POINT('Ctrl Pts',(180.161502796812,618.48934047946,-39.0589394319344)) ;
#58170 = CARTESIAN_POINT('Ctrl Pts',(180.225712322454,618.485813081276,-39.0493321260682)) ;
#58171 = CARTESIAN_POINT('Ctrl Pts',(180.258717135631,618.484039559066,-39.0435655412924)) ;
#58172 = CARTESIAN_POINT('Ctrl Pts',(180.330747227359,618.480227518069,-39.0291568835457)) ;
#58173 = CARTESIAN_POINT('Ctrl Pts',(180.369691397373,618.4782045599,-39.020178123827)) ;
#58174 = CARTESIAN_POINT('Ctrl Pts',(180.493796374131,618.471811475084,-38.9877256030707)) ;
#58175 = CARTESIAN_POINT('Ctrl Pts',(180.577716191718,618.467567438777,-38.9598955044967)) ;
#58176 = CARTESIAN_POINT('Ctrl Pts',(180.774970011025,618.457285290354,-38.8800386740116)) ;
#58177 = CARTESIAN_POINT('Ctrl Pts',(180.885861987713,618.451232463878,-38.8229414252176)) ;
#58178 = CARTESIAN_POINT('Ctrl Pts',(181.035385943492,618.442112491024,-38.7278836789447)) ;
#58179 = CARTESIAN_POINT('Ctrl Pts',(181.07876619861,618.439342195626,-38.697901246832)) ;
#58180 = CARTESIAN_POINT('Ctrl Pts',(181.162137476564,618.433736417945,-38.6354071935382)) ;
#58181 = CARTESIAN_POINT('Ctrl Pts',(181.202153551803,618.430906022112,-38.602993575127)) ;
#58182 = CARTESIAN_POINT('Ctrl Pts',(181.317403243452,618.422310838689,-38.5022397837769)) ;
#58183 = CARTESIAN_POINT('Ctrl Pts',(181.388823549767,618.416376584277,-38.4297925276021)) ;
#58184 = CARTESIAN_POINT('Ctrl Pts',(181.541737413827,618.40229258387,-38.2497665914924)) ;
#58185 = CARTESIAN_POINT('Ctrl Pts',(181.618593258647,618.394074008006,-38.1388488094641)) ;
#58186 = CARTESIAN_POINT('Ctrl Pts',(181.704910577153,618.383739431602,-37.9837170132153)) ;
#58187 = CARTESIAN_POINT('Ctrl Pts',(181.724594738408,618.381285270113,-37.9455759404892)) ;
#58188 = CARTESIAN_POINT('Ctrl Pts',(181.755437896193,618.377301698849,-37.8809200770703)) ;
#58189 = CARTESIAN_POINT('Ctrl Pts',(181.767258746696,618.375737504471,-37.8547417504993)) ;
#58190 = CARTESIAN_POINT('Ctrl Pts',(181.796316346807,618.371787103676,-37.7866176271214)) ;
#58191 = CARTESIAN_POINT('Ctrl Pts',(181.812720084319,618.369445895648,-37.7443353452659)) ;
#58192 = CARTESIAN_POINT('Ctrl Pts',(181.848797120666,618.363929626167,-37.6413593251634)) ;
#58193 = CARTESIAN_POINT('Ctrl Pts',(181.867069807588,618.360804865118,-37.5802244572526)) ;
#58194 = CARTESIAN_POINT('Ctrl Pts',(181.922437871714,618.349665604171,-37.357721203799)) ;
#58195 = CARTESIAN_POINT('Ctrl Pts',(181.942850800634,618.341788867134,-37.1928801363761)) ;
#58196 = CARTESIAN_POINT('Ctrl Pts',(181.943404022786,618.330546555151,-36.9749850571563)) ;
#58197 = CARTESIAN_POINT('Ctrl Pts',(181.941533167896,618.327787165639,-36.9226107820929)) ;
#58198 = CARTESIAN_POINT('Ctrl Pts',(181.93379970047,618.322143924147,-36.8182119053593)) ;
#58199 = CARTESIAN_POINT('Ctrl Pts',(181.927946609171,618.319262393995,-36.7662260929597)) ;
#58200 = CARTESIAN_POINT('Ctrl Pts',(181.90300970013,618.309889593059,-36.6015463543813)) ;
#58201 = CARTESIAN_POINT('Ctrl Pts',(181.876510221542,618.303170319916,-36.4902080197683)) ;
#58202 = CARTESIAN_POINT('Ctrl Pts',(181.797194748318,618.287933050784,-36.2484378800886)) ;
#58203 = CARTESIAN_POINT('Ctrl Pts',(181.739966540451,618.279386662566,-36.1200328535147)) ;
#58204 = CARTESIAN_POINT('Ctrl Pts',(181.653501196833,618.269481012114,-35.9695554823476)) ;
#58205 = CARTESIAN_POINT('Ctrl Pts',(181.63619477641,618.267612317719,-35.941064356618)) ;
#58206 = CARTESIAN_POINT('Ctrl Pts',(181.604025215241,618.264352052203,-35.8908974682713)) ;
#58207 = CARTESIAN_POINT('Ctrl Pts',(181.589425771995,618.262944376528,-35.8690630999813)) ;
#58208 = CARTESIAN_POINT('Ctrl Pts',(181.556124742666,618.259874760947,-35.8212685712881)) ;
#58209 = CARTESIAN_POINT('Ctrl Pts',(181.537232829484,618.258225086448,-35.7954604800369)) ;
#58210 = CARTESIAN_POINT('Ctrl Pts',(181.517739089185,618.256600448668,-35.770094850444)) ;
#58211 = CARTESIAN_POINT('Origin',(29.8885276254223,620.2564904411,-37.0221601717529)) ;
#58212 = CARTESIAN_POINT('',(31.5177255283109,616.918093972863,-35.7700772049646)) ;
#58213 = CARTESIAN_POINT('',(31.5177255072015,616.859929736371,-35.7700771774972)) ;
#58214 = CARTESIAN_POINT('',(31.5177255210695,620.2564904411,-35.7700771955414)) ;
#58215 = CARTESIAN_POINT('',(29.0652954453167,616.710565160562,-35.13953266209)) ;
#58216 = CARTESIAN_POINT('Ctrl Pts',(31.5177255072015,616.859929736371,-35.7700771774972)) ;
#58217 = CARTESIAN_POINT('Ctrl Pts',(31.5070758016168,616.858913289289,-35.7562198869983)) ;
#58218 = CARTESIAN_POINT('Ctrl Pts',(31.4962483273789,616.857891707172,-35.7424972042907)) ;
#58219 = CARTESIAN_POINT('Ctrl Pts',(31.3993198244515,616.848852906981,-35.622823695312)) ;
#58220 = CARTESIAN_POINT('Ctrl Pts',(31.3030407494217,616.84056895853,-35.5255688104259)) ;
#58221 = CARTESIAN_POINT('Ctrl Pts',(31.1577709294923,616.829521299164,-35.4054595155509)) ;
#58222 = CARTESIAN_POINT('Ctrl Pts',(31.1164640319347,616.826523350537,-35.3738663346817)) ;
#58223 = CARTESIAN_POINT('Ctrl Pts',(31.0496272070208,616.821948325107,-35.3266555931457)) ;
#58224 = CARTESIAN_POINT('Ctrl Pts',(31.0248811535925,616.820312007831,-35.3099717983299)) ;
#58225 = CARTESIAN_POINT('Ctrl Pts',(30.9647529495311,616.816478629932,-35.2713117111252)) ;
#58226 = CARTESIAN_POINT('Ctrl Pts',(30.9290507794141,616.814312021376,-35.2498612881938)) ;
#58227 = CARTESIAN_POINT('Ctrl Pts',(30.7974219010079,616.80662762584,-35.1761265851227)) ;
#58228 = CARTESIAN_POINT('Ctrl Pts',(30.6980120090074,616.801384371956,-35.1304235094043)) ;
#58229 = CARTESIAN_POINT('Ctrl Pts',(30.471555861231,616.78977377737,-35.0474497055228)) ;
#58230 = CARTESIAN_POINT('Ctrl Pts',(30.3436058340661,616.783413451447,-35.0141005035696)) ;
#58231 = CARTESIAN_POINT('Ctrl Pts',(30.1546124015791,616.773647561923,-34.9838435558175)) ;
#58232 = CARTESIAN_POINT('Ctrl Pts',(30.0955014531932,616.770546090958,-34.9769959522721)) ;
#58233 = CARTESIAN_POINT('Ctrl Pts',(29.9804744645932,616.764381935861,-34.9687087925195)) ;
#58234 = CARTESIAN_POINT('Ctrl Pts',(29.9246323255411,616.761331149433,-34.9669685864957)) ;
#58235 = CARTESIAN_POINT('Ctrl Pts',(29.8098147855787,616.754928891967,-34.9680714506353)) ;
#58236 = CARTESIAN_POINT('Ctrl Pts',(29.7508931735155,616.751573047756,-34.971176959048)) ;
#58237 = CARTESIAN_POINT('Ctrl Pts',(29.5090659293153,616.737541431677,-34.9943905089217)) ;
#58238 = CARTESIAN_POINT('Ctrl Pts',(29.3291426086356,616.726413364237,-35.0364799321757)) ;
#58239 = CARTESIAN_POINT('Ctrl Pts',(29.1262892653866,616.714195092401,-35.1137350351922)) ;
#58240 = CARTESIAN_POINT('Ctrl Pts',(29.0956350468344,616.712360570578,-35.1262658123426)) ;
#58241 = CARTESIAN_POINT('Ctrl Pts',(29.0652954453167,616.710565160562,-35.13953266209)) ;
#58242 = CARTESIAN_POINT('',(28.2344189562597,616.711828241264,-35.79952680519)) ;
#58243 = CARTESIAN_POINT('Origin',(29.8885276254216,616.710565160562,-37.0221601717529)) ;
#58244 = CARTESIAN_POINT('Ctrl Pts',(28.2363225441489,616.713091321964,-35.8005972663254)) ;
#58245 = CARTESIAN_POINT('Ctrl Pts',(28.2461879736039,616.713987411299,-35.787253939836)) ;
#58246 = CARTESIAN_POINT('Ctrl Pts',(28.2562150344361,616.714872582277,-35.7740301393109)) ;
#58247 = CARTESIAN_POINT('Ctrl Pts',(28.2799467919758,616.716912631926,-35.7435076644347)) ;
#58248 = CARTESIAN_POINT('Ctrl Pts',(28.2937722969416,616.718060065299,-35.7263052242832)) ;
#58249 = CARTESIAN_POINT('Ctrl Pts',(28.3869420455029,616.725551514342,-35.6141284741815)) ;
#58250 = CARTESIAN_POINT('Ctrl Pts',(28.4744573232012,616.731475828916,-35.5262580427306)) ;
#58251 = CARTESIAN_POINT('Ctrl Pts',(28.6596557087188,616.743190129311,-35.3711777069199)) ;
#58252 = CARTESIAN_POINT('Ctrl Pts',(28.7562840888164,616.748954333741,-35.3034715834117)) ;
#58253 = CARTESIAN_POINT('Ctrl Pts',(28.9040598591426,616.757766104653,-35.217822661049)) ;
#58254 = CARTESIAN_POINT('Ctrl Pts',(28.9509573279974,616.760559292809,-35.1930150451144)) ;
#58255 = CARTESIAN_POINT('Ctrl Pts',(29.0464682789855,616.766271136086,-35.1471308166295)) ;
#58256 = CARTESIAN_POINT('Ctrl Pts',(29.0950415055828,616.769187351072,-35.1260646905364)) ;
#58257 = CARTESIAN_POINT('Ctrl Pts',(29.2473293032392,616.778380676497,-35.0668947150754)) ;
#58258 = CARTESIAN_POINT('Ctrl Pts',(29.3533330904979,616.784861443889,-35.0352631740274)) ;
#58259 = CARTESIAN_POINT('Ctrl Pts',(29.5549607882299,616.797170951437,-34.9924091893092)) ;
#58260 = CARTESIAN_POINT('Ctrl Pts',(29.6498446545391,616.802952864566,-34.9790775434269)) ;
#58261 = CARTESIAN_POINT('Ctrl Pts',(29.7866736101263,616.811046505724,-34.9695173861438)) ;
#58262 = CARTESIAN_POINT('Ctrl Pts',(29.8281148978698,616.813464912003,-34.9678799296528)) ;
#58263 = CARTESIAN_POINT('Ctrl Pts',(29.9040235380157,616.817802751366,-34.9671798941917)) ;
#58264 = CARTESIAN_POINT('Ctrl Pts',(29.9384725971119,616.819736644985,-34.9677284066378)) ;
#58265 = CARTESIAN_POINT('Ctrl Pts',(30.003914294452,616.823323617532,-34.9704176490453)) ;
#58266 = CARTESIAN_POINT('Ctrl Pts',(30.0349022557098,616.824983304555,-34.9723953062286)) ;
#58267 = CARTESIAN_POINT('Ctrl Pts',(30.1377297047151,616.830393633256,-34.9813016263603)) ;
#58268 = CARTESIAN_POINT('Ctrl Pts',(30.2092536173663,616.834000962602,-34.9913125852556)) ;
#58269 = CARTESIAN_POINT('Ctrl Pts',(30.4436538618571,616.845717434096,-35.03681693915)) ;
#58270 = CARTESIAN_POINT('Ctrl Pts',(30.6027257030683,616.853550066324,-35.088336202994)) ;
#58271 = CARTESIAN_POINT('Ctrl Pts',(30.8081311364695,616.865020887423,-35.1837068592273)) ;
#58272 = CARTESIAN_POINT('Ctrl Pts',(30.8612957951291,616.868118609061,-35.2112757521316)) ;
#58273 = CARTESIAN_POINT('Ctrl Pts',(30.9563653462243,616.873947110266,-35.265970372132)) ;
#58274 = CARTESIAN_POINT('Ctrl Pts',(30.9986314399163,616.876650128572,-35.2923772591693)) ;
#58275 = CARTESIAN_POINT('Ctrl Pts',(31.1002082138946,616.883444628465,-35.3610970904895)) ;
#58276 = CARTESIAN_POINT('Ctrl Pts',(31.1583049759041,616.887597582255,-35.4050751128561)) ;
#58277 = CARTESIAN_POINT('Ctrl Pts',(31.3262979694729,616.900421320143,-35.5468859946604)) ;
#58278 = CARTESIAN_POINT('Ctrl Pts',(31.4281461657989,616.909377068406,-35.6535162573635)) ;
#58279 = CARTESIAN_POINT('Ctrl Pts',(31.5177316112097,616.918094564784,-35.7700851200118)) ;
#58280 = CARTESIAN_POINT('Origin',(29.8885276254223,620.2564904411,-37.0221601717529)) ;
#58281 = CARTESIAN_POINT('',(31.5177255210722,617.617782467769,-35.7700771955454)) ;
#58282 = CARTESIAN_POINT('',(31.5177255210691,617.559653386529,-35.7700771955414)) ;
#58283 = CARTESIAN_POINT('',(31.5177255210695,620.2564904411,-35.7700771955414)) ;
#58284 = CARTESIAN_POINT('',(29.8879638322405,617.107918393054,-39.0769100944046)) ;
#58285 = CARTESIAN_POINT('Ctrl Pts',(31.5177255210691,617.559653386529,-35.7700771955414)) ;
#58286 = CARTESIAN_POINT('Ctrl Pts',(31.502991126039,617.558435449222,-35.7509049475094)) ;
#58287 = CARTESIAN_POINT('Ctrl Pts',(31.4879129621458,617.557206784429,-35.7319858330172)) ;
#58288 = CARTESIAN_POINT('Ctrl Pts',(31.4375483698562,617.553152210874,-35.6710337459098)) ;
#58289 = CARTESIAN_POINT('Ctrl Pts',(31.4009221260746,617.550278991236,-35.6301580101145)) ;
#58290 = CARTESIAN_POINT('Ctrl Pts',(31.3267030075278,617.544561639328,-35.5537187131028)) ;
#58291 = CARTESIAN_POINT('Ctrl Pts',(31.289316142577,617.54172762946,-35.5180127086929)) ;
#58292 = CARTESIAN_POINT('Ctrl Pts',(31.1799902393308,617.533548717352,-35.4212159312012)) ;
#58293 = CARTESIAN_POINT('Ctrl Pts',(31.1051401783234,617.528066766664,-35.3636221502404)) ;
#58294 = CARTESIAN_POINT('Ctrl Pts',(30.9123588128159,617.514315078443,-35.2353764267797)) ;
#58295 = CARTESIAN_POINT('Ctrl Pts',(30.7907893302688,617.505931073154,-35.1710120597553)) ;
#58296 = CARTESIAN_POINT('Ctrl Pts',(30.6195492721135,617.495100987945,-35.1012543683798)) ;
#58297 = CARTESIAN_POINT('Ctrl Pts',(30.5747682416913,617.492356018127,-35.0848046893483)) ;
#58298 = CARTESIAN_POINT('Ctrl Pts',(30.5017221218475,617.48806195108,-35.0608234065258)) ;
#58299 = CARTESIAN_POINT('Ctrl Pts',(30.4738016783234,617.486464449153,-35.0523114567785)) ;
#58300 = CARTESIAN_POINT('Ctrl Pts',(30.4046469229523,617.482616540755,-35.0328291440998)) ;
#58301 = CARTESIAN_POINT('Ctrl Pts',(30.3632362678253,617.480401567754,-35.0225428867216)) ;
#58302 = CARTESIAN_POINT('Ctrl Pts',(30.2653072842815,617.475308431126,-35.0014318743699)) ;
#58303 = CARTESIAN_POINT('Ctrl Pts',(30.2085947381004,617.472469910751,-34.9916766096514)) ;
#58304 = CARTESIAN_POINT('Ctrl Pts',(29.9731022906157,617.460882721466,-34.9612824677208)) ;
#58305 = CARTESIAN_POINT('Ctrl Pts',(29.7924221408081,617.452382551702,-34.9617883859521)) ;
#58306 = CARTESIAN_POINT('Ctrl Pts',(29.562198858248,617.44036749658,-34.9928126447981)) ;
#58307 = CARTESIAN_POINT('Ctrl Pts',(29.510572338815,617.437601327174,-35.0017911498368)) ;
#58308 = CARTESIAN_POINT('Ctrl Pts',(29.4066479320116,617.431858312386,-35.0239876255355)) ;
#58309 = CARTESIAN_POINT('Ctrl Pts',(29.3544149773128,617.428879919666,-35.0373114459427)) ;
#58310 = CARTESIAN_POINT('Ctrl Pts',(29.2383412229445,617.422041677258,-35.0718336985198)) ;
#58311 = CARTESIAN_POINT('Ctrl Pts',(29.1748976216132,617.418149535632,-35.0941439369834)) ;
#58312 = CARTESIAN_POINT('Ctrl Pts',(28.9873492175115,617.406210048386,-35.1706228033579)) ;
#58313 = CARTESIAN_POINT('Ctrl Pts',(28.8673968171397,617.397956733476,-35.233976201964)) ;
#58314 = CARTESIAN_POINT('Ctrl Pts',(28.7050266674759,617.386422592202,-35.3414313445753)) ;
#58315 = CARTESIAN_POINT('Ctrl Pts',(28.6569455556233,617.382960385271,-35.3763379866491)) ;
#58316 = CARTESIAN_POINT('Ctrl Pts',(28.5871134581726,617.377937531909,-35.4318123188885)) ;
#58317 = CARTESIAN_POINT('Ctrl Pts',(28.5641899467216,617.376290411072,-35.4508501289309)) ;
#58318 = CARTESIAN_POINT('Ctrl Pts',(28.5137153392614,617.372679274582,-35.4946588149386)) ;
#58319 = CARTESIAN_POINT('Ctrl Pts',(28.486404875669,617.370732966615,-35.5196884152189)) ;
#58320 = CARTESIAN_POINT('Ctrl Pts',(28.4265927164114,617.36644823922,-35.5775575195833)) ;
#58321 = CARTESIAN_POINT('Ctrl Pts',(28.3944915102253,617.364132782466,-35.6107824627978)) ;
#58322 = CARTESIAN_POINT('Ctrl Pts',(28.2803180623839,617.355715753428,-35.7372176454534)) ;
#58323 = CARTESIAN_POINT('Ctrl Pts',(28.2056236270247,617.349824927486,-35.8367272637574)) ;
#58324 = CARTESIAN_POINT('Ctrl Pts',(28.0952268731418,617.339508001895,-36.0154581225617)) ;
#58325 = CARTESIAN_POINT('Ctrl Pts',(28.0547164842007,617.335204126619,-36.0912943017524)) ;
#58326 = CARTESIAN_POINT('Ctrl Pts',(27.9980973707526,617.328102653095,-36.2154226000785)) ;
#58327 = CARTESIAN_POINT('Ctrl Pts',(27.9788276283632,617.325417757679,-36.2621619029228)) ;
#58328 = CARTESIAN_POINT('Ctrl Pts',(27.9418742575579,617.319629991556,-36.3621024476641)) ;
#58329 = CARTESIAN_POINT('Ctrl Pts',(27.9246052753928,617.316515659955,-36.4154117360528)) ;
#58330 = CARTESIAN_POINT('Ctrl Pts',(27.8928049523524,617.309799908756,-36.5292542321095)) ;
#58331 = CARTESIAN_POINT('Ctrl Pts',(27.8788025471966,617.306185876264,-36.5898763071068)) ;
#58332 = CARTESIAN_POINT('Ctrl Pts',(27.8417339647674,617.294067479475,-36.7917333186514)) ;
#58333 = CARTESIAN_POINT('Ctrl Pts',(27.8306611104694,617.285318600139,-36.9347344745592)) ;
#58334 = CARTESIAN_POINT('Ctrl Pts',(27.8359513091915,617.273794571544,-37.1303028387367)) ;
#58335 = CARTESIAN_POINT('Ctrl Pts',(27.8393923308154,617.270748228964,-37.1828144292426)) ;
#58336 = CARTESIAN_POINT('Ctrl Pts',(27.8478967474127,617.266146320857,-37.2644199927145)) ;
#58337 = CARTESIAN_POINT('Ctrl Pts',(27.8515771213451,617.264526829675,-37.2936324753227)) ;
#58338 = CARTESIAN_POINT('Ctrl Pts',(27.8616648490393,617.260817914198,-37.3618451048856)) ;
#58339 = CARTESIAN_POINT('Ctrl Pts',(27.8685714178916,617.258753927448,-37.4007574734309)) ;
#58340 = CARTESIAN_POINT('Ctrl Pts',(27.8990527993423,617.251075135044,-37.5477214915681)) ;
#58341 = CARTESIAN_POINT('Ctrl Pts',(27.9302145641686,617.24575567078,-37.6540135586227)) ;
#58342 = CARTESIAN_POINT('Ctrl Pts',(28.0157023503227,617.234196138655,-37.8771438990388)) ;
#58343 = CARTESIAN_POINT('Ctrl Pts',(28.0727494026608,617.227959746302,-37.9924268047008)) ;
#58344 = CARTESIAN_POINT('Ctrl Pts',(28.168040873026,617.218611856161,-38.146765489254)) ;
#58345 = CARTESIAN_POINT('Ctrl Pts',(28.1976460384395,617.215820439363,-38.1908049243284)) ;
#58346 = CARTESIAN_POINT('Ctrl Pts',(28.2598619851919,617.210134992398,-38.2760341031513)) ;
#58347 = CARTESIAN_POINT('Ctrl Pts',(28.2924139222578,617.207244521475,-38.3172168987872)) ;
#58348 = CARTESIAN_POINT('Ctrl Pts',(28.3984101666931,617.198064207035,-38.4412433327354)) ;
#58349 = CARTESIAN_POINT('Ctrl Pts',(28.4769869049569,617.191563539166,-38.5194223987981)) ;
#58350 = CARTESIAN_POINT('Ctrl Pts',(28.6718413347213,617.176279119739,-38.6842592156002)) ;
#58351 = CARTESIAN_POINT('Ctrl Pts',(28.7917656033892,617.167437868424,-38.7657239882183)) ;
#58352 = CARTESIAN_POINT('Ctrl Pts',(28.9492871742426,617.157217127079,-38.849996417456)) ;
#58353 = CARTESIAN_POINT('Ctrl Pts',(28.9797206142325,617.155303028099,-38.8653172714772)) ;
#58354 = CARTESIAN_POINT('Ctrl Pts',(29.039259880253,617.151694418015,-38.8934570856586)) ;
#58355 = CARTESIAN_POINT('Ctrl Pts',(29.0683092671745,617.149995176269,-38.9063708426932)) ;
#58356 = CARTESIAN_POINT('Ctrl Pts',(29.1692992035839,617.144259019019,-38.9484869463668)) ;
#58357 = CARTESIAN_POINT('Ctrl Pts',(29.2425932038203,617.140388324798,-38.9742859911017)) ;
#58358 = CARTESIAN_POINT('Ctrl Pts',(29.4630978199586,617.129131617353,-39.0381175533183)) ;
#58359 = CARTESIAN_POINT('Ctrl Pts',(29.6132467134803,617.121925270207,-39.0640453542879)) ;
#58360 = CARTESIAN_POINT('Ctrl Pts',(29.8058657166775,617.112166553026,-39.0756572525885)) ;
#58361 = CARTESIAN_POINT('Ctrl Pts',(29.8469109682732,617.11006072416,-39.0768988301021)) ;
#58362 = CARTESIAN_POINT('Ctrl Pts',(29.8879638322405,617.107918393054,-39.0769100944046)) ;
#58363 = CARTESIAN_POINT('Ctrl Pts',(29.8879650432987,617.107918329855,-39.0769100947366)) ;
#58364 = CARTESIAN_POINT('Ctrl Pts',(29.9315771889072,617.105642442673,-39.0769220355636)) ;
#58365 = CARTESIAN_POINT('Ctrl Pts',(29.9751768076821,617.103326411558,-39.0755454802514)) ;
#58366 = CARTESIAN_POINT('Ctrl Pts',(30.0708303228857,617.09813884521,-39.0694735329993)) ;
#58367 = CARTESIAN_POINT('Ctrl Pts',(30.1228134801749,617.095249816721,-39.0641777290822)) ;
#58368 = CARTESIAN_POINT('Ctrl Pts',(30.3382243479021,617.082966641511,-39.03389919662)) ;
#58369 = CARTESIAN_POINT('Ctrl Pts',(30.4985175174765,617.073008081404,-38.9912251018306)) ;
#58370 = CARTESIAN_POINT('Ctrl Pts',(30.7363796074016,617.057611673656,-38.8960377293712)) ;
#58371 = CARTESIAN_POINT('Ctrl Pts',(30.8184930569696,617.052187039343,-38.856672950899)) ;
#58372 = CARTESIAN_POINT('Ctrl Pts',(30.926001939634,617.045164364312,-38.796053574394)) ;
#58373 = CARTESIAN_POINT('Ctrl Pts',(30.9538916559741,617.043350842893,-38.7794451825445)) ;
#58374 = CARTESIAN_POINT('Ctrl Pts',(31.0098105175161,617.039750175778,-38.7443243603351)) ;
#58375 = CARTESIAN_POINT('Ctrl Pts',(31.0378023568366,617.037965795252,-38.7257718348289)) ;
#58376 = CARTESIAN_POINT('Ctrl Pts',(31.171043081828,617.029496975284,-38.6326825087456)) ;
#58377 = CARTESIAN_POINT('Ctrl Pts',(31.2695811741949,617.02329746239,-38.5490283005279)) ;
#58378 = CARTESIAN_POINT('Ctrl Pts',(31.4437645929501,617.011175323734,-38.3704025050064)) ;
#58379 = CARTESIAN_POINT('Ctrl Pts',(31.5201380657735,617.005281005028,-38.276896562426)) ;
#58380 = CARTESIAN_POINT('Ctrl Pts',(31.6180742208949,616.996289879995,-38.1328141854124)) ;
#58381 = CARTESIAN_POINT('Ctrl Pts',(31.6465187571827,616.993459394362,-38.0872189692384)) ;
#58382 = CARTESIAN_POINT('Ctrl Pts',(31.6996966574815,616.987671397294,-37.9940319069262)) ;
#58383 = CARTESIAN_POINT('Ctrl Pts',(31.7244185946076,616.984716508215,-37.9464823676244)) ;
#58384 = CARTESIAN_POINT('Ctrl Pts',(31.7953781938994,616.975336137687,-37.7958945905848)) ;
#58385 = CARTESIAN_POINT('Ctrl Pts',(31.8349981783252,616.96869480133,-37.6899854309348)) ;
#58386 = CARTESIAN_POINT('Ctrl Pts',(31.8917462987526,616.956207680718,-37.4893425415177)) ;
#58387 = CARTESIAN_POINT('Ctrl Pts',(31.9113181040995,616.950414417912,-37.3956082111246)) ;
#58388 = CARTESIAN_POINT('Ctrl Pts',(31.9320022987042,616.941395619489,-37.2445156793934)) ;
#58389 = CARTESIAN_POINT('Ctrl Pts',(31.9373733476164,616.938086874235,-37.1878796874816)) ;
#58390 = CARTESIAN_POINT('Ctrl Pts',(31.9419490093459,616.933230205193,-37.101689858339)) ;
#58391 = CARTESIAN_POINT('Ctrl Pts',(31.9428778902427,616.931603421004,-37.0722570072935)) ;
#58392 = CARTESIAN_POINT('Ctrl Pts',(31.9435203274071,616.928153804639,-37.0083387008325)) ;
#58393 = CARTESIAN_POINT('Ctrl Pts',(31.942999213504,616.92634391122,-36.9738605568451)) ;
#58394 = CARTESIAN_POINT('Ctrl Pts',(31.9370641261593,616.918769897551,-36.8266080748743)) ;
#58395 = CARTESIAN_POINT('Ctrl Pts',(31.9232284056203,616.913380509238,-36.7143608993811)) ;
#58396 = CARTESIAN_POINT('Ctrl Pts',(31.8720276180124,616.901387063719,-36.4681529992633)) ;
#58397 = CARTESIAN_POINT('Ctrl Pts',(31.8301709992059,616.894798434857,-36.3357102627553)) ;
#58398 = CARTESIAN_POINT('Ctrl Pts',(31.7532891834867,616.884937280678,-36.1574327091939)) ;
#58399 = CARTESIAN_POINT('Ctrl Pts',(31.7292089626923,616.882049546242,-36.1072936903947)) ;
#58400 = CARTESIAN_POINT('Ctrl Pts',(31.6797251012503,616.87642981557,-36.0141436132491)) ;
#58401 = CARTESIAN_POINT('Ctrl Pts',(31.6547287678234,616.873714378485,-35.9709614851591)) ;
#58402 = CARTESIAN_POINT('Ctrl Pts',(31.5938687678378,616.867356440517,-35.874132168649)) ;
#58403 = CARTESIAN_POINT('Ctrl Pts',(31.5570063355971,616.863678843146,-35.8211889989262)) ;
#58404 = CARTESIAN_POINT('Ctrl Pts',(31.5177255072015,616.859929736371,-35.7700771774972)) ;
#58405 = CARTESIAN_POINT('Ctrl Pts',(31.5177255283109,616.918093972863,-35.7700772049646)) ;
#58406 = CARTESIAN_POINT('Ctrl Pts',(31.5504703761168,616.92128033574,-35.812684475242)) ;
#58407 = CARTESIAN_POINT('Ctrl Pts',(31.5815278351766,616.924425086327,-35.8565546524622)) ;
#58408 = CARTESIAN_POINT('Ctrl Pts',(31.6257430902973,616.929040762863,-35.9245140082766)) ;
#58409 = CARTESIAN_POINT('Ctrl Pts',(31.6401914556706,616.930574133232,-35.9477214087963)) ;
#58410 = CARTESIAN_POINT('Ctrl Pts',(31.6695115632588,616.93372873491,-35.9969806283676)) ;
#58411 = CARTESIAN_POINT('Ctrl Pts',(31.6842835650919,616.935341188256,-36.0230818316763)) ;
#58412 = CARTESIAN_POINT('Ctrl Pts',(31.7268984222215,616.940085810236,-36.10238056251)) ;
#58413 = CARTESIAN_POINT('Ctrl Pts',(31.7529882615877,616.9431230095,-36.1564873560444)) ;
#58414 = CARTESIAN_POINT('Ctrl Pts',(31.8297213296731,616.952761267061,-36.335245781618)) ;
#58415 = CARTESIAN_POINT('Ctrl Pts',(31.8705100498814,616.959108104695,-36.4637403265578)) ;
#58416 = CARTESIAN_POINT('Ctrl Pts',(31.9123597814348,616.96900463626,-36.6607963977105)) ;
#58417 = CARTESIAN_POINT('Ctrl Pts',(31.9230586170022,616.97234802105,-36.7269262624697)) ;
#58418 = CARTESIAN_POINT('Ctrl Pts',(31.9364883062573,616.978544805199,-36.8468335709622)) ;
#58419 = CARTESIAN_POINT('Ctrl Pts',(31.9403709603395,616.981361522084,-36.900420321945)) ;
#58420 = CARTESIAN_POINT('Ctrl Pts',(31.9438520414071,616.987006424688,-37.0054489306091)) ;
#58421 = CARTESIAN_POINT('Ctrl Pts',(31.9436271335698,616.98982675231,-37.0568452382634)) ;
#58422 = CARTESIAN_POINT('Ctrl Pts',(31.9374503976631,616.998098742825,-37.2042659241374)) ;
#58423 = CARTESIAN_POINT('Ctrl Pts',(31.9266836122089,617.003696372191,-37.2999430552917)) ;
#58424 = CARTESIAN_POINT('Ctrl Pts',(31.888853368992,617.016112342874,-37.5052493637281)) ;
#58425 = CARTESIAN_POINT('Ctrl Pts',(31.8593789487323,617.022957650745,-37.6141250879011)) ;
#58426 = CARTESIAN_POINT('Ctrl Pts',(31.8060606756644,617.0322757838,-37.761777724535)) ;
#58427 = CARTESIAN_POINT('Ctrl Pts',(31.7896382870827,617.034880784364,-37.8030223878796)) ;
#58428 = CARTESIAN_POINT('Ctrl Pts',(31.7574948070252,617.039500564444,-37.8767102755709)) ;
#58429 = CARTESIAN_POINT('Ctrl Pts',(31.742231314005,617.041533138547,-37.9093338835254)) ;
#58430 = CARTESIAN_POINT('Ctrl Pts',(31.712653570239,617.045169952847,-37.9684516292274)) ;
#58431 = CARTESIAN_POINT('Ctrl Pts',(31.6986006541938,617.046786975107,-37.995062353153)) ;
#58432 = CARTESIAN_POINT('Ctrl Pts',(31.6541338665252,617.051604966576,-38.0749640872589)) ;
#58433 = CARTESIAN_POINT('Ctrl Pts',(31.6219113062678,617.054706274737,-38.127213892491)) ;
#58434 = CARTESIAN_POINT('Ctrl Pts',(31.5123835074203,617.064349323908,-38.2882066630305)) ;
#58435 = CARTESIAN_POINT('Ctrl Pts',(31.4268140636884,617.070653774258,-38.3909037134841)) ;
#58436 = CARTESIAN_POINT('Ctrl Pts',(31.2842042798917,617.080513330055,-38.5316547445731)) ;
#58437 = CARTESIAN_POINT('Ctrl Pts',(31.2342442199837,617.08386525464,-38.5763587020572)) ;
#58438 = CARTESIAN_POINT('Ctrl Pts',(31.140624725421,617.090065034447,-38.6522255057367)) ;
#58439 = CARTESIAN_POINT('Ctrl Pts',(31.097760134777,617.092875582938,-38.6842721361552)) ;
#58440 = CARTESIAN_POINT('Ctrl Pts',(31.0108498884887,617.098551729317,-38.7441056503696)) ;
#58441 = CARTESIAN_POINT('Ctrl Pts',(30.9669019100713,617.101411522617,-38.7719635021546)) ;
#58442 = CARTESIAN_POINT('Ctrl Pts',(30.7649452818898,617.114532418059,-38.8894805824347)) ;
#58443 = CARTESIAN_POINT('Ctrl Pts',(30.5965423156839,617.125515560337,-38.9596033015113)) ;
#58444 = CARTESIAN_POINT('Ctrl Pts',(30.343239904977,617.141223374881,-39.0275887881929)) ;
#58445 = CARTESIAN_POINT('Ctrl Pts',(30.2641443442507,617.146004141819,-39.0438974097544)) ;
#58446 = CARTESIAN_POINT('Ctrl Pts',(30.1528958369099,617.152386198162,-39.060079057168)) ;
#58447 = CARTESIAN_POINT('Ctrl Pts',(30.1213984966922,617.1541551225,-39.0639181032308)) ;
#58448 = CARTESIAN_POINT('Ctrl Pts',(30.0565752019225,617.157700480766,-39.0702992396898)) ;
#58449 = CARTESIAN_POINT('Ctrl Pts',(30.0232512775326,617.159472735478,-39.0727609262248)) ;
#58450 = CARTESIAN_POINT('Ctrl Pts',(29.8595380961235,617.167996642145,-39.0808460714569)) ;
#58451 = CARTESIAN_POINT('Ctrl Pts',(29.7288648069245,617.174246301298,-39.0748518630524)) ;
#58452 = CARTESIAN_POINT('Ctrl Pts',(29.4798107975362,617.186427593269,-39.0394838586637)) ;
#58453 = CARTESIAN_POINT('Ctrl Pts',(29.3617340729236,617.192329162083,-39.011916288408)) ;
#58454 = CARTESIAN_POINT('Ctrl Pts',(29.1960941755263,617.201307513484,-38.9574586002064)) ;
#58455 = CARTESIAN_POINT('Ctrl Pts',(29.1460820623195,617.20411233534,-38.9388286312322)) ;
#58456 = CARTESIAN_POINT('Ctrl Pts',(29.0486770461878,617.2097944305,-38.898159699867)) ;
#58457 = CARTESIAN_POINT('Ctrl Pts',(29.0012875165223,617.212666733969,-38.8762172113009)) ;
#58458 = CARTESIAN_POINT('Ctrl Pts',(28.7960472441117,617.225614690331,-38.771514516949)) ;
#58459 = CARTESIAN_POINT('Ctrl Pts',(28.6485375963178,617.236378366049,-38.6702370148164)) ;
#58460 = CARTESIAN_POINT('Ctrl Pts',(28.4540009811894,617.252051311751,-38.4956136231043)) ;
#58461 = CARTESIAN_POINT('Ctrl Pts',(28.3954659820874,617.256994412151,-38.436268025622)) ;
#58462 = CARTESIAN_POINT('Ctrl Pts',(28.3197243948614,617.263537183279,-38.3495147776606)) ;
#58463 = CARTESIAN_POINT('Ctrl Pts',(28.2993182099413,617.265316107096,-38.3250138088617)) ;
#58464 = CARTESIAN_POINT('Ctrl Pts',(28.2588900992197,617.268856730283,-38.2741090997091)) ;
#58465 = CARTESIAN_POINT('Ctrl Pts',(28.2389201579336,617.27061522854,-38.2476764179967)) ;
#58466 = CARTESIAN_POINT('Ctrl Pts',(28.1416362127798,617.279295145511,-38.1122194395653)) ;
#58467 = CARTESIAN_POINT('Ctrl Pts',(28.0744433992065,617.285684147149,-37.996308591324)) ;
#58468 = CARTESIAN_POINT('Ctrl Pts',(27.9687631401648,617.29802012389,-37.7645559045053)) ;
#58469 = CARTESIAN_POINT('Ctrl Pts',(27.9283770598511,617.3039306574,-37.6502153177323)) ;
#58470 = CARTESIAN_POINT('Ctrl Pts',(27.8851688249047,617.312896547507,-37.4818737544366)) ;
#58471 = CARTESIAN_POINT('Ctrl Pts',(27.8740230286492,617.315676119635,-37.4302699809292)) ;
#58472 = CARTESIAN_POINT('Ctrl Pts',(27.8557511023794,617.321359702055,-37.3264447772798)) ;
#58473 = CARTESIAN_POINT('Ctrl Pts',(27.8486226890249,617.324261256862,-37.2742645895387)) ;
#58474 = CARTESIAN_POINT('Ctrl Pts',(27.8338595758887,617.332812085135,-37.1230919061091)) ;
#58475 = CARTESIAN_POINT('Ctrl Pts',(27.8313836469252,617.338615415119,-37.0237549811193)) ;
#58476 = CARTESIAN_POINT('Ctrl Pts',(27.8411560044508,617.350896607055,-36.8180873847492)) ;
#58477 = CARTESIAN_POINT('Ctrl Pts',(27.8545081233521,617.35737442525,-36.7120946622519)) ;
#58478 = CARTESIAN_POINT('Ctrl Pts',(27.8881306274189,617.367254916963,-36.5488655668992)) ;
#58479 = CARTESIAN_POINT('Ctrl Pts',(27.9028008764859,617.37075559266,-36.4906656854881)) ;
#58480 = CARTESIAN_POINT('Ctrl Pts',(27.928591868237,617.37582674508,-36.4044642621942)) ;
#58481 = CARTESIAN_POINT('Ctrl Pts',(27.9378138894227,617.377485457928,-36.3759305320441)) ;
#58482 = CARTESIAN_POINT('Ctrl Pts',(27.9596413734839,617.381079730528,-36.3131272538345)) ;
#58483 = CARTESIAN_POINT('Ctrl Pts',(27.9725415290632,617.382999550098,-36.2789727902339)) ;
#58484 = CARTESIAN_POINT('Ctrl Pts',(28.0487700735364,617.393388233787,-36.092352601581)) ;
#58485 = CARTESIAN_POINT('Ctrl Pts',(28.1293898941948,617.401109566302,-35.9475922514663)) ;
#58486 = CARTESIAN_POINT('Ctrl Pts',(28.2794081723667,617.413602761734,-35.7412085190113)) ;
#58487 = CARTESIAN_POINT('Ctrl Pts',(28.3370654608879,617.418096248167,-35.6719507544019)) ;
#58488 = CARTESIAN_POINT('Ctrl Pts',(28.4343066963667,617.42542942223,-35.5696262346848)) ;
#58489 = CARTESIAN_POINT('Ctrl Pts',(28.4709083876609,617.428141371419,-35.5338831756515)) ;
#58490 = CARTESIAN_POINT('Ctrl Pts',(28.5495459472495,617.433896809562,-35.4626254266216)) ;
#58491 = CARTESIAN_POINT('Ctrl Pts',(28.5917509012738,617.436947652639,-35.4273592883029)) ;
#58492 = CARTESIAN_POINT('Ctrl Pts',(28.759647540145,617.448959362497,-35.2981410543486)) ;
#58493 = CARTESIAN_POINT('Ctrl Pts',(28.8945142251436,617.458404099755,-35.2170186846993)) ;
#58494 = CARTESIAN_POINT('Ctrl Pts',(29.0948463575378,617.471623183932,-35.1258295400905)) ;
#58495 = CARTESIAN_POINT('Ctrl Pts',(29.1536077095088,617.475403672968,-35.1022921382166)) ;
#58496 = CARTESIAN_POINT('Ctrl Pts',(29.2560353067579,617.481736148464,-35.0666570952842)) ;
#58497 = CARTESIAN_POINT('Ctrl Pts',(29.2991882114397,617.484328380547,-35.053221757059)) ;
#58498 = CARTESIAN_POINT('Ctrl Pts',(29.370662057624,617.488460067083,-35.0335297595935)) ;
#58499 = CARTESIAN_POINT('Ctrl Pts',(29.398730250739,617.490040619739,-35.0264311268173)) ;
#58500 = CARTESIAN_POINT('Ctrl Pts',(29.4698531621015,617.493941723509,-35.0100348535839)) ;
#58501 = CARTESIAN_POINT('Ctrl Pts',(29.5130722666402,617.496221999972,-35.0015240268596)) ;
#58502 = CARTESIAN_POINT('Ctrl Pts',(29.6903010573981,617.505326967233,-34.972507285805)) ;
#58503 = CARTESIAN_POINT('Ctrl Pts',(29.8259155322748,617.511745300934,-34.9638949022875)) ;
#58504 = CARTESIAN_POINT('Ctrl Pts',(30.0614098466465,617.523222240443,-34.9722518193884)) ;
#58505 = CARTESIAN_POINT('Ctrl Pts',(30.1610210524882,617.528177819032,-34.9831022698607)) ;
#58506 = CARTESIAN_POINT('Ctrl Pts',(30.3104304591404,617.536043138459,-35.0105231942293)) ;
#58507 = CARTESIAN_POINT('Ctrl Pts',(30.3610465084739,617.538783291811,-35.0218075559155)) ;
#58508 = CARTESIAN_POINT('Ctrl Pts',(30.4631846030945,617.544494843745,-35.0486712308223)) ;
#58509 = CARTESIAN_POINT('Ctrl Pts',(30.5146293087276,617.547468865616,-35.0643846099378)) ;
#58510 = CARTESIAN_POINT('Ctrl Pts',(30.7251790752793,617.560068356588,-35.1378432037574)) ;
#58511 = CARTESIAN_POINT('Ctrl Pts',(30.8774438854176,617.570286891645,-35.2131098293127)) ;
#58512 = CARTESIAN_POINT('Ctrl Pts',(31.0894716818041,617.585512951448,-35.352757225089)) ;
#58513 = CARTESIAN_POINT('Ctrl Pts',(31.1572708861873,617.590545224624,-35.403683800898)) ;
#58514 = CARTESIAN_POINT('Ctrl Pts',(31.2460584333802,617.597175873938,-35.4793934037561)) ;
#58515 = CARTESIAN_POINT('Ctrl Pts',(31.2698945611658,617.598959928042,-35.500698731266)) ;
#58516 = CARTESIAN_POINT('Ctrl Pts',(31.3173271751894,617.602500572974,-35.5451293765081)) ;
#58517 = CARTESIAN_POINT('Ctrl Pts',(31.3408824356191,617.604254354984,-35.5682846927383)) ;
#58518 = CARTESIAN_POINT('Ctrl Pts',(31.4185112090113,617.610060823034,-35.6483659421535)) ;
#58519 = CARTESIAN_POINT('Ctrl Pts',(31.4698810713146,617.613950295082,-35.7078224741377)) ;
#58520 = CARTESIAN_POINT('Ctrl Pts',(31.5177255210752,617.617782467769,-35.7700771955494)) ;
#58521 = CARTESIAN_POINT('Origin',(29.8885276254223,620.2564904411,-37.0221601717529)) ;
#58522 = CARTESIAN_POINT('',(31.5172546949865,618.315547812711,-35.7705124947133)) ;
#58523 = CARTESIAN_POINT('',(31.5177255210653,618.256605597193,-35.7700771955364)) ;
#58524 = CARTESIAN_POINT('',(31.5177255210695,620.2564904411,-35.7700771955414)) ;
#58525 = CARTESIAN_POINT('',(29.8880104657039,618.564640757452,-39.076910106671)) ;
#58526 = CARTESIAN_POINT('Ctrl Pts',(29.8879717390109,618.563699092458,-39.076366355844)) ;
#58527 = CARTESIAN_POINT('Ctrl Pts',(29.958886902367,618.559625141501,-39.0762487268419)) ;
#58528 = CARTESIAN_POINT('Ctrl Pts',(30.029843646248,618.555606320871,-39.0724866387931)) ;
#58529 = CARTESIAN_POINT('Ctrl Pts',(30.1004452629841,618.551672025826,-39.0651066485485)) ;
#58530 = CARTESIAN_POINT('Ctrl Pts',(30.1710285639294,618.547738751434,-39.0577285728543)) ;
#58531 = CARTESIAN_POINT('Ctrl Pts',(30.2412569002453,618.543889988967,-39.0467344870698)) ;
#58532 = CARTESIAN_POINT('Ctrl Pts',(30.3107380554495,618.540130523603,-39.032185393595)) ;
#58533 = CARTESIAN_POINT('Ctrl Pts',(30.3802249924105,618.536370745402,-39.017635089442)) ;
#58534 = CARTESIAN_POINT('Ctrl Pts',(30.4489645533068,618.532700206655,-38.9995290920226)) ;
#58535 = CARTESIAN_POINT('Ctrl Pts',(30.5165692974033,618.529099417949,-38.9779635031361)) ;
#58536 = CARTESIAN_POINT('Ctrl Pts',(30.5842518358638,618.525494485732,-38.9563730982209)) ;
#58537 = CARTESIAN_POINT('Ctrl Pts',(30.6507968126384,618.521959278623,-38.9313149292811)) ;
#58538 = CARTESIAN_POINT('Ctrl Pts',(30.7158218297607,618.518451812108,-38.9029228453313)) ;
#58539 = CARTESIAN_POINT('Ctrl Pts',(30.7808869631807,618.514942181708,-38.8745132452724)) ;
#58540 = CARTESIAN_POINT('Ctrl Pts',(30.8444300254264,618.511459980868,-38.8427653008565)) ;
#58541 = CARTESIAN_POINT('Ctrl Pts',(30.9060769860698,618.507944643049,-38.8078544511538)) ;
#58542 = CARTESIAN_POINT('Ctrl Pts',(30.9641619067275,618.504632425932,-38.7749607948581)) ;
#58543 = CARTESIAN_POINT('Ctrl Pts',(31.0205636933408,618.501290298965,-38.7392587848989)) ;
#58544 = CARTESIAN_POINT('Ctrl Pts',(31.0749795173423,618.497857737732,-38.7009343756282)) ;
#58545 = CARTESIAN_POINT('Ctrl Pts',(31.0784253563871,618.497640373505,-38.6985075127026)) ;
#58546 = CARTESIAN_POINT('Ctrl Pts',(31.081863249142,618.497422646641,-38.6960701328843)) ;
#58547 = CARTESIAN_POINT('Ctrl Pts',(31.0852931257368,618.49720454177,-38.6936222827423)) ;
#58548 = CARTESIAN_POINT('Ctrl Pts',(31.1220574975077,618.494866705896,-38.6673841163901)) ;
#58549 = CARTESIAN_POINT('Ctrl Pts',(31.1578988857675,618.492485205559,-38.6399441114312)) ;
#58550 = CARTESIAN_POINT('Ctrl Pts',(31.1927276901434,618.490040470431,-38.6113715191787)) ;
#58551 = CARTESIAN_POINT('Ctrl Pts',(31.1927544277232,618.490038593642,-38.6113495844044)) ;
#58552 = CARTESIAN_POINT('Ctrl Pts',(31.192781164707,618.490036716816,-38.6113276489626)) ;
#58553 = CARTESIAN_POINT('Ctrl Pts',(31.1928079010947,618.490034839953,-38.6113057128533)) ;
#58554 = CARTESIAN_POINT('Ctrl Pts',(31.2425623278416,618.486542137522,-38.5704842469339)) ;
#58555 = CARTESIAN_POINT('Ctrl Pts',(31.2904310167438,618.482911067368,-38.5271940059014)) ;
#58556 = CARTESIAN_POINT('Ctrl Pts',(31.3361841844741,618.47920671304,-38.4816560532498)) ;
#58557 = CARTESIAN_POINT('Ctrl Pts',(31.3408223115385,618.478831192241,-38.4770397431421)) ;
#58558 = CARTESIAN_POINT('Ctrl Pts',(31.3454386900853,618.478454918342,-38.4724003778938)) ;
#58559 = CARTESIAN_POINT('Ctrl Pts',(31.3500330757116,618.478077959143,-38.4677382171815)) ;
#58560 = CARTESIAN_POINT('Ctrl Pts',(31.3998725111635,618.473988743479,-38.4171635643799)) ;
#58561 = CARTESIAN_POINT('Ctrl Pts',(31.4471254874043,618.469819499512,-38.363900657135)) ;
#58562 = CARTESIAN_POINT('Ctrl Pts',(31.4915281287634,618.465644591886,-38.3082689663401)) ;
#58563 = CARTESIAN_POINT('Ctrl Pts',(31.5358759040669,618.461474842977,-38.2527060167584)) ;
#58564 = CARTESIAN_POINT('Ctrl Pts',(31.5773807165747,618.457299798004,-38.1947803216217)) ;
#58565 = CARTESIAN_POINT('Ctrl Pts',(31.6158159408338,618.453174194508,-38.1348275695914)) ;
#58566 = CARTESIAN_POINT('Ctrl Pts',(31.6542254806768,618.449051347955,-38.0749148811085)) ;
#58567 = CARTESIAN_POINT('Ctrl Pts',(31.6895696959779,618.444978045726,-38.0129779087523)) ;
#58568 = CARTESIAN_POINT('Ctrl Pts',(31.7216549625858,618.44098572889,-37.9493672717772)) ;
#58569 = CARTESIAN_POINT('Ctrl Pts',(31.7537295713231,618.436994738195,-37.8857777645605)) ;
#58570 = CARTESIAN_POINT('Ctrl Pts',(31.7825474111275,618.433084719467,-37.8205157226673)) ;
#58571 = CARTESIAN_POINT('Ctrl Pts',(31.8079462877662,618.429262372097,-37.7539464378962)) ;
#58572 = CARTESIAN_POINT('Ctrl Pts',(31.8333452633637,618.425440009834,-37.6873768937589)) ;
#58573 = CARTESIAN_POINT('Ctrl Pts',(31.8553251400435,618.421705254944,-37.619500095794)) ;
#58574 = CARTESIAN_POINT('Ctrl Pts',(31.873755684885,618.418040278261,-37.5506962471976)) ;
#58575 = CARTESIAN_POINT('Ctrl Pts',(31.8922046876711,618.414371631152,-37.4818234924653)) ;
#58576 = CARTESIAN_POINT('Ctrl Pts',(31.9070970059626,618.410772723826,-37.4120218194748)) ;
#58577 = CARTESIAN_POINT('Ctrl Pts',(31.9183366521414,618.407202886512,-37.341687609629)) ;
#58578 = CARTESIAN_POINT('Ctrl Pts',(31.9295823506379,618.403631126913,-37.2713155262622)) ;
#58579 = CARTESIAN_POINT('Ctrl Pts',(31.9371710513632,618.400088131138,-37.2004103504049)) ;
#58580 = CARTESIAN_POINT('Ctrl Pts',(31.9410459640722,618.396514187764,-37.1293841390509)) ;
#58581 = CARTESIAN_POINT('Ctrl Pts',(31.9447155325314,618.393129639294,-37.0621218380576)) ;
#58582 = CARTESIAN_POINT('Ctrl Pts',(31.945054214817,618.389716845712,-36.9947506530059)) ;
#58583 = CARTESIAN_POINT('Ctrl Pts',(31.9420526097717,618.386214585767,-36.9276337594214)) ;
#58584 = CARTESIAN_POINT('Ctrl Pts',(31.9418791901511,618.386012240495,-36.9237560386523)) ;
#58585 = CARTESIAN_POINT('Ctrl Pts',(31.9416946273324,618.385809596582,-36.919879153918)) ;
#58586 = CARTESIAN_POINT('Ctrl Pts',(31.9414989218786,618.385606642221,-36.916003170487)) ;
#58587 = CARTESIAN_POINT('Ctrl Pts',(31.9393270093727,618.383354282328,-36.8729880336002)) ;
#58588 = CARTESIAN_POINT('Ctrl Pts',(31.9357827578583,618.381063467541,-36.8300859542973)) ;
#58589 = CARTESIAN_POINT('Ctrl Pts',(31.9308737538022,618.378717381752,-36.7873942606187)) ;
#58590 = CARTESIAN_POINT('Ctrl Pts',(31.9308699800843,618.378715578236,-36.787361442066)) ;
#58591 = CARTESIAN_POINT('Ctrl Pts',(31.9308662055602,618.378713774688,-36.7873286236371)) ;
#58592 = CARTESIAN_POINT('Ctrl Pts',(31.93086243023,618.378711971107,-36.7872958053321)) ;
#58593 = CARTESIAN_POINT('Ctrl Pts',(31.9234657916981,618.375178389614,-36.7229980818359)) ;
#58594 = CARTESIAN_POINT('Ctrl Pts',(31.9129413273326,618.371510719047,-36.6589569896053)) ;
#58595 = CARTESIAN_POINT('Ctrl Pts',(31.8993521999746,618.367773903285,-36.5954889062645)) ;
#58596 = CARTESIAN_POINT('Ctrl Pts',(31.8980251491897,618.36740898329,-36.5892909093221)) ;
#58597 = CARTESIAN_POINT('Ctrl Pts',(31.896668901543,618.367043403887,-36.5830984054195)) ;
#58598 = CARTESIAN_POINT('Ctrl Pts',(31.8952835353884,618.366677225559,-36.5769117071961)) ;
#58599 = CARTESIAN_POINT('Ctrl Pts',(31.8798168048714,618.36258907781,-36.5078411629959)) ;
#58600 = CARTESIAN_POINT('Ctrl Pts',(31.8607167866845,618.358427016829,-36.4394904355047)) ;
#58601 = CARTESIAN_POINT('Ctrl Pts',(31.8381083273044,618.3542626363,-36.3722470330963)) ;
#58602 = CARTESIAN_POINT('Ctrl Pts',(31.8369080392276,618.354041548423,-36.3686770660853)) ;
#58603 = CARTESIAN_POINT('Ctrl Pts',(31.8356978697627,618.353820454007,-36.3651102298551)) ;
#58604 = CARTESIAN_POINT('Ctrl Pts',(31.8344778401687,618.353599363767,-36.3615465855829)) ;
#58605 = CARTESIAN_POINT('Ctrl Pts',(31.8114027137413,618.349417755992,-36.2941453171842)) ;
#58606 = CARTESIAN_POINT('Ctrl Pts',(31.7847980465032,618.345237848864,-36.2278817047819)) ;
#58607 = CARTESIAN_POINT('Ctrl Pts',(31.7548259193759,618.341112089252,-36.1631277835381)) ;
#58608 = CARTESIAN_POINT('Ctrl Pts',(31.7248736523755,618.336989063449,-36.0984167695291)) ;
#58609 = CARTESIAN_POINT('Ctrl Pts',(31.6915585194135,618.332920271387,-36.035213352281)) ;
#58610 = CARTESIAN_POINT('Ctrl Pts',(31.6550728830991,618.328934767944,-35.9738700195009)) ;
#58611 = CARTESIAN_POINT('Ctrl Pts',(31.6185971393183,618.324950345112,-35.9125433190463)) ;
#58612 = CARTESIAN_POINT('Ctrl Pts',(31.578952627417,618.321049198024,-35.8530756978182)) ;
#58613 = CARTESIAN_POINT('Ctrl Pts',(31.5363610872593,618.317235683044,-35.7958012323473)) ;
#58614 = CARTESIAN_POINT('Ctrl Pts',(31.5300565508543,618.316671194323,-35.7873232822356)) ;
#58615 = CARTESIAN_POINT('Ctrl Pts',(31.5236874952941,618.316108581474,-35.7788933533313)) ;
#58616 = CARTESIAN_POINT('Ctrl Pts',(31.5172546949865,618.315547812711,-35.7705124947133)) ;
#58617 = CARTESIAN_POINT('',(27.9033532997491,618.710565160563,-37.5523303889371)) ;
#58618 = CARTESIAN_POINT('Ctrl Pts',(27.9033532997491,618.710565160563,-37.5523303889371)) ;
#58619 = CARTESIAN_POINT('Ctrl Pts',(27.9220878244754,618.70662834087,-37.6224801187498)) ;
#58620 = CARTESIAN_POINT('Ctrl Pts',(27.9445626526125,618.702691521177,-37.6917023881676)) ;
#58621 = CARTESIAN_POINT('Ctrl Pts',(27.9706629726565,618.698754701484,-37.75958320921)) ;
#58622 = CARTESIAN_POINT('Ctrl Pts',(27.9967424465814,618.694821026098,-37.827409814378)) ;
#58623 = CARTESIAN_POINT('Ctrl Pts',(28.0264414901395,618.690887350711,-37.8938966728783)) ;
#58624 = CARTESIAN_POINT('Ctrl Pts',(28.0595959262627,618.686953675325,-37.9586463714965)) ;
#58625 = CARTESIAN_POINT('Ctrl Pts',(28.0927405975631,618.683021158506,-38.0233769996852)) ;
#58626 = CARTESIAN_POINT('Ctrl Pts',(28.1293384354892,618.679088641687,-38.0863710722528)) ;
#58627 = CARTESIAN_POINT('Ctrl Pts',(28.1691782036139,618.675156124868,-38.1472535582005)) ;
#58628 = CARTESIAN_POINT('Ctrl Pts',(28.2090135524799,618.671224044266,-38.2081292907088)) ;
#58629 = CARTESIAN_POINT('Ctrl Pts',(28.252089864984,618.667291963665,-38.2668935165893)) ;
#58630 = CARTESIAN_POINT('Ctrl Pts',(28.2981520624203,618.663359883063,-38.3231994221628)) ;
#58631 = CARTESIAN_POINT('Ctrl Pts',(28.3442221609708,618.659427127986,-38.3795149859682)) ;
#58632 = CARTESIAN_POINT('Ctrl Pts',(28.3932788704584,618.65549437291,-38.4333710351295)) ;
#58633 = CARTESIAN_POINT('Ctrl Pts',(28.4450271473054,618.651561617833,-38.4844542366308)) ;
#58634 = CARTESIAN_POINT('Ctrl Pts',(28.4967989193162,618.647627077175,-38.5355606313331)) ;
#58635 = CARTESIAN_POINT('Ctrl Pts',(28.5512643595028,618.643692536518,-38.5838913532303)) ;
#58636 = CARTESIAN_POINT('Ctrl Pts',(28.6080929788375,618.63975799586,-38.6291712726249)) ;
#58637 = CARTESIAN_POINT('Ctrl Pts',(28.6650058778057,618.635817620086,-38.6745183443638)) ;
#58638 = CARTESIAN_POINT('Ctrl Pts',(28.7242885905112,618.631877244311,-38.716805295332)) ;
#58639 = CARTESIAN_POINT('Ctrl Pts',(28.7855794506329,618.627936868536,-38.7557987979462)) ;
#58640 = CARTESIAN_POINT('Ctrl Pts',(28.846921413001,618.62399320741,-38.7948248120241)) ;
#58641 = CARTESIAN_POINT('Ctrl Pts',(28.9102744564937,618.620049546283,-38.8305516828078)) ;
#58642 = CARTESIAN_POINT('Ctrl Pts',(28.9752522709954,618.616105885156,-38.8627920440992)) ;
#58643 = CARTESIAN_POINT('Ctrl Pts',(29.0403539253724,618.612154707887,-38.8950938516296)) ;
#58644 = CARTESIAN_POINT('Ctrl Pts',(29.1070861114417,618.608203530619,-38.9238956989972)) ;
#58645 = CARTESIAN_POINT('Ctrl Pts',(29.175042912625,618.604252353349,-38.9490584895437)) ;
#58646 = CARTESIAN_POINT('Ctrl Pts',(29.2031889328429,618.602615873801,-38.9594802927941)) ;
#58647 = CARTESIAN_POINT('Ctrl Pts',(29.2315448569522,618.600979394253,-38.9692784442526)) ;
#58648 = CARTESIAN_POINT('Ctrl Pts',(29.260081250212,618.599342914705,-38.9784456100224)) ;
#58649 = CARTESIAN_POINT('Ctrl Pts',(29.339438239858,618.594792021066,-39.0039386242396)) ;
#58650 = CARTESIAN_POINT('Ctrl Pts',(29.4204345692865,618.590241127427,-39.024626781518)) ;
#58651 = CARTESIAN_POINT('Ctrl Pts',(29.5025292142112,618.585690233788,-39.0403283483533)) ;
#58652 = CARTESIAN_POINT('Ctrl Pts',(29.5837422767609,618.581188210421,-39.055861302186)) ;
#58653 = CARTESIAN_POINT('Ctrl Pts',(29.6660300767945,618.576686187055,-39.0665141037531)) ;
#58654 = CARTESIAN_POINT('Ctrl Pts',(29.748847668175,618.572184163688,-39.0721570185904)) ;
#58655 = CARTESIAN_POINT('Ctrl Pts',(29.7951029245638,618.569669694942,-39.0753086976989)) ;
#58656 = CARTESIAN_POINT('Ctrl Pts',(29.841523075707,618.567155226197,-39.0768984062664)) ;
#58657 = CARTESIAN_POINT('Ctrl Pts',(29.8880104657039,618.564640757452,-39.076910106671)) ;
#58658 = CARTESIAN_POINT('',(27.9019744556529,618.709370847142,-36.4891342933297)) ;
#58659 = CARTESIAN_POINT('Origin',(29.888527625422,618.710565160562,-37.0221601717529)) ;
#58660 = CARTESIAN_POINT('Ctrl Pts',(27.9039518707378,618.708167248319,-36.4897537138475)) ;
#58661 = CARTESIAN_POINT('Ctrl Pts',(27.8958179074389,618.706470116412,-36.5200735308083)) ;
#58662 = CARTESIAN_POINT('Ctrl Pts',(27.88837934808,618.704812394634,-36.5505776028213)) ;
#58663 = CARTESIAN_POINT('Ctrl Pts',(27.8431917212744,618.693893956545,-36.7562537906378)) ;
#58664 = CARTESIAN_POINT('Ctrl Pts',(27.8277943162262,618.685565557881,-36.9355616976458)) ;
#58665 = CARTESIAN_POINT('Ctrl Pts',(27.8388765563881,618.673437805429,-37.1816200139386)) ;
#58666 = CARTESIAN_POINT('Ctrl Pts',(27.8451738759113,618.670081227285,-37.2484375402449)) ;
#58667 = CARTESIAN_POINT('Ctrl Pts',(27.8623906949846,618.663861917327,-37.3680818838262)) ;
#58668 = CARTESIAN_POINT('Ctrl Pts',(27.8721429166722,618.661035685576,-37.4210144017641)) ;
#58669 = CARTESIAN_POINT('Ctrl Pts',(27.8954255044598,618.655334774255,-37.5244209105406)) ;
#58670 = CARTESIAN_POINT('Ctrl Pts',(27.9088257985101,618.652466219825,-37.5748824270022)) ;
#58671 = CARTESIAN_POINT('Ctrl Pts',(27.975471419218,618.639712439912,-37.7921325404838)) ;
#58672 = CARTESIAN_POINT('Ctrl Pts',(28.047981516357,618.629174682059,-37.9522201124276)) ;
#58673 = CARTESIAN_POINT('Ctrl Pts',(28.1835046356398,618.613742648858,-38.1718545375616)) ;
#58674 = CARTESIAN_POINT('Ctrl Pts',(28.2313858534902,618.60882149254,-38.2398563278635)) ;
#58675 = CARTESIAN_POINT('Ctrl Pts',(28.3031600493299,618.602299103636,-38.3296860172536)) ;
#58676 = CARTESIAN_POINT('Ctrl Pts',(28.3236417151513,618.600522194517,-38.3541311144503)) ;
#58677 = CARTESIAN_POINT('Ctrl Pts',(28.3666148543829,618.596979225372,-38.4030596555268)) ;
#58678 = CARTESIAN_POINT('Ctrl Pts',(28.3891479676044,618.595216809177,-38.4274938656349)) ;
#58679 = CARTESIAN_POINT('Ctrl Pts',(28.5045482544813,618.586590899946,-38.5466931796163)) ;
#58680 = CARTESIAN_POINT('Ctrl Pts',(28.605856823879,618.58024870474,-38.632862847615)) ;
#58681 = CARTESIAN_POINT('Ctrl Pts',(28.7835397226048,618.569773646303,-38.756523992888)) ;
#58682 = CARTESIAN_POINT('Ctrl Pts',(28.855162398266,618.565701365462,-38.800128514935)) ;
#58683 = CARTESIAN_POINT('Ctrl Pts',(28.9878582775255,618.558183348016,-38.8701822298659)) ;
#58684 = CARTESIAN_POINT('Ctrl Pts',(29.0479313401398,618.554789699881,-38.8982698529416)) ;
#58685 = CARTESIAN_POINT('Ctrl Pts',(29.1550666372187,618.548684366271,-38.9421820553266)) ;
#58686 = CARTESIAN_POINT('Ctrl Pts',(29.2015408390967,618.54601977539,-38.9592966206159)) ;
#58687 = CARTESIAN_POINT('Ctrl Pts',(29.3094224135293,618.53977884292,-38.9946543935931)) ;
#58688 = CARTESIAN_POINT('Ctrl Pts',(29.3711529176067,618.536167017023,-39.0117376272822)) ;
#58689 = CARTESIAN_POINT('Ctrl Pts',(29.5767931540427,618.52400380586,-39.0584282827151)) ;
#58690 = CARTESIAN_POINT('Ctrl Pts',(29.7230742455795,618.515108820438,-39.0754947541036)) ;
#58691 = CARTESIAN_POINT('Ctrl Pts',(29.946364551797,618.501773289585,-39.0775188879853)) ;
#58692 = CARTESIAN_POINT('Ctrl Pts',(30.0228129104608,618.497259917235,-39.0739432896319)) ;
#58693 = CARTESIAN_POINT('Ctrl Pts',(30.130186690606,618.491143140938,-39.0628924800165)) ;
#58694 = CARTESIAN_POINT('Ctrl Pts',(30.1614084544824,618.48939165761,-39.058952708263)) ;
#58695 = CARTESIAN_POINT('Ctrl Pts',(30.225550993546,618.485866526515,-39.0493571541161)) ;
#58696 = CARTESIAN_POINT('Ctrl Pts',(30.2584488989828,618.484097910884,-39.0436128409586)) ;
#58697 = CARTESIAN_POINT('Ctrl Pts',(30.3993793160701,618.47663573984,-39.0154487994423)) ;
#58698 = CARTESIAN_POINT('Ctrl Pts',(30.5056588163018,618.471293284236,-38.985148445248)) ;
#58699 = CARTESIAN_POINT('Ctrl Pts',(30.7353702442326,618.459437023411,-38.8991426898609)) ;
#58700 = CARTESIAN_POINT('Ctrl Pts',(30.8567623873737,618.452941103242,-38.8394999771351)) ;
#58701 = CARTESIAN_POINT('Ctrl Pts',(31.0178742086254,618.443239053318,-38.7395886487558)) ;
#58702 = CARTESIAN_POINT('Ctrl Pts',(31.0631484118104,618.440383012865,-38.7089469261163)) ;
#58703 = CARTESIAN_POINT('Ctrl Pts',(31.1476668531352,618.434761371185,-38.6466905375196)) ;
#58704 = CARTESIAN_POINT('Ctrl Pts',(31.1870754443988,618.432008503317,-38.6153655663368)) ;
#58705 = CARTESIAN_POINT('Ctrl Pts',(31.2903263522578,618.424414368095,-38.5269163189289)) ;
#58706 = CARTESIAN_POINT('Ctrl Pts',(31.3518070189032,618.419467094685,-38.4672004187941)) ;
#58707 = CARTESIAN_POINT('Ctrl Pts',(31.5081110369865,618.405731835566,-38.2951512308979)) ;
#58708 = CARTESIAN_POINT('Ctrl Pts',(31.5949044640117,618.396740376852,-38.1762104052946)) ;
#58709 = CARTESIAN_POINT('Ctrl Pts',(31.6927471383449,618.385249498457,-38.0066328793852)) ;
#58710 = CARTESIAN_POINT('Ctrl Pts',(31.7156934082364,618.382424981604,-37.9633617987878)) ;
#58711 = CARTESIAN_POINT('Ctrl Pts',(31.7496755570405,618.378069848645,-37.8933427075535)) ;
#58712 = CARTESIAN_POINT('Ctrl Pts',(31.7617294867282,618.376486041313,-37.867113266449)) ;
#58713 = CARTESIAN_POINT('Ctrl Pts',(31.7892528263317,618.372776351983,-37.8037352263525)) ;
#58714 = CARTESIAN_POINT('Ctrl Pts',(31.8041910090192,618.370679291382,-37.7663712314253)) ;
#58715 = CARTESIAN_POINT('Ctrl Pts',(31.8559218303672,618.362997297284,-37.6250771314038)) ;
#58716 = CARTESIAN_POINT('Ctrl Pts',(31.8854319324121,618.357697657238,-37.5186738273582)) ;
#58717 = CARTESIAN_POINT('Ctrl Pts',(31.9302028257196,618.346233571352,-37.2859991857726)) ;
#58718 = CARTESIAN_POINT('Ctrl Pts',(31.9425826302037,618.340072427152,-37.1596482204033)) ;
#58719 = CARTESIAN_POINT('Ctrl Pts',(31.9435270491102,618.330824856966,-36.980163630891)) ;
#58720 = CARTESIAN_POINT('Ctrl Pts',(31.9417689953612,618.328047330032,-36.9273680621678)) ;
#58721 = CARTESIAN_POINT('Ctrl Pts',(31.9342531081693,618.322408310355,-36.8229084803561)) ;
#58722 = CARTESIAN_POINT('Ctrl Pts',(31.9285648533262,618.31955107272,-36.771278926938)) ;
#58723 = CARTESIAN_POINT('Ctrl Pts',(31.9053256584369,618.310672494464,-36.6150063341292)) ;
#58724 = CARTESIAN_POINT('Ctrl Pts',(31.8816250186065,618.304462782732,-36.5114681674261)) ;
#58725 = CARTESIAN_POINT('Ctrl Pts',(31.8054832463598,618.289193611457,-36.2673978465648)) ;
#58726 = CARTESIAN_POINT('Ctrl Pts',(31.7454550690875,618.280040289192,-36.1298552521645)) ;
#58727 = CARTESIAN_POINT('Ctrl Pts',(31.6543331744273,618.269578237659,-35.9709447421512)) ;
#58728 = CARTESIAN_POINT('Ctrl Pts',(31.6369330476907,618.267695948273,-35.9422518920512)) ;
#58729 = CARTESIAN_POINT('Ctrl Pts',(31.6045713756217,618.264411402832,-35.8917217301505)) ;
#58730 = CARTESIAN_POINT('Ctrl Pts',(31.589876761326,618.262993049718,-35.8697243130972)) ;
#58731 = CARTESIAN_POINT('Ctrl Pts',(31.5563615310839,618.259901609559,-35.8215917999241)) ;
#58732 = CARTESIAN_POINT('Ctrl Pts',(31.5373483985618,618.258240915251,-35.7956102882554)) ;
#58733 = CARTESIAN_POINT('Ctrl Pts',(31.5177255210653,618.256605597192,-35.7700771955364)) ;
#58734 = CARTESIAN_POINT('Origin',(29.8885276254218,617.710565160562,-37.0221601717529)) ;
#58735 = CARTESIAN_POINT('',(30.4641350798567,616.842375533648,-38.5858337721774)) ;
#58736 = CARTESIAN_POINT('',(30.4640776578153,616.710565160562,-38.5855853091393)) ;
#58737 = CARTESIAN_POINT('',(30.4640776578155,617.710565160562,-38.5855853091393)) ;
#58738 = CARTESIAN_POINT('',(31.5536749489399,616.710572711416,-37.0981817538183)) ;
#58739 = CARTESIAN_POINT('Origin',(29.8885276254216,616.710565160562,-37.0221601717529)) ;
#58740 = CARTESIAN_POINT('Ctrl Pts',(31.5536749650872,616.710572711554,-37.0981817545555)) ;
#58741 = CARTESIAN_POINT('Ctrl Pts',(31.5512370248751,616.714176385986,-37.1509048318303)) ;
#58742 = CARTESIAN_POINT('Ctrl Pts',(31.5462328618462,616.717877019601,-37.2035994968077)) ;
#58743 = CARTESIAN_POINT('Ctrl Pts',(31.538695327451,616.721620562842,-37.2559981327892)) ;
#58744 = CARTESIAN_POINT('Ctrl Pts',(31.5300852276339,616.725896799511,-37.3158529158553)) ;
#58745 = CARTESIAN_POINT('Ctrl Pts',(31.5181691960903,616.730228465095,-37.375322665228)) ;
#58746 = CARTESIAN_POINT('Ctrl Pts',(31.5030344968599,616.734549424273,-37.434030310495)) ;
#58747 = CARTESIAN_POINT('Ctrl Pts',(31.4879152270166,616.738865978358,-37.4926781050199)) ;
#58748 = CARTESIAN_POINT('Ctrl Pts',(31.4695841279748,616.74317154987,-37.5505654863396)) ;
#58749 = CARTESIAN_POINT('Ctrl Pts',(31.448162912522,616.747420965115,-37.6073326424816)) ;
#58750 = CARTESIAN_POINT('Ctrl Pts',(31.4267554075257,616.75166766056,-37.6640634653153)) ;
#58751 = CARTESIAN_POINT('Ctrl Pts',(31.4022618303736,616.755858153465,-37.719675546723)) ;
#58752 = CARTESIAN_POINT('Ctrl Pts',(31.3748356773251,616.759971151056,-37.7738244111941)) ;
#58753 = CARTESIAN_POINT('Ctrl Pts',(31.3474166723935,616.764083076671,-37.8279591627703)) ;
#58754 = CARTESIAN_POINT('Ctrl Pts',(31.3170665926437,616.768117556839,-37.8806314084233)) ;
#58755 = CARTESIAN_POINT('Ctrl Pts',(31.2839704058503,616.772077891308,-37.9315116012041)) ;
#58756 = CARTESIAN_POINT('Ctrl Pts',(31.2508463402738,616.776041561791,-37.9824346532384)) ;
#58757 = CARTESIAN_POINT('Ctrl Pts',(31.2149714186435,616.779931085611,-38.0315624785175)) ;
#58758 = CARTESIAN_POINT('Ctrl Pts',(31.176563855066,616.783773406977,-38.0785809200733)) ;
#58759 = CARTESIAN_POINT('Ctrl Pts',(31.1381418667361,616.787617171407,-38.1256170203741)) ;
#58760 = CARTESIAN_POINT('Ctrl Pts',(31.0971851356059,616.791413971087,-38.1705418763009)) ;
#58761 = CARTESIAN_POINT('Ctrl Pts',(31.053947309258,616.795211484728,-38.2130603820457)) ;
#58762 = CARTESIAN_POINT('Ctrl Pts',(31.0106273634846,616.799016210796,-38.2556596410467)) ;
#58763 = CARTESIAN_POINT('Ctrl Pts',(30.9650173952862,616.802822127504,-38.2958429243228)) ;
#58764 = CARTESIAN_POINT('Ctrl Pts',(30.9174112921772,616.806692422931,-38.3333384864927)) ;
#58765 = CARTESIAN_POINT('Ctrl Pts',(30.8746328984004,616.810170233779,-38.3670316438535)) ;
#58766 = CARTESIAN_POINT('Ctrl Pts',(30.8302424171979,616.813700617628,-38.3985548429725)) ;
#58767 = CARTESIAN_POINT('Ctrl Pts',(30.7844840289367,616.817333919169,-38.4277331502955)) ;
#58768 = CARTESIAN_POINT('Ctrl Pts',(30.7803901276804,616.817658982579,-38.4303436685752)) ;
#58769 = CARTESIAN_POINT('Ctrl Pts',(30.7762852659941,616.817984869793,-38.43293544994)) ;
#58770 = CARTESIAN_POINT('Ctrl Pts',(30.7721696117842,616.818311616863,-38.435508388295)) ;
#58771 = CARTESIAN_POINT('Ctrl Pts',(30.7721416414912,616.81831383746,-38.4355258741759)) ;
#58772 = CARTESIAN_POINT('Ctrl Pts',(30.7721136706998,616.818316058097,-38.4355433591866)) ;
#58773 = CARTESIAN_POINT('Ctrl Pts',(30.77208569941,616.818318278774,-38.435560843327)) ;
#58774 = CARTESIAN_POINT('Ctrl Pts',(30.7243139528887,616.822110939553,-38.4654217445811)) ;
#58775 = CARTESIAN_POINT('Ctrl Pts',(30.6749216910435,616.826028826852,-38.4928388875168)) ;
#58776 = CARTESIAN_POINT('Ctrl Pts',(30.6241889147218,616.830006671409,-38.5176738823377)) ;
#58777 = CARTESIAN_POINT('Ctrl Pts',(30.6187932154843,616.830429736229,-38.5203152154626)) ;
#58778 = CARTESIAN_POINT('Ctrl Pts',(30.6133824015965,616.830853479251,-38.5229273434151)) ;
#58779 = CARTESIAN_POINT('Ctrl Pts',(30.6079568443994,616.831277821956,-38.525510102549)) ;
#58780 = CARTESIAN_POINT('Ctrl Pts',(30.5610484595922,616.834946612124,-38.5478401702115)) ;
#58781 = CARTESIAN_POINT('Ctrl Pts',(30.5130337497002,616.83866013173,-38.5679758101255)) ;
#58782 = CARTESIAN_POINT('Ctrl Pts',(30.4641350798567,616.842375533648,-38.5858337721774)) ;
#58783 = CARTESIAN_POINT('Origin',(29.8885276254218,617.710565160562,-37.0221601717529)) ;
#58784 = CARTESIAN_POINT('',(30.464077664741,617.544128797339,-38.5855853065898)) ;
#58785 = CARTESIAN_POINT('',(30.4640668826956,617.349683543251,-38.5855644985231)) ;
#58786 = CARTESIAN_POINT('',(30.4640776578155,617.710565160562,-38.5855853091393)) ;
#58787 = CARTESIAN_POINT('',(29.5692971707939,616.710565160562,-38.6572894990045)) ;
#58788 = CARTESIAN_POINT('Ctrl Pts',(30.4640668826956,617.349683543251,-38.5855644985231)) ;
#58789 = CARTESIAN_POINT('Ctrl Pts',(30.521084074564,617.345357786454,-38.5644138620552)) ;
#58790 = CARTESIAN_POINT('Ctrl Pts',(30.5769971533066,617.341054683646,-38.5401308190164)) ;
#58791 = CARTESIAN_POINT('Ctrl Pts',(30.6314596324945,617.336815163341,-38.5128750276002)) ;
#58792 = CARTESIAN_POINT('Ctrl Pts',(30.6858946674952,617.332577779371,-38.4856329706495)) ;
#58793 = CARTESIAN_POINT('Ctrl Pts',(30.738880611153,617.328404005497,-38.4554212210874)) ;
#58794 = CARTESIAN_POINT('Ctrl Pts',(30.790088868766,617.324310413416,-38.4224293693333)) ;
#58795 = CARTESIAN_POINT('Ctrl Pts',(30.8412903621481,617.320217362068,-38.3894418755581)) ;
#58796 = CARTESIAN_POINT('Ctrl Pts',(30.8907145741679,617.316204439522,-38.3536749709813)) ;
#58797 = CARTESIAN_POINT('Ctrl Pts',(30.938050556099,617.312263488549,-38.3153482541213)) ;
#58798 = CARTESIAN_POINT('Ctrl Pts',(30.9854321660804,617.308318738819,-38.2769845934124)) ;
#58799 = CARTESIAN_POINT('Ctrl Pts',(31.0307213402496,617.304445949604,-38.2360560544996)) ;
#58800 = CARTESIAN_POINT('Ctrl Pts',(31.073625597012,617.300613507346,-38.1928143189112)) ;
#58801 = CARTESIAN_POINT('Ctrl Pts',(31.1165502658891,617.296779241766,-38.1495520106492)) ;
#58802 = CARTESIAN_POINT('Ctrl Pts',(31.1570874286128,617.292985051796,-38.1039741089672)) ;
#58803 = CARTESIAN_POINT('Ctrl Pts',(31.1949672362993,617.289179237764,-38.0563665633609)) ;
#58804 = CARTESIAN_POINT('Ctrl Pts',(31.2329185155416,617.285366242928,-38.0086691919196)) ;
#58805 = CARTESIAN_POINT('Ctrl Pts',(31.2682018582335,617.281541054248,-37.9589342907223)) ;
#58806 = CARTESIAN_POINT('Ctrl Pts',(31.3005754213143,617.27763777361,-37.9074866807826)) ;
#58807 = CARTESIAN_POINT('Ctrl Pts',(31.3266538243606,617.274493500445,-37.8660432503999)) ;
#58808 = CARTESIAN_POINT('Ctrl Pts',(31.3508444137161,617.271298092349,-37.8234891432328)) ;
#58809 = CARTESIAN_POINT('Ctrl Pts',(31.3730391559108,617.268014866734,-37.7800128089943)) ;
#58810 = CARTESIAN_POINT('Ctrl Pts',(31.3730527461205,617.26801285636,-37.7799861877119)) ;
#58811 = CARTESIAN_POINT('Ctrl Pts',(31.3730663355829,617.268010845954,-37.7799595660834)) ;
#58812 = CARTESIAN_POINT('Ctrl Pts',(31.373079924298,617.268008835514,-37.7799329441086)) ;
#58813 = CARTESIAN_POINT('Ctrl Pts',(31.3982667605873,617.264282463299,-37.7305888145781)) ;
#58814 = CARTESIAN_POINT('Ctrl Pts',(31.4209704355625,617.260433120364,-37.6798714193184)) ;
#58815 = CARTESIAN_POINT('Ctrl Pts',(31.4410752479256,617.256523934734,-37.6280657443909)) ;
#58816 = CARTESIAN_POINT('Ctrl Pts',(31.4429546632665,617.256158500663,-37.6232229048535)) ;
#58817 = CARTESIAN_POINT('Ctrl Pts',(31.444811375854,617.255792543645,-37.6183705919803)) ;
#58818 = CARTESIAN_POINT('Ctrl Pts',(31.4466452965835,617.255426115251,-37.6135090611418)) ;
#58819 = CARTESIAN_POINT('Ctrl Pts',(31.4683648172353,617.251086424368,-37.5559328978146)) ;
#58820 = CARTESIAN_POINT('Ctrl Pts',(31.4868866525301,617.24668128716,-37.49705784101)) ;
#58821 = CARTESIAN_POINT('Ctrl Pts',(31.5021029317602,617.242282244052,-37.4372768729893)) ;
#58822 = CARTESIAN_POINT('Ctrl Pts',(31.5170903328867,617.237949369855,-37.3783951099837)) ;
#58823 = CARTESIAN_POINT('Ctrl Pts',(31.5288713222752,617.233622692847,-37.3186344993347)) ;
#58824 = CARTESIAN_POINT('Ctrl Pts',(31.5373819205906,617.229350066148,-37.2583721573177)) ;
#58825 = CARTESIAN_POINT('Ctrl Pts',(31.5458873163396,617.225080051326,-37.1981466539369)) ;
#58826 = CARTESIAN_POINT('Ctrl Pts',(31.5511264474828,617.220864156217,-37.1374200208457)) ;
#58827 = CARTESIAN_POINT('Ctrl Pts',(31.5530707022731,617.216726391994,-37.0765703636333)) ;
#58828 = CARTESIAN_POINT('Ctrl Pts',(31.5550144937777,617.212589613735,-37.0157352059442)) ;
#58829 = CARTESIAN_POINT('Ctrl Pts',(31.5536649485285,617.208530932296,-36.9547771031583)) ;
#58830 = CARTESIAN_POINT('Ctrl Pts',(31.5490280296545,617.204549585729,-36.8940755273518)) ;
#58831 = CARTESIAN_POINT('Ctrl Pts',(31.5442614473403,617.200456907669,-36.8316765366528)) ;
#58832 = CARTESIAN_POINT('Ctrl Pts',(31.5360207133408,617.19644594262,-36.769548687579)) ;
#58833 = CARTESIAN_POINT('Ctrl Pts',(31.5243519731096,617.192489520133,-36.7081052790211)) ;
#58834 = CARTESIAN_POINT('Ctrl Pts',(31.5129859546677,617.188635739,-36.6482558950284)) ;
#58835 = CARTESIAN_POINT('Ctrl Pts',(31.4983673621653,617.184833340402,-36.5890560367305)) ;
#58836 = CARTESIAN_POINT('Ctrl Pts',(31.4805789942823,617.181035702797,-36.5308871793491)) ;
#58837 = CARTESIAN_POINT('Ctrl Pts',(31.4620799650653,617.177086346146,-36.4703944236729)) ;
#58838 = CARTESIAN_POINT('Ctrl Pts',(31.4401520065572,617.173141723026,-36.4110170374954)) ;
#58839 = CARTESIAN_POINT('Ctrl Pts',(31.4149400476954,617.169131324949,-36.3531800309747)) ;
#58840 = CARTESIAN_POINT('Ctrl Pts',(31.3931141943669,617.165659545517,-36.3031108543509)) ;
#58841 = CARTESIAN_POINT('Ctrl Pts',(31.3688269891719,617.162137815671,-36.2541951552217)) ;
#58842 = CARTESIAN_POINT('Ctrl Pts',(31.3422116372834,617.15851533858,-36.2067052002401)) ;
#58843 = CARTESIAN_POINT('Ctrl Pts',(31.3380974627472,617.157955379686,-36.1993642503878)) ;
#58844 = CARTESIAN_POINT('Ctrl Pts',(31.3339276743812,617.15739301347,-36.1920572681479)) ;
#58845 = CARTESIAN_POINT('Ctrl Pts',(31.3297027792135,617.156828052308,-36.1847851486677)) ;
#58846 = CARTESIAN_POINT('Ctrl Pts',(31.3296873928244,617.156825994811,-36.1847586647773)) ;
#58847 = CARTESIAN_POINT('Ctrl Pts',(31.3296720057043,617.156823937278,-36.1847321813494)) ;
#58848 = CARTESIAN_POINT('Ctrl Pts',(31.3296566178535,617.156821879712,-36.1847056983838)) ;
#58849 = CARTESIAN_POINT('Ctrl Pts',(31.3017663989003,617.153092575127,-36.1367057718919)) ;
#58850 = CARTESIAN_POINT('Ctrl Pts',(31.2713681144063,617.149240376061,-36.090056891097)) ;
#58851 = CARTESIAN_POINT('Ctrl Pts',(31.238639778123,617.145328386154,-36.0450113303155)) ;
#58852 = CARTESIAN_POINT('Ctrl Pts',(31.2355817960872,617.144962868189,-36.0408024846696)) ;
#58853 = CARTESIAN_POINT('Ctrl Pts',(31.2325035074693,617.144596828241,-36.0366076495894)) ;
#58854 = CARTESIAN_POINT('Ctrl Pts',(31.2294050793384,617.144230317784,-36.0324270385321)) ;
#58855 = CARTESIAN_POINT('Ctrl Pts',(31.1927794812004,617.139897906588,-35.9830092776272)) ;
#58856 = CARTESIAN_POINT('Ctrl Pts',(31.1533343681168,617.135500412305,-35.9355765055245)) ;
#58857 = CARTESIAN_POINT('Ctrl Pts',(31.1113410921262,617.131108789479,-35.890430876453)) ;
#58858 = CARTESIAN_POINT('Ctrl Pts',(31.0698813712581,617.126772965416,-35.8458588554433)) ;
#58859 = CARTESIAN_POINT('Ctrl Pts',(31.0259380743513,617.122443157015,-35.8035158665467)) ;
#58860 = CARTESIAN_POINT('Ctrl Pts',(30.9797947503753,617.118167100219,-35.7636606684064)) ;
#58861 = CARTESIAN_POINT('Ctrl Pts',(30.9336795843829,617.113893652795,-35.7238297910543)) ;
#58862 = CARTESIAN_POINT('Ctrl Pts',(30.8853671327275,617.109674026449,-35.6864835511092)) ;
#58863 = CARTESIAN_POINT('Ctrl Pts',(30.8351608804874,617.105532053112,-35.6518515018267)) ;
#58864 = CARTESIAN_POINT('Ctrl Pts',(30.7849667375342,617.10139107878,-35.6172278054765)) ;
#58865 = CARTESIAN_POINT('Ctrl Pts',(30.7328797036994,617.09732772183,-35.5853170260124)) ;
#58866 = CARTESIAN_POINT('Ctrl Pts',(30.6792231421848,617.093340991862,-35.5563204134524)) ;
#58867 = CARTESIAN_POINT('Ctrl Pts',(30.6242918057594,617.089259544991,-35.5266348981162)) ;
#58868 = CARTESIAN_POINT('Ctrl Pts',(30.5677153525766,617.085258382378,-35.5000039746551)) ;
#58869 = CARTESIAN_POINT('Ctrl Pts',(30.5098629151243,617.081310449078,-35.4766113274609)) ;
#58870 = CARTESIAN_POINT('Ctrl Pts',(30.4532818035698,617.077449272881,-35.4537327412035)) ;
#58871 = CARTESIAN_POINT('Ctrl Pts',(30.3954802001303,617.073638658514,-35.4339518764798)) ;
#58872 = CARTESIAN_POINT('Ctrl Pts',(30.336824880697,617.069831848933,-35.4174066351672)) ;
#58873 = CARTESIAN_POINT('Ctrl Pts',(30.2761926640822,617.06589673605,-35.4003037591639)) ;
#58874 = CARTESIAN_POINT('Ctrl Pts',(30.2146480804883,617.061965258915,-35.3866591106143)) ;
#58875 = CARTESIAN_POINT('Ctrl Pts',(30.1526206363921,617.057968154435,-35.3765801825369)) ;
#58876 = CARTESIAN_POINT('Ctrl Pts',(30.0986360186937,617.054489336947,-35.3678081448204)) ;
#58877 = CARTESIAN_POINT('Ctrl Pts',(30.0442847846414,617.050960158838,-35.3617368033136)) ;
#58878 = CARTESIAN_POINT('Ctrl Pts',(29.9898683199497,617.04733002798,-35.3584023356605)) ;
#58879 = CARTESIAN_POINT('Ctrl Pts',(29.9817940159459,617.046791389899,-35.3579075680258)) ;
#58880 = CARTESIAN_POINT('Ctrl Pts',(29.9737182064909,617.046250529185,-35.3574729939872)) ;
#58881 = CARTESIAN_POINT('Ctrl Pts',(29.9656418017626,617.045707280564,-35.3570986677741)) ;
#58882 = CARTESIAN_POINT('Ctrl Pts',(29.9656089326697,617.045705069668,-35.3570971443533)) ;
#58883 = CARTESIAN_POINT('Ctrl Pts',(29.9655760635669,617.045702858733,-35.3570956219304)) ;
#58884 = CARTESIAN_POINT('Ctrl Pts',(29.9655431944543,617.045700647758,-35.3570941005052)) ;
#58885 = CARTESIAN_POINT('Ctrl Pts',(29.9100643951679,617.041968808823,-35.3545261321799)) ;
#58886 = CARTESIAN_POINT('Ctrl Pts',(29.8543607837217,617.038114620666,-35.3548001091035)) ;
#58887 = CARTESIAN_POINT('Ctrl Pts',(29.7987417927496,617.034201555736,-35.357903173981)) ;
#58888 = CARTESIAN_POINT('Ctrl Pts',(29.7936860654379,617.033845860876,-35.3581852404043)) ;
#58889 = CARTESIAN_POINT('Ctrl Pts',(29.78863106613,617.033489679535,-35.3584906618042)) ;
#58890 = CARTESIAN_POINT('Ctrl Pts',(29.7835770441503,617.033133059386,-35.3588194156066)) ;
#58891 = CARTESIAN_POINT('Ctrl Pts',(29.7221734369149,617.028800319321,-35.3628135947849)) ;
#58892 = CARTESIAN_POINT('Ctrl Pts',(29.6609090204286,617.024403469515,-35.3702550211247)) ;
#58893 = CARTESIAN_POINT('Ctrl Pts',(29.6001859470569,617.02001353235,-35.381079378202)) ;
#58894 = CARTESIAN_POINT('Ctrl Pts',(29.5403647077876,617.015688792726,-35.3917429763815)) ;
#58895 = CARTESIAN_POINT('Ctrl Pts',(29.4810686797287,617.011371040941,-35.4056893581065)) ;
#58896 = CARTESIAN_POINT('Ctrl Pts',(29.4226677322369,617.007107434284,-35.4228208822698)) ;
#58897 = CARTESIAN_POINT('Ctrl Pts',(29.3643007018345,617.002846303771,-35.4399424570837)) ;
#58898 = CARTESIAN_POINT('Ctrl Pts',(29.3068276492842,616.998639386775,-35.4602453669685)) ;
#58899 = CARTESIAN_POINT('Ctrl Pts',(29.2506048261699,616.994509838509,-35.4835993866685)) ;
#58900 = CARTESIAN_POINT('Ctrl Pts',(29.1943936706659,616.990381147224,-35.5069485598384)) ;
#58901 = CARTESIAN_POINT('Ctrl Pts',(29.1394322573245,616.986329792316,-35.5333475998383)) ;
#58902 = CARTESIAN_POINT('Ctrl Pts',(29.0860638811723,616.982354047787,-35.5626341994198)) ;
#58903 = CARTESIAN_POINT('Ctrl Pts',(29.0312260496663,616.978268834327,-35.5927271819878)) ;
#58904 = CARTESIAN_POINT('Ctrl Pts',(28.9780703963664,616.97426343898,-35.6258692258559)) ;
#58905 = CARTESIAN_POINT('Ctrl Pts',(28.9269540427023,616.970309623841,-35.6618476287035)) ;
#58906 = CARTESIAN_POINT('Ctrl Pts',(28.8771392174126,616.966456481036,-35.6969099467992)) ;
#58907 = CARTESIAN_POINT('Ctrl Pts',(28.8292613449351,616.962651954101,-35.7346660907345)) ;
#58908 = CARTESIAN_POINT('Ctrl Pts',(28.7836339573324,616.958848414507,-35.7748826535162)) ;
#58909 = CARTESIAN_POINT('Ctrl Pts',(28.7362183870171,616.954895810413,-35.816675343403)) ;
#58910 = CARTESIAN_POINT('Ctrl Pts',(28.6912338124573,616.950943843878,-35.8611256952804)) ;
#58911 = CARTESIAN_POINT('Ctrl Pts',(28.649007039024,616.946921188459,-35.9079260438706)) ;
#58912 = CARTESIAN_POINT('Ctrl Pts',(28.612563757972,616.943449486738,-35.9483164909338)) ;
#58913 = CARTESIAN_POINT('Ctrl Pts',(28.5781738025082,616.939924470793,-35.9904578913708)) ;
#58914 = CARTESIAN_POINT('Ctrl Pts',(28.5460281467764,616.936295530328,-36.0341183434806)) ;
#58915 = CARTESIAN_POINT('Ctrl Pts',(28.540947446731,616.935721967352,-36.0410189854481)) ;
#58916 = CARTESIAN_POINT('Ctrl Pts',(28.5359227081795,616.93514580828,-36.0479576011575)) ;
#58917 = CARTESIAN_POINT('Ctrl Pts',(28.5309545704018,616.934566853292,-36.05493330865)) ;
#58918 = CARTESIAN_POINT('Ctrl Pts',(28.5309342646271,616.934564486987,-36.0549618197645)) ;
#58919 = CARTESIAN_POINT('Ctrl Pts',(28.5309139597978,616.934562120636,-36.0549903314986)) ;
#58920 = CARTESIAN_POINT('Ctrl Pts',(28.530893655914,616.934559754237,-36.0550188438523)) ;
#58921 = CARTESIAN_POINT('Ctrl Pts',(28.4989996356354,616.930842536283,-36.0998070033906)) ;
#58922 = CARTESIAN_POINT('Ctrl Pts',(28.4693258899516,616.926999768579,-36.1462970726815)) ;
#58923 = CARTESIAN_POINT('Ctrl Pts',(28.4420269705331,616.923094265841,-36.1942290788419)) ;
#58924 = CARTESIAN_POINT('Ctrl Pts',(28.4393659813779,616.922713573101,-36.1989012985231)) ;
#58925 = CARTESIAN_POINT('Ctrl Pts',(28.4367275537249,616.922332284279,-36.2035871781143)) ;
#58926 = CARTESIAN_POINT('Ctrl Pts',(28.434111828081,616.921950457554,-36.208286450564)) ;
#58927 = CARTESIAN_POINT('Ctrl Pts',(28.4041867740043,616.917582191555,-36.262048198287)) ;
#58928 = CARTESIAN_POINT('Ctrl Pts',(28.3772331276111,616.913144219065,-36.3175689997004)) ;
#58929 = CARTESIAN_POINT('Ctrl Pts',(28.3534166267093,616.908709835501,-36.3744743718786)) ;
#58930 = CARTESIAN_POINT('Ctrl Pts',(28.3300446441918,616.904358216615,-36.4303176449596)) ;
#58931 = CARTESIAN_POINT('Ctrl Pts',(28.3096933215118,616.900010337835,-36.4874941931902)) ;
#58932 = CARTESIAN_POINT('Ctrl Pts',(28.2924806010451,616.895715230285,-36.5456427183914)) ;
#58933 = CARTESIAN_POINT('Ctrl Pts',(28.2752787466916,616.891422834166,-36.6037545353646)) ;
#58934 = CARTESIAN_POINT('Ctrl Pts',(28.2612113991684,616.887183285358,-36.6628370886462)) ;
#58935 = CARTESIAN_POINT('Ctrl Pts',(28.2503615449872,616.883021951294,-36.7225229685776)) ;
#58936 = CARTESIAN_POINT('Ctrl Pts',(28.2395144151561,616.878861662123,-36.7821938616503)) ;
#58937 = CARTESIAN_POINT('Ctrl Pts',(28.2318831900086,616.874779559,-36.8424677555916)) ;
#58938 = CARTESIAN_POINT('Ctrl Pts',(28.2275168206484,616.870776310009,-36.9029709682656)) ;
#58939 = CARTESIAN_POINT('Ctrl Pts',(28.2229994847329,616.866634649294,-36.9655660703)) ;
#58940 = CARTESIAN_POINT('Ctrl Pts',(28.2219770714696,616.862577421011,-37.0284066053647)) ;
#58941 = CARTESIAN_POINT('Ctrl Pts',(28.2244639128333,616.858578369016,-37.0910719989216)) ;
#58942 = CARTESIAN_POINT('Ctrl Pts',(28.2268707964393,616.854707895882,-37.1517225537264)) ;
#58943 = CARTESIAN_POINT('Ctrl Pts',(28.2325649901524,616.85089153798,-37.2122089216034)) ;
#58944 = CARTESIAN_POINT('Ctrl Pts',(28.2415198331724,616.847083689211,-37.2721447271132)) ;
#58945 = CARTESIAN_POINT('Ctrl Pts',(28.2509209020711,616.843086092765,-37.3350671743111)) ;
#58946 = CARTESIAN_POINT('Ctrl Pts',(28.2639166266811,616.839097499273,-37.3973826024798)) ;
#58947 = CARTESIAN_POINT('Ctrl Pts',(28.2804231555915,616.835045936516,-37.4586406500308)) ;
#58948 = CARTESIAN_POINT('Ctrl Pts',(28.2946495273849,616.83155404319,-37.5114367142142)) ;
#58949 = CARTESIAN_POINT('Ctrl Pts',(28.3114838637982,616.828014712853,-37.5634483508293)) ;
#58950 = CARTESIAN_POINT('Ctrl Pts',(28.3308327387374,616.82437615812,-37.6143849965462)) ;
#58951 = CARTESIAN_POINT('Ctrl Pts',(28.3339272689223,616.823794231911,-37.6225314643995)) ;
#58952 = CARTESIAN_POINT('Ctrl Pts',(28.3370860862066,616.823209767673,-37.6306505391174)) ;
#58953 = CARTESIAN_POINT('Ctrl Pts',(28.3403087758142,616.822622553551,-37.6387411517518)) ;
#58954 = CARTESIAN_POINT('Ctrl Pts',(28.3403156962882,616.822621292555,-37.6387585257097)) ;
#58955 = CARTESIAN_POINT('Ctrl Pts',(28.3403226170566,616.822620031546,-37.6387758995365)) ;
#58956 = CARTESIAN_POINT('Ctrl Pts',(28.3403295381196,616.822618770524,-37.6387932732319)) ;
#58957 = CARTESIAN_POINT('Ctrl Pts',(28.3611300540204,616.818828904217,-37.6910080601294)) ;
#58958 = CARTESIAN_POINT('Ctrl Pts',(28.3846714076599,616.814914584974,-37.7422176702767)) ;
#58959 = CARTESIAN_POINT('Ctrl Pts',(28.4108107263033,616.810938157239,-37.7921428459409)) ;
#58960 = CARTESIAN_POINT('Ctrl Pts',(28.4134417842094,616.810537909177,-37.7971680736424)) ;
#58961 = CARTESIAN_POINT('Ctrl Pts',(28.416099125224,616.810137031865,-37.8021802670086)) ;
#58962 = CARTESIAN_POINT('Ctrl Pts',(28.4187825777852,616.80973558888,-37.8071791277746)) ;
#58963 = CARTESIAN_POINT('Ctrl Pts',(28.448063689259,616.805355151177,-37.8617253498502)) ;
#58964 = CARTESIAN_POINT('Ctrl Pts',(28.480458763619,616.800907997258,-37.9146874851851)) ;
#58965 = CARTESIAN_POINT('Ctrl Pts',(28.5157431936671,616.796463345162,-37.9657275419637)) ;
#58966 = CARTESIAN_POINT('Ctrl Pts',(28.5509838970871,616.792024201152,-38.0167043467759)) ;
#58967 = CARTESIAN_POINT('Ctrl Pts',(28.5891065722251,616.787587893215,-38.0657641391842)) ;
#58968 = CARTESIAN_POINT('Ctrl Pts',(28.6298609711957,616.783202799171,-38.1125984677305)) ;
#58969 = CARTESIAN_POINT('Ctrl Pts',(28.6705776712394,616.778821761458,-38.1593894732498)) ;
#58970 = CARTESIAN_POINT('Ctrl Pts',(28.713921186153,616.774491979344,-38.2039592709164)) ;
#58971 = CARTESIAN_POINT('Ctrl Pts',(28.7596174176482,616.770237644049,-38.2460251560201)) ;
#58972 = CARTESIAN_POINT('Ctrl Pts',(28.8052857253946,616.765985908465,-38.2880653357831)) ;
#58973 = CARTESIAN_POINT('Ctrl Pts',(28.8533039277465,616.761809520445,-38.3276046412806)) ;
#58974 = CARTESIAN_POINT('Ctrl Pts',(28.903373768419,616.757707658521,-38.3643848801307)) ;
#58975 = CARTESIAN_POINT('Ctrl Pts',(28.9534480750791,616.753605430732,-38.4011683996002)) ;
#58976 = CARTESIAN_POINT('Ctrl Pts',(29.0055744969324,616.749577607991,-38.4351921860378)) ;
#58977 = CARTESIAN_POINT('Ctrl Pts',(29.0594287737958,616.745599436479,-38.4662234489906)) ;
#58978 = CARTESIAN_POINT('Ctrl Pts',(29.113280978284,616.741621418052,-38.4972535178244)) ;
#58979 = CARTESIAN_POINT('Ctrl Pts',(29.1688610436538,616.73769275453,-38.5252909485167)) ;
#58980 = CARTESIAN_POINT('Ctrl Pts',(29.225816917922,616.733767924342,-38.5501323001247)) ;
#58981 = CARTESIAN_POINT('Ctrl Pts',(29.2828293655759,616.729839195681,-38.5749983262617)) ;
#58982 = CARTESIAN_POINT('Ctrl Pts',(29.3412204591112,616.72591380392,-38.5966613468097)) ;
#58983 = CARTESIAN_POINT('Ctrl Pts',(29.4006072854367,616.721931192345,-38.614953546914)) ;
#58984 = CARTESIAN_POINT('Ctrl Pts',(29.4560806936032,616.718211023225,-38.6320403445327)) ;
#58985 = CARTESIAN_POINT('Ctrl Pts',(29.5124225672536,616.714440274229,-38.6461857255948)) ;
#58986 = CARTESIAN_POINT('Ctrl Pts',(29.5692971707936,616.710565160562,-38.6572894990042)) ;
#58987 = CARTESIAN_POINT('Origin',(29.8885276254216,616.710565160562,-37.0221601717529)) ;
#58988 = CARTESIAN_POINT('Ctrl Pts',(30.4640776716666,617.544128797339,-38.5855853040402)) ;
#58989 = CARTESIAN_POINT('Ctrl Pts',(30.4870886073976,617.542498162509,-38.5771141947747)) ;
#58990 = CARTESIAN_POINT('Ctrl Pts',(30.5099115798872,617.540850531879,-38.5681354130923)) ;
#58991 = CARTESIAN_POINT('Ctrl Pts',(30.5976250051638,617.534394017862,-38.5313714471249)) ;
#58992 = CARTESIAN_POINT('Ctrl Pts',(30.660911230605,617.529463405148,-38.4999825094059)) ;
#58993 = CARTESIAN_POINT('Ctrl Pts',(30.8129108067211,617.51693396129,-38.4121577697486)) ;
#58994 = CARTESIAN_POINT('Ctrl Pts',(30.8986404385462,617.509222910576,-38.3511624079992)) ;
#58995 = CARTESIAN_POINT('Ctrl Pts',(31.0204908109826,617.49757869963,-38.2458277171379)) ;
#58996 = CARTESIAN_POINT('Ctrl Pts',(31.0610538744134,617.493569625233,-38.2070172974096)) ;
#58997 = CARTESIAN_POINT('Ctrl Pts',(31.120283128478,617.487597464982,-38.1443200794749)) ;
#58998 = CARTESIAN_POINT('Ctrl Pts',(31.1403849618483,617.485549086919,-38.1218502411609)) ;
#58999 = CARTESIAN_POINT('Ctrl Pts',(31.1872890121697,617.480729435838,-38.066466099345)) ;
#59000 = CARTESIAN_POINT('Ctrl Pts',(31.2134640920881,617.477998173657,-38.0330509294253)) ;
#59001 = CARTESIAN_POINT('Ctrl Pts',(31.2740490641244,617.471469895617,-37.9493055050781)) ;
#59002 = CARTESIAN_POINT('Ctrl Pts',(31.3070285931238,617.467731322031,-37.8980163920712)) ;
#59003 = CARTESIAN_POINT('Ctrl Pts',(31.3976063361618,617.456522781782,-37.738561859865)) ;
#59004 = CARTESIAN_POINT('Ctrl Pts',(31.4461583310577,617.449102357673,-37.6257601040785)) ;
#59005 = CARTESIAN_POINT('Ctrl Pts',(31.49695302564,617.437936044848,-37.4593979861534)) ;
#59006 = CARTESIAN_POINT('Ctrl Pts',(31.5097002534967,617.434563236637,-37.4094682140154)) ;
#59007 = CARTESIAN_POINT('Ctrl Pts',(31.5318042219605,617.42723820241,-37.3024112279107)) ;
#59008 = CARTESIAN_POINT('Ctrl Pts',(31.5405380584223,617.423270257557,-37.2452268023006)) ;
#59009 = CARTESIAN_POINT('Ctrl Pts',(31.5530848136482,617.414415644119,-37.1195881523293)) ;
#59010 = CARTESIAN_POINT('Ctrl Pts',(31.5556816478247,617.409501703735,-37.0511186579818)) ;
#59011 = CARTESIAN_POINT('Ctrl Pts',(31.551364639642,617.396283137486,-36.8689534061587)) ;
#59012 = CARTESIAN_POINT('Ctrl Pts',(31.5370261938174,617.387906413662,-36.7557870216662)) ;
#59013 = CARTESIAN_POINT('Ctrl Pts',(31.5040345977418,617.377735721192,-36.6138550900405)) ;
#59014 = CARTESIAN_POINT('Ctrl Pts',(31.4959103809542,617.375544949996,-36.5829596299875)) ;
#59015 = CARTESIAN_POINT('Ctrl Pts',(31.4765274013552,617.370944982721,-36.5170207832697)) ;
#59016 = CARTESIAN_POINT('Ctrl Pts',(31.4649863835773,617.368550943906,-36.482079237073)) ;
#59017 = CARTESIAN_POINT('Ctrl Pts',(31.4160475315186,617.359491463879,-36.348896047106)) ;
#59018 = CARTESIAN_POINT('Ctrl Pts',(31.3705412875037,617.353157847879,-36.253888274902)) ;
#59019 = CARTESIAN_POINT('Ctrl Pts',(31.2682944591186,617.341021908365,-36.083805167669)) ;
#59020 = CARTESIAN_POINT('Ctrl Pts',(31.2135776528049,617.335260542601,-36.0080073074761)) ;
#59021 = CARTESIAN_POINT('Ctrl Pts',(31.1199800046529,617.32600613038,-35.8989407106407)) ;
#59022 = CARTESIAN_POINT('Ctrl Pts',(31.085436789944,617.322695776807,-35.8622013548397)) ;
#59023 = CARTESIAN_POINT('Ctrl Pts',(31.0066504752701,617.315318776738,-35.785677373248)) ;
#59024 = CARTESIAN_POINT('Ctrl Pts',(30.9618365196369,617.311227645608,-35.746583875975)) ;
#59025 = CARTESIAN_POINT('Ctrl Pts',(30.8580545427131,617.301959437935,-35.6653966623566)) ;
#59026 = CARTESIAN_POINT('Ctrl Pts',(30.7982369156724,617.296747847191,-35.6245848501746)) ;
#59027 = CARTESIAN_POINT('Ctrl Pts',(30.6425297205435,617.283604867001,-35.5325918978048)) ;
#59028 = CARTESIAN_POINT('Ctrl Pts',(30.5439205953216,617.275637758637,-35.4866484003713)) ;
#59029 = CARTESIAN_POINT('Ctrl Pts',(30.412278357908,617.265930567536,-35.4403247633842)) ;
#59030 = CARTESIAN_POINT('Ctrl Pts',(30.3827336529789,617.263811058756,-35.4308465257249)) ;
#59031 = CARTESIAN_POINT('Ctrl Pts',(30.3155656254478,617.25914548512,-35.4113502077275)) ;
#59032 = CARTESIAN_POINT('Ctrl Pts',(30.2778229749583,617.256624228392,-35.4018145475948)) ;
#59033 = CARTESIAN_POINT('Ctrl Pts',(30.1884327320442,617.250811724477,-35.3825346584289)) ;
#59034 = CARTESIAN_POINT('Ctrl Pts',(30.1365894251518,617.247562366096,-35.3738941068678)) ;
#59035 = CARTESIAN_POINT('Ctrl Pts',(29.9487586834912,617.23595861954,-35.3516540917144)) ;
#59036 = CARTESIAN_POINT('Ctrl Pts',(29.8116487772101,617.227755495534,-35.352338267726)) ;
#59037 = CARTESIAN_POINT('Ctrl Pts',(29.6248758931455,617.215677846966,-35.3763419584364)) ;
#59038 = CARTESIAN_POINT('Ctrl Pts',(29.5739286708588,617.212295000644,-35.385316760625)) ;
#59039 = CARTESIAN_POINT('Ctrl Pts',(29.4675158041588,617.204992700149,-35.4092139180621)) ;
#59040 = CARTESIAN_POINT('Ctrl Pts',(29.4122395552297,617.201059631714,-35.4246637422172)) ;
#59041 = CARTESIAN_POINT('Ctrl Pts',(29.2939847461709,617.192319808958,-35.4643997058494)) ;
#59042 = CARTESIAN_POINT('Ctrl Pts',(29.2314621985705,617.187487711256,-35.4897234637654)) ;
#59043 = CARTESIAN_POINT('Ctrl Pts',(29.0648593524841,617.174104739204,-35.5692767664972)) ;
#59044 = CARTESIAN_POINT('Ctrl Pts',(28.9646911415418,617.165465063662,-35.6308195405618)) ;
#59045 = CARTESIAN_POINT('Ctrl Pts',(28.8467753484453,617.15508972846,-35.7216576232664)) ;
#59046 = CARTESIAN_POINT('Ctrl Pts',(28.8222907732495,617.152925045025,-35.7416546882143)) ;
#59047 = CARTESIAN_POINT('Ctrl Pts',(28.7699301968425,617.148296699119,-35.7869630925057)) ;
#59048 = CARTESIAN_POINT('Ctrl Pts',(28.7423139543213,617.145851855969,-35.8125458436048)) ;
#59049 = CARTESIAN_POINT('Ctrl Pts',(28.6802983183195,617.140285778908,-35.8740282239296)) ;
#59050 = CARTESIAN_POINT('Ctrl Pts',(28.6465914251868,617.137201230933,-35.9105756221166)) ;
#59051 = CARTESIAN_POINT('Ctrl Pts',(28.5176323076652,617.124896791614,-36.0636042640291)) ;
#59052 = CARTESIAN_POINT('Ctrl Pts',(28.4367314832795,617.115900369978,-36.1912158425178)) ;
#59053 = CARTESIAN_POINT('Ctrl Pts',(28.3530185123571,617.102925574984,-36.3738420434138)) ;
#59054 = CARTESIAN_POINT('Ctrl Pts',(28.3340811954692,617.099599431862,-36.4206620424088)) ;
#59055 = CARTESIAN_POINT('Ctrl Pts',(28.2967020748125,617.092024017412,-36.5266950412998)) ;
#59056 = CARTESIAN_POINT('Ctrl Pts',(28.2793821606208,617.087741875056,-36.5862204813015)) ;
#59057 = CARTESIAN_POINT('Ctrl Pts',(28.2289550007918,617.071942889591,-36.8041385018246)) ;
#59058 = CARTESIAN_POINT('Ctrl Pts',(28.2156358069072,617.059870181053,-36.9661528427404)) ;
#59059 = CARTESIAN_POINT('Ctrl Pts',(28.2281399435907,617.045929972079,-37.1634557467531)) ;
#59060 = CARTESIAN_POINT('Ctrl Pts',(28.231580517554,617.043433705033,-37.1992999385523)) ;
#59061 = CARTESIAN_POINT('Ctrl Pts',(28.2403058126092,617.038819791819,-37.2670348364461)) ;
#59062 = CARTESIAN_POINT('Ctrl Pts',(28.2453618284591,617.036693075322,-37.2989364693367)) ;
#59063 = CARTESIAN_POINT('Ctrl Pts',(28.2585259665357,617.032099508037,-37.3687946786095)) ;
#59064 = CARTESIAN_POINT('Ctrl Pts',(28.2670395693494,617.029651298592,-37.4066570143532)) ;
#59065 = CARTESIAN_POINT('Ctrl Pts',(28.3006255818359,617.021395066578,-37.5349161828583)) ;
#59066 = CARTESIAN_POINT('Ctrl Pts',(28.3320023335011,617.015749891101,-37.6234771640302)) ;
#59067 = CARTESIAN_POINT('Ctrl Pts',(28.4044325190586,617.004956760119,-37.7835583937137)) ;
#59068 = CARTESIAN_POINT('Ctrl Pts',(28.4436523053243,616.999851902999,-37.8555858466508)) ;
#59069 = CARTESIAN_POINT('Ctrl Pts',(28.5151216221253,616.991317092595,-37.966521728796)) ;
#59070 = CARTESIAN_POINT('Ctrl Pts',(28.5441181483823,616.988013561413,-38.0073632187489)) ;
#59071 = CARTESIAN_POINT('Ctrl Pts',(28.613441705303,616.980408985052,-38.0962352706777)) ;
#59072 = CARTESIAN_POINT('Ctrl Pts',(28.6547275293901,616.97607115754,-38.1434170302327)) ;
#59073 = CARTESIAN_POINT('Ctrl Pts',(28.779915770761,616.96341450797,-38.2711780970165)) ;
#59074 = CARTESIAN_POINT('Ctrl Pts',(28.8697239072827,616.954876062616,-38.3454513757762)) ;
#59075 = CARTESIAN_POINT('Ctrl Pts',(29.0150749100818,616.942224296778,-38.442031868612)) ;
#59076 = CARTESIAN_POINT('Ctrl Pts',(29.0653010087839,616.938040557698,-38.4717306523879)) ;
#59077 = CARTESIAN_POINT('Ctrl Pts',(29.1442432960397,616.931847911846,-38.5129796347347)) ;
#59078 = CARTESIAN_POINT('Ctrl Pts',(29.1718933303721,616.929748206103,-38.5264665690584)) ;
#59079 = CARTESIAN_POINT('Ctrl Pts',(29.2364771420603,616.925019053216,-38.5557830506843)) ;
#59080 = CARTESIAN_POINT('Ctrl Pts',(29.2736396780909,616.922419203892,-38.5710573407325)) ;
#59081 = CARTESIAN_POINT('Ctrl Pts',(29.3631528456667,616.916358122219,-38.6041179052323)) ;
#59082 = CARTESIAN_POINT('Ctrl Pts',(29.4159079588574,616.912943380221,-38.6206721111095)) ;
#59083 = CARTESIAN_POINT('Ctrl Pts',(29.6014600615896,616.901175595285,-38.6689051125641)) ;
#59084 = CARTESIAN_POINT('Ctrl Pts',(29.7372310334632,616.892937798099,-38.6868770490437)) ;
#59085 = CARTESIAN_POINT('Ctrl Pts',(29.9247134127121,616.880839787882,-38.6885491645884)) ;
#59086 = CARTESIAN_POINT('Ctrl Pts',(29.9757459591647,616.877480072484,-38.6866582045623)) ;
#59087 = CARTESIAN_POINT('Ctrl Pts',(30.0875067893749,616.869930109791,-38.6773634004201)) ;
#59088 = CARTESIAN_POINT('Ctrl Pts',(30.1480740184896,616.86571182508,-38.668952337198)) ;
#59089 = CARTESIAN_POINT('Ctrl Pts',(30.2951511863831,616.855140363488,-38.6402121081937)) ;
#59090 = CARTESIAN_POINT('Ctrl Pts',(30.380757274049,616.848696268288,-38.6162559893195)) ;
#59091 = CARTESIAN_POINT('Ctrl Pts',(30.4640381476845,616.84223029543,-38.585599853597)) ;
#59092 = CARTESIAN_POINT('Origin',(29.8885276254218,617.710565160562,-37.0221601717529)) ;
#59093 = CARTESIAN_POINT('',(30.4640776731091,618.242171074983,-38.5855853035092)) ;
#59094 = CARTESIAN_POINT('',(30.4640776576043,618.051524931058,-38.5855853092171)) ;
#59095 = CARTESIAN_POINT('',(30.4640776578155,617.710565160562,-38.5855853091393)) ;
#59096 = CARTESIAN_POINT('',(29.8896085855951,618.281230024789,-38.6886301592882)) ;
#59097 = CARTESIAN_POINT('Ctrl Pts',(29.889588780989,618.280960192427,-38.6881598338024)) ;
#59098 = CARTESIAN_POINT('Ctrl Pts',(29.9346123899361,618.277705627339,-38.6881311560935)) ;
#59099 = CARTESIAN_POINT('Ctrl Pts',(29.9796197792924,618.274477707997,-38.6862773372091)) ;
#59100 = CARTESIAN_POINT('Ctrl Pts',(30.0545924905335,618.269194666625,-38.6801378871634)) ;
#59101 = CARTESIAN_POINT('Ctrl Pts',(30.0846152551122,618.267104597096,-38.676855790806)) ;
#59102 = CARTESIAN_POINT('Ctrl Pts',(30.1454735976508,618.262941509797,-38.6685228094867)) ;
#59103 = CARTESIAN_POINT('Ctrl Pts',(30.1762873146518,618.260876176576,-38.6634175088081)) ;
#59104 = CARTESIAN_POINT('Ctrl Pts',(30.2944515861005,618.253067360093,-38.6404092731344)) ;
#59105 = CARTESIAN_POINT('Ctrl Pts',(30.3804395485023,618.247609791015,-38.6163753462388)) ;
#59106 = CARTESIAN_POINT('Ctrl Pts',(30.4640776731659,618.242171075974,-38.5855853034883)) ;
#59107 = CARTESIAN_POINT('',(30.9678862784725,618.710565160562,-35.7530892919022)) ;
#59108 = CARTESIAN_POINT('Ctrl Pts',(29.8896085855951,618.281230024788,-38.6886301592882)) ;
#59109 = CARTESIAN_POINT('Ctrl Pts',(29.8297449858523,618.285479107441,-38.6885353801434)) ;
#59110 = CARTESIAN_POINT('Ctrl Pts',(29.7697812032065,618.289767378033,-38.6851881605191)) ;
#59111 = CARTESIAN_POINT('Ctrl Pts',(29.7100945358446,618.294034879536,-38.678613355152)) ;
#59112 = CARTESIAN_POINT('Ctrl Pts',(29.6504725284024,618.298297757958,-38.6720456724206)) ;
#59113 = CARTESIAN_POINT('Ctrl Pts',(29.5911270001335,618.302539653761,-38.6622576307303)) ;
#59114 = CARTESIAN_POINT('Ctrl Pts',(29.5324254623936,618.306721098468,-38.6493109448699)) ;
#59115 = CARTESIAN_POINT('Ctrl Pts',(29.4737645016973,618.31089965278,-38.6363732083192)) ;
#59116 = CARTESIAN_POINT('Ctrl Pts',(29.4157466608234,618.315017741293,-38.620281262818)) ;
#59117 = CARTESIAN_POINT('Ctrl Pts',(29.3587302988432,618.319058873962,-38.601131373573)) ;
#59118 = CARTESIAN_POINT('Ctrl Pts',(29.30173080255,618.323098811247,-38.5819871489481)) ;
#59119 = CARTESIAN_POINT('Ctrl Pts',(29.2457322858195,618.327061860551,-38.559786746764)) ;
#59120 = CARTESIAN_POINT('Ctrl Pts',(29.1910835605629,618.330954988191,-38.5346608511779)) ;
#59121 = CARTESIAN_POINT('Ctrl Pts',(29.1363907934061,618.334851253337,-38.5095147064062)) ;
#59122 = CARTESIAN_POINT('Ctrl Pts',(29.0830501679372,618.33867762189,-38.4814382115276)) ;
#59123 = CARTESIAN_POINT('Ctrl Pts',(29.0314001022382,618.342463380071,-38.4505983134762)) ;
#59124 = CARTESIAN_POINT('Ctrl Pts',(28.9797307970573,618.346250548434,-38.4197469276628)) ;
#59125 = CARTESIAN_POINT('Ctrl Pts',(28.9297535935047,618.349997366089,-38.3861298563673)) ;
#59126 = CARTESIAN_POINT('Ctrl Pts',(28.8817926756802,618.353752293416,-38.3499529169218)) ;
#59127 = CARTESIAN_POINT('Ctrl Pts',(28.8337428817942,618.357514178974,-38.3137089382278)) ;
#59128 = CARTESIAN_POINT('Ctrl Pts',(28.7877173256831,618.361284694683,-38.274895306099)) ;
#59129 = CARTESIAN_POINT('Ctrl Pts',(28.7440217543737,618.365125980119,-38.2337617297627)) ;
#59130 = CARTESIAN_POINT('Ctrl Pts',(28.7057698880118,618.368488708485,-38.197752678551)) ;
#59131 = CARTESIAN_POINT('Ctrl Pts',(28.6693036492513,618.371906199368,-38.1599662778762)) ;
#59132 = CARTESIAN_POINT('Ctrl Pts',(28.6348100298656,618.37542306303,-38.120599317061)) ;
#59133 = CARTESIAN_POINT('Ctrl Pts',(28.6347883455892,618.375425273892,-38.120574569178)) ;
#59134 = CARTESIAN_POINT('Ctrl Pts',(28.6347666620908,618.375427484794,-38.1205498206701)) ;
#59135 = CARTESIAN_POINT('Ctrl Pts',(28.6347449793705,618.375429695735,-38.1205250715374)) ;
#59136 = CARTESIAN_POINT('Ctrl Pts',(28.5981467952976,618.379161534733,-38.0787511013883)) ;
#59137 = CARTESIAN_POINT('Ctrl Pts',(28.5636303654075,618.383015722911,-38.0350294420995)) ;
#59138 = CARTESIAN_POINT('Ctrl Pts',(28.531378565565,618.386928787822,-37.9896100342397)) ;
#59139 = CARTESIAN_POINT('Ctrl Pts',(28.5284469004474,618.387284482573,-37.9854814431429)) ;
#59140 = CARTESIAN_POINT('Ctrl Pts',(28.5255339488775,618.387640663803,-37.9813388596409)) ;
#59141 = CARTESIAN_POINT('Ctrl Pts',(28.5226398486572,618.38799728384,-37.977182492738)) ;
#59142 = CARTESIAN_POINT('Ctrl Pts',(28.4874781000698,618.392330023944,-37.9266848883172)) ;
#59143 = CARTESIAN_POINT('Ctrl Pts',(28.4550983019595,618.396726873743,-37.8741467840394)) ;
#59144 = CARTESIAN_POINT('Ctrl Pts',(28.425700907645,618.401116810854,-37.8199226959434)) ;
#59145 = CARTESIAN_POINT('Ctrl Pts',(28.396740112552,618.405441550244,-37.7665039239378)) ;
#59146 = CARTESIAN_POINT('Ctrl Pts',(28.3706733647025,618.40975930175,-37.7114489965768)) ;
#59147 = CARTESIAN_POINT('Ctrl Pts',(28.347654934977,618.414022908089,-37.6551079675871)) ;
#59148 = CARTESIAN_POINT('Ctrl Pts',(28.324649873497,618.418284038284,-37.5987996593654)) ;
#59149 = CARTESIAN_POINT('Ctrl Pts',(28.3046894658897,618.422490954923,-37.5412067612326)) ;
#59150 = CARTESIAN_POINT('Ctrl Pts',(28.2878940171809,618.426620502795,-37.482688995998)) ;
#59151 = CARTESIAN_POINT('Ctrl Pts',(28.2711020539386,618.430749193685,-37.4241833746311)) ;
#59152 = CARTESIAN_POINT('Ctrl Pts',(28.2574737739795,618.434800548162,-37.364753280186)) ;
#59153 = CARTESIAN_POINT('Ctrl Pts',(28.2470963213345,618.438776292223,-37.3047683084225)) ;
#59154 = CARTESIAN_POINT('Ctrl Pts',(28.236433133094,618.4428615055,-37.2431316941786)) ;
#59155 = CARTESIAN_POINT('Ctrl Pts',(28.229202618305,618.446866900611,-37.1809092011108)) ;
#59156 = CARTESIAN_POINT('Ctrl Pts',(28.2254611411747,618.450820715466,-37.1185126557978)) ;
#59157 = CARTESIAN_POINT('Ctrl Pts',(28.221814930076,618.454673857716,-37.0577048603424)) ;
#59158 = CARTESIAN_POINT('Ctrl Pts',(28.221482507039,618.458478384057,-36.9967318626566)) ;
#59159 = CARTESIAN_POINT('Ctrl Pts',(28.2244768711679,618.462281923013,-36.9359843188411)) ;
#59160 = CARTESIAN_POINT('Ctrl Pts',(28.2275885877403,618.46623452687,-36.8728560115677)) ;
#59161 = CARTESIAN_POINT('Ctrl Pts',(28.2342938498349,618.47018649312,-36.8099713082175)) ;
#59162 = CARTESIAN_POINT('Ctrl Pts',(28.2445558748495,618.474209148222,-36.7477775418026)) ;
#59163 = CARTESIAN_POINT('Ctrl Pts',(28.2534123844592,618.477680849325,-36.6941020061133)) ;
#59164 = CARTESIAN_POINT('Ctrl Pts',(28.2649180720467,618.481205864618,-36.6409401234693)) ;
#59165 = CARTESIAN_POINT('Ctrl Pts',(28.2790106999861,618.484834804392,-36.5885857918049)) ;
#59166 = CARTESIAN_POINT('Ctrl Pts',(28.2812380762404,618.485408367698,-36.5803110544275)) ;
#59167 = CARTESIAN_POINT('Ctrl Pts',(28.2835300330796,618.485984527103,-36.5720563932982)) ;
#59168 = CARTESIAN_POINT('Ctrl Pts',(28.2858862795444,618.486563482427,-36.5638228581211)) ;
#59169 = CARTESIAN_POINT('Ctrl Pts',(28.2858959098962,618.486565848709,-36.5637892063614)) ;
#59170 = CARTESIAN_POINT('Ctrl Pts',(28.2859055413219,618.486568215038,-36.5637555549545)) ;
#59171 = CARTESIAN_POINT('Ctrl Pts',(28.2859151738214,618.486570581413,-36.5637219039006)) ;
#59172 = CARTESIAN_POINT('Ctrl Pts',(28.3010463718862,618.490287798736,-36.5108611940827)) ;
#59173 = CARTESIAN_POINT('Ctrl Pts',(28.3188924951506,618.494130565774,-36.4586752415526)) ;
#59174 = CARTESIAN_POINT('Ctrl Pts',(28.3393466499888,618.498036067807,-36.4074469701344)) ;
#59175 = CARTESIAN_POINT('Ctrl Pts',(28.3413404373472,618.498416760172,-36.4024534477544)) ;
#59176 = CARTESIAN_POINT('Ctrl Pts',(28.3433589712799,618.498798048617,-36.397469047839)) ;
#59177 = CARTESIAN_POINT('Ctrl Pts',(28.3454021306024,618.499179874965,-36.3924940467439)) ;
#59178 = CARTESIAN_POINT('Ctrl Pts',(28.3687767930042,618.503548140265,-36.3355777946607)) ;
#59179 = CARTESIAN_POINT('Ctrl Pts',(28.3953793814839,618.507986112013,-36.2798879307798)) ;
#59180 = CARTESIAN_POINT('Ctrl Pts',(28.4250204492715,618.512420494789,-36.2257875204666)) ;
#59181 = CARTESIAN_POINT('Ctrl Pts',(28.4541082846005,618.516772112514,-36.1726968613278)) ;
#59182 = CARTESIAN_POINT('Ctrl Pts',(28.4861218665686,618.521119990088,-36.1211365656175)) ;
#59183 = CARTESIAN_POINT('Ctrl Pts',(28.5208522567435,618.525415096405,-36.071424110073)) ;
#59184 = CARTESIAN_POINT('Ctrl Pts',(28.5555607222739,618.529707491302,-36.0217430370702)) ;
#59185 = CARTESIAN_POINT('Ctrl Pts',(28.5929824726078,618.53394703886,-35.9739073758844)) ;
#59186 = CARTESIAN_POINT('Ctrl Pts',(28.6328819965436,618.538108371662,-35.9282110840983)) ;
#59187 = CARTESIAN_POINT('Ctrl Pts',(28.6727715019973,618.542268659583,-35.8825262663209)) ;
#59188 = CARTESIAN_POINT('Ctrl Pts',(28.7151375358478,618.546350761444,-35.8389797790131)) ;
#59189 = CARTESIAN_POINT('Ctrl Pts',(28.7597184621479,618.550354009176,-35.7978428806241)) ;
#59190 = CARTESIAN_POINT('Ctrl Pts',(28.8058407739393,618.554495669195,-35.755283674006)) ;
#59191 = CARTESIAN_POINT('Ctrl Pts',(28.854334021853,618.558552896762,-35.7153038834646)) ;
#59192 = CARTESIAN_POINT('Ctrl Pts',(28.9048783231777,618.56255194805,-35.6781769381591)) ;
#59193 = CARTESIAN_POINT('Ctrl Pts',(28.95379750039,618.566422419963,-35.6422437158344)) ;
#59194 = CARTESIAN_POINT('Ctrl Pts',(29.0046379149652,618.570238776668,-35.6089829846873)) ;
#59195 = CARTESIAN_POINT('Ctrl Pts',(29.0570808636889,618.574046624285,-35.5786148015285)) ;
#59196 = CARTESIAN_POINT('Ctrl Pts',(29.1121370912538,618.57804422034,-35.5467333447566)) ;
#59197 = CARTESIAN_POINT('Ctrl Pts',(29.168959963637,618.582032813487,-35.5180407741232)) ;
#59198 = CARTESIAN_POINT('Ctrl Pts',(29.227145093238,618.586084376013,-35.4927523278367)) ;
#59199 = CARTESIAN_POINT('Ctrl Pts',(29.277292708399,618.58957626818,-35.4709571495654)) ;
#59200 = CARTESIAN_POINT('Ctrl Pts',(29.3284530721797,618.593115597418,-35.4516900420697)) ;
#59201 = CARTESIAN_POINT('Ctrl Pts',(29.380340762874,618.596754151116,-35.4350591250646)) ;
#59202 = CARTESIAN_POINT('Ctrl Pts',(29.3886393508534,618.597336078304,-35.4323992817357)) ;
#59203 = CARTESIAN_POINT('Ctrl Pts',(29.3969566044291,618.597920543533,-35.4298067796712)) ;
#59204 = CARTESIAN_POINT('Ctrl Pts',(29.4052914292488,618.598507758659,-35.4272819610661)) ;
#59205 = CARTESIAN_POINT('Ctrl Pts',(29.4053093277901,618.598509019668,-35.4272765391681)) ;
#59206 = CARTESIAN_POINT('Ctrl Pts',(29.4053272264123,618.598510280691,-35.4272711175822)) ;
#59207 = CARTESIAN_POINT('Ctrl Pts',(29.4053451251156,618.598511541726,-35.4272656963085)) ;
#59208 = CARTESIAN_POINT('Ctrl Pts',(29.4591371956578,618.602301407442,-35.410972809824)) ;
#59209 = CARTESIAN_POINT('Ctrl Pts',(29.5138522715128,618.606215726214,-35.3974495137543)) ;
#59210 = CARTESIAN_POINT('Ctrl Pts',(29.5691829405726,618.610192153612,-35.3867582200091)) ;
#59211 = CARTESIAN_POINT('Ctrl Pts',(29.5747522698706,618.610592402406,-35.3856820838174)) ;
#59212 = CARTESIAN_POINT('Ctrl Pts',(29.580327795787,618.610993280455,-35.3846346234691)) ;
#59213 = CARTESIAN_POINT('Ctrl Pts',(29.5859091781601,618.611394724179,-35.3836158907974)) ;
#59214 = CARTESIAN_POINT('Ctrl Pts',(29.6468116129468,618.615775162321,-35.3724997736849)) ;
#59215 = CARTESIAN_POINT('Ctrl Pts',(29.7084170829286,618.620222316849,-35.3648059135374)) ;
#59216 = CARTESIAN_POINT('Ctrl Pts',(29.7703212950613,618.624666969685,-35.3605694397996)) ;
#59217 = CARTESIAN_POINT('Ctrl Pts',(29.8321487915922,618.629106114427,-35.356338216167)) ;
#59218 = CARTESIAN_POINT('Ctrl Pts',(29.8942743873207,618.633542423227,-35.3555554472147)) ;
#59219 = CARTESIAN_POINT('Ctrl Pts',(29.9563008980942,618.637927518225,-35.3582177975719)) ;
#59220 = CARTESIAN_POINT('Ctrl Pts',(30.0182700325272,618.64230855688,-35.3608776851769)) ;
#59221 = CARTESIAN_POINT('Ctrl Pts',(30.0801403488002,618.646638340028,-35.3669762005155)) ;
#59222 = CARTESIAN_POINT('Ctrl Pts',(30.1415199219065,618.650892676407,-35.3764753083873)) ;
#59223 = CARTESIAN_POINT('Ctrl Pts',(30.2028619874384,618.655144413065,-35.3859686115837)) ;
#59224 = CARTESIAN_POINT('Ctrl Pts',(30.2637139257696,618.659320802209,-35.3988584066383)) ;
#59225 = CARTESIAN_POINT('Ctrl Pts',(30.3236879141443,618.663422665272,-35.4150724876848)) ;
#59226 = CARTESIAN_POINT('Ctrl Pts',(30.3836672515966,618.66752489418,-35.4312880148645)) ;
#59227 = CARTESIAN_POINT('Ctrl Pts',(30.442768415426,618.671552718056,-35.4508286163203)) ;
#59228 = CARTESIAN_POINT('Ctrl Pts',(30.5006072297424,618.675530890686,-35.4735859176792)) ;
#59229 = CARTESIAN_POINT('Ctrl Pts',(30.5584438181912,618.679508910221,-35.4963423432467)) ;
#59230 = CARTESIAN_POINT('Ctrl Pts',(30.6150179711524,618.683437574835,-35.5223155447779)) ;
#59231 = CARTESIAN_POINT('Ctrl Pts',(30.6699511312009,618.687362406073,-35.551357120278)) ;
#59232 = CARTESIAN_POINT('Ctrl Pts',(30.7249388551544,618.691291135759,-35.5804275421391)) ;
#59233 = CARTESIAN_POINT('Ctrl Pts',(30.7782819396851,618.695216528502,-35.6125728745798)) ;
#59234 = CARTESIAN_POINT('Ctrl Pts',(30.8296104393782,618.699199140992,-35.6475983749195)) ;
#59235 = CARTESIAN_POINT('Ctrl Pts',(30.8775564809086,618.7029193063,-35.6803157561786)) ;
#59236 = CARTESIAN_POINT('Ctrl Pts',(30.9237443136949,618.706690051297,-35.7155460684294)) ;
#59237 = CARTESIAN_POINT('Ctrl Pts',(30.9678862784723,618.710565160562,-35.7530892919022)) ;
#59238 = CARTESIAN_POINT('',(30.9861662751902,618.710557609671,-38.2766259197886)) ;
#59239 = CARTESIAN_POINT('Origin',(29.888527625422,618.710565160562,-37.0221601717529)) ;
#59240 = CARTESIAN_POINT('',(29.8893921427819,618.088263764204,-38.6876853814548)) ;
#59241 = CARTESIAN_POINT('Ctrl Pts',(30.9861662858252,618.710557609533,-38.2766259319431)) ;
#59242 = CARTESIAN_POINT('Ctrl Pts',(31.0258667566383,618.70695394026,-38.2418476139244)) ;
#59243 = CARTESIAN_POINT('Ctrl Pts',(31.0639450042156,618.703253312121,-38.2050806626661)) ;
#59244 = CARTESIAN_POINT('Ctrl Pts',(31.1002122807239,618.699509774449,-38.1665176179903)) ;
#59245 = CARTESIAN_POINT('Ctrl Pts',(31.1416403247482,618.695233538173,-38.1224671221618)) ;
#59246 = CARTESIAN_POINT('Ctrl Pts',(31.1807061224321,618.690901872949,-38.0760720093977)) ;
#59247 = CARTESIAN_POINT('Ctrl Pts',(31.2171692764965,618.686580914103,-38.0276356050523)) ;
#59248 = CARTESIAN_POINT('Ctrl Pts',(31.2535952574382,618.682264360348,-37.9792485802092)) ;
#59249 = CARTESIAN_POINT('Ctrl Pts',(31.2874241804867,618.677958789138,-37.92882455607)) ;
#59250 = CARTESIAN_POINT('Ctrl Pts',(31.3184506199994,618.673709374166,-37.8766830306392)) ;
#59251 = CARTESIAN_POINT('Ctrl Pts',(31.3494572013223,618.669462678993,-37.8245748779165)) ;
#59252 = CARTESIAN_POINT('Ctrl Pts',(31.3776649807041,618.66527218633,-37.7707514607234)) ;
#59253 = CARTESIAN_POINT('Ctrl Pts',(31.4029003397019,618.661159188947,-37.7155475642533)) ;
#59254 = CARTESIAN_POINT('Ctrl Pts',(31.4281291215752,618.65704726354,-37.6603580556468)) ;
#59255 = CARTESIAN_POINT('Ctrl Pts',(31.4503869748622,618.653012783546,-37.6037887980431)) ;
#59256 = CARTESIAN_POINT('Ctrl Pts',(31.4695315749085,618.649052449208,-37.5461898742506)) ;
#59257 = CARTESIAN_POINT('Ctrl Pts',(31.4886923015302,618.645088778857,-37.4885424316393)) ;
#59258 = CARTESIAN_POINT('Ctrl Pts',(31.5047343325093,618.641199255126,-37.4298635887972)) ;
#59259 = CARTESIAN_POINT('Ctrl Pts',(31.5175481043101,618.637356933796,-37.3705198260656)) ;
#59260 = CARTESIAN_POINT('Ctrl Pts',(31.5303666885878,618.633513169403,-37.311153775557)) ;
#59261 = CARTESIAN_POINT('Ctrl Pts',(31.539954249111,618.629716369706,-37.2511223227426)) ;
#59262 = CARTESIAN_POINT('Ctrl Pts',(31.5462382095542,618.625918855984,-37.1908077727697)) ;
#59263 = CARTESIAN_POINT('Ctrl Pts',(31.5525341048052,618.622114129837,-37.1303786704265)) ;
#59264 = CARTESIAN_POINT('Ctrl Pts',(31.5555133084016,618.618308212986,-37.0696654927814)) ;
#59265 = CARTESIAN_POINT('Ctrl Pts',(31.555146597125,618.614437917341,-37.0090674408427)) ;
#59266 = CARTESIAN_POINT('Ctrl Pts',(31.5548170738568,618.610960106454,-36.9546146072387)) ;
#59267 = CARTESIAN_POINT('Ctrl Pts',(31.5517858889841,618.607429722511,-36.9002543398607)) ;
#59268 = CARTESIAN_POINT('Ctrl Pts',(31.5460685179213,618.603796420824,-36.8462866158652)) ;
#59269 = CARTESIAN_POINT('Ctrl Pts',(31.545556999344,618.603471358608,-36.8414582615226)) ;
#59270 = CARTESIAN_POINT('Ctrl Pts',(31.5450239981011,618.603145472594,-36.8366330202235)) ;
#59271 = CARTESIAN_POINT('Ctrl Pts',(31.5444695359318,618.60281872673,-36.8318110893893)) ;
#59272 = CARTESIAN_POINT('Ctrl Pts',(31.5444657676938,618.602816506098,-36.831778318564)) ;
#59273 = CARTESIAN_POINT('Ctrl Pts',(31.5444619984646,618.602814285427,-36.8317455478917)) ;
#59274 = CARTESIAN_POINT('Ctrl Pts',(31.5444582282442,618.602812064716,-36.8317127773723)) ;
#59275 = CARTESIAN_POINT('Ctrl Pts',(31.5381108427545,618.599073368529,-36.7765417002896)) ;
#59276 = CARTESIAN_POINT('Ctrl Pts',(31.5289226744486,618.595212190571,-36.7216055721164)) ;
#59277 = CARTESIAN_POINT('Ctrl Pts',(31.5169560025884,618.591291590598,-36.6672070009179)) ;
#59278 = CARTESIAN_POINT('Ctrl Pts',(31.5158419372211,618.590926593153,-36.6621426384192)) ;
#59279 = CARTESIAN_POINT('Ctrl Pts',(31.5147038169095,618.590561080691,-36.6570829610815)) ;
#59280 = CARTESIAN_POINT('Ctrl Pts',(31.5135417086785,618.590195104094,-36.6520282286846)) ;
#59281 = CARTESIAN_POINT('Ctrl Pts',(31.4997587502424,618.585854509907,-36.5920775591406)) ;
#59282 = CARTESIAN_POINT('Ctrl Pts',(31.4825975136841,618.58144928703,-36.5328179968727)) ;
#59283 = CARTESIAN_POINT('Ctrl Pts',(31.4621857936471,618.577050252619,-36.4746349590504)) ;
#59284 = CARTESIAN_POINT('Ctrl Pts',(31.4420337111258,618.572707174019,-36.4171920107145)) ;
#59285 = CARTESIAN_POINT('Ctrl Pts',(31.4187136805253,618.568370419492,-36.3607981428071)) ;
#59286 = CARTESIAN_POINT('Ctrl Pts',(31.3923820323704,618.564087593537,-36.3058038966044)) ;
#59287 = CARTESIAN_POINT('Ctrl Pts',(31.3660662969591,618.55980735578,-36.2508428845287)) ;
#59288 = CARTESIAN_POINT('Ctrl Pts',(31.3367426822218,618.555581116504,-36.197279718318)) ;
#59289 = CARTESIAN_POINT('Ctrl Pts',(31.3045974844214,618.551432583277,-36.1454461744282)) ;
#59290 = CARTESIAN_POINT('Ctrl Pts',(31.2724598498184,618.547285026127,-36.0936248260561)) ;
#59291 = CARTESIAN_POINT('Ctrl Pts',(31.2375019420153,618.543215140447,-36.0435323174582)) ;
#59292 = CARTESIAN_POINT('Ctrl Pts',(31.1999396127379,618.539221816271,-35.9954824563047)) ;
#59293 = CARTESIAN_POINT('Ctrl Pts',(31.1614845324218,618.535133581999,-35.9462905849436)) ;
#59294 = CARTESIAN_POINT('Ctrl Pts',(31.1202995205151,618.531125564924,-35.8992398452946)) ;
#59295 = CARTESIAN_POINT('Ctrl Pts',(31.0766494256803,618.527170583501,-35.8546462743732)) ;
#59296 = CARTESIAN_POINT('Ctrl Pts',(31.0339583163552,618.523302492379,-35.8110324169781)) ;
#59297 = CARTESIAN_POINT('Ctrl Pts',(30.9889091924407,618.519484778323,-35.7697691473266)) ;
#59298 = CARTESIAN_POINT('Ctrl Pts',(30.9417830813077,618.515670566426,-35.7311296085355)) ;
#59299 = CARTESIAN_POINT('Ctrl Pts',(30.8930690543857,618.511727834539,-35.6911881092758)) ;
#59300 = CARTESIAN_POINT('Ctrl Pts',(30.8421352602933,618.50778841439,-35.6540508351474)) ;
#59301 = CARTESIAN_POINT('Ctrl Pts',(30.7893324095246,618.503782920354,-35.6199881496201)) ;
#59302 = CARTESIAN_POINT('Ctrl Pts',(30.7433891606403,618.500297778799,-35.5903505369521)) ;
#59303 = CARTESIAN_POINT('Ctrl Pts',(30.6960302507629,618.496761965997,-35.5630399679191)) ;
#59304 = CARTESIAN_POINT('Ctrl Pts',(30.6475172782936,618.493124863879,-35.5382100550777)) ;
#59305 = CARTESIAN_POINT('Ctrl Pts',(30.640301374707,618.492583875008,-35.5345168108173)) ;
#59306 = CARTESIAN_POINT('Ctrl Pts',(30.6330599000393,618.492040645201,-35.530878363005)) ;
#59307 = CARTESIAN_POINT('Ctrl Pts',(30.6257936722541,618.491495007886,-35.5272951280833)) ;
#59308 = CARTESIAN_POINT('Ctrl Pts',(30.6257661079495,618.491492938021,-35.5272815351459)) ;
#59309 = CARTESIAN_POINT('Ctrl Pts',(30.6257385432886,618.491490868121,-35.5272679430031)) ;
#59310 = CARTESIAN_POINT('Ctrl Pts',(30.6257109782715,618.491488798186,-35.5272543516547)) ;
#59311 = CARTESIAN_POINT('Ctrl Pts',(30.5759895713561,618.487755077898,-35.5027384603596)) ;
#59312 = CARTESIAN_POINT('Ctrl Pts',(30.5249275120125,618.483898811178,-35.4807273012484)) ;
#59313 = CARTESIAN_POINT('Ctrl Pts',(30.4728117649734,618.479983217499,-35.461332928774)) ;
#59314 = CARTESIAN_POINT('Ctrl Pts',(30.4679799255449,618.479620188645,-35.4595348063458)) ;
#59315 = CARTESIAN_POINT('Ctrl Pts',(30.4631390649157,618.479256649827,-35.4577591692149)) ;
#59316 = CARTESIAN_POINT('Ctrl Pts',(30.458289433724,618.478892651429,-35.4560061011717)) ;
#59317 = CARTESIAN_POINT('Ctrl Pts',(30.4004223207642,618.474549323946,-35.4350880184408)) ;
#59318 = CARTESIAN_POINT('Ctrl Pts',(30.3413005195102,618.470141228125,-35.4173842219975)) ;
#59319 = CARTESIAN_POINT('Ctrl Pts',(30.281318183977,618.465739742904,-35.4029973618508)) ;
#59320 = CARTESIAN_POINT('Ctrl Pts',(30.2222367147747,618.461404362975,-35.3888265759499)) ;
#59321 = CARTESIAN_POINT('Ctrl Pts',(30.1623203746084,618.457075679211,-35.3778733946167)) ;
#59322 = CARTESIAN_POINT('Ctrl Pts',(30.1019469813105,618.452801348568,-35.3701968730303)) ;
#59323 = CARTESIAN_POINT('Ctrl Pts',(30.0416110635627,618.448529671129,-35.3625251164877)) ;
#59324 = CARTESIAN_POINT('Ctrl Pts',(29.9808186466924,618.444312413336,-35.3581258264937)) ;
#59325 = CARTESIAN_POINT('Ctrl Pts',(29.9199481378645,618.440173371419,-35.3570227113294)) ;
#59326 = CARTESIAN_POINT('Ctrl Pts',(29.8590927072241,618.436035354782,-35.3559198694169)) ;
#59327 = CARTESIAN_POINT('Ctrl Pts',(29.7981592444871,618.431975517372,-35.3581116017446)) ;
#59328 = CARTESIAN_POINT('Ctrl Pts',(29.7375271299118,618.427992883047,-35.3635870253733)) ;
#59329 = CARTESIAN_POINT('Ctrl Pts',(29.6752004343361,618.423898939782,-35.3692154792717)) ;
#59330 = CARTESIAN_POINT('Ctrl Pts',(29.6131922391728,618.419886566595,-35.3783140957345)) ;
#59331 = CARTESIAN_POINT('Ctrl Pts',(29.5519152757824,618.415928380366,-35.3908313429493)) ;
#59332 = CARTESIAN_POINT('Ctrl Pts',(29.4922285529616,618.412072915747,-35.4030237464832)) ;
#59333 = CARTESIAN_POINT('Ctrl Pts',(29.4332357413764,618.408268493894,-35.4184597707061)) ;
#59334 = CARTESIAN_POINT('Ctrl Pts',(29.3753173076147,618.404468336497,-35.4370515913484)) ;
#59335 = CARTESIAN_POINT('Ctrl Pts',(29.3150841821071,618.40051630702,-35.4563864281773)) ;
#59336 = CARTESIAN_POINT('Ctrl Pts',(29.2560133821818,618.396568471163,-35.4791351648903)) ;
#59337 = CARTESIAN_POINT('Ctrl Pts',(29.1985281518379,618.392554218511,-35.5051471697204)) ;
#59338 = CARTESIAN_POINT('Ctrl Pts',(29.148800094153,618.389081657189,-35.5276490622754)) ;
#59339 = CARTESIAN_POINT('Ctrl Pts',(29.1002576320191,618.385558736114,-35.5525931822916)) ;
#59340 = CARTESIAN_POINT('Ctrl Pts',(29.0531707881797,618.381934784252,-35.5798429037858)) ;
#59341 = CARTESIAN_POINT('Ctrl Pts',(29.0458515041979,618.381371469095,-35.5840786612454)) ;
#59342 = CARTESIAN_POINT('Ctrl Pts',(29.0385672899433,618.380805712803,-35.5883701117772)) ;
#59343 = CARTESIAN_POINT('Ctrl Pts',(29.031319046969,618.380237325065,-35.5927167281838)) ;
#59344 = CARTESIAN_POINT('Ctrl Pts',(29.0312934173751,618.380235315261,-35.5927320977036)) ;
#59345 = CARTESIAN_POINT('Ctrl Pts',(29.0312677882308,618.380233305424,-35.5927474679131)) ;
#59346 = CARTESIAN_POINT('Ctrl Pts',(29.0312421595363,618.380231295554,-35.5927628388123)) ;
#59347 = CARTESIAN_POINT('Ctrl Pts',(28.9837044478577,618.376503263034,-35.6212737476888)) ;
#59348 = CARTESIAN_POINT('Ctrl Pts',(28.9375467752205,618.372652138925,-35.6522677068982)) ;
#59349 = CARTESIAN_POINT('Ctrl Pts',(28.8930184784191,618.368741066252,-35.6855640604781)) ;
#59350 = CARTESIAN_POINT('Ctrl Pts',(28.8888546870006,618.368375346205,-35.6886775654011)) ;
#59351 = CARTESIAN_POINT('Ctrl Pts',(28.8847051555669,618.368009101972,-35.691811166888)) ;
#59352 = CARTESIAN_POINT('Ctrl Pts',(28.8805700953766,618.367642385182,-35.6949646952095)) ;
#59353 = CARTESIAN_POINT('Ctrl Pts',(28.8316436881913,618.363303358867,-35.7322775283065)) ;
#59354 = CARTESIAN_POINT('Ctrl Pts',(28.7847407909223,618.358898842722,-35.7723855885088)) ;
#59355 = CARTESIAN_POINT('Ctrl Pts',(28.7401608122143,618.354500231938,-35.8150129554806)) ;
#59356 = CARTESIAN_POINT('Ctrl Pts',(28.6962222493042,618.350164908274,-35.8570270007912)) ;
#59357 = CARTESIAN_POINT('Ctrl Pts',(28.6545398706444,618.34583560831,-35.9014881307113)) ;
#59358 = CARTESIAN_POINT('Ctrl Pts',(28.6153680467039,618.341560153364,-35.9481101168694)) ;
#59359 = CARTESIAN_POINT('Ctrl Pts',(28.5762202788798,618.337287324051,-35.9947034716336)) ;
#59360 = CARTESIAN_POINT('Ctrl Pts',(28.539579866489,618.333068408917,-36.0434549721131)) ;
#59361 = CARTESIAN_POINT('Ctrl Pts',(28.5056717224049,618.32892735311,-36.0940588161533)) ;
#59362 = CARTESIAN_POINT('Ctrl Pts',(28.4717717941343,618.324787300665,-36.1446503990759)) ;
#59363 = CARTESIAN_POINT('Ctrl Pts',(28.4406028467046,618.320725072517,-36.1970934286391)) ;
#59364 = CARTESIAN_POINT('Ctrl Pts',(28.4123612160282,618.316739811669,-36.2510626063029)) ;
#59365 = CARTESIAN_POINT('Ctrl Pts',(28.38336289804,618.312647772415,-36.3064777979177)) ;
#59366 = CARTESIAN_POINT('Ctrl Pts',(28.3574511941756,618.30863686713,-36.3635021437826)) ;
#59367 = CARTESIAN_POINT('Ctrl Pts',(28.3348057428245,618.30467990851,-36.4217615767189)) ;
#59368 = CARTESIAN_POINT('Ctrl Pts',(28.3127230432915,618.30082128247,-36.478573230969)) ;
#59369 = CARTESIAN_POINT('Ctrl Pts',(28.2937464644792,618.297013591652,-36.5365593056891)) ;
#59370 = CARTESIAN_POINT('Ctrl Pts',(28.2780083026968,618.293210123154,-36.5953520015067)) ;
#59371 = CARTESIAN_POINT('Ctrl Pts',(28.2616685378942,618.289261264225,-36.6563920921512)) ;
#59372 = CARTESIAN_POINT('Ctrl Pts',(28.2488203709418,618.285316536279,-36.7183017893232)) ;
#59373 = CARTESIAN_POINT('Ctrl Pts',(28.2395660305023,618.281305714831,-36.7806454803147)) ;
#59374 = CARTESIAN_POINT('Ctrl Pts',(28.2315445039564,618.277829193633,-36.8346840771793)) ;
#59375 = CARTESIAN_POINT('Ctrl Pts',(28.2262227954632,618.274302359799,-36.889049637097)) ;
#59376 = CARTESIAN_POINT('Ctrl Pts',(28.2236324605726,618.270674475694,-36.9434406507769)) ;
#59377 = CARTESIAN_POINT('Ctrl Pts',(28.223235763576,618.270118883158,-36.9517703659216)) ;
#59378 = CARTESIAN_POINT('Ctrl Pts',(28.2229030607497,618.26956092065,-36.960100752751)) ;
#59379 = CARTESIAN_POINT('Ctrl Pts',(28.2226343961012,618.26900040593,-36.9684308115211)) ;
#59380 = CARTESIAN_POINT('Ctrl Pts',(28.2226334432837,618.268998418067,-36.9684603540242)) ;
#59381 = CARTESIAN_POINT('Ctrl Pts',(28.2226324912715,618.268996430173,-36.9684898965232)) ;
#59382 = CARTESIAN_POINT('Ctrl Pts',(28.2226315400648,618.268994442247,-36.9685194390181)) ;
#59383 = CARTESIAN_POINT('Ctrl Pts',(28.2208468079136,618.26526453179,-37.0239494927733)) ;
#59384 = CARTESIAN_POINT('Ctrl Pts',(28.2218993982417,618.261411768754,-37.0795641973424)) ;
#59385 = CARTESIAN_POINT('Ctrl Pts',(28.2257723975202,618.257499301475,-37.1350557789974)) ;
#59386 = CARTESIAN_POINT('Ctrl Pts',(28.2261333900683,618.257134630213,-37.1402280101343)) ;
#59387 = CARTESIAN_POINT('Ctrl Pts',(28.2265188627023,618.256769440263,-37.1453991418306)) ;
#59388 = CARTESIAN_POINT('Ctrl Pts',(28.2269287873742,618.256403782759,-37.1505689068973)) ;
#59389 = CARTESIAN_POINT('Ctrl Pts',(28.2317923068705,618.252065467639,-37.2119051838194)) ;
#59390 = CARTESIAN_POINT('Ctrl Pts',(28.2401011002908,618.247662003083,-37.2730541153256)) ;
#59391 = CARTESIAN_POINT('Ctrl Pts',(28.2517853580537,618.24326465075,-37.3336147428047)) ;
#59392 = CARTESIAN_POINT('Ctrl Pts',(28.2633042205175,618.238929544683,-37.3933181106021)) ;
#59393 = CARTESIAN_POINT('Ctrl Pts',(28.2781032539723,618.234600666219,-37.4524498885658)) ;
#59394 = CARTESIAN_POINT('Ctrl Pts',(28.2960795570283,618.230325746232,-37.51064111304)) ;
#59395 = CARTESIAN_POINT('Ctrl Pts',(28.3140448906859,618.226053434863,-37.5687968283932)) ;
#59396 = CARTESIAN_POINT('Ctrl Pts',(28.3351835064466,618.221835151049,-37.6260132048384)) ;
#59397 = CARTESIAN_POINT('Ctrl Pts',(28.3593600959597,618.217694743611,-37.6819354353026)) ;
#59398 = CARTESIAN_POINT('Ctrl Pts',(28.3835309127598,618.21355532479,-37.7378443130568)) ;
#59399 = CARTESIAN_POINT('Ctrl Pts',(28.41073827333,618.209493747495,-37.7924596325546)) ;
#59400 = CARTESIAN_POINT('Ctrl Pts',(28.4408149988073,618.205509057314,-37.8454400449)) ;
#59401 = CARTESIAN_POINT('Ctrl Pts',(28.4716846556205,618.201419316279,-37.899817212659)) ;
#59402 = CARTESIAN_POINT('Ctrl Pts',(28.5055772510173,618.197410554523,-37.9524719262378)) ;
#59403 = CARTESIAN_POINT('Ctrl Pts',(28.5422758315809,618.193455524331,-38.003050887678)) ;
#59404 = CARTESIAN_POINT('Ctrl Pts',(28.578077631573,618.189597140771,-38.0523938822431)) ;
#59405 = CARTESIAN_POINT('Ctrl Pts',(28.6165500236072,618.185789532356,-38.0997611500694)) ;
#59406 = CARTESIAN_POINT('Ctrl Pts',(28.6574553993652,618.181985915573,-38.1448421396957)) ;
#59407 = CARTESIAN_POINT('Ctrl Pts',(28.6998977011823,618.178039386579,-38.1916169445344)) ;
#59408 = CARTESIAN_POINT('Ctrl Pts',(28.744959830827,618.17409673234,-38.2359297901857)) ;
#59409 = CARTESIAN_POINT('Ctrl Pts',(28.7923314482007,618.170087815097,-38.2774592594093)) ;
#59410 = CARTESIAN_POINT('Ctrl Pts',(28.8334067265285,618.166611738056,-38.3134688913732)) ;
#59411 = CARTESIAN_POINT('Ctrl Pts',(28.8762189636619,618.163085187076,-38.3473865949876)) ;
#59412 = CARTESIAN_POINT('Ctrl Pts',(28.9205319247919,618.159457468053,-38.3790226032246)) ;
#59413 = CARTESIAN_POINT('Ctrl Pts',(28.927300312747,618.158903368099,-38.383854705879)) ;
#59414 = CARTESIAN_POINT('Ctrl Pts',(28.9341037390459,618.158346907925,-38.3886336726395)) ;
#59415 = CARTESIAN_POINT('Ctrl Pts',(28.9409413939369,618.15778790689,-38.3933589298167)) ;
#59416 = CARTESIAN_POINT('Ctrl Pts',(28.9409658904565,618.157785904218,-38.3933758584796)) ;
#59417 = CARTESIAN_POINT('Ctrl Pts',(28.9409903874154,618.157783901514,-38.3933927864532)) ;
#59418 = CARTESIAN_POINT('Ctrl Pts',(28.9410148848135,618.157781898776,-38.3934097137375)) ;
#59419 = CARTESIAN_POINT('Ctrl Pts',(28.9869438604082,618.154027064591,-38.4251458524531)) ;
#59420 = CARTESIAN_POINT('Ctrl Pts',(29.0345829173173,618.150147935566,-38.454563664042)) ;
#59421 = CARTESIAN_POINT('Ctrl Pts',(29.0836625571254,618.146208705783,-38.4815110330523)) ;
#59422 = CARTESIAN_POINT('Ctrl Pts',(29.088569528916,618.14581486244,-38.4842052251874)) ;
#59423 = CARTESIAN_POINT('Ctrl Pts',(29.0934908577691,618.145420418332,-38.4868747247128)) ;
#59424 = CARTESIAN_POINT('Ctrl Pts',(29.0984262458447,618.145025437615,-38.4895193815645)) ;
#59425 = CARTESIAN_POINT('Ctrl Pts',(29.1526346499945,618.140687121352,-38.5185672751158)) ;
#59426 = CARTESIAN_POINT('Ctrl Pts',(29.2085451927026,618.136284701166,-38.5446184457616)) ;
#59427 = CARTESIAN_POINT('Ctrl Pts',(29.2657894773234,618.131888823386,-38.5675167492335)) ;
#59428 = CARTESIAN_POINT('Ctrl Pts',(29.3229458365822,618.127499697532,-38.590379881655)) ;
#59429 = CARTESIAN_POINT('Ctrl Pts',(29.3814318336443,618.123117430252,-38.6101002015592)) ;
#59430 = CARTESIAN_POINT('Ctrl Pts',(29.4408743003571,618.118790860888,-38.6265597151448)) ;
#59431 = CARTESIAN_POINT('Ctrl Pts',(29.5002633325708,618.114468180799,-38.6430044328125)) ;
#59432 = CARTESIAN_POINT('Ctrl Pts',(29.5606071605186,618.110201238562,-38.6561943411892)) ;
#59433 = CARTESIAN_POINT('Ctrl Pts',(29.621526796277,618.106013793532,-38.666045369854)) ;
#59434 = CARTESIAN_POINT('Ctrl Pts',(29.6824149151413,618.101828514884,-38.6758913020695)) ;
#59435 = CARTESIAN_POINT('Ctrl Pts',(29.7438782808071,618.097722656485,-38.6824017641329)) ;
#59436 = CARTESIAN_POINT('Ctrl Pts',(29.8055310461891,618.093693952894,-38.6855257554669)) ;
#59437 = CARTESIAN_POINT('Ctrl Pts',(29.8334581163121,618.091869056849,-38.6869408408163)) ;
#59438 = CARTESIAN_POINT('Ctrl Pts',(29.8614239439526,618.090059638097,-38.6876615252047)) ;
#59439 = CARTESIAN_POINT('Ctrl Pts',(29.8893921427819,618.088263764204,-38.6876853814548)) ;
#59440 = CARTESIAN_POINT('Ctrl Pts',(29.8893746478611,618.087990585226,-38.6881599564327)) ;
#59441 = CARTESIAN_POINT('Ctrl Pts',(29.9622844351597,618.083368135722,-38.6881228878649)) ;
#59442 = CARTESIAN_POINT('Ctrl Pts',(30.0351169275643,618.07887743536,-38.683299808865)) ;
#59443 = CARTESIAN_POINT('Ctrl Pts',(30.2114913540784,618.067997029309,-38.6599253324782)) ;
#59444 = CARTESIAN_POINT('Ctrl Pts',(30.3140297828991,618.0616708931,-38.6363236340286)) ;
#59445 = CARTESIAN_POINT('Ctrl Pts',(30.4305569294752,618.053832960999,-38.5976212057701)) ;
#59446 = CARTESIAN_POINT('Ctrl Pts',(30.4473670450482,618.052685496838,-38.5917370547404)) ;
#59447 = CARTESIAN_POINT('Ctrl Pts',(30.4640776573931,618.051524931058,-38.5855853092948)) ;
#59448 = CARTESIAN_POINT('Origin',(179.888527625422,617.710565160536,-37.0221601717597)) ;
#59449 = CARTESIAN_POINT('',(180.464123912022,616.842332842895,-38.5858650494033)) ;
#59450 = CARTESIAN_POINT('',(180.464060715702,616.710565160536,-38.5855915460107)) ;
#59451 = CARTESIAN_POINT('',(180.464060715702,617.710565160536,-38.5855915460107)) ;
#59452 = CARTESIAN_POINT('',(181.553667127593,616.710572776564,-37.0987295421981)) ;
#59453 = CARTESIAN_POINT('Origin',(179.888527625422,616.710565160536,-37.0221601717597)) ;
#59454 = CARTESIAN_POINT('Ctrl Pts',(181.553667143704,616.710572776701,-37.0987295429389)) ;
#59455 = CARTESIAN_POINT('Ctrl Pts',(181.551219015739,616.71416598167,-37.1513058672652)) ;
#59456 = CARTESIAN_POINT('Ctrl Pts',(181.546218975108,616.717855507709,-37.2038530482861)) ;
#59457 = CARTESIAN_POINT('Ctrl Pts',(181.538699664615,616.721587750684,-37.2561056544767)) ;
#59458 = CARTESIAN_POINT('Ctrl Pts',(181.530086063372,616.725863149705,-37.3159626206176)) ;
#59459 = CARTESIAN_POINT('Ctrl Pts',(181.518166274836,616.730194042225,-37.3754342915452)) ;
#59460 = CARTESIAN_POINT('Ctrl Pts',(181.503027609458,616.734514285927,-37.4341435669554)) ;
#59461 = CARTESIAN_POINT('Ctrl Pts',(181.487904369475,616.738830127558,-37.492793021121)) ;
#59462 = CARTESIAN_POINT('Ctrl Pts',(181.469569088151,616.743135044131,-37.5506817707635)) ;
#59463 = CARTESIAN_POINT('Ctrl Pts',(181.448143519656,616.747383864401,-37.6074499818234)) ;
#59464 = CARTESIAN_POINT('Ctrl Pts',(181.426731654152,616.751629967285,-37.6641818860634)) ;
#59465 = CARTESIAN_POINT('Ctrl Pts',(181.402233542896,616.755819927562,-37.7197947350221)) ;
#59466 = CARTESIAN_POINT('Ctrl Pts',(181.374802719427,616.759932463143,-37.7739440349984)) ;
#59467 = CARTESIAN_POINT('Ctrl Pts',(181.347379033597,616.76404392862,-37.8280792450522)) ;
#59468 = CARTESIAN_POINT('Ctrl Pts',(181.317024134035,616.768078019286,-37.8807516162109)) ;
#59469 = CARTESIAN_POINT('Ctrl Pts',(181.283923023809,616.772038052194,-37.9316315845311)) ;
#59470 = CARTESIAN_POINT('Ctrl Pts',(181.250794021577,616.776001421948,-37.9825544258659)) ;
#59471 = CARTESIAN_POINT('Ctrl Pts',(181.214914057745,616.779890733246,-38.0316816889812)) ;
#59472 = CARTESIAN_POINT('Ctrl Pts',(181.176501382908,616.783732952265,-38.0786991995177)) ;
#59473 = CARTESIAN_POINT('Ctrl Pts',(181.138074270226,616.787576615427,-38.1257343821257)) ;
#59474 = CARTESIAN_POINT('Ctrl Pts',(181.097112343844,616.791373424309,-38.1706579499562)) ;
#59475 = CARTESIAN_POINT('Ctrl Pts',(181.053869293275,616.795171081348,-38.2131747791317)) ;
#59476 = CARTESIAN_POINT('Ctrl Pts',(181.010544127622,616.798975949833,-38.255772344356)) ;
#59477 = CARTESIAN_POINT('Ctrl Pts',(180.964928911648,616.802782144032,-38.2959535452537)) ;
#59478 = CARTESIAN_POINT('Ctrl Pts',(180.917317584923,616.806652873016,-38.3334466202017)) ;
#59479 = CARTESIAN_POINT('Ctrl Pts',(180.874538611528,616.810130738969,-38.3671343026506)) ;
#59480 = CARTESIAN_POINT('Ctrl Pts',(180.830147886244,616.813661294112,-38.3986521148746)) ;
#59481 = CARTESIAN_POINT('Ctrl Pts',(180.784389550097,616.817294877271,-38.4278251727132)) ;
#59482 = CARTESIAN_POINT('Ctrl Pts',(180.780328267656,616.817617376049,-38.4304144283009)) ;
#59483 = CARTESIAN_POINT('Ctrl Pts',(180.776256201053,616.817940686425,-38.4329852454072)) ;
#59484 = CARTESIAN_POINT('Ctrl Pts',(180.77217351419,616.818264843595,-38.4355375204749)) ;
#59485 = CARTESIAN_POINT('Ctrl Pts',(180.772144653369,616.818267135086,-38.435555562699)) ;
#59486 = CARTESIAN_POINT('Ctrl Pts',(180.772115792019,616.81826942662,-38.4355736039966)) ;
#59487 = CARTESIAN_POINT('Ctrl Pts',(180.772086930137,616.818271718196,-38.4355916443677)) ;
#59488 = CARTESIAN_POINT('Ctrl Pts',(180.724316691767,616.822064580185,-38.4654508490374)) ;
#59489 = CARTESIAN_POINT('Ctrl Pts',(180.674926046349,616.825982750278,-38.4928664980066)) ;
#59490 = CARTESIAN_POINT('Ctrl Pts',(180.624194942044,616.82996095168,-38.5177002140637)) ;
#59491 = CARTESIAN_POINT('Ctrl Pts',(180.618794683314,616.83038442594,-38.5203437301822)) ;
#59492 = CARTESIAN_POINT('Ctrl Pts',(180.61337928401,616.830808580434,-38.5229579922498)) ;
#59493 = CARTESIAN_POINT('Ctrl Pts',(180.607949116393,616.831233336425,-38.5255428361978)) ;
#59494 = CARTESIAN_POINT('Ctrl Pts',(180.561039635885,616.834902667516,-38.5478724759674)) ;
#59495 = CARTESIAN_POINT('Ctrl Pts',(180.513023781992,616.838616789469,-38.5680076336995)) ;
#59496 = CARTESIAN_POINT('Ctrl Pts',(180.464123912022,616.842332842895,-38.5858650494033)) ;
#59497 = CARTESIAN_POINT('Origin',(179.888527625422,617.710565160536,-37.0221601717597)) ;
#59498 = CARTESIAN_POINT('',(180.464060722638,617.544113575794,-38.5855915434574)) ;
#59499 = CARTESIAN_POINT('',(180.464050813976,617.349688765578,-38.5855724216838)) ;
#59500 = CARTESIAN_POINT('',(180.464060715702,617.710565160536,-38.5855915460107)) ;
#59501 = CARTESIAN_POINT('',(179.569297170793,616.710565160536,-38.6572894990111)) ;
#59502 = CARTESIAN_POINT('Ctrl Pts',(180.464050813976,617.349688765578,-38.5855724216838)) ;
#59503 = CARTESIAN_POINT('Ctrl Pts',(180.521067355346,617.345363131574,-38.5644227170943)) ;
#59504 = CARTESIAN_POINT('Ctrl Pts',(180.576979882282,617.341060163679,-38.5401406905439)) ;
#59505 = CARTESIAN_POINT('Ctrl Pts',(180.63144191744,617.336820795064,-38.5128859853913)) ;
#59506 = CARTESIAN_POINT('Ctrl Pts',(180.685876495539,617.332583563729,-38.4856450207099)) ;
#59507 = CARTESIAN_POINT('Ctrl Pts',(180.73886209061,617.328409959241,-38.4554344345994)) ;
#59508 = CARTESIAN_POINT('Ctrl Pts',(180.790070116881,617.324316560357,-38.4224438033602)) ;
#59509 = CARTESIAN_POINT('Ctrl Pts',(180.841271368363,617.320223703028,-38.38945753676)) ;
#59510 = CARTESIAN_POINT('Ctrl Pts',(180.890695456401,617.316210998305,-38.3536919176301)) ;
#59511 = CARTESIAN_POINT('Ctrl Pts',(180.938031441646,617.31227029805,-38.3153665301434)) ;
#59512 = CARTESIAN_POINT('Ctrl Pts',(180.985413050195,617.308325799675,-38.2770042039347)) ;
#59513 = CARTESIAN_POINT('Ctrl Pts',(181.030702350892,617.304453294816,-38.2360770441486)) ;
#59514 = CARTESIAN_POINT('Ctrl Pts',(181.073606872153,617.300621180435,-38.1928367164287)) ;
#59515 = CARTESIAN_POINT('Ctrl Pts',(181.116531800229,617.296787243374,-38.1495758221731)) ;
#59516 = CARTESIAN_POINT('Ctrl Pts',(181.157069360915,617.292993425576,-38.1039993639689)) ;
#59517 = CARTESIAN_POINT('Ctrl Pts',(181.194949715568,617.289188038191,-38.0563932722058)) ;
#59518 = CARTESIAN_POINT('Ctrl Pts',(181.232901550976,617.285375469987,-38.008697347087)) ;
#59519 = CARTESIAN_POINT('Ctrl Pts',(181.268185598401,617.281550762776,-37.9589639018266)) ;
#59520 = CARTESIAN_POINT('Ctrl Pts',(181.300560023502,617.27764802761,-37.9075177337117)) ;
#59521 = CARTESIAN_POINT('Ctrl Pts',(181.326651139868,617.274502744968,-37.8660563655292)) ;
#59522 = CARTESIAN_POINT('Ctrl Pts',(181.350852802808,617.271306321776,-37.8234832859932)) ;
#59523 = CARTESIAN_POINT('Ctrl Pts',(181.373056836464,617.268022027636,-37.7799871945257)) ;
#59524 = CARTESIAN_POINT('Ctrl Pts',(181.373070496917,617.268020007059,-37.7799604346884)) ;
#59525 = CARTESIAN_POINT('Ctrl Pts',(181.373084156616,617.268017986449,-37.7799336745013)) ;
#59526 = CARTESIAN_POINT('Ctrl Pts',(181.373097815559,617.268015965807,-37.7799069139645)) ;
#59527 = CARTESIAN_POINT('Ctrl Pts',(181.398284435998,617.26428996986,-37.7305614064458)) ;
#59528 = CARTESIAN_POINT('Ctrl Pts',(181.420987785486,617.26044103349,-37.6798426520705)) ;
#59529 = CARTESIAN_POINT('Ctrl Pts',(181.441092167919,617.256532284097,-37.6280356574811)) ;
#59530 = CARTESIAN_POINT('Ctrl Pts',(181.442970993693,617.256166997616,-37.6231941102701)) ;
#59531 = CARTESIAN_POINT('Ctrl Pts',(181.444827129073,617.255801188755,-37.6183430956054)) ;
#59532 = CARTESIAN_POINT('Ctrl Pts',(181.44666048504,617.255434909036,-37.6134828686495)) ;
#59533 = CARTESIAN_POINT('Ctrl Pts',(181.468379666709,617.251095710374,-37.5559053146194)) ;
#59534 = CARTESIAN_POINT('Ctrl Pts',(181.486901038978,617.246691099595,-37.4970289075518)) ;
#59535 = CARTESIAN_POINT('Ctrl Pts',(181.50211674275,617.242292615532,-37.4372466548332)) ;
#59536 = CARTESIAN_POINT('Ctrl Pts',(181.517103241382,617.237960389013,-37.378364945384)) ;
#59537 = CARTESIAN_POINT('Ctrl Pts',(181.528883363017,617.233634390947,-37.3186044913533)) ;
#59538 = CARTESIAN_POINT('Ctrl Pts',(181.53739314816,617.229362469258,-37.2583424046209)) ;
#59539 = CARTESIAN_POINT('Ctrl Pts',(181.545897740001,617.225093154612,-37.1981170942769)) ;
#59540 = CARTESIAN_POINT('Ctrl Pts',(181.55113611504,617.220877985803,-37.1373907518155)) ;
#59541 = CARTESIAN_POINT('Ctrl Pts',(181.553079682457,617.216740970537,-37.0765414751807)) ;
#59542 = CARTESIAN_POINT('Ctrl Pts',(181.555022788807,617.212604936685,-37.0157066336646)) ;
#59543 = CARTESIAN_POINT('Ctrl Pts',(181.553672620198,617.208547022454,-36.9547489367615)) ;
#59544 = CARTESIAN_POINT('Ctrl Pts',(181.549035161303,617.204566464328,-36.8940478445899)) ;
#59545 = CARTESIAN_POINT('Ctrl Pts',(181.544267852721,617.200474449854,-36.8316471108539)) ;
#59546 = CARTESIAN_POINT('Ctrl Pts',(181.536026230921,617.196464176835,-36.7695176204549)) ;
#59547 = CARTESIAN_POINT('Ctrl Pts',(181.524356469931,617.1925084719,-36.7080726968388)) ;
#59548 = CARTESIAN_POINT('Ctrl Pts',(181.512989833439,617.188655517234,-36.6482238180451)) ;
#59549 = CARTESIAN_POINT('Ctrl Pts',(181.498370712369,617.18485396578,-36.5890245417342)) ;
#59550 = CARTESIAN_POINT('Ctrl Pts',(181.480581926585,617.181057197148,-36.5308563210037)) ;
#59551 = CARTESIAN_POINT('Ctrl Pts',(181.462081556055,617.177108550662,-36.4703612625095)) ;
#59552 = CARTESIAN_POINT('Ctrl Pts',(181.440152039501,617.173164661938,-36.4109817420282)) ;
#59553 = CARTESIAN_POINT('Ctrl Pts',(181.414938348395,617.169155014526,-36.3531427996677)) ;
#59554 = CARTESIAN_POINT('Ctrl Pts',(181.393112096556,617.165684060042,-36.3030744730292)) ;
#59555 = CARTESIAN_POINT('Ctrl Pts',(181.368824610677,617.162163172294,-36.2541596554739)) ;
#59556 = CARTESIAN_POINT('Ctrl Pts',(181.34220910718,617.15854155645,-36.2066705884739)) ;
#59557 = CARTESIAN_POINT('Ctrl Pts',(181.338093638701,617.157981557806,-36.1993275089659)) ;
#59558 = CARTESIAN_POINT('Ctrl Pts',(181.333922525122,617.157419150812,-36.1920184182069)) ;
#59559 = CARTESIAN_POINT('Ctrl Pts',(181.329696273981,617.156854147676,-36.184744212076)) ;
#59560 = CARTESIAN_POINT('Ctrl Pts',(181.329680599364,617.156852052153,-36.184717232989)) ;
#59561 = CARTESIAN_POINT('Ctrl Pts',(181.329664923988,617.156849956594,-36.1846902543819)) ;
#59562 = CARTESIAN_POINT('Ctrl Pts',(181.329649247854,617.156847860999,-36.1846632762546)) ;
#59563 = CARTESIAN_POINT('Ctrl Pts',(181.301756420849,617.153119131574,-36.1366606097866)) ;
#59564 = CARTESIAN_POINT('Ctrl Pts',(181.271355310078,617.149267513494,-36.0900092851452)) ;
#59565 = CARTESIAN_POINT('Ctrl Pts',(181.238623991347,617.145356115883,-36.0449615989856)) ;
#59566 = CARTESIAN_POINT('Ctrl Pts',(181.235567339023,617.144990845461,-36.0407547683434)) ;
#59567 = CARTESIAN_POINT('Ctrl Pts',(181.232490400108,617.144625053704,-36.0365619363146)) ;
#59568 = CARTESIAN_POINT('Ctrl Pts',(181.229393341455,617.144258792007,-36.0323833160391)) ;
#59569 = CARTESIAN_POINT('Ctrl Pts',(181.192767074204,617.139927327777,-35.9829663433142)) ;
#59570 = CARTESIAN_POINT('Ctrl Pts',(181.153321467234,617.135530799576,-35.9355344739163)) ;
#59571 = CARTESIAN_POINT('Ctrl Pts',(181.111327896403,617.131140147732,-35.8903898196592)) ;
#59572 = CARTESIAN_POINT('Ctrl Pts',(181.069866774346,617.126805166248,-35.8458175676854)) ;
#59573 = CARTESIAN_POINT('Ctrl Pts',(181.025922137155,617.1224762055,-35.8034745375498)) ;
#59574 = CARTESIAN_POINT('Ctrl Pts',(180.979777570001,617.118200988637,-35.7636194641676)) ;
#59575 = CARTESIAN_POINT('Ctrl Pts',(180.933661057763,617.113928371014,-35.7237886218225)) ;
#59576 = CARTESIAN_POINT('Ctrl Pts',(180.885347346948,617.109709566932,-35.6864425937983)) ;
#59577 = CARTESIAN_POINT('Ctrl Pts',(180.835139953425,617.105568392055,-35.6518109058117)) ;
#59578 = CARTESIAN_POINT('Ctrl Pts',(180.784944556286,617.101428206656,-35.6171874926035)) ;
#59579 = CARTESIAN_POINT('Ctrl Pts',(180.732856377519,617.097365615128,-35.5852771577545)) ;
#59580 = CARTESIAN_POINT('Ctrl Pts',(180.67919880623,617.09337960808,-35.5562811206363)) ;
#59581 = CARTESIAN_POINT('Ctrl Pts',(180.624269322871,617.089299115755,-35.5265977544294)) ;
#59582 = CARTESIAN_POINT('Ctrl Pts',(180.567695037457,617.085298854405,-35.4999687958035)) ;
#59583 = CARTESIAN_POINT('Ctrl Pts',(180.509845044716,617.081351751734,-35.4765778642259)) ;
#59584 = CARTESIAN_POINT('Ctrl Pts',(180.453263041289,617.077491163924,-35.4536996285002)) ;
#59585 = CARTESIAN_POINT('Ctrl Pts',(180.395460668928,617.073681076396,-35.4339192356413)) ;
#59586 = CARTESIAN_POINT('Ctrl Pts',(180.336804723169,617.069874711177,-35.4173745540024)) ;
#59587 = CARTESIAN_POINT('Ctrl Pts',(180.276177078602,617.065940396342,-35.4002737287596)) ;
#59588 = CARTESIAN_POINT('Ctrl Pts',(180.214637376693,617.062009628139,-35.3866306287752)) ;
#59589 = CARTESIAN_POINT('Ctrl Pts',(180.152615030787,617.058013140031,-35.3765526801095)) ;
#59590 = CARTESIAN_POINT('Ctrl Pts',(180.098634181558,617.054534815907,-35.3677813861586)) ;
#59591 = CARTESIAN_POINT('Ctrl Pts',(180.044286870739,617.051006059877,-35.3617104242035)) ;
#59592 = CARTESIAN_POINT('Ctrl Pts',(179.989874428038,617.047376279796,-35.3583759379269)) ;
#59593 = CARTESIAN_POINT('Ctrl Pts',(179.981802538768,617.046837815036,-35.3578812789361)) ;
#59594 = CARTESIAN_POINT('Ctrl Pts',(179.973729146896,617.046297127075,-35.3574467776772)) ;
#59595 = CARTESIAN_POINT('Ctrl Pts',(179.965655161798,617.04575405075,-35.3570724882378)) ;
#59596 = CARTESIAN_POINT('Ctrl Pts',(179.965621251352,617.045751769849,-35.3570709162356)) ;
#59597 = CARTESIAN_POINT('Ctrl Pts',(179.965587340896,617.045749488906,-35.3570693452956)) ;
#59598 = CARTESIAN_POINT('Ctrl Pts',(179.965553430429,617.04574720792,-35.3570677754175)) ;
#59599 = CARTESIAN_POINT('Ctrl Pts',(179.910075199561,617.042015468516,-35.3544994222692)) ;
#59600 = CARTESIAN_POINT('Ctrl Pts',(179.854372203603,617.038161292594,-35.3547729571841)) ;
#59601 = CARTESIAN_POINT('Ctrl Pts',(179.79875385633,617.034248155015,-35.3578755092052)) ;
#59602 = CARTESIAN_POINT('Ctrl Pts',(179.793694805022,617.033892215568,-35.3581577176963)) ;
#59603 = CARTESIAN_POINT('Ctrl Pts',(179.788636482925,617.033535788287,-35.3584633118414)) ;
#59604 = CARTESIAN_POINT('Ctrl Pts',(179.783579139854,617.033178920942,-35.3587922690107)) ;
#59605 = CARTESIAN_POINT('Ctrl Pts',(179.722178408227,617.028846227719,-35.362786107392)) ;
#59606 = CARTESIAN_POINT('Ctrl Pts',(179.660916913678,617.024449330578,-35.3702268616423)) ;
#59607 = CARTESIAN_POINT('Ctrl Pts',(179.600196733796,617.020059248428,-35.3810502102344)) ;
#59608 = CARTESIAN_POINT('Ctrl Pts',(179.540372919564,617.015733973708,-35.3917137819958)) ;
#59609 = CARTESIAN_POINT('Ctrl Pts',(179.481074384113,617.011415593643,-35.4056604068221)) ;
#59610 = CARTESIAN_POINT('Ctrl Pts',(179.422671023473,617.007151276808,-35.4227924252981)) ;
#59611 = CARTESIAN_POINT('Ctrl Pts',(179.364301587598,617.002889436988,-35.4399144922975)) ;
#59612 = CARTESIAN_POINT('Ctrl Pts',(179.306826223232,616.998681728917,-35.460218144617)) ;
#59613 = CARTESIAN_POINT('Ctrl Pts',(179.250601206137,616.994551313171,-35.4835731411944)) ;
#59614 = CARTESIAN_POINT('Ctrl Pts',(179.194387866254,616.990421755259,-35.5069232872396)) ;
#59615 = CARTESIAN_POINT('Ctrl Pts',(179.139424385703,616.986369457334,-35.5333235335825)) ;
#59616 = CARTESIAN_POINT('Ctrl Pts',(179.086054084856,616.982392692462,-35.5626115586872)) ;
#59617 = CARTESIAN_POINT('Ctrl Pts',(179.03122286064,616.978307070254,-35.5927012948489)) ;
#59618 = CARTESIAN_POINT('Ctrl Pts',(178.978073437803,616.974301158905,-35.6258393683047)) ;
#59619 = CARTESIAN_POINT('Ctrl Pts',(178.92696280325,616.970346727896,-35.6618131631219)) ;
#59620 = CARTESIAN_POINT('Ctrl Pts',(178.877145801042,616.966492385252,-35.6968764455774)) ;
#59621 = CARTESIAN_POINT('Ctrl Pts',(178.829265868988,616.962686579411,-35.7346337876853)) ;
#59622 = CARTESIAN_POINT('Ctrl Pts',(178.783636576234,616.958881672114,-35.7748517693634)) ;
#59623 = CARTESIAN_POINT('Ctrl Pts',(178.736229952656,616.954928557852,-35.8166363030122)) ;
#59624 = CARTESIAN_POINT('Ctrl Pts',(178.691253370136,616.950975984402,-35.8610775107474)) ;
#59625 = CARTESIAN_POINT('Ctrl Pts',(178.64903346043,616.946952659638,-35.9078679213963)) ;
#59626 = CARTESIAN_POINT('Ctrl Pts',(178.612588289104,616.943479635624,-35.9482584514652)) ;
#59627 = CARTESIAN_POINT('Ctrl Pts',(178.578196485834,616.939953228555,-35.9904000939721)) ;
#59628 = CARTESIAN_POINT('Ctrl Pts',(178.546049053209,616.936322818761,-36.0340609455452)) ;
#59629 = CARTESIAN_POINT('Ctrl Pts',(178.540976461048,616.935749970892,-36.0409502575478)) ;
#59630 = CARTESIAN_POINT('Ctrl Pts',(178.535959647509,616.935174533547,-36.0478774219443)) ;
#59631 = CARTESIAN_POINT('Ctrl Pts',(178.530999248853,616.934596307854,-36.0548415611402)) ;
#59632 = CARTESIAN_POINT('Ctrl Pts',(178.530978547663,616.93459389475,-36.054870624524)) ;
#59633 = CARTESIAN_POINT('Ctrl Pts',(178.530957847456,616.934591481597,-36.0548996885518)) ;
#59634 = CARTESIAN_POINT('Ctrl Pts',(178.53093714823,616.934589068395,-36.0549287532235)) ;
#59635 = CARTESIAN_POINT('Ctrl Pts',(178.499041670027,616.93087056117,-36.099714564886)) ;
#59636 = CARTESIAN_POINT('Ctrl Pts',(178.469366274533,616.927026440125,-36.146202366481)) ;
#59637 = CARTESIAN_POINT('Ctrl Pts',(178.442065521419,616.923119508642,-36.1941322661498)) ;
#59638 = CARTESIAN_POINT('Ctrl Pts',(178.439400200466,616.922738082302,-36.1988115717106)) ;
#59639 = CARTESIAN_POINT('Ctrl Pts',(178.436757509736,616.9223560573,-36.203504581388)) ;
#59640 = CARTESIAN_POINT('Ctrl Pts',(178.4341375904,616.921973492075,-36.2082110269501)) ;
#59641 = CARTESIAN_POINT('Ctrl Pts',(178.404212362585,616.917603757737,-36.2619689628102)) ;
#59642 = CARTESIAN_POINT('Ctrl Pts',(178.377258123467,616.913164238395,-36.317485980025)) ;
#59643 = CARTESIAN_POINT('Ctrl Pts',(178.353440625791,616.908728220843,-36.3743877416019)) ;
#59644 = CARTESIAN_POINT('Ctrl Pts',(178.330063871458,616.904374291898,-36.4302365347711)) ;
#59645 = CARTESIAN_POINT('Ctrl Pts',(178.309708369483,616.900024020985,-36.4874192037108)) ;
#59646 = CARTESIAN_POINT('Ctrl Pts',(178.292492160655,616.895726470822,-36.5455744061963)) ;
#59647 = CARTESIAN_POINT('Ctrl Pts',(178.275286911396,616.891431656411,-36.603692587987)) ;
#59648 = CARTESIAN_POINT('Ctrl Pts',(178.261216825728,616.887189638468,-36.662782052018)) ;
#59649 = CARTESIAN_POINT('Ctrl Pts',(178.250364993454,616.883025817115,-36.7224753350455)) ;
#59650 = CARTESIAN_POINT('Ctrl Pts',(178.23951594627,616.878863064394,-36.7821532979702)) ;
#59651 = CARTESIAN_POINT('Ctrl Pts',(178.231883527854,616.874778478766,-36.8424347474778)) ;
#59652 = CARTESIAN_POINT('Ctrl Pts',(178.2275167976,616.870772761268,-36.9029459335317)) ;
#59653 = CARTESIAN_POINT('Ctrl Pts',(178.223000286466,616.866629645796,-36.9655326814236)) ;
#59654 = CARTESIAN_POINT('Ctrl Pts',(178.221977733339,616.862570931832,-37.0283651792618)) ;
#59655 = CARTESIAN_POINT('Ctrl Pts',(178.224463587513,616.858570423963,-37.0910230850861)) ;
#59656 = CARTESIAN_POINT('Ctrl Pts',(178.226870116644,616.854697574613,-37.1516815409108)) ;
#59657 = CARTESIAN_POINT('Ctrl Pts',(178.23256480618,616.850878896739,-37.212176243007)) ;
#59658 = CARTESIAN_POINT('Ctrl Pts',(178.241521117425,616.847068824741,-37.2721207145744)) ;
#59659 = CARTESIAN_POINT('Ctrl Pts',(178.25092026132,616.843070368906,-37.3350290591588)) ;
#59660 = CARTESIAN_POINT('Ctrl Pts',(178.263912478694,616.839081015093,-37.3973311977644)) ;
#59661 = CARTESIAN_POINT('Ctrl Pts',(178.280414158202,616.835028919848,-37.4585771180169)) ;
#59662 = CARTESIAN_POINT('Ctrl Pts',(178.294643595531,616.83153478852,-37.5113896201309)) ;
#59663 = CARTESIAN_POINT('Ctrl Pts',(178.311482658404,616.827993342589,-37.5634177529276)) ;
#59664 = CARTESIAN_POINT('Ctrl Pts',(178.330837982447,616.824352802783,-37.6143707302497)) ;
#59665 = CARTESIAN_POINT('Ctrl Pts',(178.333922252396,616.823772682941,-37.6224900847196)) ;
#59666 = CARTESIAN_POINT('Ctrl Pts',(178.337070385027,616.823190046867,-37.6305822413713)) ;
#59667 = CARTESIAN_POINT('Ctrl Pts',(178.340281970335,616.822604685048,-37.6386461419468)) ;
#59668 = CARTESIAN_POINT('Ctrl Pts',(178.340288743505,616.822603450531,-37.6386631485557)) ;
#59669 = CARTESIAN_POINT('Ctrl Pts',(178.340295516958,616.822602216003,-37.6386801550389)) ;
#59670 = CARTESIAN_POINT('Ctrl Pts',(178.340302290693,616.822600981462,-37.6386971613965)) ;
#59671 = CARTESIAN_POINT('Ctrl Pts',(178.361103043185,616.818809959359,-37.6909202003039)) ;
#59672 = CARTESIAN_POINT('Ctrl Pts',(178.384645358417,616.81489472151,-37.7421380766257)) ;
#59673 = CARTESIAN_POINT('Ctrl Pts',(178.410786328454,616.810917637055,-37.7920713750955)) ;
#59674 = CARTESIAN_POINT('Ctrl Pts',(178.413407689976,616.810518823387,-37.7970785812978)) ;
#59675 = CARTESIAN_POINT('Ctrl Pts',(178.416055144893,616.81011938781,-37.8020728492216)) ;
#59676 = CARTESIAN_POINT('Ctrl Pts',(178.418728523548,616.809719393216,-37.8070538837687)) ;
#59677 = CARTESIAN_POINT('Ctrl Pts',(178.447999575829,616.805339818079,-37.8615916584148)) ;
#59678 = CARTESIAN_POINT('Ctrl Pts',(178.480383390813,616.800893861143,-37.9145463535274)) ;
#59679 = CARTESIAN_POINT('Ctrl Pts',(178.515655526665,616.796450665732,-37.965580102408)) ;
#59680 = CARTESIAN_POINT('Ctrl Pts',(178.550884077367,616.792012960698,-38.0165507897931)) ;
#59681 = CARTESIAN_POINT('Ctrl Pts',(178.588993588597,616.787578349975,-38.0656055793173)) ;
#59682 = CARTESIAN_POINT('Ctrl Pts',(178.62973396628,616.783195130616,-38.1124361119914)) ;
#59683 = CARTESIAN_POINT('Ctrl Pts',(178.670436832959,616.778815947031,-38.1592235262559)) ;
#59684 = CARTESIAN_POINT('Ctrl Pts',(178.713765681151,616.774488196203,-38.203790917384)) ;
#59685 = CARTESIAN_POINT('Ctrl Pts',(178.759446552293,616.770235991496,-38.2458556574152)) ;
#59686 = CARTESIAN_POINT('Ctrl Pts',(178.80509973814,616.765986363875,-38.287894903739)) ;
#59687 = CARTESIAN_POINT('Ctrl Pts',(178.853102149004,616.761812183564,-38.3274345100296)) ;
#59688 = CARTESIAN_POINT('Ctrl Pts',(178.903155657434,616.757712558082,-38.3642163568452)) ;
#59689 = CARTESIAN_POINT('Ctrl Pts',(178.953214146788,616.753612524639,-38.4010018638952)) ;
#59690 = CARTESIAN_POINT('Ctrl Pts',(179.005324252406,616.749586926448,-38.4350288880954)) ;
#59691 = CARTESIAN_POINT('Ctrl Pts',(179.059161832729,616.745610946358,-38.4660647118646)) ;
#59692 = CARTESIAN_POINT('Ctrl Pts',(179.112997641711,616.741635097085,-38.4970995145057)) ;
#59693 = CARTESIAN_POINT('Ctrl Pts',(179.168560950204,616.737708570083,-38.5251429685137)) ;
#59694 = CARTESIAN_POINT('Ctrl Pts',(179.225499824143,616.733785788633,-38.5499917127387)) ;
#59695 = CARTESIAN_POINT('Ctrl Pts',(179.282495967825,616.729859061606,-38.5748654501032)) ;
#59696 = CARTESIAN_POINT('Ctrl Pts',(179.340870547703,616.725935583558,-38.5965374738112)) ;
#59697 = CARTESIAN_POINT('Ctrl Pts',(179.40024076439,616.721954749816,-38.6148400532057)) ;
#59698 = CARTESIAN_POINT('Ctrl Pts',(179.455832998681,616.718227233657,-38.6319779607059)) ;
#59699 = CARTESIAN_POINT('Ctrl Pts',(179.512297835651,616.714448772708,-38.6461613739341)) ;
#59700 = CARTESIAN_POINT('Ctrl Pts',(179.569297170793,616.710565160536,-38.6572894990112)) ;
#59701 = CARTESIAN_POINT('Origin',(179.888527625422,616.710565160536,-37.0221601717597)) ;
#59702 = CARTESIAN_POINT('Ctrl Pts',(180.464060729575,617.544113575794,-38.585591540904)) ;
#59703 = CARTESIAN_POINT('Ctrl Pts',(180.487228259808,617.54247185516,-38.5770630689456)) ;
#59704 = CARTESIAN_POINT('Ctrl Pts',(180.510205228593,617.54081290889,-38.5680200076004)) ;
#59705 = CARTESIAN_POINT('Ctrl Pts',(180.598264253176,617.534329295097,-38.5310812183154)) ;
#59706 = CARTESIAN_POINT('Ctrl Pts',(180.661732357622,617.529382284152,-38.4995635541931)) ;
#59707 = CARTESIAN_POINT('Ctrl Pts',(180.814529967429,617.516779470276,-38.4111381976683)) ;
#59708 = CARTESIAN_POINT('Ctrl Pts',(180.900808349455,617.509009249844,-38.3495731762099)) ;
#59709 = CARTESIAN_POINT('Ctrl Pts',(181.02252012136,617.49736285427,-38.2439169440387)) ;
#59710 = CARTESIAN_POINT('Ctrl Pts',(181.062544230677,617.4934042498,-38.2055091790602)) ;
#59711 = CARTESIAN_POINT('Ctrl Pts',(181.121210631552,617.487486759853,-38.1432991555566)) ;
#59712 = CARTESIAN_POINT('Ctrl Pts',(181.141244782052,617.485444870038,-38.1208686359069)) ;
#59713 = CARTESIAN_POINT('Ctrl Pts',(181.188402366363,617.480597787042,-38.0651016607649)) ;
#59714 = CARTESIAN_POINT('Ctrl Pts',(181.214863737876,617.477834830551,-38.0312362765351)) ;
#59715 = CARTESIAN_POINT('Ctrl Pts',(181.27640650444,617.471193517949,-37.9458628722803)) ;
#59716 = CARTESIAN_POINT('Ctrl Pts',(181.309965329618,617.46737642322,-37.893337728381)) ;
#59717 = CARTESIAN_POINT('Ctrl Pts',(181.398989250749,617.456283390246,-37.7351031546239)) ;
#59718 = CARTESIAN_POINT('Ctrl Pts',(181.44613467645,617.449045828247,-37.6251848230472)) ;
#59719 = CARTESIAN_POINT('Ctrl Pts',(181.496308291822,617.438080488535,-37.4617822287019)) ;
#59720 = CARTESIAN_POINT('Ctrl Pts',(181.50916818018,617.434699240502,-37.4117104832382)) ;
#59721 = CARTESIAN_POINT('Ctrl Pts',(181.531369068561,617.42739201278,-37.3048767218375)) ;
#59722 = CARTESIAN_POINT('Ctrl Pts',(181.540139374621,617.423452018443,-37.2480669562751)) ;
#59723 = CARTESIAN_POINT('Ctrl Pts',(181.552805283756,617.414690183658,-37.1236745399862)) ;
#59724 = CARTESIAN_POINT('Ctrl Pts',(181.555552878684,617.409842640143,-37.0560780101603)) ;
#59725 = CARTESIAN_POINT('Ctrl Pts',(181.55183161418,617.396485359588,-36.8718907693089)) ;
#59726 = CARTESIAN_POINT('Ctrl Pts',(181.537235299013,617.387889720624,-36.7558388670058)) ;
#59727 = CARTESIAN_POINT('Ctrl Pts',(181.503417768927,617.377549023494,-36.6114444148363)) ;
#59728 = CARTESIAN_POINT('Ctrl Pts',(181.495323354846,617.375380372175,-36.5808374754927)) ;
#59729 = CARTESIAN_POINT('Ctrl Pts',(181.475778917983,617.370764665774,-36.5146307816251)) ;
#59730 = CARTESIAN_POINT('Ctrl Pts',(181.463993473597,617.368335480354,-36.4791494249022)) ;
#59731 = CARTESIAN_POINT('Ctrl Pts',(181.413956652883,617.359140256472,-36.3439020594885)) ;
#59732 = CARTESIAN_POINT('Ctrl Pts',(181.367336133876,617.35271142634,-36.2475003903021)) ;
#59733 = CARTESIAN_POINT('Ctrl Pts',(181.264639212964,617.340621636482,-36.0787061870358)) ;
#59734 = CARTESIAN_POINT('Ctrl Pts',(181.211231081331,617.335011868706,-36.0051836672477)) ;
#59735 = CARTESIAN_POINT('Ctrl Pts',(181.119272786496,617.325924136133,-35.8981670026294)) ;
#59736 = CARTESIAN_POINT('Ctrl Pts',(181.084724634698,617.322614635726,-35.8614680953434)) ;
#59737 = CARTESIAN_POINT('Ctrl Pts',(181.005758281013,617.315223312717,-35.7848609089031)) ;
#59738 = CARTESIAN_POINT('Ctrl Pts',(180.960752412362,617.31111621247,-35.7456625238566)) ;
#59739 = CARTESIAN_POINT('Ctrl Pts',(180.85632288467,617.301794342589,-35.6641337814623)) ;
#59740 = CARTESIAN_POINT('Ctrl Pts',(180.796025743465,617.296544107431,-35.6231217188557)) ;
#59741 = CARTESIAN_POINT('Ctrl Pts',(180.640921235174,617.283464816743,-35.5318806821652)) ;
#59742 = CARTESIAN_POINT('Ctrl Pts',(180.543569190138,617.27560524913,-35.4865973621708)) ;
#59743 = CARTESIAN_POINT('Ctrl Pts',(180.413194050154,617.265986146595,-35.4406263574173)) ;
#59744 = CARTESIAN_POINT('Ctrl Pts',(180.383562890426,617.263859232689,-35.431102416498)) ;
#59745 = CARTESIAN_POINT('Ctrl Pts',(180.316529223903,617.259200903316,-35.4116114343015)) ;
#59746 = CARTESIAN_POINT('Ctrl Pts',(180.279012906293,617.25669325476,-35.4021063274235)) ;
#59747 = CARTESIAN_POINT('Ctrl Pts',(180.190361868786,617.250925295162,-35.3829050293004)) ;
#59748 = CARTESIAN_POINT('Ctrl Pts',(180.13903628989,617.247705932207,-35.3742804706709)) ;
#59749 = CARTESIAN_POINT('Ctrl Pts',(179.95021003229,617.236034891206,-35.3515791153275)) ;
#59750 = CARTESIAN_POINT('Ctrl Pts',(179.811526663085,617.227744455219,-35.3522158946241)) ;
#59751 = CARTESIAN_POINT('Ctrl Pts',(179.623314558065,617.215567638189,-35.376595360912)) ;
#59752 = CARTESIAN_POINT('Ctrl Pts',(179.572454955257,617.212188742156,-35.3856032325347)) ;
#59753 = CARTESIAN_POINT('Ctrl Pts',(179.465904619507,617.204873098296,-35.4096266942594)) ;
#59754 = CARTESIAN_POINT('Ctrl Pts',(179.410411295285,617.200921696622,-35.4252012566082)) ;
#59755 = CARTESIAN_POINT('Ctrl Pts',(179.291449808206,617.192121917137,-35.4653453175336)) ;
#59756 = CARTESIAN_POINT('Ctrl Pts',(179.228454648776,617.187247210815,-35.4909918645347)) ;
#59757 = CARTESIAN_POINT('Ctrl Pts',(179.06323587317,617.173956964152,-35.5703497614573)) ;
#59758 = CARTESIAN_POINT('Ctrl Pts',(178.964727400564,617.165461933159,-35.6309534828837)) ;
#59759 = CARTESIAN_POINT('Ctrl Pts',(178.848055629101,617.155198408885,-35.7206283528762)) ;
#59760 = CARTESIAN_POINT('Ctrl Pts',(178.823401220682,617.153018832484,-35.7407260444342)) ;
#59761 = CARTESIAN_POINT('Ctrl Pts',(178.771131236274,617.148398800956,-35.7858873849874)) ;
#59762 = CARTESIAN_POINT('Ctrl Pts',(178.743751859662,617.145975444034,-35.8111960524104)) ;
#59763 = CARTESIAN_POINT('Ctrl Pts',(178.641725376111,617.136823836361,-35.912062543586)) ;
#59764 = CARTESIAN_POINT('Ctrl Pts',(178.573512241876,617.130429170258,-35.9937771284451)) ;
#59765 = CARTESIAN_POINT('Ctrl Pts',(178.462018006044,617.118346099454,-36.1567404778624)) ;
#59766 = CARTESIAN_POINT('Ctrl Pts',(178.416776960854,617.112705913602,-36.236139802998)) ;
#59767 = CARTESIAN_POINT('Ctrl Pts',(178.357004338013,617.103586191004,-36.3644910274877)) ;
#59768 = CARTESIAN_POINT('Ctrl Pts',(178.337826770242,617.100277869931,-36.411080612624)) ;
#59769 = CARTESIAN_POINT('Ctrl Pts',(178.300632149563,617.092892382787,-36.5145252269169)) ;
#59770 = CARTESIAN_POINT('Ctrl Pts',(178.28349857953,617.088790104647,-36.5716210725207)) ;
#59771 = CARTESIAN_POINT('Ctrl Pts',(178.252336116539,617.079486436461,-36.7001160867461)) ;
#59772 = CARTESIAN_POINT('Ctrl Pts',(178.239850899794,617.074249916677,-36.7717641053334)) ;
#59773 = CARTESIAN_POINT('Ctrl Pts',(178.220532786075,617.061117841501,-36.9513657376716)) ;
#59774 = CARTESIAN_POINT('Ctrl Pts',(178.219450268508,617.053188866332,-37.0596161349644)) ;
#59775 = CARTESIAN_POINT('Ctrl Pts',(178.231557357831,617.043513198459,-37.1981407962776)) ;
#59776 = CARTESIAN_POINT('Ctrl Pts',(178.235124343208,617.041391167387,-37.2289882729264)) ;
#59777 = CARTESIAN_POINT('Ctrl Pts',(178.245062069491,617.036740668009,-37.2979679740585)) ;
#59778 = CARTESIAN_POINT('Ctrl Pts',(178.251901199839,617.034236020005,-37.3360128886887)) ;
#59779 = CARTESIAN_POINT('Ctrl Pts',(178.271021189482,617.028475398674,-37.4245616654215)) ;
#59780 = CARTESIAN_POINT('Ctrl Pts',(178.2843535863,617.025260287678,-37.4747973884619)) ;
#59781 = CARTESIAN_POINT('Ctrl Pts',(178.341537898242,617.013617805404,-37.6556882475495)) ;
#59782 = CARTESIAN_POINT('Ctrl Pts',(178.399190595616,617.005351022861,-37.7813752338753)) ;
#59783 = CARTESIAN_POINT('Ctrl Pts',(178.498673764095,616.993216947292,-37.9422148638106)) ;
#59784 = CARTESIAN_POINT('Ctrl Pts',(178.52769655212,616.98985543118,-37.9846217154074)) ;
#59785 = CARTESIAN_POINT('Ctrl Pts',(178.592964375516,616.982597822027,-38.0711222828626)) ;
#59786 = CARTESIAN_POINT('Ctrl Pts',(178.629608481935,616.978688092588,-38.1148297682013)) ;
#59787 = CARTESIAN_POINT('Ctrl Pts',(178.713874978571,616.970014753276,-38.205462398813)) ;
#59788 = CARTESIAN_POINT('Ctrl Pts',(178.762226758882,616.965226466012,-38.2515737338429)) ;
#59789 = CARTESIAN_POINT('Ctrl Pts',(178.905026198199,616.951662503466,-38.3722458681657)) ;
#59790 = CARTESIAN_POINT('Ctrl Pts',(179.004974215103,616.94278270056,-38.4396730858431)) ;
#59791 = CARTESIAN_POINT('Ctrl Pts',(179.139025842964,616.932217469467,-38.5103754587916)) ;
#59792 = CARTESIAN_POINT('Ctrl Pts',(179.16714957219,616.930071729297,-38.5242094426074)) ;
#59793 = CARTESIAN_POINT('Ctrl Pts',(179.230670040116,616.925402451974,-38.5532585032686)) ;
#59794 = CARTESIAN_POINT('Ctrl Pts',(179.266236107803,616.922901044047,-38.5680555656971)) ;
#59795 = CARTESIAN_POINT('Ctrl Pts',(179.350445356438,616.91716668458,-38.5997122333386)) ;
#59796 = CARTESIAN_POINT('Ctrl Pts',(179.399420487653,616.913973055928,-38.615577250843)) ;
#59797 = CARTESIAN_POINT('Ctrl Pts',(179.58278955523,616.902274090356,-38.6657242579006)) ;
#59798 = CARTESIAN_POINT('Ctrl Pts',(179.720553916021,616.893934831471,-38.6854583440229)) ;
#59799 = CARTESIAN_POINT('Ctrl Pts',(179.910889613995,616.881693872816,-38.6888130582876)) ;
#59800 = CARTESIAN_POINT('Ctrl Pts',(179.962619718989,616.878301359716,-38.687315207343)) ;
#59801 = CARTESIAN_POINT('Ctrl Pts',(180.072718072115,616.870891710868,-38.6789868878036)) ;
#59802 = CARTESIAN_POINT('Ctrl Pts',(180.130961974825,616.866856791597,-38.6714706279383)) ;
#59803 = CARTESIAN_POINT('Ctrl Pts',(180.282456566663,616.85603692188,-38.6437225766261)) ;
#59804 = CARTESIAN_POINT('Ctrl Pts',(180.374572525789,616.849118914138,-38.6185312683209)) ;
#59805 = CARTESIAN_POINT('Ctrl Pts',(180.464017215185,616.842172979815,-38.58560755881)) ;
#59806 = CARTESIAN_POINT('Origin',(179.888527625422,617.710565160536,-37.0221601717597)) ;
#59807 = CARTESIAN_POINT('',(180.464060715702,618.242141445689,-38.5855915460107)) ;
#59808 = CARTESIAN_POINT('',(180.464060715494,618.051541226924,-38.5855915460876)) ;
#59809 = CARTESIAN_POINT('',(180.464060715702,617.710565160536,-38.5855915460107)) ;
#59810 = CARTESIAN_POINT('',(179.889570327489,618.281200386648,-38.688647256677)) ;
#59811 = CARTESIAN_POINT('Ctrl Pts',(179.889549821694,618.280920770248,-38.6881598581687)) ;
#59812 = CARTESIAN_POINT('Ctrl Pts',(179.935372015437,618.277609385829,-38.6881317433521)) ;
#59813 = CARTESIAN_POINT('Ctrl Pts',(179.981177137719,618.274325601274,-38.6862131676218)) ;
#59814 = CARTESIAN_POINT('Ctrl Pts',(180.057497874022,618.268952524589,-38.6798546522522)) ;
#59815 = CARTESIAN_POINT('Ctrl Pts',(180.088073891955,618.266826693261,-38.6764526338771)) ;
#59816 = CARTESIAN_POINT('Ctrl Pts',(180.150064623838,618.262594201886,-38.6678112488637)) ;
#59817 = CARTESIAN_POINT('Ctrl Pts',(180.181456640678,618.260495094555,-38.6625143410322)) ;
#59818 = CARTESIAN_POINT('Ctrl Pts',(180.298227785343,618.252793862451,-38.6393516539469)) ;
#59819 = CARTESIAN_POINT('Ctrl Pts',(180.382278599981,618.247457897413,-38.6156973214008)) ;
#59820 = CARTESIAN_POINT('Ctrl Pts',(180.464060715702,618.242141445689,-38.5855915460107)) ;
#59821 = CARTESIAN_POINT('',(180.967886278469,618.710565160535,-35.7530892919062)) ;
#59822 = CARTESIAN_POINT('Ctrl Pts',(179.889570327489,618.281200386648,-38.688647256677)) ;
#59823 = CARTESIAN_POINT('Ctrl Pts',(179.829704746323,618.285448698176,-38.6885516393912)) ;
#59824 = CARTESIAN_POINT('Ctrl Pts',(179.769739180832,618.289736185626,-38.6852034082082)) ;
#59825 = CARTESIAN_POINT('Ctrl Pts',(179.710050946309,618.294002899686,-38.6786274687905)) ;
#59826 = CARTESIAN_POINT('Ctrl Pts',(179.650427244363,618.298265000742,-38.6720586390204)) ;
#59827 = CARTESIAN_POINT('Ctrl Pts',(179.591080237905,618.302506114863,-38.6622693141872)) ;
#59828 = CARTESIAN_POINT('Ctrl Pts',(179.532377447291,618.306686786384,-38.6493212577048)) ;
#59829 = CARTESIAN_POINT('Ctrl Pts',(179.47371511148,618.310864576811,-38.6363821243258)) ;
#59830 = CARTESIAN_POINT('Ctrl Pts',(179.415696123102,618.314981909742,-38.6202886814295)) ;
#59831 = CARTESIAN_POINT('Ctrl Pts',(179.358678843421,618.319022312191,-38.6011372402441)) ;
#59832 = CARTESIAN_POINT('Ctrl Pts',(179.301678310872,618.323061527892,-38.5819914242253)) ;
#59833 = CARTESIAN_POINT('Ctrl Pts',(179.24567899163,618.327023880714,-38.5597893633856)) ;
#59834 = CARTESIAN_POINT('Ctrl Pts',(179.191029694323,618.330916357404,-38.5346617854854)) ;
#59835 = CARTESIAN_POINT('Ctrl Pts',(179.136336185405,618.334811983132,-38.5095138792235)) ;
#59836 = CARTESIAN_POINT('Ctrl Pts',(179.082995057282,618.338637757528,-38.481435580952)) ;
#59837 = CARTESIAN_POINT('Ctrl Pts',(179.031344721663,618.342422989758,-38.450593880277)) ;
#59838 = CARTESIAN_POINT('Ctrl Pts',(178.979675054896,618.346209638685,-38.419740636492)) ;
#59839 = CARTESIAN_POINT('Ctrl Pts',(178.929697728594,618.349956005156,-38.3861216980553)) ;
#59840 = CARTESIAN_POINT('Ctrl Pts',(178.881736917209,618.353710573408,-38.3499429252659)) ;
#59841 = CARTESIAN_POINT('Ctrl Pts',(178.833687107688,618.357472108798,-38.3136970175966)) ;
#59842 = CARTESIAN_POINT('Ctrl Pts',(178.787661776309,618.361242367052,-38.2748814771352)) ;
#59843 = CARTESIAN_POINT('Ctrl Pts',(178.743966658101,618.365083510243,-38.2337460600409)) ;
#59844 = CARTESIAN_POINT('Ctrl Pts',(178.705730437837,618.368444773542,-38.1977497535161)) ;
#59845 = CARTESIAN_POINT('Ctrl Pts',(178.669278595077,618.371860843973,-38.1599775677742)) ;
#59846 = CARTESIAN_POINT('Ctrl Pts',(178.634797890773,618.375376290139,-38.1206260862659)) ;
#59847 = CARTESIAN_POINT('Ctrl Pts',(178.634775519202,618.375378571011,-38.1206005544658)) ;
#59848 = CARTESIAN_POINT('Ctrl Pts',(178.63475314846,618.375380851924,-38.1205750220006)) ;
#59849 = CARTESIAN_POINT('Ctrl Pts',(178.634730778545,618.375383132879,-38.1205494888704)) ;
#59850 = CARTESIAN_POINT('Ctrl Pts',(178.598132648023,618.379114872309,-38.078776203119)) ;
#59851 = CARTESIAN_POINT('Ctrl Pts',(178.563616256322,618.38296904822,-38.0350553006912)) ;
#59852 = CARTESIAN_POINT('Ctrl Pts',(178.531364456865,618.386882185751,-37.9896367159316)) ;
#59853 = CARTESIAN_POINT('Ctrl Pts',(178.52843083029,618.387238125093,-37.9855054373826)) ;
#59854 = CARTESIAN_POINT('Ctrl Pts',(178.525515942001,618.387594552267,-37.981360148246)) ;
#59855 = CARTESIAN_POINT('Ctrl Pts',(178.522619930061,618.387951419504,-37.9772010579421)) ;
#59856 = CARTESIAN_POINT('Ctrl Pts',(178.487459707981,618.392284112733,-37.9267059143508)) ;
#59857 = CARTESIAN_POINT('Ctrl Pts',(178.455081206244,618.396681009839,-37.8741705136963)) ;
#59858 = CARTESIAN_POINT('Ctrl Pts',(178.425684827552,618.401071091914,-37.8199493167374)) ;
#59859 = CARTESIAN_POINT('Ctrl Pts',(178.396722406297,618.405396366388,-37.7665285480182)) ;
#59860 = CARTESIAN_POINT('Ctrl Pts',(178.370654285138,618.409714746169,-37.7114715087366)) ;
#59861 = CARTESIAN_POINT('Ctrl Pts',(178.347634737273,618.413979062684,-37.6551282848904)) ;
#59862 = CARTESIAN_POINT('Ctrl Pts',(178.324628560771,618.418240902185,-37.5988177891295)) ;
#59863 = CARTESIAN_POINT('Ctrl Pts',(178.304667292194,618.422448609902,-37.5412226206631)) ;
#59864 = CARTESIAN_POINT('Ctrl Pts',(178.287871239278,618.426579025262,-37.4827025310582)) ;
#59865 = CARTESIAN_POINT('Ctrl Pts',(178.271078674683,618.430708582788,-37.4241945953139)) ;
#59866 = CARTESIAN_POINT('Ctrl Pts',(178.257450048961,618.434760880296,-37.3647621325426)) ;
#59867 = CARTESIAN_POINT('Ctrl Pts',(178.247072510769,618.438737644718,-37.3047747672279)) ;
#59868 = CARTESIAN_POINT('Ctrl Pts',(178.236410903974,618.442823266741,-37.2431453431988)) ;
#59869 = CARTESIAN_POINT('Ctrl Pts',(178.229181169598,618.446829177861,-37.1809301971565)) ;
#59870 = CARTESIAN_POINT('Ctrl Pts',(178.22543965551,618.450783608598,-37.1185409966365)) ;
#59871 = CARTESIAN_POINT('Ctrl Pts',(178.221792841014,618.454637950716,-37.0577308979622)) ;
#59872 = CARTESIAN_POINT('Ctrl Pts',(178.221460070539,618.458443755999,-36.9967555430253)) ;
#59873 = CARTESIAN_POINT('Ctrl Pts',(178.224454356076,618.462248662701,-36.9360056250828)) ;
#59874 = CARTESIAN_POINT('Ctrl Pts',(178.227565273931,618.46620177674,-36.8728893985096)) ;
#59875 = CARTESIAN_POINT('Ctrl Pts',(178.234268369628,618.470154349927,-36.8100166453997)) ;
#59876 = CARTESIAN_POINT('Ctrl Pts',(178.244526904074,618.474177674403,-36.7478344419943)) ;
#59877 = CARTESIAN_POINT('Ctrl Pts',(178.253382299866,618.477650697846,-36.6941573767934)) ;
#59878 = CARTESIAN_POINT('Ctrl Pts',(178.264887024461,618.481177104316,-36.6409938986677)) ;
#59879 = CARTESIAN_POINT('Ctrl Pts',(178.278978856662,618.484807513478,-36.588637928831)) ;
#59880 = CARTESIAN_POINT('Ctrl Pts',(178.281202429831,618.485380361657,-36.5803765950255)) ;
#59881 = CARTESIAN_POINT('Ctrl Pts',(178.283490374685,618.485955799315,-36.5721352701504)) ;
#59882 = CARTESIAN_POINT('Ctrl Pts',(178.285842401795,618.486534025323,-36.5639149988284)) ;
#59883 = CARTESIAN_POINT('Ctrl Pts',(178.285852217406,618.486536438409,-36.5638806935319)) ;
#59884 = CARTESIAN_POINT('Ctrl Pts',(178.285862034133,618.486538851542,-36.563846388602)) ;
#59885 = CARTESIAN_POINT('Ctrl Pts',(178.285871851977,618.486541264725,-36.5638120840387)) ;
#59886 = CARTESIAN_POINT('Ctrl Pts',(178.301000305292,618.49025977141,-36.5109516979469)) ;
#59887 = CARTESIAN_POINT('Ctrl Pts',(178.318843626882,618.494103891889,-36.4587658691368)) ;
#59888 = CARTESIAN_POINT('Ctrl Pts',(178.339294991459,618.498010822778,-36.4075374771681)) ;
#59889 = CARTESIAN_POINT('Ctrl Pts',(178.341291618342,618.49839224883,-36.4025361490564)) ;
#59890 = CARTESIAN_POINT('Ctrl Pts',(178.343313069218,618.498774273543,-36.3975439695781)) ;
#59891 = CARTESIAN_POINT('Ctrl Pts',(178.345359222393,618.499156838477,-36.3925612163449)) ;
#59892 = CARTESIAN_POINT('Ctrl Pts',(178.368730796001,618.503526572189,-36.3356472055365)) ;
#59893 = CARTESIAN_POINT('Ctrl Pts',(178.395330056032,618.507966090875,-36.279959238087)) ;
#59894 = CARTESIAN_POINT('Ctrl Pts',(178.424967679135,618.512402107738,-36.2258603000353)) ;
#59895 = CARTESIAN_POINT('Ctrl Pts',(178.454056855601,618.516756035746,-36.1727624672529)) ;
#59896 = CARTESIAN_POINT('Ctrl Pts',(178.486072617855,618.521106305691,-36.1211950867261)) ;
#59897 = CARTESIAN_POINT('Ctrl Pts',(178.520806054384,618.525403854869,-36.0714757396111)) ;
#59898 = CARTESIAN_POINT('Ctrl Pts',(178.555517380224,618.529698668303,-36.0217880429491)) ;
#59899 = CARTESIAN_POINT('Ctrl Pts',(178.592942827306,618.533940685251,-35.9739459312664)) ;
#59900 = CARTESIAN_POINT('Ctrl Pts',(178.632846906928,618.538104505605,-35.9282434763273)) ;
#59901 = CARTESIAN_POINT('Ctrl Pts',(178.672740745377,618.542267257336,-35.8825527506836)) ;
#59902 = CARTESIAN_POINT('Ctrl Pts',(178.71511194355,618.546351841969,-35.8390006188666)) ;
#59903 = CARTESIAN_POINT('Ctrl Pts',(178.759698879925,618.55035755848,-35.7978584663417)) ;
#59904 = CARTESIAN_POINT('Ctrl Pts',(178.805815173444,618.554500673334,-35.7553051147069)) ;
#59905 = CARTESIAN_POINT('Ctrl Pts',(178.854302049302,618.558559386672,-35.7153302272149)) ;
#59906 = CARTESIAN_POINT('Ctrl Pts',(178.904839879814,618.562559893931,-35.6782071797221)) ;
#59907 = CARTESIAN_POINT('Ctrl Pts',(178.95376501449,618.566432742339,-35.6422687534043)) ;
#59908 = CARTESIAN_POINT('Ctrl Pts',(179.004612255485,618.570251419296,-35.6090032130565)) ;
#59909 = CARTESIAN_POINT('Ctrl Pts',(179.057062896466,618.574061490419,-35.5786307741719)) ;
#59910 = CARTESIAN_POINT('Ctrl Pts',(179.112106895572,618.578059945874,-35.5467566070012)) ;
#59911 = CARTESIAN_POINT('Ctrl Pts',(179.168917188531,618.582049299349,-35.5180695816817)) ;
#59912 = CARTESIAN_POINT('Ctrl Pts',(179.227089810526,618.58610139435,-35.4927849063632)) ;
#59913 = CARTESIAN_POINT('Ctrl Pts',(179.277252190683,618.589595524799,-35.4709818751094)) ;
#59914 = CARTESIAN_POINT('Ctrl Pts',(179.328428400699,618.593136969904,-35.451708177045)) ;
#59915 = CARTESIAN_POINT('Ctrl Pts',(179.380332883121,618.596777508938,-35.435072119092)) ;
#59916 = CARTESIAN_POINT('Ctrl Pts',(179.388603871233,618.597357629453,-35.4324211604245)) ;
#59917 = CARTESIAN_POINT('Ctrl Pts',(179.396893413007,618.597940266208,-35.4298370893434)) ;
#59918 = CARTESIAN_POINT('Ctrl Pts',(179.405200425425,618.598525628718,-35.4273202451089)) ;
#59919 = CARTESIAN_POINT('Ctrl Pts',(179.405217944885,618.598526863246,-35.4273149370932)) ;
#59920 = CARTESIAN_POINT('Ctrl Pts',(179.405235464423,618.598528097785,-35.4273096293765)) ;
#59921 = CARTESIAN_POINT('Ctrl Pts',(179.405252984039,618.598529332337,-35.4273043219588)) ;
#59922 = CARTESIAN_POINT('Ctrl Pts',(179.459051654156,618.60232035397,-35.4110064750025)) ;
#59923 = CARTESIAN_POINT('Ctrl Pts',(179.51377379274,618.606235591445,-35.3974787764822)) ;
#59924 = CARTESIAN_POINT('Ctrl Pts',(179.569111842561,618.610212675629,-35.3867837090165)) ;
#59925 = CARTESIAN_POINT('Ctrl Pts',(179.574661034334,618.610611489879,-35.3857112284976)) ;
#59926 = CARTESIAN_POINT('Ctrl Pts',(179.580216379535,618.611010926041,-35.3846672155845)) ;
#59927 = CARTESIAN_POINT('Ctrl Pts',(179.585777541669,618.611410921222,-35.383651721626)) ;
#59928 = CARTESIAN_POINT('Ctrl Pts',(179.646667098476,618.615790496704,-35.3725330065825)) ;
#59929 = CARTESIAN_POINT('Ctrl Pts',(179.70825972965,618.620236454121,-35.3648349819728)) ;
#59930 = CARTESIAN_POINT('Ctrl Pts',(179.7701513431,618.624679650117,-35.3605928285274)) ;
#59931 = CARTESIAN_POINT('Ctrl Pts',(179.831966478092,618.629117355727,-35.3563559170419)) ;
#59932 = CARTESIAN_POINT('Ctrl Pts',(179.894079953235,618.63355196713,-35.3555659745547)) ;
#59933 = CARTESIAN_POINT('Ctrl Pts',(179.956094752594,618.637935187241,-35.3582197283047)) ;
#59934 = CARTESIAN_POINT('Ctrl Pts',(180.01805245278,618.642314371569,-35.3608710386517)) ;
#59935 = CARTESIAN_POINT('Ctrl Pts',(180.079911741523,618.646642123212,-35.3669595863454)) ;
#59936 = CARTESIAN_POINT('Ctrl Pts',(180.141280840958,618.650894328773,-35.3764473975845)) ;
#59937 = CARTESIAN_POINT('Ctrl Pts',(180.202612746982,618.655143957238,-35.3859294586323)) ;
#59938 = CARTESIAN_POINT('Ctrl Pts',(180.263455073361,618.659318138432,-35.3988067183323)) ;
#59939 = CARTESIAN_POINT('Ctrl Pts',(180.323420134712,618.663417764808,-35.4150070260749)) ;
#59940 = CARTESIAN_POINT('Ctrl Pts',(180.383391163055,618.66751779913,-35.4312089458747)) ;
#59941 = CARTESIAN_POINT('Ctrl Pts',(180.442484684221,618.67154339821,-35.4507347702405)) ;
#59942 = CARTESIAN_POINT('Ctrl Pts',(180.500316653274,618.675519379174,-35.4734761721196)) ;
#59943 = CARTESIAN_POINT('Ctrl Pts',(180.558146719432,618.679495229314,-35.4962168257189)) ;
#59944 = CARTESIAN_POINT('Ctrl Pts',(180.61471513308,618.683421757168,-35.5221731686129)) ;
#59945 = CARTESIAN_POINT('Ctrl Pts',(180.669643472711,618.687344539433,-35.5511968412561)) ;
#59946 = CARTESIAN_POINT('Ctrl Pts',(180.724627059594,618.691271267257,-35.580249706082)) ;
#59947 = CARTESIAN_POINT('Ctrl Pts',(180.777966886512,618.695194746064,-35.6123765119138)) ;
#59948 = CARTESIAN_POINT('Ctrl Pts',(180.82929314479,618.69917558051,-35.6473825524794)) ;
#59949 = CARTESIAN_POINT('Ctrl Pts',(180.877353246692,618.702903093786,-35.6801609768813)) ;
#59950 = CARTESIAN_POINT('Ctrl Pts',(180.923647493842,618.706681551705,-35.7154637220932)) ;
#59951 = CARTESIAN_POINT('Ctrl Pts',(180.967886278469,618.710565160535,-35.7530892919061)) ;
#59952 = CARTESIAN_POINT('',(180.986589642961,618.710557544484,-38.2762782920169)) ;
#59953 = CARTESIAN_POINT('Origin',(179.888527625422,618.710565160536,-37.0221601717597)) ;
#59954 = CARTESIAN_POINT('',(179.889399881814,618.088273794561,-38.6876911816457)) ;
#59955 = CARTESIAN_POINT('Ctrl Pts',(180.986589653577,618.710557544348,-38.2762783041407)) ;
#59956 = CARTESIAN_POINT('Ctrl Pts',(181.026169046573,618.706964343704,-38.2415835129224)) ;
#59957 = CARTESIAN_POINT('Ctrl Pts',(181.064134566316,618.703274822254,-38.2049117313778)) ;
#59958 = CARTESIAN_POINT('Ctrl Pts',(181.100299043188,618.699542583949,-38.1664539739033)) ;
#59959 = CARTESIAN_POINT('Ctrl Pts',(181.141726611101,618.695267185291,-38.1223993795229)) ;
#59960 = CARTESIAN_POINT('Ctrl Pts',(181.180791568861,618.690936293108,-38.076000131448)) ;
#59961 = CARTESIAN_POINT('Ctrl Pts',(181.217253524757,618.68661604972,-38.0275596099569)) ;
#59962 = CARTESIAN_POINT('Ctrl Pts',(181.253678328109,618.682300208401,-37.9791684464486)) ;
#59963 = CARTESIAN_POINT('Ctrl Pts',(181.287505713534,618.677995292116,-37.9287402994145)) ;
#59964 = CARTESIAN_POINT('Ctrl Pts',(181.318530263923,618.67374647211,-37.8765947129868)) ;
#59965 = CARTESIAN_POINT('Ctrl Pts',(181.349534972181,618.669500369488,-37.8244824769068)) ;
#59966 = CARTESIAN_POINT('Ctrl Pts',(181.377740524878,618.665310409449,-37.7706550363168)) ;
#59967 = CARTESIAN_POINT('Ctrl Pts',(181.402973312593,618.661197874076,-37.7154472169003)) ;
#59968 = CARTESIAN_POINT('Ctrl Pts',(181.428199534615,618.657086408805,-37.660253762824)) ;
#59969 = CARTESIAN_POINT('Ctrl Pts',(181.450454481109,618.653052318317,-37.6036806587458)) ;
#59970 = CARTESIAN_POINT('Ctrl Pts',(181.46959583614,618.649092285549,-37.5460780256657)) ;
#59971 = CARTESIAN_POINT('Ctrl Pts',(181.488753320266,618.645128915935,-37.488426854835)) ;
#59972 = CARTESIAN_POINT('Ctrl Pts',(181.504791768155,618.641239604739,-37.4297444203877)) ;
#59973 = CARTESIAN_POINT('Ctrl Pts',(181.517601625427,618.637397385774,-37.3703972420371)) ;
#59974 = CARTESIAN_POINT('Ctrl Pts',(181.530416297433,618.633553722667,-37.3110277573567)) ;
#59975 = CARTESIAN_POINT('Ctrl Pts',(181.539999611886,618.629756913792,-37.2509930458803)) ;
#59976 = CARTESIAN_POINT('Ctrl Pts',(181.546279004478,618.625959256704,-37.1906754568052)) ;
#59977 = CARTESIAN_POINT('Ctrl Pts',(181.552570321133,618.622154388169,-37.1302433294688)) ;
#59978 = CARTESIAN_POINT('Ctrl Pts',(181.555544624921,618.618348193862,-37.0695273473087)) ;
#59979 = CARTESIAN_POINT('Ctrl Pts',(181.555172712382,618.614477464704,-37.0089267621576)) ;
#59980 = CARTESIAN_POINT('Ctrl Pts',(181.554838547445,618.610999598739,-36.954476888776)) ;
#59981 = CARTESIAN_POINT('Ctrl Pts',(181.551802998906,618.607469043536,-36.9001197890744)) ;
#59982 = CARTESIAN_POINT('Ctrl Pts',(181.546081556269,618.603835460268,-36.8461553786571)) ;
#59983 = CARTESIAN_POINT('Ctrl Pts',(181.545573751228,618.603512962602,-36.8413657825042)) ;
#59984 = CARTESIAN_POINT('Ctrl Pts',(181.545044806735,618.603189653342,-36.8365792511381)) ;
#59985 = CARTESIAN_POINT('Ctrl Pts',(181.544494744016,618.602865497294,-36.8317959772675)) ;
#59986 = CARTESIAN_POINT('Ctrl Pts',(181.544490855517,618.602863205773,-36.8317621633852)) ;
#59987 = CARTESIAN_POINT('Ctrl Pts',(181.544486965962,618.602860914209,-36.8317283496656)) ;
#59988 = CARTESIAN_POINT('Ctrl Pts',(181.544483075352,618.602858622603,-36.8316945361088)) ;
#59989 = CARTESIAN_POINT('Ctrl Pts',(181.538135447463,618.599119809511,-36.7765268651732)) ;
#59990 = CARTESIAN_POINT('Ctrl Pts',(181.528947374573,618.595258438764,-36.7215940585193)) ;
#59991 = CARTESIAN_POINT('Ctrl Pts',(181.516981104278,618.591337573943,-36.6671986732568)) ;
#59992 = CARTESIAN_POINT('Ctrl Pts',(181.51586624176,618.590972278398,-36.66213081379)) ;
#59993 = CARTESIAN_POINT('Ctrl Pts',(181.514727290899,618.590606466438,-36.6570676453316)) ;
#59994 = CARTESIAN_POINT('Ctrl Pts',(181.513564318844,618.590240189063,-36.6520094282069)) ;
#59995 = CARTESIAN_POINT('Ctrl Pts',(181.499781160261,618.585899191248,-36.5920611186054)) ;
#59996 = CARTESIAN_POINT('Ctrl Pts',(181.482619962743,618.581493479981,-36.5328037999466)) ;
#59997 = CARTESIAN_POINT('Ctrl Pts',(181.462208479127,618.577093884059,-36.4746228510559)) ;
#59998 = CARTESIAN_POINT('Ctrl Pts',(181.44205587073,618.57275008743,-36.4171798007995)) ;
#59999 = CARTESIAN_POINT('Ctrl Pts',(181.418735267596,618.56841254422,-36.3607857591996)) ;
#60000 = CARTESIAN_POINT('Ctrl Pts',(181.392402973023,618.56412887647,-36.3057912769584)) ;
#60001 = CARTESIAN_POINT('Ctrl Pts',(181.366086649505,618.559847806849,-36.2508301499537)) ;
#60002 = CARTESIAN_POINT('Ctrl Pts',(181.336762385989,618.555620682448,-36.1972668002697)) ;
#60003 = CARTESIAN_POINT('Ctrl Pts',(181.304616451639,618.551471225851,-36.1454330180176)) ;
#60004 = CARTESIAN_POINT('Ctrl Pts',(181.272478151229,618.547322754656,-36.0936115451292)) ;
#60005 = CARTESIAN_POINT('Ctrl Pts',(181.237519502145,618.543251916378,-36.0435188495208)) ;
#60006 = CARTESIAN_POINT('Ctrl Pts',(181.199956330705,618.539257613532,-35.9954687581075)) ;
#60007 = CARTESIAN_POINT('Ctrl Pts',(181.161502667911,618.535168619743,-35.9462795671642)) ;
#60008 = CARTESIAN_POINT('Ctrl Pts',(181.120319291636,618.531159806111,-35.8992312085298)) ;
#60009 = CARTESIAN_POINT('Ctrl Pts',(181.076670980546,618.527204007082,-35.8546396928581)) ;
#60010 = CARTESIAN_POINT('Ctrl Pts',(181.033979319065,618.523334908169,-35.8110254992176)) ;
#60011 = CARTESIAN_POINT('Ctrl Pts',(180.988929530562,618.519516171893,-35.76976183486)) ;
#60012 = CARTESIAN_POINT('Ctrl Pts',(180.941802622243,618.51570093191,-35.7311218745408)) ;
#60013 = CARTESIAN_POINT('Ctrl Pts',(180.893091659676,618.511757452089,-35.6911831277021)) ;
#60014 = CARTESIAN_POINT('Ctrl Pts',(180.842161143015,618.507817277096,-35.6540481292493)) ;
#60015 = CARTESIAN_POINT('Ctrl Pts',(180.789361683744,618.503811044041,-35.6199872221115)) ;
#60016 = CARTESIAN_POINT('Ctrl Pts',(180.743416088697,618.50032485755,-35.590347739664)) ;
#60017 = CARTESIAN_POINT('Ctrl Pts',(180.69605459303,618.49678800037,-35.5630354622988)) ;
#60018 = CARTESIAN_POINT('Ctrl Pts',(180.647538816787,618.493149850119,-35.5382040513801)) ;
#60019 = CARTESIAN_POINT('Ctrl Pts',(180.6403294513,618.492609226905,-35.5345141440816)) ;
#60020 = CARTESIAN_POINT('Ctrl Pts',(180.633094559179,618.492066366991,-35.5308789322976)) ;
#60021 = CARTESIAN_POINT('Ctrl Pts',(180.625834956093,618.49152110427,-35.5272988314416)) ;
#60022 = CARTESIAN_POINT('Ctrl Pts',(180.625806860057,618.491518994001,-35.527284975775)) ;
#60023 = CARTESIAN_POINT('Ctrl Pts',(180.625778763652,618.491516883695,-35.5272711209338)) ;
#60024 = CARTESIAN_POINT('Ctrl Pts',(180.625750666876,618.491514773353,-35.5272572669181)) ;
#60025 = CARTESIAN_POINT('Ctrl Pts',(180.576030268583,618.487780286783,-35.5027410308854)) ;
#60026 = CARTESIAN_POINT('Ctrl Pts',(180.524969197056,618.483923273951,-35.480729384318)) ;
#60027 = CARTESIAN_POINT('Ctrl Pts',(180.472854387436,618.48000695136,-35.4613343960481)) ;
#60028 = CARTESIAN_POINT('Ctrl Pts',(180.468022513008,618.479643845765,-35.4595361711569)) ;
#60029 = CARTESIAN_POINT('Ctrl Pts',(180.463181616492,618.479280230328,-35.4577604315961)) ;
#60030 = CARTESIAN_POINT('Ctrl Pts',(180.45833194852,618.478916155434,-35.4560072611747)) ;
#60031 = CARTESIAN_POINT('Ctrl Pts',(180.400464932603,618.474571955415,-35.4350881505736)) ;
#60032 = CARTESIAN_POINT('Ctrl Pts',(180.341343124075,618.470163005833,-35.4173832741389)) ;
#60033 = CARTESIAN_POINT('Ctrl Pts',(180.281360663462,618.465760686335,-35.4029953114805)) ;
#60034 = CARTESIAN_POINT('Ctrl Pts',(180.222280077188,618.461424558502,-35.3888236809662)) ;
#60035 = CARTESIAN_POINT('Ctrl Pts',(180.162364534116,618.457095145439,-35.3778695236006)) ;
#60036 = CARTESIAN_POINT('Ctrl Pts',(180.10199182776,618.452820103473,-35.3701919206502)) ;
#60037 = CARTESIAN_POINT('Ctrl Pts',(180.041656666309,618.448547720093,-35.362519092289)) ;
#60038 = CARTESIAN_POINT('Ctrl Pts',(179.980864896819,618.444329774189,-35.3581186178058)) ;
#60039 = CARTESIAN_POINT('Ctrl Pts',(179.91999490829,618.440190063795,-35.3570142327182)) ;
#60040 = CARTESIAN_POINT('Ctrl Pts',(179.859140066554,618.436051383519,-35.355910122444)) ;
#60041 = CARTESIAN_POINT('Ctrl Pts',(179.798207065939,618.431990901943,-35.3581004936399)) ;
#60042 = CARTESIAN_POINT('Ctrl Pts',(179.737575273906,618.42800764707,-35.3635744907322)) ;
#60043 = CARTESIAN_POINT('Ctrl Pts',(179.675246879113,618.4239129325,-35.3692016615684)) ;
#60044 = CARTESIAN_POINT('Ctrl Pts',(179.613236858033,618.419899818461,-35.3782991522623)) ;
#60045 = CARTESIAN_POINT('Ctrl Pts',(179.551957974696,618.415940925301,-35.3908154544142)) ;
#60046 = CARTESIAN_POINT('Ctrl Pts',(179.492271481222,618.412084907731,-35.4030065085917)) ;
#60047 = CARTESIAN_POINT('Ctrl Pts',(179.433278761062,618.40827996142,-35.4184411264926)) ;
#60048 = CARTESIAN_POINT('Ctrl Pts',(179.375360275416,618.40447931491,-35.4370315093212)) ;
#60049 = CARTESIAN_POINT('Ctrl Pts',(179.315123958615,618.400526570899,-35.4563658578809)) ;
#60050 = CARTESIAN_POINT('Ctrl Pts',(179.256049933563,618.396578059386,-35.4791144283665)) ;
#60051 = CARTESIAN_POINT('Ctrl Pts',(179.198561508483,618.392563166561,-35.5051265924183)) ;
#60052 = CARTESIAN_POINT('Ctrl Pts',(179.148831933066,618.389090138464,-35.5276280589684)) ;
#60053 = CARTESIAN_POINT('Ctrl Pts',(179.10028791631,618.385566779611,-35.5525718741155)) ;
#60054 = CARTESIAN_POINT('Ctrl Pts',(179.053199503989,618.381942418963,-35.5798214164548)) ;
#60055 = CARTESIAN_POINT('Ctrl Pts',(179.04587875353,618.381378946156,-35.5840578536113)) ;
#60056 = CARTESIAN_POINT('Ctrl Pts',(179.038593084181,618.380813032099,-35.5883500054825)) ;
#60057 = CARTESIAN_POINT('Ctrl Pts',(179.031343398033,618.380244486385,-35.5926973446195)) ;
#60058 = CARTESIAN_POINT('Ctrl Pts',(179.031317627898,618.380242465401,-35.5927127979116)) ;
#60059 = CARTESIAN_POINT('Ctrl Pts',(179.031291858218,618.380240444383,-35.592728251901)) ;
#60060 = CARTESIAN_POINT('Ctrl Pts',(179.031266088992,618.380238423333,-35.5927437065876)) ;
#60061 = CARTESIAN_POINT('Ctrl Pts',(178.983727870414,618.376510055907,-35.6212540030795)) ;
#60062 = CARTESIAN_POINT('Ctrl Pts',(178.937569640057,618.372658630446,-35.6522473603323)) ;
#60063 = CARTESIAN_POINT('Ctrl Pts',(178.893040739353,618.36874728734,-35.6855431319309)) ;
#60064 = CARTESIAN_POINT('Ctrl Pts',(178.888877711047,618.368381613995,-35.6886559696035)) ;
#60065 = CARTESIAN_POINT('Ctrl Pts',(178.884728936709,618.368015416941,-35.6917888961039)) ;
#60066 = CARTESIAN_POINT('Ctrl Pts',(178.880594627477,618.367648747775,-35.6949417418113)) ;
#60067 = CARTESIAN_POINT('Ctrl Pts',(178.831666573002,618.363309350806,-35.732254530445)) ;
#60068 = CARTESIAN_POINT('Ctrl Pts',(178.784762041634,618.358904497748,-35.7723626795533)) ;
#60069 = CARTESIAN_POINT('Ctrl Pts',(178.740180467144,618.354505584414,-35.8149902629322)) ;
#60070 = CARTESIAN_POINT('Ctrl Pts',(178.696241885767,618.350170115922,-35.8570030353077)) ;
#60071 = CARTESIAN_POINT('Ctrl Pts',(178.654559366142,618.345840703961,-35.9014628428434)) ;
#60072 = CARTESIAN_POINT('Ctrl Pts',(178.615387274715,618.341565164946,-35.9480834766588)) ;
#60073 = CARTESIAN_POINT('Ctrl Pts',(178.57623923858,618.337292251509,-35.9946754810876)) ;
#60074 = CARTESIAN_POINT('Ctrl Pts',(178.539598431727,618.333073280143,-36.04342560137)) ;
#60075 = CARTESIAN_POINT('Ctrl Pts',(178.50568976433,618.328932193516,-36.0940280527371)) ;
#60076 = CARTESIAN_POINT('Ctrl Pts',(178.471789310876,618.324792110015,-36.1446182463039)) ;
#60077 = CARTESIAN_POINT('Ctrl Pts',(178.440619709841,618.320729876237,-36.1970598741901)) ;
#60078 = CARTESIAN_POINT('Ctrl Pts',(178.412377294774,618.31674463504,-36.2510276540207)) ;
#60079 = CARTESIAN_POINT('Ctrl Pts',(178.383376399135,618.312652365886,-36.3064447968897)) ;
#60080 = CARTESIAN_POINT('Ctrl Pts',(178.357462357362,618.308641267557,-36.363471294895)) ;
#60081 = CARTESIAN_POINT('Ctrl Pts',(178.334814837055,618.304684149029,-36.4217330290475)) ;
#60082 = CARTESIAN_POINT('Ctrl Pts',(178.312731460251,618.300825601236,-36.4785434794226)) ;
#60083 = CARTESIAN_POINT('Ctrl Pts',(178.293754082553,618.297018013748,-36.5365283491731)) ;
#60084 = CARTESIAN_POINT('Ctrl Pts',(178.278014995893,618.293214675688,-36.5953198544874)) ;
#60085 = CARTESIAN_POINT('Ctrl Pts',(178.261672801505,618.289265597114,-36.6563641977219)) ;
#60086 = CARTESIAN_POINT('Ctrl Pts',(178.248822697785,618.28532067976,-36.7182783197643)) ;
#60087 = CARTESIAN_POINT('Ctrl Pts',(178.239566934482,618.281309682721,-36.7806265090767)) ;
#60088 = CARTESIAN_POINT('Ctrl Pts',(178.231544843613,618.277833299233,-36.8346644985706)) ;
#60089 = CARTESIAN_POINT('Ctrl Pts',(178.226222505982,618.274306621661,-36.8890294525564)) ;
#60090 = CARTESIAN_POINT('Ctrl Pts',(178.22363147269,618.270678912868,-36.9434198669935)) ;
#60091 = CARTESIAN_POINT('Ctrl Pts',(178.223234423111,618.27012300328,-36.9517546464896)) ;
#60092 = CARTESIAN_POINT('Ctrl Pts',(178.222901445326,618.269564721232,-36.9600900986547)) ;
#60093 = CARTESIAN_POINT('Ctrl Pts',(178.2226325834,618.269003884147,-36.9684252219111)) ;
#60094 = CARTESIAN_POINT('Ctrl Pts',(178.222631627995,618.269001891203,-36.9684548409136)) ;
#60095 = CARTESIAN_POINT('Ctrl Pts',(178.222630673399,618.268999898226,-36.9684844599119)) ;
#60096 = CARTESIAN_POINT('Ctrl Pts',(178.222629719612,618.268997905217,-36.9685140789061)) ;
#60097 = CARTESIAN_POINT('Ctrl Pts',(178.220844750902,618.265268077855,-37.0239447132894)) ;
#60098 = CARTESIAN_POINT('Ctrl Pts',(178.221897153798,618.261415407973,-37.0795599854219)) ;
#60099 = CARTESIAN_POINT('Ctrl Pts',(178.225770009133,618.25750304258,-37.1350521154175)) ;
#60100 = CARTESIAN_POINT('Ctrl Pts',(178.226130966848,618.257138402451,-37.1402240907859)) ;
#60101 = CARTESIAN_POINT('Ctrl Pts',(178.22651640212,618.25677324377,-37.1453949666777)) ;
#60102 = CARTESIAN_POINT('Ctrl Pts',(178.226926286903,618.256407617662,-37.150564475947)) ;
#60103 = CARTESIAN_POINT('Ctrl Pts',(178.231789640912,618.252069400506,-37.2119015997002)) ;
#60104 = CARTESIAN_POINT('Ctrl Pts',(178.240098348827,618.247666043529,-37.2730513545185)) ;
#60105 = CARTESIAN_POINT('Ctrl Pts',(178.251782591525,618.243268807749,-37.333612770775)) ;
#60106 = CARTESIAN_POINT('Ctrl Pts',(178.263301349628,618.238933850269,-37.393316452245)) ;
#60107 = CARTESIAN_POINT('Ctrl Pts',(178.278100296117,618.234605129,-37.4524485192166)) ;
#60108 = CARTESIAN_POINT('Ctrl Pts',(178.296076521841,618.230330372981,-37.5106400083246)) ;
#60109 = CARTESIAN_POINT('Ctrl Pts',(178.314041786601,618.226058223484,-37.5687960153033)) ;
#60110 = CARTESIAN_POINT('Ctrl Pts',(178.335180346023,618.22184010836,-37.6260126581506)) ;
#60111 = CARTESIAN_POINT('Ctrl Pts',(178.359356884229,618.217699875044,-37.6819351315033)) ;
#60112 = CARTESIAN_POINT('Ctrl Pts',(178.38352766094,618.213560628384,-37.7378442780082)) ;
#60113 = CARTESIAN_POINT('Ctrl Pts',(178.410734989242,618.209499228755,-37.792459841562)) ;
#60114 = CARTESIAN_POINT('Ctrl Pts',(178.44081168331,618.205514720716,-37.8454404763845)) ;
#60115 = CARTESIAN_POINT('Ctrl Pts',(178.471681683884,618.201425116813,-37.8998185348105)) ;
#60116 = CARTESIAN_POINT('Ctrl Pts',(178.50557469763,618.197416498929,-37.9524740743393)) ;
#60117 = CARTESIAN_POINT('Ctrl Pts',(178.542273756713,618.193461617409,-38.0030537894537)) ;
#60118 = CARTESIAN_POINT('Ctrl Pts',(178.578075628569,618.189603421452,-38.0523969749278)) ;
#60119 = CARTESIAN_POINT('Ctrl Pts',(178.616548090732,618.18579600404,-38.0997644085252)) ;
#60120 = CARTESIAN_POINT('Ctrl Pts',(178.657453529299,618.181992580754,-38.1448455442407)) ;
#60121 = CARTESIAN_POINT('Ctrl Pts',(178.699896590135,618.178046188011,-38.1916212653381)) ;
#60122 = CARTESIAN_POINT('Ctrl Pts',(178.744959556691,618.174103672878,-38.2359349255075)) ;
#60123 = CARTESIAN_POINT('Ctrl Pts',(178.792332068751,618.170094893156,-38.2774650993131)) ;
#60124 = CARTESIAN_POINT('Ctrl Pts',(178.833407260991,618.166619008289,-38.313474586644)) ;
#60125 = CARTESIAN_POINT('Ctrl Pts',(178.876219382718,618.163092650363,-38.3473921510311)) ;
#60126 = CARTESIAN_POINT('Ctrl Pts',(178.920532199528,618.159465125344,-38.3790280332569)) ;
#60127 = CARTESIAN_POINT('Ctrl Pts',(178.927301502472,618.158910978315,-38.3838607856317)) ;
#60128 = CARTESIAN_POINT('Ctrl Pts',(178.934105852788,618.158354470436,-38.3886403877065)) ;
#60129 = CARTESIAN_POINT('Ctrl Pts',(178.940944440391,618.157795420989,-38.3933662655828)) ;
#60130 = CARTESIAN_POINT('Ctrl Pts',(178.940969073529,618.157793407248,-38.3933832885721)) ;
#60131 = CARTESIAN_POINT('Ctrl Pts',(178.940993707112,618.157791393474,-38.3934003108644)) ;
#60132 = CARTESIAN_POINT('Ctrl Pts',(178.941018341139,618.157789379668,-38.3934173324596)) ;
#60133 = CARTESIAN_POINT('Ctrl Pts',(178.986947887101,618.154034685892,-38.4251536842743)) ;
#60134 = CARTESIAN_POINT('Ctrl Pts',(179.034587519952,618.150155694842,-38.4545716490728)) ;
#60135 = CARTESIAN_POINT('Ctrl Pts',(179.083667732432,618.146216600731,-38.4815191143161)) ;
#60136 = CARTESIAN_POINT('Ctrl Pts',(179.088574774354,618.145822769918,-38.4842133231419)) ;
#60137 = CARTESIAN_POINT('Ctrl Pts',(179.093496173381,618.145428338316,-38.486882838659)) ;
#60138 = CARTESIAN_POINT('Ctrl Pts',(179.098431631662,618.145033370078,-38.4895275108052)) ;
#60139 = CARTESIAN_POINT('Ctrl Pts',(179.152640696328,618.140695199735,-38.5185755130836)) ;
#60140 = CARTESIAN_POINT('Ctrl Pts',(179.208551896439,618.136292922672,-38.5446267206134)) ;
#60141 = CARTESIAN_POINT('Ctrl Pts',(179.265796825254,618.131897185162,-38.5675249941924)) ;
#60142 = CARTESIAN_POINT('Ctrl Pts',(179.322953854601,618.127508197298,-38.5903881075203)) ;
#60143 = CARTESIAN_POINT('Ctrl Pts',(179.381440509849,618.123126065173,-38.6101083388411)) ;
#60144 = CARTESIAN_POINT('Ctrl Pts',(179.440883614391,618.118799627606,-38.6265677000373)) ;
#60145 = CARTESIAN_POINT('Ctrl Pts',(179.500273299633,618.114477078047,-38.6430122698199)) ;
#60146 = CARTESIAN_POINT('Ctrl Pts',(179.560617760819,618.110210263012,-38.6562019649169)) ;
#60147 = CARTESIAN_POINT('Ctrl Pts',(179.621538003104,618.106022940803,-38.6660527208549)) ;
#60148 = CARTESIAN_POINT('Ctrl Pts',(179.682426749525,618.101837783448,-38.6758983839358)) ;
#60149 = CARTESIAN_POINT('Ctrl Pts',(179.743890716494,618.097732042013,-38.682408515153)) ;
#60150 = CARTESIAN_POINT('Ctrl Pts',(179.805544051061,618.093703449542,-38.6855321198862)) ;
#60151 = CARTESIAN_POINT('Ctrl Pts',(179.833469375583,618.091878734741,-38.6869469286142)) ;
#60152 = CARTESIAN_POINT('Ctrl Pts',(179.861433445486,618.090069493796,-38.6876674245861)) ;
#60153 = CARTESIAN_POINT('Ctrl Pts',(179.889399881814,618.088273794561,-38.6876911816457)) ;
#60154 = CARTESIAN_POINT('Ctrl Pts',(179.889382603702,618.088003960412,-38.6881599523756)) ;
#60155 = CARTESIAN_POINT('Ctrl Pts',(179.962423314324,618.083373402089,-38.6881224684444)) ;
#60156 = CARTESIAN_POINT('Ctrl Pts',(180.035386280762,618.078875076633,-38.6832817710899)) ;
#60157 = CARTESIAN_POINT('Ctrl Pts',(180.211867029433,618.067988436433,-38.6598500499037)) ;
#60158 = CARTESIAN_POINT('Ctrl Pts',(180.314382464896,618.061663276376,-38.6362294483913)) ;
#60159 = CARTESIAN_POINT('Ctrl Pts',(180.430769124812,618.053833524208,-38.5975468162584)) ;
#60160 = CARTESIAN_POINT('Ctrl Pts',(180.447464000146,618.052693836644,-38.5917011579464)) ;
#60161 = CARTESIAN_POINT('Ctrl Pts',(180.464060715285,618.051541226924,-38.5855915461645)) ;
#60162 = CARTESIAN_POINT('Origin',(179.888527625422,617.710565160536,-37.0221601717597)) ;
#60163 = CARTESIAN_POINT('Ctrl Pts',(180.464060715285,618.051541226924,-38.5855915461645)) ;
#60164 = CARTESIAN_POINT('Ctrl Pts',(180.481897953674,618.050302465268,-38.5790252707955)) ;
#60165 = CARTESIAN_POINT('Ctrl Pts',(180.499621809325,618.04904877561,-38.5721541087867)) ;
#60166 = CARTESIAN_POINT('Ctrl Pts',(180.54651059363,618.045661037341,-38.5530470101377)) ;
#60167 = CARTESIAN_POINT('Ctrl Pts',(180.575446202966,618.043493376976,-38.5402834717153)) ;
#60168 = CARTESIAN_POINT('Ctrl Pts',(180.708426674847,618.033221401202,-38.4770461607259)) ;
#60169 = CARTESIAN_POINT('Ctrl Pts',(180.807395110013,618.024703257508,-38.4166519385844)) ;
#60170 = CARTESIAN_POINT('Ctrl Pts',(180.953122418519,618.0114092671,-38.3054283094891)) ;
#60171 = CARTESIAN_POINT('Ctrl Pts',(181.004389048798,618.006551978326,-38.2611089786966)) ;
#60172 = CARTESIAN_POINT('Ctrl Pts',(181.093844965957,617.997784965623,-38.1737051200831)) ;
#60173 = CARTESIAN_POINT('Ctrl Pts',(181.13277581992,617.99384898638,-38.1315264288429)) ;
#60174 = CARTESIAN_POINT('Ctrl Pts',(181.202199529866,617.986574524375,-38.0480472311912)) ;
#60175 = CARTESIAN_POINT('Ctrl Pts',(181.23311165478,617.983220872074,-38.007184469839)) ;
#60176 = CARTESIAN_POINT('Ctrl Pts',(181.341487075236,617.970925665975,-37.8492917778832)) ;
#60177 = CARTESIAN_POINT('Ctrl Pts',(181.405950168592,617.962514325683,-37.7240642386614)) ;
#60178 = CARTESIAN_POINT('Ctrl Pts',(181.471436080325,617.950761540825,-37.5442384131307)) ;
#60179 = CARTESIAN_POINT('Ctrl Pts',(181.486696060997,617.947597142538,-37.4954695604202)) ;
#60180 = CARTESIAN_POINT('Ctrl Pts',(181.509415473696,617.941915047848,-37.4091215745386)) ;
#60181 = CARTESIAN_POINT('Ctrl Pts',(181.517864380543,617.939436579263,-37.3718424456813)) ;
#60182 = CARTESIAN_POINT('Ctrl Pts',(181.530825902746,617.934818756473,-37.3038895239917)) ;
#60183 = CARTESIAN_POINT('Ctrl Pts',(181.535777960001,617.932701947745,-37.2733190358721)) ;
#60184 = CARTESIAN_POINT('Ctrl Pts',(181.55606650409,617.922033117617,-37.1213570598269)) ;
#60185 = CARTESIAN_POINT('Ctrl Pts',(181.558848367516,617.913001116171,-36.9986751456239)) ;
#60186 = CARTESIAN_POINT('Ctrl Pts',(181.542437192452,617.899377626793,-36.8112979469856)) ;
#60187 = CARTESIAN_POINT('Ctrl Pts',(181.532826603064,617.89466940303,-36.7461851866537)) ;
#60188 = CARTESIAN_POINT('Ctrl Pts',(181.507846104336,617.886112625852,-36.6264873322731)) ;
#60189 = CARTESIAN_POINT('Ctrl Pts',(181.493493454421,617.882241218155,-36.5717876978933)) ;
#60190 = CARTESIAN_POINT('Ctrl Pts',(181.460787725981,617.875011179151,-36.4687975027266)) ;
#60191 = CARTESIAN_POINT('Ctrl Pts',(181.442917151037,617.871641128152,-36.4204241573451)) ;
#60192 = CARTESIAN_POINT('Ctrl Pts',(181.370334565773,617.859700978261,-36.2488863271084)) ;
#60193 = CARTESIAN_POINT('Ctrl Pts',(181.302986370131,617.851604417519,-36.1316471018976)) ;
#60194 = CARTESIAN_POINT('Ctrl Pts',(181.190495127365,617.840091392759,-35.9813697762763)) ;
#60195 = CARTESIAN_POINT('Ctrl Pts',(181.156736065954,617.836815544789,-35.9404898957237)) ;
#60196 = CARTESIAN_POINT('Ctrl Pts',(181.094803513211,617.830967522098,-35.8723858724377)) ;
#60197 = CARTESIAN_POINT('Ctrl Pts',(181.067511624564,617.828438114352,-35.8444171751952)) ;
#60198 = CARTESIAN_POINT('Ctrl Pts',(181.017087578928,617.823789225325,-35.7962527466986)) ;
#60199 = CARTESIAN_POINT('Ctrl Pts',(180.994333773178,617.821696055835,-35.7756896605593)) ;
#60200 = CARTESIAN_POINT('Ctrl Pts',(180.8859585382,617.811787212068,-35.6830513970048)) ;
#60201 = CARTESIAN_POINT('Ctrl Pts',(180.793784812806,617.803562281883,-35.6190969098238)) ;
#60202 = CARTESIAN_POINT('Ctrl Pts',(180.633804794777,617.790276838319,-35.5304637832991)) ;
#60203 = CARTESIAN_POINT('Ctrl Pts',(180.569563479209,617.785166760879,-35.5000602517913)) ;
#60204 = CARTESIAN_POINT('Ctrl Pts',(180.448972575006,617.776046706314,-35.4521573034835)) ;
#60205 = CARTESIAN_POINT('Ctrl Pts',(180.393258611658,617.772004446071,-35.4333695375535)) ;
#60206 = CARTESIAN_POINT('Ctrl Pts',(180.288341428885,617.76469073467,-35.4040681191089)) ;
#60207 = CARTESIAN_POINT('Ctrl Pts',(180.239432459861,617.761396353379,-35.3927616118759)) ;
#60208 = CARTESIAN_POINT('Ctrl Pts',(180.097263404458,617.752089697059,-35.3665960179337)) ;
#60209 = CARTESIAN_POINT('Ctrl Pts',(180.003155295399,617.746266518971,-35.3574299056535)) ;
#60210 = CARTESIAN_POINT('Ctrl Pts',(179.803917019628,617.734083293749,-35.355009218212)) ;
#60211 = CARTESIAN_POINT('Ctrl Pts',(179.699191733516,617.727761225642,-35.3636371751317)) ;
#60212 = CARTESIAN_POINT('Ctrl Pts',(179.560424461082,617.718749503903,-35.388388748647)) ;
#60213 = CARTESIAN_POINT('Ctrl Pts',(179.525083564929,617.716396234846,-35.3958857032905)) ;
#60214 = CARTESIAN_POINT('Ctrl Pts',(179.458974965252,617.711835810747,-35.4121717697229)) ;
#60215 = CARTESIAN_POINT('Ctrl Pts',(179.428163433488,617.709641588438,-35.4207100937302)) ;
#60216 = CARTESIAN_POINT('Ctrl Pts',(179.36111135906,617.704741214122,-35.441385751569)) ;
#60217 = CARTESIAN_POINT('Ctrl Pts',(179.325002435639,617.702020470419,-35.4538953285266)) ;
#60218 = CARTESIAN_POINT('Ctrl Pts',(179.205029954759,617.692769006359,-35.5001369653809)) ;
#60219 = CARTESIAN_POINT('Ctrl Pts',(179.12348652897,617.686133575331,-35.5394477233273)) ;
#60220 = CARTESIAN_POINT('Ctrl Pts',(178.973590584431,617.673587492226,-35.6273830842508)) ;
#60221 = CARTESIAN_POINT('Ctrl Pts',(178.904910537178,617.66767715157,-35.6749355785667)) ;
#60222 = CARTESIAN_POINT('Ctrl Pts',(178.800941350191,617.658506359587,-35.7591290789971)) ;
#60223 = CARTESIAN_POINT('Ctrl Pts',(178.763263218048,617.655126930392,-35.7925779590251)) ;
#60224 = CARTESIAN_POINT('Ctrl Pts',(178.68373363466,617.647836855873,-35.8699036244448)) ;
#60225 = CARTESIAN_POINT('Ctrl Pts',(178.64264363275,617.643963540511,-35.9144606854707)) ;
#60226 = CARTESIAN_POINT('Ctrl Pts',(178.495167109237,617.629437107523,-36.0929978521746)) ;
#60227 = CARTESIAN_POINT('Ctrl Pts',(178.407232128629,617.619482714398,-36.2407877980694)) ;
#60228 = CARTESIAN_POINT('Ctrl Pts',(178.330962865376,617.606334115431,-36.4300103031779)) ;
#60229 = CARTESIAN_POINT('Ctrl Pts',(178.319517726683,617.604162615672,-36.4610389239493)) ;
#60230 = CARTESIAN_POINT('Ctrl Pts',(178.298025315358,617.599607077456,-36.5251185099032)) ;
#60231 = CARTESIAN_POINT('Ctrl Pts',(178.288067709336,617.59722021884,-36.5581821585891)) ;
#60232 = CARTESIAN_POINT('Ctrl Pts',(178.252184011448,617.587459129075,-36.6922886260786)) ;
#60233 = CARTESIAN_POINT('Ctrl Pts',(178.234746540399,617.579793336494,-36.7953527166721)) ;
#60234 = CARTESIAN_POINT('Ctrl Pts',(178.219806339448,617.565078570355,-36.9974984904036)) ;
#60235 = CARTESIAN_POINT('Ctrl Pts',(178.221260917136,617.558048176043,-37.096096092647)) ;
#60236 = CARTESIAN_POINT('Ctrl Pts',(178.236591290263,617.547836417959,-37.243930067945)) ;
#60237 = CARTESIAN_POINT('Ctrl Pts',(178.244022889307,617.54445897066,-37.2936019992806)) ;
#60238 = CARTESIAN_POINT('Ctrl Pts',(178.264971093302,617.537288777169,-37.4003877287565)) ;
#60239 = CARTESIAN_POINT('Ctrl Pts',(178.279283479626,617.533526962457,-37.4572767621196)) ;
#60240 = CARTESIAN_POINT('Ctrl Pts',(178.317408361774,617.525387688406,-37.5808535502216)) ;
#60241 = CARTESIAN_POINT('Ctrl Pts',(178.342529754871,617.521052477997,-37.6470166490607)) ;
#60242 = CARTESIAN_POINT('Ctrl Pts',(178.418383129549,617.509851591488,-37.8139436064132)) ;
#60243 = CARTESIAN_POINT('Ctrl Pts',(178.475261176036,617.503047173335,-37.9114950001219)) ;
#60244 = CARTESIAN_POINT('Ctrl Pts',(178.559547380461,617.493728927175,-38.0272993081169)) ;
#60245 = CARTESIAN_POINT('Ctrl Pts',(178.578237443446,617.49169889003,-38.0515447945929)) ;
#60246 = CARTESIAN_POINT('Ctrl Pts',(178.622388799909,617.486954332514,-38.1056673925264)) ;
#60247 = CARTESIAN_POINT('Ctrl Pts',(178.648253970182,617.484216302292,-38.135181308198)) ;
#60248 = CARTESIAN_POINT('Ctrl Pts',(178.711701551785,617.477648053624,-38.2026195335171)) ;
#60249 = CARTESIAN_POINT('Ctrl Pts',(178.750113677462,617.47378401114,-38.2397056173296)) ;
#60250 = CARTESIAN_POINT('Ctrl Pts',(178.89083544996,617.460172189489,-38.3630797396613)) ;
#60251 = CARTESIAN_POINT('Ctrl Pts',(179.001713128486,617.45043168011,-38.438856263214)) ;
#60252 = CARTESIAN_POINT('Ctrl Pts',(179.166289939739,617.437632975247,-38.524356562795)) ;
#60253 = CARTESIAN_POINT('Ctrl Pts',(179.213188107954,617.434144599432,-38.5460167409303)) ;
#60254 = CARTESIAN_POINT('Ctrl Pts',(179.313255941849,617.427001611517,-38.5867041908084)) ;
#60255 = CARTESIAN_POINT('Ctrl Pts',(179.366538847938,617.423366244538,-38.6052787333947)) ;
#60256 = CARTESIAN_POINT('Ctrl Pts',(179.483502705193,617.415661988358,-38.6395028159113)) ;
#60257 = CARTESIAN_POINT('Ctrl Pts',(179.547371262191,617.411625001174,-38.6541698911928)) ;
#60258 = CARTESIAN_POINT('Ctrl Pts',(179.733491680605,617.400071792041,-38.6855041671382)) ;
#60259 = CARTESIAN_POINT('Ctrl Pts',(179.856919981988,617.392680955341,-38.6924120822337)) ;
#60260 = CARTESIAN_POINT('Ctrl Pts',(180.010811444156,617.38266695113,-38.6839535939988)) ;
#60261 = CARTESIAN_POINT('Ctrl Pts',(180.041608285039,617.380620620016,-38.6814000296106)) ;
#60262 = CARTESIAN_POINT('Ctrl Pts',(180.110659331588,617.375906596588,-38.6737357262902)) ;
#60263 = CARTESIAN_POINT('Ctrl Pts',(180.148839272739,617.373218078077,-38.6681497055414)) ;
#60264 = CARTESIAN_POINT('Ctrl Pts',(180.281221338282,617.363685573126,-38.6440605424444)) ;
#60265 = CARTESIAN_POINT('Ctrl Pts',(180.373989177562,617.356640793906,-38.6187486185409)) ;
#60266 = CARTESIAN_POINT('Ctrl Pts',(180.464057359858,617.349676493477,-38.5855927813658)) ;
#60267 = CARTESIAN_POINT('Ctrl Pts',(180.464060715702,618.242141445689,-38.5855915460107)) ;
#60268 = CARTESIAN_POINT('Ctrl Pts',(180.490194428087,618.240442558113,-38.5759711581275)) ;
#60269 = CARTESIAN_POINT('Ctrl Pts',(180.51609650473,618.238746139063,-38.5656919854818)) ;
#60270 = CARTESIAN_POINT('Ctrl Pts',(180.604553925177,618.232876486745,-38.5279903063056)) ;
#60271 = CARTESIAN_POINT('Ctrl Pts',(180.665657202885,618.228684944444,-38.4973844480904)) ;
#60272 = CARTESIAN_POINT('Ctrl Pts',(180.774581177908,618.220751282732,-38.4341765186819)) ;
#60273 = CARTESIAN_POINT('Ctrl Pts',(180.822913785187,618.217046656664,-38.4026681695486)) ;
#60274 = CARTESIAN_POINT('Ctrl Pts',(180.910828907134,618.209872686146,-38.338621019691)) ;
#60275 = CARTESIAN_POINT('Ctrl Pts',(180.950733997755,618.206428499142,-38.3066389331058)) ;
#60276 = CARTESIAN_POINT('Ctrl Pts',(181.095794146144,618.19312813507,-38.1789924057104)) ;
#60277 = CARTESIAN_POINT('Ctrl Pts',(181.190016720997,618.182763120211,-38.071857226188)) ;
#60278 = CARTESIAN_POINT('Ctrl Pts',(181.29771299437,618.168776489805,-37.912272000729)) ;
#60279 = CARTESIAN_POINT('Ctrl Pts',(181.324027984768,618.165131180131,-37.8691795562848)) ;
#60280 = CARTESIAN_POINT('Ctrl Pts',(181.366644813164,618.158872424577,-37.7916843154949)) ;
#60281 = CARTESIAN_POINT('Ctrl Pts',(181.38380119825,618.156228951123,-37.7577927976852)) ;
#60282 = CARTESIAN_POINT('Ctrl Pts',(181.412962731757,618.151533023018,-37.6949408348441)) ;
#60283 = CARTESIAN_POINT('Ctrl Pts',(181.425336677519,618.149462748053,-37.6661743641821)) ;
#60284 = CARTESIAN_POINT('Ctrl Pts',(181.481202190975,618.139644580347,-37.5255040248104)) ;
#60285 = CARTESIAN_POINT('Ctrl Pts',(181.513328644025,618.132436677686,-37.409454884974)) ;
#60286 = CARTESIAN_POINT('Ctrl Pts',(181.543457971187,618.121017193802,-37.225152904422)) ;
#60287 = CARTESIAN_POINT('Ctrl Pts',(181.550254256156,618.116913500324,-37.1587768240989)) ;
#60288 = CARTESIAN_POINT('Ctrl Pts',(181.555453049174,618.109102948324,-37.035182985312)) ;
#60289 = CARTESIAN_POINT('Ctrl Pts',(181.554921452956,618.105430084247,-36.9781105238886)) ;
#60290 = CARTESIAN_POINT('Ctrl Pts',(181.548326608462,618.098240988607,-36.8695043256539)) ;
#60291 = CARTESIAN_POINT('Ctrl Pts',(181.542781725836,618.09474582968,-36.8180063112746)) ;
#60292 = CARTESIAN_POINT('Ctrl Pts',(181.514217595271,618.081890330671,-36.6338123856813)) ;
#60293 = CARTESIAN_POINT('Ctrl Pts',(181.477537922047,618.072092912377,-36.5037827927049)) ;
#60294 = CARTESIAN_POINT('Ctrl Pts',(181.4051474434,618.058446751,-36.330610455888)) ;
#60295 = CARTESIAN_POINT('Ctrl Pts',(181.382331038764,618.054602807897,-36.2826138745859)) ;
#60296 = CARTESIAN_POINT('Ctrl Pts',(181.33877039037,618.048059947729,-36.2012544218042)) ;
#60297 = CARTESIAN_POINT('Ctrl Pts',(181.319067309146,618.04532760079,-36.1673811517677)) ;
#60298 = CARTESIAN_POINT('Ctrl Pts',(181.281655611491,618.040562685271,-36.1079870961481)) ;
#60299 = CARTESIAN_POINT('Ctrl Pts',(181.264395351703,618.038507677835,-36.082210112539)) ;
#60300 = CARTESIAN_POINT('Ctrl Pts',(181.18324135259,618.029404533506,-35.9680419194571)) ;
#60301 = CARTESIAN_POINT('Ctrl Pts',(181.111474053317,618.022802296828,-35.8855610055033)) ;
#60302 = CARTESIAN_POINT('Ctrl Pts',(180.979684533357,618.011732999542,-35.7611534299474)) ;
#60303 = CARTESIAN_POINT('Ctrl Pts',(180.924060478161,618.007314191531,-35.7150901261825)) ;
#60304 = CARTESIAN_POINT('Ctrl Pts',(180.817543656596,617.9990439276,-35.6379601023475)) ;
#60305 = CARTESIAN_POINT('Ctrl Pts',(180.767636494697,617.995237429849,-35.6057397172037)) ;
#60306 = CARTESIAN_POINT('Ctrl Pts',(180.67230584161,617.98800298968,-35.5511753422206)) ;
#60307 = CARTESIAN_POINT('Ctrl Pts',(180.627378452858,617.984607805762,-35.5281042324051)) ;
#60308 = CARTESIAN_POINT('Ctrl Pts',(180.492855145002,617.97444604565,-35.4665763354144)) ;
#60309 = CARTESIAN_POINT('Ctrl Pts',(180.400862332379,617.967489679353,-35.4339031853769)) ;
#60310 = CARTESIAN_POINT('Ctrl Pts',(180.205307591823,617.952828631034,-35.3832133669089)) ;
#60311 = CARTESIAN_POINT('Ctrl Pts',(180.101808264679,617.945138619823,-35.3665607107201)) ;
#60312 = CARTESIAN_POINT('Ctrl Pts',(179.962411799729,617.935307397315,-35.3574294270901)) ;
#60313 = CARTESIAN_POINT('Ctrl Pts',(179.927329284662,617.932878886535,-35.3562423325857)) ;
#60314 = CARTESIAN_POINT('Ctrl Pts',(179.859148410935,617.928280646042,-35.3560907253344)) ;
#60315 = CARTESIAN_POINT('Ctrl Pts',(179.826067574678,617.926106581649,-35.3570026463725)) ;
#60316 = CARTESIAN_POINT('Ctrl Pts',(179.622054283409,617.912930531312,-35.3687158150226)) ;
#60317 = CARTESIAN_POINT('Ctrl Pts',(179.453592199867,617.902959063726,-35.4048368675258)) ;
#60318 = CARTESIAN_POINT('Ctrl Pts',(179.236807105958,617.888398989924,-35.4877188114953)) ;
#60319 = CARTESIAN_POINT('Ctrl Pts',(179.181273563675,617.884512014318,-35.5125111275231)) ;
#60320 = CARTESIAN_POINT('Ctrl Pts',(179.082117176405,617.877183776244,-35.5634519465076)) ;
#60321 = CARTESIAN_POINT('Ctrl Pts',(179.038097834638,617.873779650298,-35.5886694350974)) ;
#60322 = CARTESIAN_POINT('Ctrl Pts',(178.870350467298,617.860149939329,-35.6952154510869)) ;
#60323 = CARTESIAN_POINT('Ctrl Pts',(178.756556325577,617.849354523522,-35.7908641331461)) ;
#60324 = CARTESIAN_POINT('Ctrl Pts',(178.623170438448,617.834965240491,-35.9372923197068)) ;
#60325 = CARTESIAN_POINT('Ctrl Pts',(178.591111446813,617.83134612524,-35.9758433125001)) ;
#60326 = CARTESIAN_POINT('Ctrl Pts',(178.5379905656,617.825124128182,-36.0459244798413)) ;
#60327 = CARTESIAN_POINT('Ctrl Pts',(178.516174348507,617.822491688664,-36.0768382457494)) ;
#60328 = CARTESIAN_POINT('Ctrl Pts',(178.478181265355,617.817797384028,-36.1347662242504)) ;
#60329 = CARTESIAN_POINT('Ctrl Pts',(178.461682738277,617.815718549283,-36.1615448824615)) ;
#60330 = CARTESIAN_POINT('Ctrl Pts',(178.386570477318,617.805980574862,-36.2915631430463)) ;
#60331 = CARTESIAN_POINT('Ctrl Pts',(178.338337018995,617.798845451376,-36.4004171944896)) ;
#60332 = CARTESIAN_POINT('Ctrl Pts',(178.281630845691,617.787485780771,-36.5772719921208)) ;
#60333 = CARTESIAN_POINT('Ctrl Pts',(178.265045721292,617.783362615903,-36.6422282488572)) ;
#60334 = CARTESIAN_POINT('Ctrl Pts',(178.241632304904,617.775522841004,-36.7641637083477)) ;
#60335 = CARTESIAN_POINT('Ctrl Pts',(178.233748462783,617.771840787283,-36.8208368324697)) ;
#60336 = CARTESIAN_POINT('Ctrl Pts',(178.224306918,617.764641388769,-36.9293866685259)) ;
#60337 = CARTESIAN_POINT('Ctrl Pts',(178.2222279399,617.761145566237,-36.981150417142)) ;
#60338 = CARTESIAN_POINT('Ctrl Pts',(178.223436185084,617.748245595999,-37.1681850253089)) ;
#60339 = CARTESIAN_POINT('Ctrl Pts',(178.240780196684,617.738399051056,-37.3028164182479)) ;
#60340 = CARTESIAN_POINT('Ctrl Pts',(178.287279400566,617.724716188803,-37.4851555156929)) ;
#60341 = CARTESIAN_POINT('Ctrl Pts',(178.30280591029,617.720883078943,-37.5358214309226)) ;
#60342 = CARTESIAN_POINT('Ctrl Pts',(178.333947161654,617.714355432036,-37.6224640495473)) ;
#60343 = CARTESIAN_POINT('Ctrl Pts',(178.348466762302,617.71162764015,-37.6587906234727)) ;
#60344 = CARTESIAN_POINT('Ctrl Pts',(178.376753752475,617.706870023981,-37.7229133633042)) ;
#60345 = CARTESIAN_POINT('Ctrl Pts',(178.390042208449,617.704817839497,-37.750896646296)) ;
#60346 = CARTESIAN_POINT('Ctrl Pts',(178.453788972829,617.695692104082,-37.8760095192563)) ;
#60347 = CARTESIAN_POINT('Ctrl Pts',(178.512969306994,617.68906890695,-37.9684052799323)) ;
#60348 = CARTESIAN_POINT('Ctrl Pts',(178.625433370478,617.677983737327,-38.110893464217)) ;
#60349 = CARTESIAN_POINT('Ctrl Pts',(178.673692213999,617.67357124519,-38.164491644234)) ;
#60350 = CARTESIAN_POINT('Ctrl Pts',(178.76773664091,617.665310238577,-38.2562198768082)) ;
#60351 = CARTESIAN_POINT('Ctrl Pts',(178.812385195234,617.661506511059,-38.2953419920857)) ;
#60352 = CARTESIAN_POINT('Ctrl Pts',(178.898698805325,617.654276242552,-38.3631828414228)) ;
#60353 = CARTESIAN_POINT('Ctrl Pts',(178.939768869025,617.650882377663,-38.392546522685)) ;
#60354 = CARTESIAN_POINT('Ctrl Pts',(179.066737170712,617.640487596817,-38.4748786383695)) ;
#60355 = CARTESIAN_POINT('Ctrl Pts',(179.156164820347,617.633277320209,-38.5219498022823)) ;
#60356 = CARTESIAN_POINT('Ctrl Pts',(179.320072900304,617.620387193143,-38.5900541117436)) ;
#60357 = CARTESIAN_POINT('Ctrl Pts',(179.392808387375,617.614775331473,-38.6145467771622)) ;
#60358 = CARTESIAN_POINT('Ctrl Pts',(179.513421079715,617.605836683831,-38.6460924593733)) ;
#60359 = CARTESIAN_POINT('Ctrl Pts',(179.560377762781,617.60244506509,-38.6562286103148)) ;
#60360 = CARTESIAN_POINT('Ctrl Pts',(179.636914680734,617.597124331008,-38.6693167197998)) ;
#60361 = CARTESIAN_POINT('Ctrl Pts',(179.666243421498,617.595137480711,-38.673530440253)) ;
#60362 = CARTESIAN_POINT('Ctrl Pts',(179.749303130417,617.589644790209,-38.6832102881073)) ;
#60363 = CARTESIAN_POINT('Ctrl Pts',(179.803208794525,617.586228243378,-38.6868502193651)) ;
#60364 = CARTESIAN_POINT('Ctrl Pts',(179.966553087462,617.576069001618,-38.6899221444192)) ;
#60365 = CARTESIAN_POINT('Ctrl Pts',(180.075843088827,617.569517619354,-38.6812058408644)) ;
#60366 = CARTESIAN_POINT('Ctrl Pts',(180.254133677697,617.558300975726,-38.6491327420644)) ;
#60367 = CARTESIAN_POINT('Ctrl Pts',(180.323870596851,617.553777851979,-38.6318750748062)) ;
#60368 = CARTESIAN_POINT('Ctrl Pts',(180.416389474131,617.547459445753,-38.6025265992448)) ;
#60369 = CARTESIAN_POINT('Ctrl Pts',(180.440325112796,617.545795552742,-38.5943291378804)) ;
#60370 = CARTESIAN_POINT('Ctrl Pts',(180.464060729575,617.544113575794,-38.585591540904)) ;
#60371 = CARTESIAN_POINT('Origin',(29.8885276254218,617.710565160562,-37.0221601717529)) ;
#60372 = CARTESIAN_POINT('Ctrl Pts',(30.4640776573931,618.051524931058,-38.5855853092948)) ;
#60373 = CARTESIAN_POINT('Ctrl Pts',(30.4818456719863,618.050290927823,-38.5790442980743)) ;
#60374 = CARTESIAN_POINT('Ctrl Pts',(30.4995011921984,618.049042110479,-38.5722007556456)) ;
#60375 = CARTESIAN_POINT('Ctrl Pts',(30.5462955678426,618.045661610561,-38.5531387759382)) ;
#60376 = CARTESIAN_POINT('Ctrl Pts',(30.5752048818118,618.04349626312,-38.5403920002099)) ;
#60377 = CARTESIAN_POINT('Ctrl Pts',(30.7084201927192,618.033207854487,-38.4770719684504)) ;
#60378 = CARTESIAN_POINT('Ctrl Pts',(30.8076237962935,618.024668323971,-38.4165243395425)) ;
#60379 = CARTESIAN_POINT('Ctrl Pts',(30.9534704852753,618.011360591802,-38.3051350959759)) ;
#60380 = CARTESIAN_POINT('Ctrl Pts',(31.0046631393638,618.006509591305,-38.2608575267715)) ;
#60381 = CARTESIAN_POINT('Ctrl Pts',(31.0940165469926,617.997751623709,-38.1735235524342)) ;
#60382 = CARTESIAN_POINT('Ctrl Pts',(31.1329149943528,617.993818537425,-38.131368290329)) ;
#60383 = CARTESIAN_POINT('Ctrl Pts',(31.2023047439392,617.986547018802,-38.0479124602167)) ;
#60384 = CARTESIAN_POINT('Ctrl Pts',(31.2332123482895,617.983193540939,-38.0070469768964)) ;
#60385 = CARTESIAN_POINT('Ctrl Pts',(31.3414893771724,617.970908134843,-37.849263170228)) ;
#60386 = CARTESIAN_POINT('Ctrl Pts',(31.405888891316,617.962504936777,-37.7241677596789)) ;
#60387 = CARTESIAN_POINT('Ctrl Pts',(31.4713684294433,617.950758747922,-37.5444477170903)) ;
#60388 = CARTESIAN_POINT('Ctrl Pts',(31.4866471646106,617.947591831547,-37.4956393027532)) ;
#60389 = CARTESIAN_POINT('Ctrl Pts',(31.5093891828534,617.941906059241,-37.4092334991467)) ;
#60390 = CARTESIAN_POINT('Ctrl Pts',(31.5178445228336,617.939426510315,-37.3719369672922)) ;
#60391 = CARTESIAN_POINT('Ctrl Pts',(31.5308101022122,617.93480854639,-37.3039801052054)) ;
#60392 = CARTESIAN_POINT('Ctrl Pts',(31.5357617716007,617.9326927768,-37.2734234931605)) ;
#60393 = CARTESIAN_POINT('Ctrl Pts',(31.5560746289672,617.922017345664,-37.1213625090232)) ;
#60394 = CARTESIAN_POINT('Ctrl Pts',(31.5588552417217,617.912976513806,-36.9985643991712)) ;
#60395 = CARTESIAN_POINT('Ctrl Pts',(31.5424119202767,617.899347648282,-36.8111112224762)) ;
#60396 = CARTESIAN_POINT('Ctrl Pts',(31.5328000530154,617.894642212824,-36.7460357643791)) ;
#60397 = CARTESIAN_POINT('Ctrl Pts',(31.5078226835382,617.886089580696,-36.6263942265101)) ;
#60398 = CARTESIAN_POINT('Ctrl Pts',(31.4934720677684,617.882219584392,-36.5717138933188)) ;
#60399 = CARTESIAN_POINT('Ctrl Pts',(31.4607696472319,617.874991198607,-36.468746469291)) ;
#60400 = CARTESIAN_POINT('Ctrl Pts',(31.4428987856974,617.871621439277,-36.4203770229569)) ;
#60401 = CARTESIAN_POINT('Ctrl Pts',(31.3703281803715,617.859684239035,-36.2488809902844)) ;
#60402 = CARTESIAN_POINT('Ctrl Pts',(31.303000783241,617.85158996359,-36.1316759864843)) ;
#60403 = CARTESIAN_POINT('Ctrl Pts',(31.1905334887416,617.840078860783,-35.9814172372909)) ;
#60404 = CARTESIAN_POINT('Ctrl Pts',(31.1567691755805,617.836802427588,-35.9405282078948)) ;
#60405 = CARTESIAN_POINT('Ctrl Pts',(31.094829049508,617.830953626428,-35.8724125513417)) ;
#60406 = CARTESIAN_POINT('Ctrl Pts',(31.0675354311014,617.828424046375,-35.8444408971369)) ;
#60407 = CARTESIAN_POINT('Ctrl Pts',(31.0171161273781,617.823775587866,-35.7962792455947)) ;
#60408 = CARTESIAN_POINT('Ctrl Pts',(30.9943692913621,617.821683057149,-35.7757213844907)) ;
#60409 = CARTESIAN_POINT('Ctrl Pts',(30.8859443273232,617.811769591665,-35.6830342742105)) ;
#60410 = CARTESIAN_POINT('Ctrl Pts',(30.7937035328853,617.803538683679,-35.6190382322996)) ;
#60411 = CARTESIAN_POINT('Ctrl Pts',(30.6336727989741,617.790249959462,-35.5303993200199)) ;
#60412 = CARTESIAN_POINT('Ctrl Pts',(30.5694572331204,617.785142238358,-35.5000141661783)) ;
#60413 = CARTESIAN_POINT('Ctrl Pts',(30.4489076266454,617.776025657702,-35.4521347194695)) ;
#60414 = CARTESIAN_POINT('Ctrl Pts',(30.3932081870512,617.771984564492,-35.4333541118267)) ;
#60415 = CARTESIAN_POINT('Ctrl Pts',(30.2883116761563,617.764672414124,-35.4040609573287)) ;
#60416 = CARTESIAN_POINT('Ctrl Pts',(30.2394084863563,617.761378460968,-35.3927566374694)) ;
#60417 = CARTESIAN_POINT('Ctrl Pts',(30.0972470102894,617.752072374018,-35.3665940584388)) ;
#60418 = CARTESIAN_POINT('Ctrl Pts',(30.0031407018643,617.746249342071,-35.3574290077688)) ;
#60419 = CARTESIAN_POINT('Ctrl Pts',(29.8039076173302,617.734066485181,-35.3550099045083)) ;
#60420 = CARTESIAN_POINT('Ctrl Pts',(29.6991857058721,617.727744633259,-35.3636380733002)) ;
#60421 = CARTESIAN_POINT('Ctrl Pts',(29.5604244046807,617.718733336085,-35.3883888196727)) ;
#60422 = CARTESIAN_POINT('Ctrl Pts',(29.5250861460649,617.716380256525,-35.3958851863884)) ;
#60423 = CARTESIAN_POINT('Ctrl Pts',(29.4589862350037,617.71182047343,-35.4121688880796)) ;
#60424 = CARTESIAN_POINT('Ctrl Pts',(29.4281807049303,617.709626711706,-35.4207052546039)) ;
#60425 = CARTESIAN_POINT('Ctrl Pts',(29.3611441736728,617.704727563542,-35.4413750519209)) ;
#60426 = CARTESIAN_POINT('Ctrl Pts',(29.3250446726323,617.702007596982,-35.4538804024139)) ;
#60427 = CARTESIAN_POINT('Ctrl Pts',(29.205128899131,617.692760763286,-35.5000956307671)) ;
#60428 = CARTESIAN_POINT('Ctrl Pts',(29.1236295352537,617.686129251742,-35.5393771226264)) ;
#60429 = CARTESIAN_POINT('Ctrl Pts',(28.9738555782342,617.673594072776,-35.6272153975295)) ;
#60430 = CARTESIAN_POINT('Ctrl Pts',(28.9052495406499,617.667690568227,-35.6746944628909)) ;
#60431 = CARTESIAN_POINT('Ctrl Pts',(28.8013261420252,617.658524957484,-35.7587974524013)) ;
#60432 = CARTESIAN_POINT('Ctrl Pts',(28.7636306321819,617.655144428079,-35.7922414189451)) ;
#60433 = CARTESIAN_POINT('Ctrl Pts',(28.684157823262,617.647860736573,-35.8694665821047)) ;
#60434 = CARTESIAN_POINT('Ctrl Pts',(28.643131838263,617.643994449372,-35.9139184005192)) ;
#60435 = CARTESIAN_POINT('Ctrl Pts',(28.5567277594694,617.635487501786,-36.0184118363563)) ;
#60436 = CARTESIAN_POINT('Ctrl Pts',(28.5128168078336,617.630898412853,-36.0794925029505)) ;
#60437 = CARTESIAN_POINT('Ctrl Pts',(28.4199550443869,617.620151354334,-36.2290458686609)) ;
#60438 = CARTESIAN_POINT('Ctrl Pts',(28.3746356837195,617.614019268511,-36.3194073610899)) ;
#60439 = CARTESIAN_POINT('Ctrl Pts',(28.3263148046611,617.605447153156,-36.442479280643)) ;
#60440 = CARTESIAN_POINT('Ctrl Pts',(28.3156840190504,617.603375712698,-36.4719768539655)) ;
#60441 = CARTESIAN_POINT('Ctrl Pts',(28.2942597075081,617.598730379822,-36.5371317734945)) ;
#60442 = CARTESIAN_POINT('Ctrl Pts',(28.2838179719575,617.596141088353,-36.5728839674862)) ;
#60443 = CARTESIAN_POINT('Ctrl Pts',(28.2481799774797,617.585982904501,-36.7120819264732)) ;
#60444 = CARTESIAN_POINT('Ctrl Pts',(28.2317228367642,617.578145749688,-36.8175006276438)) ;
#60445 = CARTESIAN_POINT('Ctrl Pts',(28.2200722279935,617.563857051982,-37.0144211210282)) ;
#60446 = CARTESIAN_POINT('Ctrl Pts',(28.2221293580943,617.557391996336,-37.1053757923779)) ;
#60447 = CARTESIAN_POINT('Ctrl Pts',(28.2368128262116,617.547712859347,-37.2455536526412)) ;
#60448 = CARTESIAN_POINT('Ctrl Pts',(28.2442783419981,617.5443432134,-37.2951284196061)) ;
#60449 = CARTESIAN_POINT('Ctrl Pts',(28.2653598088032,617.537162685162,-37.4020984579944)) ;
#60450 = CARTESIAN_POINT('Ctrl Pts',(28.2798102019331,617.533384023455,-37.4592601579964)) ;
#60451 = CARTESIAN_POINT('Ctrl Pts',(28.3184101836088,617.52518551653,-37.5837537888375)) ;
#60452 = CARTESIAN_POINT('Ctrl Pts',(28.3439248318459,617.520809406309,-37.6505385477115)) ;
#60453 = CARTESIAN_POINT('Ctrl Pts',(28.4196780636781,617.509691722744,-37.8160561374397)) ;
#60454 = CARTESIAN_POINT('Ctrl Pts',(28.4756028865259,617.503003894171,-37.9117817467726)) ;
#60455 = CARTESIAN_POINT('Ctrl Pts',(28.5586555933462,617.493816530612,-38.0261231713888)) ;
#60456 = CARTESIAN_POINT('Ctrl Pts',(28.5774087359438,617.49177902755,-38.0504930315122)) ;
#60457 = CARTESIAN_POINT('Ctrl Pts',(28.6213285451078,617.487058127052,-38.1044114277407)) ;
#60458 = CARTESIAN_POINT('Ctrl Pts',(28.6468725582231,617.484352754573,-38.1336246865377)) ;
#60459 = CARTESIAN_POINT('Ctrl Pts',(28.7092403974957,617.477890662774,-38.2001163093121)) ;
#60460 = CARTESIAN_POINT('Ctrl Pts',(28.7468501226909,617.474101439079,-38.2366027750438)) ;
#60461 = CARTESIAN_POINT('Ctrl Pts',(28.8885330197957,617.46036169212,-38.3616479536149)) ;
#60462 = CARTESIAN_POINT('Ctrl Pts',(29.0017041054897,617.450409256473,-38.4391197454327)) ;
#60463 = CARTESIAN_POINT('Ctrl Pts',(29.1687690805487,617.43743934702,-38.5255395688852)) ;
#60464 = CARTESIAN_POINT('Ctrl Pts',(29.2155312610575,617.433966408222,-38.5470466895237)) ;
#60465 = CARTESIAN_POINT('Ctrl Pts',(29.3158620762587,617.42681389369,-38.587674758124)) ;
#60466 = CARTESIAN_POINT('Ctrl Pts',(29.3695650709878,617.423155481785,-38.6062879455168)) ;
#60467 = CARTESIAN_POINT('Ctrl Pts',(29.4878944797641,617.415373055664,-38.64063445404)) ;
#60468 = CARTESIAN_POINT('Ctrl Pts',(29.5527225575204,617.411282742807,-38.6553171937956)) ;
#60469 = CARTESIAN_POINT('Ctrl Pts',(29.7366612888557,617.399877920146,-38.6855576059664)) ;
#60470 = CARTESIAN_POINT('Ctrl Pts',(29.8568045362706,617.392671455821,-38.692172106418)) ;
#60471 = CARTESIAN_POINT('Ctrl Pts',(30.0077543928523,617.382863710481,-38.6841813934836)) ;
#60472 = CARTESIAN_POINT('Ctrl Pts',(30.0388585672411,617.380800388477,-38.681657096448)) ;
#60473 = CARTESIAN_POINT('Ctrl Pts',(30.1074146886604,617.376126461875,-38.674150100114)) ;
#60474 = CARTESIAN_POINT('Ctrl Pts',(30.1448019559705,617.373498443337,-38.6687643008992)) ;
#60475 = CARTESIAN_POINT('Ctrl Pts',(30.2780697697598,617.36392042104,-38.6449182485453)) ;
#60476 = CARTESIAN_POINT('Ctrl Pts',(30.3724668659848,617.356753594313,-38.6193101182596)) ;
#60477 = CARTESIAN_POINT('Ctrl Pts',(30.4640740060252,617.349670188918,-38.5855866534828)) ;
#60478 = CARTESIAN_POINT('Ctrl Pts',(30.4640776731659,618.242171075974,-38.5855853034883)) ;
#60479 = CARTESIAN_POINT('Ctrl Pts',(30.478405831787,618.24123936245,-38.5803106202233)) ;
#60480 = CARTESIAN_POINT('Ctrl Pts',(30.4926650383209,618.240308364873,-38.5748376596405)) ;
#60481 = CARTESIAN_POINT('Ctrl Pts',(30.575751765421,618.234852090735,-38.541628719478)) ;
#60482 = CARTESIAN_POINT('Ctrl Pts',(30.64273248298,618.230321559955,-38.5095188079244)) ;
#60483 = CARTESIAN_POINT('Ctrl Pts',(30.7597095722704,618.221895633445,-38.4435022114046)) ;
#60484 = CARTESIAN_POINT('Ctrl Pts',(30.8104287437074,618.218049965343,-38.411141148849)) ;
#60485 = CARTESIAN_POINT('Ctrl Pts',(30.9002930855428,618.210781366303,-38.3467102479627)) ;
#60486 = CARTESIAN_POINT('Ctrl Pts',(30.9399406736874,618.207394080935,-38.3154628759016)) ;
#60487 = CARTESIAN_POINT('Ctrl Pts',(31.0901105503909,618.193779859586,-38.1856359376912)) ;
#60488 = CARTESIAN_POINT('Ctrl Pts',(31.1886875255874,618.182979929582,-38.0743215218763)) ;
#60489 = CARTESIAN_POINT('Ctrl Pts',(31.2991000518324,618.168601050621,-37.9100426161833)) ;
#60490 = CARTESIAN_POINT('Ctrl Pts',(31.3250807476398,618.164994686982,-37.8673616701239)) ;
#60491 = CARTESIAN_POINT('Ctrl Pts',(31.3672539176288,618.15879213722,-37.7905011188881)) ;
#60492 = CARTESIAN_POINT('Ctrl Pts',(31.3842749784051,618.15616656847,-37.7568163467594)) ;
#60493 = CARTESIAN_POINT('Ctrl Pts',(31.4133330058182,618.151483323579,-37.6941046929351)) ;
#60494 = CARTESIAN_POINT('Ctrl Pts',(31.4257200000535,618.149408774511,-37.6652625159311)) ;
#60495 = CARTESIAN_POINT('Ctrl Pts',(31.4750099867373,618.140734675637,-37.5409181177682)) ;
#60496 = CARTESIAN_POINT('Ctrl Pts',(31.5038876224152,618.134517533878,-37.4424622096123)) ;
#60497 = CARTESIAN_POINT('Ctrl Pts',(31.5378980340447,618.123703999771,-37.2685833891882)) ;
#60498 = CARTESIAN_POINT('Ctrl Pts',(31.547294361471,618.119136678163,-37.1943201711079)) ;
#60499 = CARTESIAN_POINT('Ctrl Pts',(31.5552085104096,618.110652375872,-37.0593504951988)) ;
#60500 = CARTESIAN_POINT('Ctrl Pts',(31.5554604097298,618.106785992725,-36.998878804543)) ;
#60501 = CARTESIAN_POINT('Ctrl Pts',(31.549879823527,618.099476058329,-36.8878451430808)) ;
#60502 = CARTESIAN_POINT('Ctrl Pts',(31.5450178368784,618.09606831119,-36.8373065749465)) ;
#60503 = CARTESIAN_POINT('Ctrl Pts',(31.5183605802869,618.083108479532,-36.6502839179391)) ;
#60504 = CARTESIAN_POINT('Ctrl Pts',(31.4819251881433,618.073077486742,-36.5164757788996)) ;
#60505 = CARTESIAN_POINT('Ctrl Pts',(31.4085455969428,618.059038998112,-36.3379722042353)) ;
#60506 = CARTESIAN_POINT('Ctrl Pts',(31.3851831201593,618.055061839461,-36.2882726876611)) ;
#60507 = CARTESIAN_POINT('Ctrl Pts',(31.340654505117,618.048330936388,-36.2045548300127)) ;
#60508 = CARTESIAN_POINT('Ctrl Pts',(31.3206364270694,618.045541417183,-36.1699770867571)) ;
#60509 = CARTESIAN_POINT('Ctrl Pts',(31.2830349939648,618.040736876678,-36.1101013706384)) ;
#60510 = CARTESIAN_POINT('Ctrl Pts',(31.2659615111449,618.038696445318,-36.084515216137)) ;
#60511 = CARTESIAN_POINT('Ctrl Pts',(31.1983867054137,618.031087428169,-35.9890815479631)) ;
#60512 = CARTESIAN_POINT('Ctrl Pts',(31.1431987958555,618.025787189952,-35.9227119536607)) ;
#60513 = CARTESIAN_POINT('Ctrl Pts',(31.0241135103691,618.015339944938,-35.8002084646993)) ;
#60514 = CARTESIAN_POINT('Ctrl Pts',(30.9605738535416,618.010205023156,-35.7441001621896)) ;
#60515 = CARTESIAN_POINT('Ctrl Pts',(30.8418513938379,618.000913950436,-35.6543707141084)) ;
#60516 = CARTESIAN_POINT('Ctrl Pts',(30.7884684064382,617.996831089576,-35.6186719285698)) ;
#60517 = CARTESIAN_POINT('Ctrl Pts',(30.6898354743301,617.989336436594,-35.5606579933332)) ;
#60518 = CARTESIAN_POINT('Ctrl Pts',(30.6453799794246,617.985975435694,-35.5371495815042)) ;
#60519 = CARTESIAN_POINT('Ctrl Pts',(30.5273010973506,617.977054153712,-35.4813887995339)) ;
#60520 = CARTESIAN_POINT('Ctrl Pts',(30.4522940376825,617.97138790265,-35.4523920555794)) ;
#60521 = CARTESIAN_POINT('Ctrl Pts',(30.2838439518898,617.958708337387,-35.4009056120791)) ;
#60522 = CARTESIAN_POINT('Ctrl Pts',(30.1899471763949,617.951666351828,-35.3808537809)) ;
#60523 = CARTESIAN_POINT('Ctrl Pts',(30.0560091198578,617.941943615365,-35.3641378474514)) ;
#60524 = CARTESIAN_POINT('Ctrl Pts',(30.0170069283446,617.939152099863,-35.360660368693)) ;
#60525 = CARTESIAN_POINT('Ctrl Pts',(29.9454843796962,617.934144009723,-35.3568173353109)) ;
#60526 = CARTESIAN_POINT('Ctrl Pts',(29.9130044188139,617.931911667228,-35.3560232270462)) ;
#60527 = CARTESIAN_POINT('Ctrl Pts',(29.8446125751714,617.927326629971,-35.3563520635515)) ;
#60528 = CARTESIAN_POINT('Ctrl Pts',(29.8087191204132,617.924984799699,-35.3576853897329)) ;
#60529 = CARTESIAN_POINT('Ctrl Pts',(29.6116020615684,617.912341183982,-35.3714000279462)) ;
#60530 = CARTESIAN_POINT('Ctrl Pts',(29.4527894116313,617.902877757318,-35.4060408198108)) ;
#60531 = CARTESIAN_POINT('Ctrl Pts',(29.2434699455966,617.888871839149,-35.4848593017614)) ;
#60532 = CARTESIAN_POINT('Ctrl Pts',(29.1867661957619,617.884917842321,-35.5099026427465)) ;
#60533 = CARTESIAN_POINT('Ctrl Pts',(29.0866160899477,617.877537851914,-35.5609815355461)) ;
#60534 = CARTESIAN_POINT('Ctrl Pts',(29.0427101341918,617.874153834571,-35.5859509509979)) ;
#60535 = CARTESIAN_POINT('Ctrl Pts',(28.8724525947701,617.86037050265,-35.6932938257871)) ;
#60536 = CARTESIAN_POINT('Ctrl Pts',(28.7564275144876,617.849371175943,-35.7906471723882)) ;
#60537 = CARTESIAN_POINT('Ctrl Pts',(28.6217341314801,617.834818458955,-35.9389913871157)) ;
#60538 = CARTESIAN_POINT('Ctrl Pts',(28.5900205326611,617.831234689477,-35.9772198201013)) ;
#60539 = CARTESIAN_POINT('Ctrl Pts',(28.5373671982883,617.82506361963,-36.0467958201318)) ;
#60540 = CARTESIAN_POINT('Ctrl Pts',(28.5156939178457,617.82244737342,-36.0775447441099)) ;
#60541 = CARTESIAN_POINT('Ctrl Pts',(28.4777961269415,617.817763697418,-36.1353756591398)) ;
#60542 = CARTESIAN_POINT('Ctrl Pts',(28.4612660100266,617.815680211949,-36.162233108645)) ;
#60543 = CARTESIAN_POINT('Ctrl Pts',(28.3866327544997,617.805999203518,-36.2915813352369)) ;
#60544 = CARTESIAN_POINT('Ctrl Pts',(28.338738448464,617.798915398544,-36.3995889590225)) ;
#60545 = CARTESIAN_POINT('Ctrl Pts',(28.2820367281247,617.787596668335,-36.5757694074248)) ;
#60546 = CARTESIAN_POINT('Ctrl Pts',(28.265331217687,617.783458758455,-36.6409644953251)) ;
#60547 = CARTESIAN_POINT('Ctrl Pts',(28.2417727246344,617.775597861706,-36.763245465266)) ;
#60548 = CARTESIAN_POINT('Ctrl Pts',(28.2338443967964,617.771909955589,-36.8200198026846)) ;
#60549 = CARTESIAN_POINT('Ctrl Pts',(28.224353135804,617.764709795088,-36.9286005588733)) ;
#60550 = CARTESIAN_POINT('Ctrl Pts',(28.2222514882408,617.761219630867,-36.9802921882637)) ;
#60551 = CARTESIAN_POINT('Ctrl Pts',(28.2233603958254,617.748264883254,-37.1681689594493)) ;
#60552 = CARTESIAN_POINT('Ctrl Pts',(28.2408576916802,617.738349618598,-37.3037107583147)) ;
#60553 = CARTESIAN_POINT('Ctrl Pts',(28.2876994686318,617.724625479872,-37.4865690028681)) ;
#60554 = CARTESIAN_POINT('Ctrl Pts',(28.3031705176895,617.720816770115,-37.5369124109155)) ;
#60555 = CARTESIAN_POINT('Ctrl Pts',(28.3341957218464,617.714323906873,-37.6230978954343)) ;
#60556 = CARTESIAN_POINT('Ctrl Pts',(28.348674509093,617.711606926103,-37.6592840365282)) ;
#60557 = CARTESIAN_POINT('Ctrl Pts',(28.3769324541012,617.706857621446,-37.7233003641909)) ;
#60558 = CARTESIAN_POINT('Ctrl Pts',(28.3902440041931,617.704803511503,-37.7513129941224)) ;
#60559 = CARTESIAN_POINT('Ctrl Pts',(28.4537487116756,617.695719699661,-37.8758585683142)) ;
#60560 = CARTESIAN_POINT('Ctrl Pts',(28.5125486704521,617.689133728099,-37.9677182434717)) ;
#60561 = CARTESIAN_POINT('Ctrl Pts',(28.6246247468857,617.678075055629,-38.1099696175061)) ;
#60562 = CARTESIAN_POINT('Ctrl Pts',(28.6729992614358,617.673649685354,-38.1637685392274)) ;
#60563 = CARTESIAN_POINT('Ctrl Pts',(28.7672250576991,617.665370428635,-38.2557592545631)) ;
#60564 = CARTESIAN_POINT('Ctrl Pts',(28.8119242010044,617.661561811506,-38.2949562666162)) ;
#60565 = CARTESIAN_POINT('Ctrl Pts',(28.8982534605353,617.654329529728,-38.3628524801289)) ;
#60566 = CARTESIAN_POINT('Ctrl Pts',(28.939280250983,617.650938960327,-38.3922066114468)) ;
#60567 = CARTESIAN_POINT('Ctrl Pts',(29.0606903072189,617.64099843398,-38.4710003153332)) ;
#60568 = CARTESIAN_POINT('Ctrl Pts',(29.1440141330573,617.634275604268,-38.5155277819997)) ;
#60569 = CARTESIAN_POINT('Ctrl Pts',(29.3052302844579,617.621552783197,-38.5848217212131)) ;
#60570 = CARTESIAN_POINT('Ctrl Pts',(29.3820604664016,617.615602499589,-38.6113858330639)) ;
#60571 = CARTESIAN_POINT('Ctrl Pts',(29.508270477064,617.606226831418,-38.6449360530594)) ;
#60572 = CARTESIAN_POINT('Ctrl Pts',(29.5565657400658,617.602730967901,-38.6555001333034)) ;
#60573 = CARTESIAN_POINT('Ctrl Pts',(29.6344098776543,617.5973121353,-38.6689312362371)) ;
#60574 = CARTESIAN_POINT('Ctrl Pts',(29.6636824628802,617.595325881698,-38.6731827991571)) ;
#60575 = CARTESIAN_POINT('Ctrl Pts',(29.7465698481081,617.589837088992,-38.6829754234697)) ;
#60576 = CARTESIAN_POINT('Ctrl Pts',(29.8003615577277,617.586424048284,-38.6866983577146)) ;
#60577 = CARTESIAN_POINT('Ctrl Pts',(29.9642624515506,617.57622300459,-38.6900718178251)) ;
#60578 = CARTESIAN_POINT('Ctrl Pts',(30.0742358677732,617.569633292837,-38.6814308653686)) ;
#60579 = CARTESIAN_POINT('Ctrl Pts',(30.2533719695118,617.558366428119,-38.6493112177922)) ;
#60580 = CARTESIAN_POINT('Ctrl Pts',(30.3232813592806,617.553833519323,-38.6320418896756)) ;
#60581 = CARTESIAN_POINT('Ctrl Pts',(30.4161161524597,617.547494864546,-38.6026203312522)) ;
#60582 = CARTESIAN_POINT('Ctrl Pts',(30.4401981230646,617.545820985094,-38.5943761792912)) ;
#60583 = CARTESIAN_POINT('Ctrl Pts',(30.4640776716666,617.544128797339,-38.5855853040402)) ;
#60584 = CARTESIAN_POINT('Origin',(29.8885276254223,620.2564904411,-37.0221601717529)) ;
#60585 = CARTESIAN_POINT('Ctrl Pts',(31.5177255210653,618.256605597192,-35.7700771955364)) ;
#60586 = CARTESIAN_POINT('Ctrl Pts',(31.4358975948208,618.249786276961,-35.6636035130611)) ;
#60587 = CARTESIAN_POINT('Ctrl Pts',(31.3438305866016,618.243420671915,-35.5654073397872)) ;
#60588 = CARTESIAN_POINT('Ctrl Pts',(31.1659268453259,618.231906784935,-35.4094901911848)) ;
#60589 = CARTESIAN_POINT('Ctrl Pts',(31.0841098667658,618.226850009824,-35.3479339294522)) ;
#60590 = CARTESIAN_POINT('Ctrl Pts',(30.9541032131772,618.218854762731,-35.2645272696165)) ;
#60591 = CARTESIAN_POINT('Ctrl Pts',(30.9090927907251,618.21609514327,-35.2380158855215)) ;
#60592 = CARTESIAN_POINT('Ctrl Pts',(30.8154875863962,618.210345137083,-35.187583728142)) ;
#60593 = CARTESIAN_POINT('Ctrl Pts',(30.7668596171457,618.207352245656,-35.1638120824583)) ;
#60594 = CARTESIAN_POINT('Ctrl Pts',(30.5631220148783,618.194769322437,-35.0739995647562)) ;
#60595 = CARTESIAN_POINT('Ctrl Pts',(30.4011298183337,618.184593215762,-35.0252553221851)) ;
#60596 = CARTESIAN_POINT('Ctrl Pts',(30.1764578127107,618.170920420864,-34.9868158716723)) ;
#60597 = CARTESIAN_POINT('Ctrl Pts',(30.1174626865178,618.167378316383,-34.9793386835085)) ;
#60598 = CARTESIAN_POINT('Ctrl Pts',(30.0148354621986,618.16138019276,-34.9708339230574)) ;
#60599 = CARTESIAN_POINT('Ctrl Pts',(29.9713403548589,618.158888849364,-34.9686179490241)) ;
#60600 = CARTESIAN_POINT('Ctrl Pts',(29.8986584161905,618.154846009495,-34.9672283612392)) ;
#60601 = CARTESIAN_POINT('Ctrl Pts',(29.8695057571334,618.153258829605,-34.9672913864728)) ;
#60602 = CARTESIAN_POINT('Ctrl Pts',(29.7937955336326,618.149221228424,-34.9690667123986)) ;
#60603 = CARTESIAN_POINT('Ctrl Pts',(29.747279033869,618.146818877027,-34.971741582058)) ;
#60604 = CARTESIAN_POINT('Ctrl Pts',(29.5646466340215,618.137558997937,-34.9884893175988)) ;
#60605 = CARTESIAN_POINT('Ctrl Pts',(29.4299833001195,618.131089343044,-35.0145600535208)) ;
#60606 = CARTESIAN_POINT('Ctrl Pts',(29.2069408376618,618.119725902436,-35.0813734454084)) ;
#60607 = CARTESIAN_POINT('Ctrl Pts',(29.1170285565647,618.114956535324,-35.1153302566464)) ;
#60608 = CARTESIAN_POINT('Ctrl Pts',(28.9827665072291,618.107293831612,-35.1770917490866)) ;
#60609 = CARTESIAN_POINT('Ctrl Pts',(28.9365464882667,618.1045520558,-35.2005092851128)) ;
#60610 = CARTESIAN_POINT('Ctrl Pts',(28.8434668763486,618.098786513679,-35.252178809114)) ;
#60611 = CARTESIAN_POINT('Ctrl Pts',(28.7967522536233,618.095757797261,-35.2806057745684)) ;
#60612 = CARTESIAN_POINT('Ctrl Pts',(28.6159992991661,618.08347149598,-35.4007307871783)) ;
#60613 = CARTESIAN_POINT('Ctrl Pts',(28.4919153680927,618.073683245127,-35.5063038391899)) ;
#60614 = CARTESIAN_POINT('Ctrl Pts',(28.3213146111363,618.058617679057,-35.6903578754549)) ;
#60615 = CARTESIAN_POINT('Ctrl Pts',(28.2653241296603,618.05333994272,-35.7592005477882)) ;
#60616 = CARTESIAN_POINT('Ctrl Pts',(28.1952477771545,618.046463800495,-35.8577536017175)) ;
#60617 = CARTESIAN_POINT('Ctrl Pts',(28.1771649606245,618.044661272511,-35.8844970129365)) ;
#60618 = CARTESIAN_POINT('Ctrl Pts',(28.1418160754024,618.041096823548,-35.939527475035)) ;
#60619 = CARTESIAN_POINT('Ctrl Pts',(28.1245891198471,618.039337256018,-35.9678281433063)) ;
#60620 = CARTESIAN_POINT('Ctrl Pts',(28.0406662650907,618.030582618844,-36.1135173168416)) ;
#60621 = CARTESIAN_POINT('Ctrl Pts',(27.9849650321949,618.024133348046,-36.2368697454498)) ;
#60622 = CARTESIAN_POINT('Ctrl Pts',(27.915405734525,618.013602410858,-36.4428706121116)) ;
#60623 = CARTESIAN_POINT('Ctrl Pts',(27.8937665689741,618.009590964145,-36.5224465309044)) ;
#60624 = CARTESIAN_POINT('Ctrl Pts',(27.8635604156702,618.002160791058,-36.6674425830066)) ;
#60625 = CARTESIAN_POINT('Ctrl Pts',(27.8532525194182,617.998791543164,-36.732382878791)) ;
#60626 = CARTESIAN_POINT('Ctrl Pts',(27.8406308303826,617.992692065399,-36.847233566189)) ;
#60627 = CARTESIAN_POINT('Ctrl Pts',(27.8369914157998,617.99000672271,-36.8969436513977)) ;
#60628 = CARTESIAN_POINT('Ctrl Pts',(27.8327554744115,617.98365306082,-37.0122609985426)) ;
#60629 = CARTESIAN_POINT('Ctrl Pts',(27.8334866667382,617.97994521523,-37.0778595938705)) ;
#60630 = CARTESIAN_POINT('Ctrl Pts',(27.8460559423183,617.967614698141,-37.2906753371488)) ;
#60631 = CARTESIAN_POINT('Ctrl Pts',(27.8706162737434,617.958649045103,-37.4366674794061)) ;
#60632 = CARTESIAN_POINT('Ctrl Pts',(27.9309603652972,617.945331043468,-37.651111086265)) ;
#60633 = CARTESIAN_POINT('Ctrl Pts',(27.9552813842903,617.940892200627,-37.7223099487288)) ;
#60634 = CARTESIAN_POINT('Ctrl Pts',(27.9952319771609,617.934847575687,-37.8211705799566)) ;
#60635 = CARTESIAN_POINT('Ctrl Pts',(28.0076803922372,617.933097230471,-37.8500491306183)) ;
#60636 = CARTESIAN_POINT('Ctrl Pts',(28.0350613669596,617.92952734202,-37.9097597191898)) ;
#60637 = CARTESIAN_POINT('Ctrl Pts',(28.0501114284404,617.92771457136,-37.9405262861034)) ;
#60638 = CARTESIAN_POINT('Ctrl Pts',(28.1320656161547,617.918505662467,-38.097965968923)) ;
#60639 = CARTESIAN_POINT('Ctrl Pts',(28.2113196451691,617.911707233053,-38.2177768922417)) ;
#60640 = CARTESIAN_POINT('Ctrl Pts',(28.3513203719568,617.901020474753,-38.3877783254848)) ;
#60641 = CARTESIAN_POINT('Ctrl Pts',(28.4035349621028,617.897254965393,-38.4443819938088)) ;
#60642 = CARTESIAN_POINT('Ctrl Pts',(28.5042370854527,617.890193705942,-38.5419429858827)) ;
#60643 = CARTESIAN_POINT('Ctrl Pts',(28.5516810214853,617.886937925585,-38.5838388270995)) ;
#60644 = CARTESIAN_POINT('Ctrl Pts',(28.6398428414635,617.880949627062,-38.6547258645091)) ;
#60645 = CARTESIAN_POINT('Ctrl Pts',(28.6798286065754,617.878254620663,-38.6845471616879)) ;
#60646 = CARTESIAN_POINT('Ctrl Pts',(28.7771038448506,617.871727751243,-38.7517287382187)) ;
#60647 = CARTESIAN_POINT('Ctrl Pts',(28.8352485933516,617.867848073146,-38.7877399621918)) ;
#60648 = CARTESIAN_POINT('Ctrl Pts',(29.0256835504104,617.855216377419,-38.8929248440873)) ;
#60649 = CARTESIAN_POINT('Ctrl Pts',(29.1637549042228,617.84613100121,-38.9506199250456)) ;
#60650 = CARTESIAN_POINT('Ctrl Pts',(29.373239653949,617.83310852921,-39.0124541009729)) ;
#60651 = CARTESIAN_POINT('Ctrl Pts',(29.4406005402208,617.829037462199,-39.0286881568952)) ;
#60652 = CARTESIAN_POINT('Ctrl Pts',(29.5390805754258,617.823367767415,-39.0472139081433)) ;
#60653 = CARTESIAN_POINT('Ctrl Pts',(29.5696320867122,617.821647890139,-39.0522493161275)) ;
#60654 = CARTESIAN_POINT('Ctrl Pts',(29.6349849706317,617.818067302193,-39.0615085068973)) ;
#60655 = CARTESIAN_POINT('Ctrl Pts',(29.6698029308128,617.816216386936,-39.0655361382003)) ;
#60656 = CARTESIAN_POINT('Ctrl Pts',(29.841214681719,617.807308357833,-39.0809324168315)) ;
#60657 = CARTESIAN_POINT('Ctrl Pts',(29.9786188482924,617.800784336763,-39.0795063047954)) ;
#60658 = CARTESIAN_POINT('Ctrl Pts',(30.1933287323379,617.790310328148,-39.0557101414683)) ;
#60659 = CARTESIAN_POINT('Ctrl Pts',(30.2712194056519,617.786454970081,-39.0425005435805)) ;
#60660 = CARTESIAN_POINT('Ctrl Pts',(30.4107047848824,617.779258388538,-39.0104879362867)) ;
#60661 = CARTESIAN_POINT('Ctrl Pts',(30.4725440640204,617.775960531024,-38.9932106564754)) ;
#60662 = CARTESIAN_POINT('Ctrl Pts',(30.5807903085818,617.769931969393,-38.9574260083721)) ;
#60663 = CARTESIAN_POINT('Ctrl Pts',(30.6275224364838,617.7672415241,-38.9400672455821)) ;
#60664 = CARTESIAN_POINT('Ctrl Pts',(30.7356896889251,617.760786251495,-38.8953477587663)) ;
#60665 = CARTESIAN_POINT('Ctrl Pts',(30.7965014227713,617.756977011846,-38.8666377186207)) ;
#60666 = CARTESIAN_POINT('Ctrl Pts',(30.985519277444,617.744556563513,-38.7657848103514)) ;
#60667 = CARTESIAN_POINT('Ctrl Pts',(31.1074334120279,617.735617258806,-38.6828462819815)) ;
#60668 = CARTESIAN_POINT('Ctrl Pts',(31.2748917162738,617.722490179842,-38.5404783517974)) ;
#60669 = CARTESIAN_POINT('Ctrl Pts',(31.3278069179047,617.718199385269,-38.4904150521286)) ;
#60670 = CARTESIAN_POINT('Ctrl Pts',(31.3994862933326,617.712305016767,-38.4149911634673)) ;
#60671 = CARTESIAN_POINT('Ctrl Pts',(31.4204979899222,617.710566447073,-38.3918468073721)) ;
#60672 = CARTESIAN_POINT('Ctrl Pts',(31.463600068895,617.706993217141,-38.3421363360367)) ;
#60673 = CARTESIAN_POINT('Ctrl Pts',(31.4855644910323,617.705166446979,-38.3154752292432)) ;
#60674 = CARTESIAN_POINT('Ctrl Pts',(31.5937264732664,617.696067076666,-38.1772245693299)) ;
#60675 = CARTESIAN_POINT('Ctrl Pts',(31.6689541465479,617.689368066327,-38.0575185047584)) ;
#60676 = CARTESIAN_POINT('Ctrl Pts',(31.7800214613876,617.677186996813,-37.8323232483487)) ;
#60677 = CARTESIAN_POINT('Ctrl Pts',(31.8206949480617,617.671782433778,-37.7298603194332)) ;
#60678 = CARTESIAN_POINT('Ctrl Pts',(31.868547838031,617.66336608807,-37.5738320623766)) ;
#60679 = CARTESIAN_POINT('Ctrl Pts',(31.8821524409297,617.660567822003,-37.5224414165118)) ;
#60680 = CARTESIAN_POINT('Ctrl Pts',(31.9053145869008,617.654846192592,-37.4188670259445)) ;
#60681 = CARTESIAN_POINT('Ctrl Pts',(31.9148740395048,617.65192538401,-37.3667257612899)) ;
#60682 = CARTESIAN_POINT('Ctrl Pts',(31.9394633157647,617.642186555127,-37.1955212758493)) ;
#60683 = CARTESIAN_POINT('Ctrl Pts',(31.9460838023301,617.635111722276,-37.0755161923445)) ;
#60684 = CARTESIAN_POINT('Ctrl Pts',(31.9378084543984,617.619782006461,-36.8200534179514)) ;
#60685 = CARTESIAN_POINT('Ctrl Pts',(31.9200009801735,617.611529753312,-36.6852345299975)) ;
#60686 = CARTESIAN_POINT('Ctrl Pts',(31.8814869554307,617.60191314656,-36.520957650826)) ;
#60687 = CARTESIAN_POINT('Ctrl Pts',(31.8731631764905,617.600062235772,-36.4889501979671)) ;
#60688 = CARTESIAN_POINT('Ctrl Pts',(31.8551799581335,617.596490641857,-36.4260717544974)) ;
#60689 = CARTESIAN_POINT('Ctrl Pts',(31.845557137723,617.594768955087,-36.3952004401708)) ;
#60690 = CARTESIAN_POINT('Ctrl Pts',(31.8064878533971,617.588395574146,-36.2795430377554)) ;
#60691 = CARTESIAN_POINT('Ctrl Pts',(31.7722239974252,617.583973963416,-36.19648308121)) ;
#60692 = CARTESIAN_POINT('Ctrl Pts',(31.6725973313151,617.572986535961,-35.993752053494)) ;
#60693 = CARTESIAN_POINT('Ctrl Pts',(31.6005982485012,617.566503602382,-35.8779103629146)) ;
#60694 = CARTESIAN_POINT('Ctrl Pts',(31.5177255210691,617.559653386529,-35.7700771955414)) ;
#60695 = CARTESIAN_POINT('Ctrl Pts',(31.5177255210752,617.617782467769,-35.7700771955494)) ;
#60696 = CARTESIAN_POINT('Ctrl Pts',(31.5180340350894,617.61780717866,-35.7704786309113)) ;
#60697 = CARTESIAN_POINT('Ctrl Pts',(31.5183424025187,617.6178318871,-35.7708801826247)) ;
#60698 = CARTESIAN_POINT('Ctrl Pts',(31.6277791123126,617.626603994928,-35.913496210444)) ;
#60699 = CARTESIAN_POINT('Ctrl Pts',(31.7178211712387,617.635075826489,-36.0693669297009)) ;
#60700 = CARTESIAN_POINT('Ctrl Pts',(31.8064719691583,617.64704221832,-36.2831031261027)) ;
#60701 = CARTESIAN_POINT('Ctrl Pts',(31.824605112006,617.64979460496,-36.3320013986807)) ;
#60702 = CARTESIAN_POINT('Ctrl Pts',(31.8575018699649,617.655494926049,-36.4322553547147)) ;
#60703 = CARTESIAN_POINT('Ctrl Pts',(31.8721612338588,617.658443792538,-36.4836026361227)) ;
#60704 = CARTESIAN_POINT('Ctrl Pts',(31.9136213921269,617.668321364748,-36.6536576592669)) ;
#60705 = CARTESIAN_POINT('Ctrl Pts',(31.9318804715396,617.67551337769,-36.7741664863849)) ;
#60706 = CARTESIAN_POINT('Ctrl Pts',(31.9473606350084,617.690595886966,-37.0249490179732)) ;
#60707 = CARTESIAN_POINT('Ctrl Pts',(31.9430861333298,617.698466249787,-37.1548032883533)) ;
#60708 = CARTESIAN_POINT('Ctrl Pts',(31.9223487291596,617.707777324383,-37.3165908073956)) ;
#60709 = CARTESIAN_POINT('Ctrl Pts',(31.9172829720951,617.709653944115,-37.3496807373195)) ;
#60710 = CARTESIAN_POINT('Ctrl Pts',(31.9058656688665,617.713213906091,-37.4137515633074)) ;
#60711 = CARTESIAN_POINT('Ctrl Pts',(31.8996031592225,617.714900683671,-37.4447379100561)) ;
#60712 = CARTESIAN_POINT('Ctrl Pts',(31.8751872213228,617.720690602479,-37.5526582438874)) ;
#60713 = CARTESIAN_POINT('Ctrl Pts',(31.8533112900984,617.724618758108,-37.6286846519606)) ;
#60714 = CARTESIAN_POINT('Ctrl Pts',(31.7659917248468,617.737495969088,-37.8772151824743)) ;
#60715 = CARTESIAN_POINT('Ctrl Pts',(31.6817493213936,617.74618521428,-38.0421334800298)) ;
#60716 = CARTESIAN_POINT('Ctrl Pts',(31.5470254037552,617.758416264534,-38.2362773444608)) ;
#60717 = CARTESIAN_POINT('Ctrl Pts',(31.5158079386885,617.761160536737,-38.2778088173608)) ;
#60718 = CARTESIAN_POINT('Ctrl Pts',(31.4492087337778,617.766869307908,-38.3597518160478)) ;
#60719 = CARTESIAN_POINT('Ctrl Pts',(31.4137494187332,617.769835906617,-38.4000479180391)) ;
#60720 = CARTESIAN_POINT('Ctrl Pts',(31.3304755612378,617.776657183452,-38.4875232888393)) ;
#60721 = CARTESIAN_POINT('Ctrl Pts',(31.2818445737556,617.780544443793,-38.5338378737254)) ;
#60722 = CARTESIAN_POINT('Ctrl Pts',(31.1286329000272,617.792476275938,-38.6660685062465)) ;
#60723 = CARTESIAN_POINT('Ctrl Pts',(31.0177580551296,617.800726936988,-38.7441158107718)) ;
#60724 = CARTESIAN_POINT('Ctrl Pts',(30.8483644354746,617.812257679575,-38.839915099798)) ;
#60725 = CARTESIAN_POINT('Ctrl Pts',(30.7954600204953,617.815718687625,-38.8668808714581)) ;
#60726 = CARTESIAN_POINT('Ctrl Pts',(30.7142323980204,617.820748628273,-38.9039425083672)) ;
#60727 = CARTESIAN_POINT('Ctrl Pts',(30.6867359131042,617.822403573995,-38.9157697089775)) ;
#60728 = CARTESIAN_POINT('Ctrl Pts',(30.6249935488472,617.826002520568,-38.9407430068953)) ;
#60729 = CARTESIAN_POINT('Ctrl Pts',(30.5906360310009,617.827930192851,-38.9535809690912)) ;
#60730 = CARTESIAN_POINT('Ctrl Pts',(30.5128330442322,617.832167248719,-38.9803018334237)) ;
#60731 = CARTESIAN_POINT('Ctrl Pts',(30.4692317208715,617.834454358745,-38.993672082564)) ;
#60732 = CARTESIAN_POINT('Ctrl Pts',(30.3089052561877,617.842664824357,-39.0370546611192)) ;
#60733 = CARTESIAN_POINT('Ctrl Pts',(30.1900458390625,617.848385983677,-39.0582362199247)) ;
#60734 = CARTESIAN_POINT('Ctrl Pts',(29.9812567813018,617.858654048457,-39.0767497507778)) ;
#60735 = CARTESIAN_POINT('Ctrl Pts',(29.8920914668346,617.863104435427,-39.0788376245131)) ;
#60736 = CARTESIAN_POINT('Ctrl Pts',(29.7520591887535,617.870387400234,-39.0730090851948)) ;
#60737 = CARTESIAN_POINT('Ctrl Pts',(29.7011416541196,617.87309574215,-39.0689847297956)) ;
#60738 = CARTESIAN_POINT('Ctrl Pts',(29.5957084870295,617.87885413864,-39.0566846056944)) ;
#60739 = CARTESIAN_POINT('Ctrl Pts',(29.5412704864294,617.881912031968,-39.0481030063165)) ;
#60740 = CARTESIAN_POINT('Ctrl Pts',(29.3727972044363,617.891654219457,-39.0145551405766)) ;
#60741 = CARTESIAN_POINT('Ctrl Pts',(29.2605111867686,617.898565782613,-38.9820593640228)) ;
#60742 = CARTESIAN_POINT('Ctrl Pts',(29.0327082543802,617.913217783146,-38.8945365403378)) ;
#60743 = CARTESIAN_POINT('Ctrl Pts',(28.9183125322229,617.920944464703,-38.8378987004513)) ;
#60744 = CARTESIAN_POINT('Ctrl Pts',(28.7812622343372,617.930140187678,-38.7533714455176)) ;
#60745 = CARTESIAN_POINT('Ctrl Pts',(28.7530672089189,617.932027196406,-38.7350113220697)) ;
#60746 = CARTESIAN_POINT('Ctrl Pts',(28.6993872913163,617.935590656082,-38.6981475093762)) ;
#60747 = CARTESIAN_POINT('Ctrl Pts',(28.6738526812261,617.937271193357,-38.6797346655057)) ;
#60748 = CARTESIAN_POINT('Ctrl Pts',(28.5871926029027,617.942960327631,-38.6141662490702)) ;
#60749 = CARTESIAN_POINT('Ctrl Pts',(28.5283026621049,617.946802630882,-38.5641544513786)) ;
#60750 = CARTESIAN_POINT('Ctrl Pts',(28.3651729182075,617.957819087282,-38.4089816282746)) ;
#60751 = CARTESIAN_POINT('Ctrl Pts',(28.2693112317538,617.964818442891,-38.2957463715584)) ;
#60752 = CARTESIAN_POINT('Ctrl Pts',(28.1504925531068,617.975480884393,-38.120044093854)) ;
#60753 = CARTESIAN_POINT('Ctrl Pts',(28.1170593858906,617.978776929684,-38.0652393763678)) ;
#60754 = CARTESIAN_POINT('Ctrl Pts',(28.0624492446223,617.984787255473,-37.9655003438917)) ;
#60755 = CARTESIAN_POINT('Ctrl Pts',(28.0402334305266,617.987460715738,-37.9211934899408)) ;
#60756 = CARTESIAN_POINT('Ctrl Pts',(27.9921124174203,617.993842119472,-37.8158821245273)) ;
#60757 = CARTESIAN_POINT('Ctrl Pts',(27.9675148339435,617.997592184172,-37.7543443252872)) ;
#60758 = CARTESIAN_POINT('Ctrl Pts',(27.9186100081024,618.006282466616,-37.6124590119968)) ;
#60759 = CARTESIAN_POINT('Ctrl Pts',(27.8961665822768,618.011267532517,-37.5315948613946)) ;
#60760 = CARTESIAN_POINT('Ctrl Pts',(27.8515192470603,618.024146599155,-37.3216612272472)) ;
#60761 = CARTESIAN_POINT('Ctrl Pts',(27.8365872739035,618.032089078202,-37.1914189904872)) ;
#60762 = CARTESIAN_POINT('Ctrl Pts',(27.8335127814323,618.041457646263,-37.027258609981)) ;
#60763 = CARTESIAN_POINT('Ctrl Pts',(27.8337011390787,618.043328702714,-36.9938686816973)) ;
#60764 = CARTESIAN_POINT('Ctrl Pts',(27.8356557756322,618.046890095625,-36.928766286273)) ;
#60765 = CARTESIAN_POINT('Ctrl Pts',(27.8373436346707,618.048583372588,-36.8970616310105)) ;
#60766 = CARTESIAN_POINT('Ctrl Pts',(27.8459430115139,618.054479068767,-36.7846674820529)) ;
#60767 = CARTESIAN_POINT('Ctrl Pts',(27.8568885788465,618.058497213992,-36.704355455598)) ;
#60768 = CARTESIAN_POINT('Ctrl Pts',(27.9071682153037,618.071198047,-36.4492054111199)) ;
#60769 = CARTESIAN_POINT('Ctrl Pts',(27.9646014670271,618.079654419607,-36.2788102552533)) ;
#60770 = CARTESIAN_POINT('Ctrl Pts',(28.066479086708,618.091612202793,-36.0709035896473)) ;
#60771 = CARTESIAN_POINT('Ctrl Pts',(28.0913585827081,618.094378294162,-36.024697025177)) ;
#60772 = CARTESIAN_POINT('Ctrl Pts',(28.1448566010235,618.100067665725,-35.9338519664303)) ;
#60773 = CARTESIAN_POINT('Ctrl Pts',(28.1734887009863,618.102990056983,-35.8892682357778)) ;
#60774 = CARTESIAN_POINT('Ctrl Pts',(28.2719351544637,618.112681648458,-35.7482734849555)) ;
#60775 = CARTESIAN_POINT('Ctrl Pts',(28.3483991152899,618.11970177772,-35.6568192324954)) ;
#60776 = CARTESIAN_POINT('Ctrl Pts',(28.5280465940214,618.134976739336,-35.4763616215468)) ;
#60777 = CARTESIAN_POINT('Ctrl Pts',(28.6330486402326,618.143231348471,-35.3899291418472)) ;
#60778 = CARTESIAN_POINT('Ctrl Pts',(28.7731860236744,618.152843600943,-35.2961544183743)) ;
#60779 = CARTESIAN_POINT('Ctrl Pts',(28.8010024513293,618.154688161838,-35.2784939105625)) ;
#60780 = CARTESIAN_POINT('Ctrl Pts',(28.856567681903,618.158231014209,-35.2450631377593)) ;
#60781 = CARTESIAN_POINT('Ctrl Pts',(28.8842826298613,618.159930958142,-35.2292554409532)) ;
#60782 = CARTESIAN_POINT('Ctrl Pts',(28.9865275629576,618.166002003966,-35.1740534260238)) ;
#60783 = CARTESIAN_POINT('Ctrl Pts',(29.0631005461686,618.170171579565,-35.138606241793)) ;
#60784 = CARTESIAN_POINT('Ctrl Pts',(29.3058957098525,618.182873570332,-35.0438718466805)) ;
#60785 = CARTESIAN_POINT('Ctrl Pts',(29.4777021296833,618.191215298445,-35.0011938116259)) ;
#60786 = CARTESIAN_POINT('Ctrl Pts',(29.7045357200796,618.203016184373,-34.9750031743947)) ;
#60787 = CARTESIAN_POINT('Ctrl Pts',(29.7564278281711,618.205761213353,-34.9710010402733)) ;
#60788 = CARTESIAN_POINT('Ctrl Pts',(29.861217999348,618.211423558823,-34.9669121681846)) ;
#60789 = CARTESIAN_POINT('Ctrl Pts',(29.9140788300582,618.214340776853,-34.9668897348822)) ;
#60790 = CARTESIAN_POINT('Ctrl Pts',(30.0862446390824,618.224056975366,-34.9734594725751)) ;
#60791 = CARTESIAN_POINT('Ctrl Pts',(30.204970376356,618.231110943419,-34.9884139630212)) ;
#60792 = CARTESIAN_POINT('Ctrl Pts',(30.454214332906,618.246422379792,-35.0421677326057)) ;
#60793 = CARTESIAN_POINT('Ctrl Pts',(30.5835714136637,618.254678187611,-35.0837872724778)) ;
#60794 = CARTESIAN_POINT('Ctrl Pts',(30.7380873653048,618.26429119596,-35.1509760529953)) ;
#60795 = CARTESIAN_POINT('Ctrl Pts',(30.7679653662581,618.266136373358,-35.1648310929445)) ;
#60796 = CARTESIAN_POINT('Ctrl Pts',(30.8264487915323,618.269701792271,-35.1936789898314)) ;
#60797 = CARTESIAN_POINT('Ctrl Pts',(30.8550595855715,618.271423278598,-35.2086398987449)) ;
#60798 = CARTESIAN_POINT('Ctrl Pts',(30.9597720477065,618.277681566113,-35.2665777293345)) ;
#60799 = CARTESIAN_POINT('Ctrl Pts',(31.0334669062337,618.282003747505,-35.3137248703129)) ;
#60800 = CARTESIAN_POINT('Ctrl Pts',(31.2188041883793,618.293222620977,-35.4496919881979)) ;
#60801 = CARTESIAN_POINT('Ctrl Pts',(31.3245872744644,618.300020038451,-35.5456699319762)) ;
#60802 = CARTESIAN_POINT('Ctrl Pts',(31.453785607836,618.30983286356,-35.6900213807411)) ;
#60803 = CARTESIAN_POINT('Ctrl Pts',(31.4865351379034,618.31247668497,-35.7294894016799)) ;
#60804 = CARTESIAN_POINT('Ctrl Pts',(31.5177728528538,618.315179696467,-35.7701387855975)) ;
#60805 = CARTESIAN_POINT('Origin',(179.888527625422,620.256490441073,-37.0221601717597)) ;
#60806 = CARTESIAN_POINT('Ctrl Pts',(181.517739089186,618.256600448668,-35.7700948504444)) ;
#60807 = CARTESIAN_POINT('Ctrl Pts',(181.437873718606,618.249944347976,-35.6661724950447)) ;
#60808 = CARTESIAN_POINT('Ctrl Pts',(181.348249767962,618.243721061608,-35.570129746345)) ;
#60809 = CARTESIAN_POINT('Ctrl Pts',(181.195083460485,618.233775904554,-35.4346147506586)) ;
#60810 = CARTESIAN_POINT('Ctrl Pts',(181.137527457287,618.230168969855,-35.3889464336022)) ;
#60811 = CARTESIAN_POINT('Ctrl Pts',(181.02740908538,618.223347923362,-35.3108032938592)) ;
#60812 = CARTESIAN_POINT('Ctrl Pts',(180.975590249206,618.220167953579,-35.2774288967524)) ;
#60813 = CARTESIAN_POINT('Ctrl Pts',(180.879136016606,618.214246816729,-35.2212733318131)) ;
#60814 = CARTESIAN_POINT('Ctrl Pts',(180.835017433914,618.211538046367,-35.1977000263673)) ;
#60815 = CARTESIAN_POINT('Ctrl Pts',(180.726321802718,618.204844827544,-35.1446262477408)) ;
#60816 = CARTESIAN_POINT('Ctrl Pts',(180.660994372857,618.200804800214,-35.1168186941649)) ;
#60817 = CARTESIAN_POINT('Ctrl Pts',(180.458058867961,618.188217198479,-35.0425903292061)) ;
#60818 = CARTESIAN_POINT('Ctrl Pts',(180.316859792524,618.179377619175,-35.0073183715969)) ;
#60819 = CARTESIAN_POINT('Ctrl Pts',(180.105276350539,618.166643278124,-34.9777253772246)) ;
#60820 = CARTESIAN_POINT('Ctrl Pts',(180.036970588114,618.162615853314,-34.9716334337022)) ;
#60821 = CARTESIAN_POINT('Ctrl Pts',(179.937609290037,618.156990888051,-34.9677641076903)) ;
#60822 = CARTESIAN_POINT('Ctrl Pts',(179.906709234979,618.155274718387,-34.9672582147298)) ;
#60823 = CARTESIAN_POINT('Ctrl Pts',(179.840630094085,618.151690790556,-34.9676673477673)) ;
#60824 = CARTESIAN_POINT('Ctrl Pts',(179.805463482461,618.149833283473,-34.9687884054165)) ;
#60825 = CARTESIAN_POINT('Ctrl Pts',(179.634630225367,618.140978746619,-34.9786308331627)) ;
#60826 = CARTESIAN_POINT('Ctrl Pts',(179.500016396077,618.134503612775,-34.9998983833042)) ;
#60827 = CARTESIAN_POINT('Ctrl Pts',(179.257342681304,618.122341237677,-35.0633850829905)) ;
#60828 = CARTESIAN_POINT('Ctrl Pts',(179.148847608016,618.11670887439,-35.1017267899532)) ;
#60829 = CARTESIAN_POINT('Ctrl Pts',(178.995979528623,618.108050729845,-35.1706350433054)) ;
#60830 = CARTESIAN_POINT('Ctrl Pts',(178.948684856959,618.105266263961,-35.1941879897356)) ;
#60831 = CARTESIAN_POINT('Ctrl Pts',(178.855566939141,618.099538155132,-35.2451306830427)) ;
#60832 = CARTESIAN_POINT('Ctrl Pts',(178.809798989781,618.096595426967,-35.2725358238972)) ;
#60833 = CARTESIAN_POINT('Ctrl Pts',(178.660690677841,618.086556154298,-35.3698955778976)) ;
#60834 = CARTESIAN_POINT('Ctrl Pts',(178.562672736491,618.079177333738,-35.4474656185981)) ;
#60835 = CARTESIAN_POINT('Ctrl Pts',(178.39206117652,618.065036370574,-35.6097678900672)) ;
#60836 = CARTESIAN_POINT('Ctrl Pts',(178.318117621821,618.058326716948,-35.6924691697643)) ;
#60837 = CARTESIAN_POINT('Ctrl Pts',(178.226263122883,618.049502861199,-35.8136165960414)) ;
#60838 = CARTESIAN_POINT('Ctrl Pts',(178.202322847058,618.047149847546,-35.8472496264347)) ;
#60839 = CARTESIAN_POINT('Ctrl Pts',(178.163153824184,618.043236621683,-35.9059431292964)) ;
#60840 = CARTESIAN_POINT('Ctrl Pts',(178.147421604658,618.041647703269,-35.9306450870052)) ;
#60841 = CARTESIAN_POINT('Ctrl Pts',(178.106421886834,618.037449095999,-35.9981644481978)) ;
#60842 = CARTESIAN_POINT('Ctrl Pts',(178.082171713741,618.034897738397,-36.0415750563872)) ;
#60843 = CARTESIAN_POINT('Ctrl Pts',(177.996868291576,618.025492041655,-36.2082043311838)) ;
#60844 = CARTESIAN_POINT('Ctrl Pts',(177.94665568358,618.018997394029,-36.3365676894766)) ;
#60845 = CARTESIAN_POINT('Ctrl Pts',(177.884915100193,618.007779020365,-36.5574362968693)) ;
#60846 = CARTESIAN_POINT('Ctrl Pts',(177.866150899087,618.003201296153,-36.6474316265925)) ;
#60847 = CARTESIAN_POINT('Ctrl Pts',(177.846352136007,617.995757740068,-36.7894110523277)) ;
#60848 = CARTESIAN_POINT('Ctrl Pts',(177.841158103839,617.993026342084,-36.8406931434261)) ;
#60849 = CARTESIAN_POINT('Ctrl Pts',(177.834399433318,617.987235725424,-36.9472666228647)) ;
#60850 = CARTESIAN_POINT('Ctrl Pts',(177.833128477895,617.984169388746,-37.0025341873973)) ;
#60851 = CARTESIAN_POINT('Ctrl Pts',(177.836799212377,617.972164379123,-37.2142370524895)) ;
#60852 = CARTESIAN_POINT('Ctrl Pts',(177.85737511703,617.962745757134,-37.3698509347612)) ;
#60853 = CARTESIAN_POINT('Ctrl Pts',(177.910842681946,617.949534056878,-37.5832279587215)) ;
#60854 = CARTESIAN_POINT('Ctrl Pts',(177.92913802079,617.945736579996,-37.6441150812566)) ;
#60855 = CARTESIAN_POINT('Ctrl Pts',(177.965278909125,617.939377232603,-37.7468457875381)) ;
#60856 = CARTESIAN_POINT('Ctrl Pts',(177.981745267152,617.936774790996,-37.7891259613203)) ;
#60857 = CARTESIAN_POINT('Ctrl Pts',(178.011067588354,617.932623106229,-37.8576184659271)) ;
#60858 = CARTESIAN_POINT('Ctrl Pts',(178.023104254186,617.93103262878,-37.8841593730473)) ;
#60859 = CARTESIAN_POINT('Ctrl Pts',(178.055016794302,617.927088698896,-37.9507243446462)) ;
#60860 = CARTESIAN_POINT('Ctrl Pts',(178.075640008708,617.924777153273,-37.9903711277945)) ;
#60861 = CARTESIAN_POINT('Ctrl Pts',(178.164190357098,617.915626338094,-38.1478367251896)) ;
#60862 = CARTESIAN_POINT('Ctrl Pts',(178.242444116224,617.909190339745,-38.259456095989)) ;
#60863 = CARTESIAN_POINT('Ctrl Pts',(178.395878966116,617.897729245373,-38.43773123747)) ;
#60864 = CARTESIAN_POINT('Ctrl Pts',(178.465957254829,617.89281231411,-38.5081387441332)) ;
#60865 = CARTESIAN_POINT('Ctrl Pts',(178.580118574358,617.884978478061,-38.6073323098885)) ;
#60866 = CARTESIAN_POINT('Ctrl Pts',(178.620675195722,617.882226948479,-38.6399532712892)) ;
#60867 = CARTESIAN_POINT('Ctrl Pts',(178.706046920997,617.876470022482,-38.7034371289031)) ;
#60868 = CARTESIAN_POINT('Ctrl Pts',(178.75093685773,617.873461018884,-38.7341295842102)) ;
#60869 = CARTESIAN_POINT('Ctrl Pts',(178.937250291898,617.861023947727,-38.8509513511697)) ;
#60870 = CARTESIAN_POINT('Ctrl Pts',(179.087610563969,617.85103698966,-38.9216130500305)) ;
#60871 = CARTESIAN_POINT('Ctrl Pts',(179.327263755383,617.83589498556,-39.000675757637)) ;
#60872 = CARTESIAN_POINT('Ctrl Pts',(179.411394071568,617.830729134247,-39.0226319020823)) ;
#60873 = CARTESIAN_POINT('Ctrl Pts',(179.528275146704,617.82396131699,-39.0453389732761)) ;
#60874 = CARTESIAN_POINT('Ctrl Pts',(179.56002534863,617.822163787926,-39.0507362494448)) ;
#60875 = CARTESIAN_POINT('Ctrl Pts',(179.62480548891,617.81859728985,-39.0601872975185)) ;
#60876 = CARTESIAN_POINT('Ctrl Pts',(179.657833049303,617.816831163087,-39.064189610487)) ;
#60877 = CARTESIAN_POINT('Ctrl Pts',(179.82387116428,617.808149224599,-39.080229970175)) ;
#60878 = CARTESIAN_POINT('Ctrl Pts',(179.957747433404,617.80176492764,-39.0800834622948)) ;
#60879 = CARTESIAN_POINT('Ctrl Pts',(180.173234897981,617.791278765631,-39.0587804834641)) ;
#60880 = CARTESIAN_POINT('Ctrl Pts',(180.255222823787,617.787241673223,-39.0456260498202)) ;
#60881 = CARTESIAN_POINT('Ctrl Pts',(180.400575981089,617.779773145553,-39.0131791288436)) ;
#60882 = CARTESIAN_POINT('Ctrl Pts',(180.464229605377,617.776392225983,-38.9957143499616)) ;
#60883 = CARTESIAN_POINT('Ctrl Pts',(180.574299998063,617.770280646188,-38.9597353443057)) ;
#60884 = CARTESIAN_POINT('Ctrl Pts',(180.621088322488,617.767595627313,-38.9425339680021)) ;
#60885 = CARTESIAN_POINT('Ctrl Pts',(180.727670551739,617.761255754453,-38.898887711218)) ;
#60886 = CARTESIAN_POINT('Ctrl Pts',(180.786917531223,617.757562060431,-38.8712576097892)) ;
#60887 = CARTESIAN_POINT('Ctrl Pts',(180.978456773859,617.745049833906,-38.7705519177621)) ;
#60888 = CARTESIAN_POINT('Ctrl Pts',(181.104000237173,617.735864903547,-38.6857215822447)) ;
#60889 = CARTESIAN_POINT('Ctrl Pts',(181.274650382973,617.722489422965,-38.5407044179735)) ;
#60890 = CARTESIAN_POINT('Ctrl Pts',(181.327659326773,617.718191225634,-38.4905656560473)) ;
#60891 = CARTESIAN_POINT('Ctrl Pts',(181.39943471103,617.712289046957,-38.4150474504193)) ;
#60892 = CARTESIAN_POINT('Ctrl Pts',(181.420457131513,617.710549601624,-38.391892842992)) ;
#60893 = CARTESIAN_POINT('Ctrl Pts',(181.463570710291,617.706975438668,-38.3421713948152)) ;
#60894 = CARTESIAN_POINT('Ctrl Pts',(181.485536379775,617.705148581621,-38.3155099691309)) ;
#60895 = CARTESIAN_POINT('Ctrl Pts',(181.593725727476,617.696047024736,-38.1772303833297)) ;
#60896 = CARTESIAN_POINT('Ctrl Pts',(181.668973288057,617.689346319362,-38.05749084968)) ;
#60897 = CARTESIAN_POINT('Ctrl Pts',(181.780046550597,617.677163736028,-37.8322636695395)) ;
#60898 = CARTESIAN_POINT('Ctrl Pts',(181.820714272263,617.671759491951,-37.729806412972)) ;
#60899 = CARTESIAN_POINT('Ctrl Pts',(181.868564944837,617.663342836343,-37.5737718847934)) ;
#60900 = CARTESIAN_POINT('Ctrl Pts',(181.88217107972,617.660543875888,-37.5223684848638)) ;
#60901 = CARTESIAN_POINT('Ctrl Pts',(181.905336639262,617.654820230289,-37.4187580074584)) ;
#60902 = CARTESIAN_POINT('Ctrl Pts',(181.914897171684,617.651898076025,-37.3665932739173)) ;
#60903 = CARTESIAN_POINT('Ctrl Pts',(181.939535636014,617.64213428699,-37.1949527141264)) ;
#60904 = CARTESIAN_POINT('Ctrl Pts',(181.946133435778,617.635033634421,-37.07452804646)) ;
#60905 = CARTESIAN_POINT('Ctrl Pts',(181.937691298984,617.619716274516,-36.8192952740957)) ;
#60906 = CARTESIAN_POINT('Ctrl Pts',(181.919939188561,617.611504833389,-36.6851189235826)) ;
#60907 = CARTESIAN_POINT('Ctrl Pts',(181.881597471068,617.601919569737,-36.5213930895733)) ;
#60908 = CARTESIAN_POINT('Ctrl Pts',(181.873264142803,617.600064804971,-36.4893221787337)) ;
#60909 = CARTESIAN_POINT('Ctrl Pts',(181.855284539896,617.596491511571,-36.4264191375629)) ;
#60910 = CARTESIAN_POINT('Ctrl Pts',(181.845679736028,617.59477176136,-36.3955853820921)) ;
#60911 = CARTESIAN_POINT('Ctrl Pts',(181.806946761933,617.588448244574,-36.2808415770441)) ;
#60912 = CARTESIAN_POINT('Ctrl Pts',(181.773113145488,617.584069505766,-36.1986156242123)) ;
#60913 = CARTESIAN_POINT('Ctrl Pts',(181.673742299194,617.573071562562,-35.9955974580883)) ;
#60914 = CARTESIAN_POINT('Ctrl Pts',(181.601263946288,617.566541251821,-35.8787790000532)) ;
#60915 = CARTESIAN_POINT('Ctrl Pts',(181.517739089189,617.559637408341,-35.7700948504488)) ;
#60916 = CARTESIAN_POINT('Ctrl Pts',(181.517739089197,617.617803659368,-35.7700948504595)) ;
#60917 = CARTESIAN_POINT('Ctrl Pts',(181.518095630332,617.617832217488,-35.7705587886382)) ;
#60918 = CARTESIAN_POINT('Ctrl Pts',(181.518451975681,617.617860772335,-35.7710228822118)) ;
#60919 = CARTESIAN_POINT('Ctrl Pts',(181.627854687921,617.626631318891,-35.9136317836402)) ;
#60920 = CARTESIAN_POINT('Ctrl Pts',(181.717835755209,617.635098718416,-36.0694147208747)) ;
#60921 = CARTESIAN_POINT('Ctrl Pts',(181.806455767298,617.647060039349,-36.2830603899659)) ;
#60922 = CARTESIAN_POINT('Ctrl Pts',(181.824593293176,617.649812918917,-36.3319675041867)) ;
#60923 = CARTESIAN_POINT('Ctrl Pts',(181.857496237792,617.655514064215,-36.4322360169524)) ;
#60924 = CARTESIAN_POINT('Ctrl Pts',(181.872157667491,617.658463251945,-36.4835889102274)) ;
#60925 = CARTESIAN_POINT('Ctrl Pts',(181.913623345838,617.668341972707,-36.6536636167769)) ;
#60926 = CARTESIAN_POINT('Ctrl Pts',(181.931883817161,617.675534875931,-36.7741869567704)) ;
#60927 = CARTESIAN_POINT('Ctrl Pts',(181.947359583335,617.690617298293,-37.0249679291579)) ;
#60928 = CARTESIAN_POINT('Ctrl Pts',(181.943084944151,617.698486619465,-37.1548057823885)) ;
#60929 = CARTESIAN_POINT('Ctrl Pts',(181.922350183053,617.70779701347,-37.3165812157369)) ;
#60930 = CARTESIAN_POINT('Ctrl Pts',(181.917283948896,617.709673857797,-37.3496750927066)) ;
#60931 = CARTESIAN_POINT('Ctrl Pts',(181.905865114521,617.713234307245,-37.4137548281389)) ;
#60932 = CARTESIAN_POINT('Ctrl Pts',(181.899601512369,617.714921345098,-37.4447461266343)) ;
#60933 = CARTESIAN_POINT('Ctrl Pts',(181.875175102307,617.72071353073,-37.5527094656252)) ;
#60934 = CARTESIAN_POINT('Ctrl Pts',(181.853285634692,617.724643504571,-37.6287728636373)) ;
#60935 = CARTESIAN_POINT('Ctrl Pts',(181.765951233217,617.737520269442,-37.8772949850392)) ;
#60936 = CARTESIAN_POINT('Ctrl Pts',(181.681722843776,617.746207733743,-38.0421723956153)) ;
#60937 = CARTESIAN_POINT('Ctrl Pts',(181.547016737167,617.758437027098,-38.2362896192365)) ;
#60938 = CARTESIAN_POINT('Ctrl Pts',(181.515792733701,617.76118182434,-38.2778289439284)) ;
#60939 = CARTESIAN_POINT('Ctrl Pts',(181.449178602575,617.766891745284,-38.3597874225629)) ;
#60940 = CARTESIAN_POINT('Ctrl Pts',(181.413710833998,617.769858970664,-38.4000910647036)) ;
#60941 = CARTESIAN_POINT('Ctrl Pts',(181.330424375225,617.776681063526,-38.4875737824711)) ;
#60942 = CARTESIAN_POINT('Ctrl Pts',(181.281789720238,617.78056848916,-38.5338885539261)) ;
#60943 = CARTESIAN_POINT('Ctrl Pts',(181.128524844758,617.792504024189,-38.666155026847)) ;
#60944 = CARTESIAN_POINT('Ctrl Pts',(181.017593418918,617.800758404951,-38.7442285517428)) ;
#60945 = CARTESIAN_POINT('Ctrl Pts',(180.848194792386,617.81228784728,-38.8400024129723)) ;
#60946 = CARTESIAN_POINT('Ctrl Pts',(180.795349973558,617.815744547612,-38.8669327484932)) ;
#60947 = CARTESIAN_POINT('Ctrl Pts',(180.714454502399,617.820753601928,-38.9038403353509)) ;
#60948 = CARTESIAN_POINT('Ctrl Pts',(180.687233212605,617.822392376592,-38.9155553319779)) ;
#60949 = CARTESIAN_POINT('Ctrl Pts',(180.625964320843,617.825965667593,-38.9403662220668)) ;
#60950 = CARTESIAN_POINT('Ctrl Pts',(180.591803853648,617.827883621515,-38.9531522047013)) ;
#60951 = CARTESIAN_POINT('Ctrl Pts',(180.514572273599,617.832092728787,-38.9797376190929)) ;
#60952 = CARTESIAN_POINT('Ctrl Pts',(180.471349262852,617.834362103501,-38.9930383347324)) ;
#60953 = CARTESIAN_POINT('Ctrl Pts',(180.313980242041,617.842428209806,-39.0358337325119)) ;
#60954 = CARTESIAN_POINT('Ctrl Pts',(180.197787086735,617.848029108326,-39.0569209600502)) ;
#60955 = CARTESIAN_POINT('Ctrl Pts',(179.989324054953,617.85827029962,-39.0764751043245)) ;
#60956 = CARTESIAN_POINT('Ctrl Pts',(179.897763572593,617.86283109334,-39.0789251444881)) ;
#60957 = CARTESIAN_POINT('Ctrl Pts',(179.755136767785,617.870241532697,-39.0732163393845)) ;
#60958 = CARTESIAN_POINT('Ctrl Pts',(179.704022034082,617.872957554038,-39.0692511757925)) ;
#60959 = CARTESIAN_POINT('Ctrl Pts',(179.598727673481,617.878702809099,-39.057107473486)) ;
#60960 = CARTESIAN_POINT('Ctrl Pts',(179.544620161169,617.881738535767,-39.0486648901577)) ;
#60961 = CARTESIAN_POINT('Ctrl Pts',(179.425183348615,617.888635827255,-39.0251076829347)) ;
#60962 = CARTESIAN_POINT('Ctrl Pts',(179.360127861777,617.892526544909,-39.0089362167855)) ;
#60963 = CARTESIAN_POINT('Ctrl Pts',(179.15568788159,617.905138467976,-38.9473644362442)) ;
#60964 = CARTESIAN_POINT('Ctrl Pts',(179.020323518093,617.914106625274,-38.8902298605387)) ;
#60965 = CARTESIAN_POINT('Ctrl Pts',(178.849011608638,617.925603804225,-38.7952482934308)) ;
#60966 = CARTESIAN_POINT('Ctrl Pts',(178.806706640264,617.928452190648,-38.7697582791156)) ;
#60967 = CARTESIAN_POINT('Ctrl Pts',(178.740981499184,617.932843638587,-38.726854536905)) ;
#60968 = CARTESIAN_POINT('Ctrl Pts',(178.71694539454,617.934440598286,-38.7104256673135)) ;
#60969 = CARTESIAN_POINT('Ctrl Pts',(178.660022721154,617.938196261291,-38.669716919506)) ;
#60970 = CARTESIAN_POINT('Ctrl Pts',(178.627497185245,617.940324828458,-38.6449572106225)) ;
#60971 = CARTESIAN_POINT('Ctrl Pts',(178.509826818459,617.948046921445,-38.5497059906233)) ;
#60972 = CARTESIAN_POINT('Ctrl Pts',(178.429667506768,617.953357959992,-38.4733469483095)) ;
#60973 = CARTESIAN_POINT('Ctrl Pts',(178.272427868787,617.964781052121,-38.2972962350808)) ;
#60974 = CARTESIAN_POINT('Ctrl Pts',(178.197578377633,617.97088958731,-38.1962288902197)) ;
#60975 = CARTESIAN_POINT('Ctrl Pts',(178.10484972858,617.980092729238,-38.0435861039979)) ;
#60976 = CARTESIAN_POINT('Ctrl Pts',(178.079049440486,617.982886524483,-37.9971503194508)) ;
#60977 = CARTESIAN_POINT('Ctrl Pts',(178.031411536465,617.988570269215,-37.9029925202018)) ;
#60978 = CARTESIAN_POINT('Ctrl Pts',(178.009545665626,617.991456392188,-37.8553299455452)) ;
#60979 = CARTESIAN_POINT('Ctrl Pts',(177.947311039176,618.000620288519,-37.7047250903747)) ;
#60980 = CARTESIAN_POINT('Ctrl Pts',(177.913412898147,618.007106835018,-37.5993368503828)) ;
#60981 = CARTESIAN_POINT('Ctrl Pts',(177.855407924417,618.022287572548,-37.3522439600267)) ;
#60982 = CARTESIAN_POINT('Ctrl Pts',(177.837341483634,618.031034681777,-37.2096951201353)) ;
#60983 = CARTESIAN_POINT('Ctrl Pts',(177.833519332619,618.041178766265,-37.0323067071832)) ;
#60984 = CARTESIAN_POINT('Ctrl Pts',(177.833634184828,618.043095164956,-36.9981748902709)) ;
#60985 = CARTESIAN_POINT('Ctrl Pts',(177.835482181044,618.046674985967,-36.9328458811284)) ;
#60986 = CARTESIAN_POINT('Ctrl Pts',(177.837076574522,618.048344116495,-36.9016557064381)) ;
#60987 = CARTESIAN_POINT('Ctrl Pts',(177.844823471743,618.053845811982,-36.7969750243422)) ;
#60988 = CARTESIAN_POINT('Ctrl Pts',(177.854220836984,618.057528018489,-36.7237765142689)) ;
#60989 = CARTESIAN_POINT('Ctrl Pts',(177.894080442057,618.068357128435,-36.5065999790718)) ;
#60990 = CARTESIAN_POINT('Ctrl Pts',(177.93607485989,618.075308188106,-36.3652348839258)) ;
#60991 = CARTESIAN_POINT('Ctrl Pts',(178.018347766972,618.085996525488,-36.1684556289195)) ;
#60992 = CARTESIAN_POINT('Ctrl Pts',(178.046833262195,618.089388001467,-36.1086258958834)) ;
#60993 = CARTESIAN_POINT('Ctrl Pts',(178.101571516978,618.095491478451,-36.006662181027)) ;
#60994 = CARTESIAN_POINT('Ctrl Pts',(178.126554005481,618.098156361988,-35.963908465536)) ;
#60995 = CARTESIAN_POINT('Ctrl Pts',(178.187329449229,618.104399400863,-35.8680280414585)) ;
#60996 = CARTESIAN_POINT('Ctrl Pts',(178.224109770048,618.108013341282,-35.8155914268306)) ;
#60997 = CARTESIAN_POINT('Ctrl Pts',(178.311505435181,618.116259575137,-35.7026101109687)) ;
#60998 = CARTESIAN_POINT('Ctrl Pts',(178.363280506203,618.120928390997,-35.6430913293319)) ;
#60999 = CARTESIAN_POINT('Ctrl Pts',(178.51429149906,618.1338774019,-35.4884275239333)) ;
#61000 = CARTESIAN_POINT('Ctrl Pts',(178.619854154395,618.142250560222,-35.4000222785229)) ;
#61001 = CARTESIAN_POINT('Ctrl Pts',(178.762315899289,618.152122669112,-35.3031887229354)) ;
#61002 = CARTESIAN_POINT('Ctrl Pts',(178.79167809621,618.154087433079,-35.2843059970602)) ;
#61003 = CARTESIAN_POINT('Ctrl Pts',(178.847667853496,618.157683606821,-35.2502839214104)) ;
#61004 = CARTESIAN_POINT('Ctrl Pts',(178.874178700074,618.159323929544,-35.234975002494)) ;
#61005 = CARTESIAN_POINT('Ctrl Pts',(178.959724829872,618.16444980428,-35.1880925940932)) ;
#61006 = CARTESIAN_POINT('Ctrl Pts',(179.019969480134,618.167813730566,-35.1588065362308)) ;
#61007 = CARTESIAN_POINT('Ctrl Pts',(179.207962434688,618.177887125873,-35.078522918502)) ;
#61008 = CARTESIAN_POINT('Ctrl Pts',(179.339482349915,618.184384509566,-35.0373564701003)) ;
#61009 = CARTESIAN_POINT('Ctrl Pts',(179.547903589878,618.194925984724,-34.9944407611673)) ;
#61010 = CARTESIAN_POINT('Ctrl Pts',(179.622449604035,618.198737527365,-34.9833194004161)) ;
#61011 = CARTESIAN_POINT('Ctrl Pts',(179.746970597257,618.205282495372,-34.9716883961272)) ;
#61012 = CARTESIAN_POINT('Ctrl Pts',(179.796656018017,618.207939844539,-34.968862358626)) ;
#61013 = CARTESIAN_POINT('Ctrl Pts',(179.90441661017,618.213824090264,-34.9666521229542)) ;
#61014 = CARTESIAN_POINT('Ctrl Pts',(179.962460511373,618.217069714695,-34.9679209561088)) ;
#61015 = CARTESIAN_POINT('Ctrl Pts',(180.086747750104,618.224189448023,-34.9759122177706)) ;
#61016 = CARTESIAN_POINT('Ctrl Pts',(180.152875020548,618.228082282332,-34.9834004601559)) ;
#61017 = CARTESIAN_POINT('Ctrl Pts',(180.353461336179,618.240157507464,-35.0160380716334)) ;
#61018 = CARTESIAN_POINT('Ctrl Pts',(180.485870393457,618.2485227758,-35.0514066279319)) ;
#61019 = CARTESIAN_POINT('Ctrl Pts',(180.660296817167,618.259483124503,-35.1172084034319)) ;
#61020 = CARTESIAN_POINT('Ctrl Pts',(180.706161606558,618.262355662103,-35.1364389914603)) ;
#61021 = CARTESIAN_POINT('Ctrl Pts',(180.777776895497,618.266775942372,-35.1695713839637)) ;
#61022 = CARTESIAN_POINT('Ctrl Pts',(180.804002672154,618.268378666778,-35.1823897484777)) ;
#61023 = CARTESIAN_POINT('Ctrl Pts',(180.866487035888,618.272155884006,-35.2145975842519)) ;
#61024 = CARTESIAN_POINT('Ctrl Pts',(180.902452338712,618.274299968275,-35.2345236712379)) ;
#61025 = CARTESIAN_POINT('Ctrl Pts',(181.033539577708,618.28209016693,-35.3123808916821)) ;
#61026 = CARTESIAN_POINT('Ctrl Pts',(181.124507528037,618.287454254803,-35.3769383077405)) ;
#61027 = CARTESIAN_POINT('Ctrl Pts',(181.284059731833,618.297571184532,-35.5109057772926)) ;
#61028 = CARTESIAN_POINT('Ctrl Pts',(181.35380900263,618.302300739728,-35.5784328434861)) ;
#61029 = CARTESIAN_POINT('Ctrl Pts',(181.453109681435,618.309836560498,-35.6892067446014)) ;
#61030 = CARTESIAN_POINT('Ctrl Pts',(181.486218887169,618.312508604253,-35.7290770797887)) ;
#61031 = CARTESIAN_POINT('Ctrl Pts',(181.517784450449,618.315241095141,-35.7701538776056)) ;
#61032 = CARTESIAN_POINT('Origin',(179.888527625402,504.710565160536,-37.0221601717597)) ;
#61033 = CARTESIAN_POINT('Ctrl Pts',(180.464073435314,504.369601015799,-35.4587334799406)) ;
#61034 = CARTESIAN_POINT('Ctrl Pts',(180.481858241129,504.370836174127,-35.4652806180445)) ;
#61035 = CARTESIAN_POINT('Ctrl Pts',(180.499530337435,504.372086174135,-35.4721308578578)) ;
#61036 = CARTESIAN_POINT('Ctrl Pts',(180.546347805476,504.375468445644,-35.4912038536254)) ;
#61037 = CARTESIAN_POINT('Ctrl Pts',(180.575263684777,504.377634369866,-35.5039547808052)) ;
#61038 = CARTESIAN_POINT('Ctrl Pts',(180.708421118899,504.387918732243,-35.5672543707548)) ;
#61039 = CARTESIAN_POINT('Ctrl Pts',(180.807566701039,504.396452987282,-35.6277640822013)) ;
#61040 = CARTESIAN_POINT('Ctrl Pts',(180.95338416137,504.409757351566,-35.739112506369)) ;
#61041 = CARTESIAN_POINT('Ctrl Pts',(181.004595257379,504.414609923142,-35.7834005229483)) ;
#61042 = CARTESIAN_POINT('Ctrl Pts',(181.093974244796,504.423370154077,-35.8707520135229)) ;
#61043 = CARTESIAN_POINT('Ctrl Pts',(181.13288079304,504.427303966535,-35.9129131777258)) ;
#61044 = CARTESIAN_POINT('Ctrl Pts',(181.202279033618,504.434576227059,-35.9963749455418)) ;
#61045 = CARTESIAN_POINT('Ctrl Pts',(181.233187769377,504.43792975164,-36.0372398000582)) ;
#61046 = CARTESIAN_POINT('Ctrl Pts',(181.341488947989,504.450217569608,-36.1950503917734)) ;
#61047 = CARTESIAN_POINT('Ctrl Pts',(181.405904049199,504.458622768934,-36.320178246905)) ;
#61048 = CARTESIAN_POINT('Ctrl Pts',(181.471385110967,504.470370578089,-36.4999242282575)) ;
#61049 = CARTESIAN_POINT('Ctrl Pts',(181.486659222833,504.473536874829,-36.5487228939999)) ;
#61050 = CARTESIAN_POINT('Ctrl Pts',(181.509395675403,504.479221744144,-36.6351144775146)) ;
#61051 = CARTESIAN_POINT('Ctrl Pts',(181.517849434592,504.481701029314,-36.672406748695)) ;
#61052 = CARTESIAN_POINT('Ctrl Pts',(181.530814044339,504.486318972039,-36.7403628224682)) ;
#61053 = CARTESIAN_POINT('Ctrl Pts',(181.535765828239,504.488435009197,-36.7709230099683)) ;
#61054 = CARTESIAN_POINT('Ctrl Pts',(181.556072539052,504.499108764789,-36.922958848566)) ;
#61055 = CARTESIAN_POINT('Ctrl Pts',(181.55885349808,504.50814735064,-37.0457273969157)) ;
#61056 = CARTESIAN_POINT('Ctrl Pts',(181.542418390989,504.521774856124,-37.2331613357748)) ;
#61057 = CARTESIAN_POINT('Ctrl Pts',(181.532806844696,504.526481007609,-37.2982463718979)) ;
#61058 = CARTESIAN_POINT('Ctrl Pts',(181.507828654272,504.535034705643,-37.417902391721)) ;
#61059 = CARTESIAN_POINT('Ctrl Pts',(181.493477503475,504.538905065808,-37.4725877020964)) ;
#61060 = CARTESIAN_POINT('Ctrl Pts',(181.46077419599,504.546133880742,-37.5755610408141)) ;
#61061 = CARTESIAN_POINT('Ctrl Pts',(181.44290338083,504.549503718074,-37.6239315340321)) ;
#61062 = CARTESIAN_POINT('Ctrl Pts',(181.370329768133,504.5614416565,-37.7954380240948)) ;
#61063 = CARTESIAN_POINT('Ctrl Pts',(181.302997205377,504.569536499776,-37.912651528029)) ;
#61064 = CARTESIAN_POINT('Ctrl Pts',(181.190523936661,504.58104808268,-38.0629149270111)) ;
#61065 = CARTESIAN_POINT('Ctrl Pts',(181.15676089823,504.584324373238,-38.1038017167691)) ;
#61066 = CARTESIAN_POINT('Ctrl Pts',(181.094822590378,504.590172986603,-38.171914542327)) ;
#61067 = CARTESIAN_POINT('Ctrl Pts',(181.067529369425,504.592702526645,-38.1998854886461)) ;
#61068 = CARTESIAN_POINT('Ctrl Pts',(181.017108761082,504.597351103467,-38.2480479364742)) ;
#61069 = CARTESIAN_POINT('Ctrl Pts',(180.994360096597,504.599443801643,-38.2686071725116)) ;
#61070 = CARTESIAN_POINT('Ctrl Pts',(180.885948072353,504.609356063916,-38.3612815766562)) ;
#61071 = CARTESIAN_POINT('Ctrl Pts',(180.793724748195,504.617585414284,-38.4252667992938)) ;
#61072 = CARTESIAN_POINT('Ctrl Pts',(180.633707227214,504.630873282899,-38.5139042103486)) ;
#61073 = CARTESIAN_POINT('Ctrl Pts',(180.56948495682,504.63598161717,-38.5442941518347)) ;
#61074 = CARTESIAN_POINT('Ctrl Pts',(180.448924593769,504.64509910191,-38.592179724118)) ;
#61075 = CARTESIAN_POINT('Ctrl Pts',(180.39322136868,504.649140498909,-38.6109621989148)) ;
#61076 = CARTESIAN_POINT('Ctrl Pts',(180.288319456093,504.656453056308,-38.6402575138159)) ;
#61077 = CARTESIAN_POINT('Ctrl Pts',(180.239414745928,504.65974712157,-38.6515624075983)) ;
#61078 = CARTESIAN_POINT('Ctrl Pts',(180.09725129968,504.669053355141,-38.6777257711572)) ;
#61079 = CARTESIAN_POINT('Ctrl Pts',(180.003144542073,504.674876422941,-38.686891098083)) ;
#61080 = CARTESIAN_POINT('Ctrl Pts',(179.803910120013,504.687059372146,-38.6893106208155)) ;
#61081 = CARTESIAN_POINT('Ctrl Pts',(179.699187324155,504.693381278864,-38.6806825099998)) ;
#61082 = CARTESIAN_POINT('Ctrl Pts',(179.560424373139,504.702392689467,-38.6559315350542)) ;
#61083 = CARTESIAN_POINT('Ctrl Pts',(179.525085339673,504.704745823462,-38.6484349945293)) ;
#61084 = CARTESIAN_POINT('Ctrl Pts',(179.45898303548,504.709305781391,-38.6321506353186)) ;
#61085 = CARTESIAN_POINT('Ctrl Pts',(179.428175899254,504.711499665684,-38.6236137411598)) ;
#61086 = CARTESIAN_POINT('Ctrl Pts',(179.361135219858,504.716399139524,-38.6029423705984)) ;
#61087 = CARTESIAN_POINT('Ctrl Pts',(179.325033208504,504.719119312238,-38.5904358887148)) ;
#61088 = CARTESIAN_POINT('Ctrl Pts',(179.20510232603,504.728367376382,-38.5442136059551)) ;
#61089 = CARTESIAN_POINT('Ctrl Pts',(179.123591223014,504.734999929496,-38.5049243036887)) ;
#61090 = CARTESIAN_POINT('Ctrl Pts',(178.973786538971,504.747537859219,-38.4170611779224)) ;
#61091 = CARTESIAN_POINT('Ctrl Pts',(178.905162392707,504.753443039656,-38.3695638406436)) ;
#61092 = CARTESIAN_POINT('Ctrl Pts',(178.801228055316,504.762609901532,-38.2854383732187)) ;
#61093 = CARTESIAN_POINT('Ctrl Pts',(178.763537028124,504.765990143768,-38.2519932022954)) ;
#61094 = CARTESIAN_POINT('Ctrl Pts',(178.684049726041,504.773275459142,-38.1747424229036)) ;
#61095 = CARTESIAN_POINT('Ctrl Pts',(178.643007357345,504.777143540881,-38.1302637216515)) ;
#61096 = CARTESIAN_POINT('Ctrl Pts',(178.495864022097,504.791632256073,-37.9522676721351)) ;
#61097 = CARTESIAN_POINT('Ctrl Pts',(178.408082403847,504.801558392518,-37.8050249291368)) ;
#61098 = CARTESIAN_POINT('Ctrl Pts',(178.331650789944,504.814679505556,-37.6161327611039)) ;
#61099 = CARTESIAN_POINT('Ctrl Pts',(178.320070429599,504.816868296652,-37.5848417560817)) ;
#61100 = CARTESIAN_POINT('Ctrl Pts',(178.298541512778,504.821417232173,-37.5208270475406)) ;
#61101 = CARTESIAN_POINT('Ctrl Pts',(178.288645824104,504.823778477856,-37.4881024983474)) ;
#61102 = CARTESIAN_POINT('Ctrl Pts',(178.25282757581,504.833462184719,-37.3550053630662)) ;
#61103 = CARTESIAN_POINT('Ctrl Pts',(178.235292629288,504.841076982294,-37.2526213268534)) ;
#61104 = CARTESIAN_POINT('Ctrl Pts',(178.219768308788,504.855851642582,-37.0497541533174)) ;
#61105 = CARTESIAN_POINT('Ctrl Pts',(178.221110629713,504.862987234671,-36.9497326292546)) ;
#61106 = CARTESIAN_POINT('Ctrl Pts',(178.236577142803,504.873295703593,-36.800497027016)) ;
#61107 = CARTESIAN_POINT('Ctrl Pts',(178.244004565297,504.876672748673,-36.7508304797807)) ;
#61108 = CARTESIAN_POINT('Ctrl Pts',(178.264939968442,504.883841173954,-36.6440694655757)) ;
#61109 = CARTESIAN_POINT('Ctrl Pts',(178.279242130992,504.887601676615,-36.5871993360155)) ;
#61110 = CARTESIAN_POINT('Ctrl Pts',(178.31733388124,504.895736764827,-36.4636820923205)) ;
#61111 = CARTESIAN_POINT('Ctrl Pts',(178.342428995667,504.900069186051,-36.3975582380914)) ;
#61112 = CARTESIAN_POINT('Ctrl Pts',(178.418298193856,504.911276768654,-36.230511463264)) ;
#61113 = CARTESIAN_POINT('Ctrl Pts',(178.475253640498,504.918090076071,-36.1328168640231)) ;
#61114 = CARTESIAN_POINT('Ctrl Pts',(178.559638748932,504.927418211188,-36.0169006278278)) ;
#61115 = CARTESIAN_POINT('Ctrl Pts',(178.578323145101,504.929447466619,-35.9926668476939)) ;
#61116 = CARTESIAN_POINT('Ctrl Pts',(178.622485743589,504.934192868097,-35.9385388064811)) ;
#61117 = CARTESIAN_POINT('Ctrl Pts',(178.648369637508,504.936932630799,-35.9090093099107)) ;
#61118 = CARTESIAN_POINT('Ctrl Pts',(178.711879488288,504.943506582762,-35.8415209538879)) ;
#61119 = CARTESIAN_POINT('Ctrl Pts',(178.750337606184,504.947374659445,-35.8044029719168)) ;
#61120 = CARTESIAN_POINT('Ctrl Pts',(178.890976691694,504.960975631911,-35.6811555490257)) ;
#61121 = CARTESIAN_POINT('Ctrl Pts',(179.001689524252,504.970700730576,-35.6054978313398)) ;
#61122 = CARTESIAN_POINT('Ctrl Pts',(179.16608245433,504.983486431906,-35.52006329648)) ;
#61123 = CARTESIAN_POINT('Ctrl Pts',(179.212984515209,504.986975423506,-35.4983935918746)) ;
#61124 = CARTESIAN_POINT('Ctrl Pts',(179.313032025306,504.994117532734,-35.4576993606721)) ;
#61125 = CARTESIAN_POINT('Ctrl Pts',(179.366289628779,504.997751507513,-35.4391246524085)) ;
#61126 = CARTESIAN_POINT('Ctrl Pts',(179.48317199108,505.005451058986,-35.4049026082535)) ;
#61127 = CARTESIAN_POINT('Ctrl Pts',(179.546983568035,505.009484837401,-35.390233749576)) ;
#61128 = CARTESIAN_POINT('Ctrl Pts',(179.733261232255,505.021048411961,-35.3588211267165)) ;
#61129 = CARTESIAN_POINT('Ctrl Pts',(179.856913734484,505.028451606098,-35.3518919182735)) ;
#61130 = CARTESIAN_POINT('Ctrl Pts',(180.011004067251,505.038479399329,-35.3603813560293)) ;
#61131 = CARTESIAN_POINT('Ctrl Pts',(180.04177803009,505.040524403632,-35.3629364047818)) ;
#61132 = CARTESIAN_POINT('Ctrl Pts',(180.110841560923,505.045239624819,-35.3706082979794)) ;
#61133 = CARTESIAN_POINT('Ctrl Pts',(180.149056365601,505.047930843947,-35.3762041444531)) ;
#61134 = CARTESIAN_POINT('Ctrl Pts',(180.281390474302,505.057460813301,-35.4003055456713)) ;
#61135 = CARTESIAN_POINT('Ctrl Pts',(180.374077836177,505.064499610795,-35.4256035430713)) ;
#61136 = CARTESIAN_POINT('Ctrl Pts',(180.464069889026,505.071458111631,-35.4587321744464)) ;
#61137 = CARTESIAN_POINT('Ctrl Pts',(180.464073435749,504.178966917533,-35.4587334801008)) ;
#61138 = CARTESIAN_POINT('Ctrl Pts',(180.464397541983,504.178987991548,-35.4588527936485)) ;
#61139 = CARTESIAN_POINT('Ctrl Pts',(180.464721613219,504.179009065212,-35.4589722087537)) ;
#61140 = CARTESIAN_POINT('Ctrl Pts',(180.542007893517,504.184035291354,-35.4874782755891)) ;
#61141 = CARTESIAN_POINT('Ctrl Pts',(180.616766377915,504.189013538016,-35.5215095031763)) ;
#61142 = CARTESIAN_POINT('Ctrl Pts',(180.744111715052,504.198079427466,-35.5912438595097)) ;
#61143 = CARTESIAN_POINT('Ctrl Pts',(180.797736273365,504.202099652675,-35.6247039981196)) ;
#61144 = CARTESIAN_POINT('Ctrl Pts',(180.890184944929,504.20951228652,-35.6899665679881)) ;
#61145 = CARTESIAN_POINT('Ctrl Pts',(180.929718254343,504.212856745465,-35.7206309484186)) ;
#61146 = CARTESIAN_POINT('Ctrl Pts',(181.031217494982,504.221960738824,-35.8069465722094)) ;
#61147 = CARTESIAN_POINT('Ctrl Pts',(181.09048547241,504.22784103648,-35.8655367559403)) ;
#61148 = CARTESIAN_POINT('Ctrl Pts',(181.206383767911,504.240565513492,-35.9986773236304)) ;
#61149 = CARTESIAN_POINT('Ctrl Pts',(181.261623646416,504.247419689051,-36.0740733575443)) ;
#61150 = CARTESIAN_POINT('Ctrl Pts',(181.33044396571,504.256925330051,-36.1867367240614)) ;
#61151 = CARTESIAN_POINT('Ctrl Pts',(181.349470664175,504.259685073744,-36.2204738574176)) ;
#61152 = CARTESIAN_POINT('Ctrl Pts',(181.382160963986,504.264645208874,-36.283475009766)) ;
#61153 = CARTESIAN_POINT('Ctrl Pts',(181.39618383512,504.266860849097,-36.3125337374002)) ;
#61154 = CARTESIAN_POINT('Ctrl Pts',(181.424081059909,504.271439445078,-36.3749102183598)) ;
#61155 = CARTESIAN_POINT('Ctrl Pts',(181.437734619378,504.273790409771,-36.4083075344695)) ;
#61156 = CARTESIAN_POINT('Ctrl Pts',(181.506556796633,504.286431058303,-36.5936138726663)) ;
#61157 = CARTESIAN_POINT('Ctrl Pts',(181.540485136173,504.295886806324,-36.7524949464847)) ;
#61158 = CARTESIAN_POINT('Ctrl Pts',(181.55502809248,504.309883907322,-36.9755956979436)) ;
#61159 = CARTESIAN_POINT('Ctrl Pts',(181.555606853691,504.313836537297,-37.0375701003839)) ;
#61160 = CARTESIAN_POINT('Ctrl Pts',(181.550393409002,504.321214382679,-37.1498584706652)) ;
#61161 = CARTESIAN_POINT('Ctrl Pts',(181.545761145486,504.324597636104,-37.2001512812365)) ;
#61162 = CARTESIAN_POINT('Ctrl Pts',(181.518277621417,504.338348576201,-37.3990917244728)) ;
#61163 = CARTESIAN_POINT('Ctrl Pts',(181.477636852574,504.349311778951,-37.5445347395339)) ;
#61164 = CARTESIAN_POINT('Ctrl Pts',(181.398355636548,504.363835546107,-37.7281687492511)) ;
#61165 = CARTESIAN_POINT('Ctrl Pts',(181.376609984472,504.367424777227,-37.7729199624627)) ;
#61166 = CARTESIAN_POINT('Ctrl Pts',(181.334940390606,504.373603875988,-37.8497249432087)) ;
#61167 = CARTESIAN_POINT('Ctrl Pts',(181.315868805024,504.376222749187,-37.8822014920658)) ;
#61168 = CARTESIAN_POINT('Ctrl Pts',(181.27879310803,504.38091367585,-37.9407006800149)) ;
#61169 = CARTESIAN_POINT('Ctrl Pts',(181.261118668403,504.383001687648,-37.966908152936)) ;
#61170 = CARTESIAN_POINT('Ctrl Pts',(181.17440346602,504.392650976523,-38.0879133588464)) ;
#61171 = CARTESIAN_POINT('Ctrl Pts',(181.096216522383,504.399705139639,-38.1757639646798)) ;
#61172 = CARTESIAN_POINT('Ctrl Pts',(180.95958800213,504.411000265744,-38.3000202866712)) ;
#61173 = CARTESIAN_POINT('Ctrl Pts',(180.907033714774,504.41514676577,-38.3422893903067)) ;
#61174 = CARTESIAN_POINT('Ctrl Pts',(180.805275970627,504.423020531029,-38.4144311223862)) ;
#61175 = CARTESIAN_POINT('Ctrl Pts',(180.75680742599,504.426712462012,-38.4451622452122)) ;
#61176 = CARTESIAN_POINT('Ctrl Pts',(180.661807857348,504.433917033347,-38.4987333038483)) ;
#61177 = CARTESIAN_POINT('Ctrl Pts',(180.615607305877,504.437407378656,-38.5220217087054)) ;
#61178 = CARTESIAN_POINT('Ctrl Pts',(180.443722488701,504.450389216829,-38.5988548089519)) ;
#61179 = CARTESIAN_POINT('Ctrl Pts',(180.312681905936,504.460334784631,-38.6390358048322)) ;
#61180 = CARTESIAN_POINT('Ctrl Pts',(180.126490967855,504.47408234086,-38.6719150463779)) ;
#61181 = CARTESIAN_POINT('Ctrl Pts',(180.074333077924,504.477885165741,-38.6786005447031)) ;
#61182 = CARTESIAN_POINT('Ctrl Pts',(179.983144057023,504.484369812791,-38.6859266367473)) ;
#61183 = CARTESIAN_POINT('Ctrl Pts',(179.944243066473,504.48708437079,-38.6876833726016)) ;
#61184 = CARTESIAN_POINT('Ctrl Pts',(179.874292763182,504.491832202552,-38.6883881544817)) ;
#61185 = CARTESIAN_POINT('Ctrl Pts',(179.843270351526,504.493887127312,-38.6878342748889)) ;
#61186 = CARTESIAN_POINT('Ctrl Pts',(179.703842866005,504.502956098488,-38.6814463918579)) ;
#61187 = CARTESIAN_POINT('Ctrl Pts',(179.59613540767,504.509528829693,-38.6658914873721)) ;
#61188 = CARTESIAN_POINT('Ctrl Pts',(179.420462885489,504.520576584962,-38.6226920564744)) ;
#61189 = CARTESIAN_POINT('Ctrl Pts',(179.351432812034,504.525004994953,-38.6008669429078)) ;
#61190 = CARTESIAN_POINT('Ctrl Pts',(179.228664767574,504.533288239,-38.5530647086376)) ;
#61191 = CARTESIAN_POINT('Ctrl Pts',(179.174486032451,504.537097696241,-38.5285568600258)) ;
#61192 = CARTESIAN_POINT('Ctrl Pts',(179.076978581403,504.544330184364,-38.4780055800623)) ;
#61193 = CARTESIAN_POINT('Ctrl Pts',(179.033301757414,504.54772004277,-38.4527843209506)) ;
#61194 = CARTESIAN_POINT('Ctrl Pts',(178.912002547721,504.557609319271,-38.375198508149)) ;
#61195 = CARTESIAN_POINT('Ctrl Pts',(178.837567588632,504.564277771763,-38.3182280124686)) ;
#61196 = CARTESIAN_POINT('Ctrl Pts',(178.690540302175,504.578677649443,-38.1846676287889)) ;
#61197 = CARTESIAN_POINT('Ctrl Pts',(178.619619798217,504.586408943609,-38.1068129682312)) ;
#61198 = CARTESIAN_POINT('Ctrl Pts',(178.534475663348,504.596417829104,-37.9934708275068)) ;
#61199 = CARTESIAN_POINT('Ctrl Pts',(178.513419489688,504.598964773972,-37.9634248877142)) ;
#61200 = CARTESIAN_POINT('Ctrl Pts',(178.475880213643,504.603610417177,-37.9059063941441)) ;
#61201 = CARTESIAN_POINT('Ctrl Pts',(178.459165135602,504.605721025403,-37.8786081533552)) ;
#61202 = CARTESIAN_POINT('Ctrl Pts',(178.386961736296,504.615114106342,-37.7526804414239)) ;
#61203 = CARTESIAN_POINT('Ctrl Pts',(178.340817151707,504.621933938469,-37.6490247083484)) ;
#61204 = CARTESIAN_POINT('Ctrl Pts',(178.284137746364,504.633047924257,-37.4762540826236)) ;
#61205 = CARTESIAN_POINT('Ctrl Pts',(178.266792826746,504.637265865347,-37.4097726105492)) ;
#61206 = CARTESIAN_POINT('Ctrl Pts',(178.242469212816,504.645243797963,-37.2855983544642)) ;
#61207 = CARTESIAN_POINT('Ctrl Pts',(178.234310246879,504.648965943941,-37.2282465556806)) ;
#61208 = CARTESIAN_POINT('Ctrl Pts',(178.2245658586,504.656184142796,-37.1193098536697)) ;
#61209 = CARTESIAN_POINT('Ctrl Pts',(178.222358868817,504.659655386995,-37.0678490207687)) ;
#61210 = CARTESIAN_POINT('Ctrl Pts',(178.22302421881,504.672848961248,-36.8763052320636)) ;
#61211 = CARTESIAN_POINT('Ctrl Pts',(178.241173435281,504.683057876188,-36.7368801978048)) ;
#61212 = CARTESIAN_POINT('Ctrl Pts',(178.289492096273,504.696961405301,-36.5517631179949)) ;
#61213 = CARTESIAN_POINT('Ctrl Pts',(178.304735847762,504.700669898913,-36.5027448502892)) ;
#61214 = CARTESIAN_POINT('Ctrl Pts',(178.335290740104,504.707020036296,-36.4184358237774)) ;
#61215 = CARTESIAN_POINT('Ctrl Pts',(178.349606417897,504.709692759533,-36.3828245552561)) ;
#61216 = CARTESIAN_POINT('Ctrl Pts',(178.377783719757,504.714412846952,-36.3191777561543)) ;
#61217 = CARTESIAN_POINT('Ctrl Pts',(178.391227475442,504.716479468642,-36.2909804335926)) ;
#61218 = CARTESIAN_POINT('Ctrl Pts',(178.453430439315,504.725342171005,-36.1694345175893)) ;
#61219 = CARTESIAN_POINT('Ctrl Pts',(178.510190745571,504.731728824381,-36.0804391382631)) ;
#61220 = CARTESIAN_POINT('Ctrl Pts',(178.620236259792,504.742651695549,-35.9393833058967)) ;
#61221 = CARTESIAN_POINT('Ctrl Pts',(178.669281124357,504.747151170526,-35.8844406563264)) ;
#61222 = CARTESIAN_POINT('Ctrl Pts',(178.764584924159,504.75553769545,-35.7909403012174)) ;
#61223 = CARTESIAN_POINT('Ctrl Pts',(178.8096062676,504.759376751538,-35.7513034015851)) ;
#61224 = CARTESIAN_POINT('Ctrl Pts',(178.896607173533,504.766668763896,-35.6826682676852)) ;
#61225 = CARTESIAN_POINT('Ctrl Pts',(178.937971197453,504.770088021529,-35.6530048726729)) ;
#61226 = CARTESIAN_POINT('Ctrl Pts',(179.05693685158,504.779829784863,-35.5756828560351)) ;
#61227 = CARTESIAN_POINT('Ctrl Pts',(179.137173942613,504.786306529392,-35.5324277339193)) ;
#61228 = CARTESIAN_POINT('Ctrl Pts',(179.297212372072,504.798959401514,-35.4623816376404)) ;
#61229 = CARTESIAN_POINT('Ctrl Pts',(179.376315704695,504.805097940736,-35.4346457977434)) ;
#61230 = CARTESIAN_POINT('Ctrl Pts',(179.505610781237,504.814714457185,-35.3999869536163)) ;
#61231 = CARTESIAN_POINT('Ctrl Pts',(179.554620108505,504.818265938231,-35.3891941194007)) ;
#61232 = CARTESIAN_POINT('Ctrl Pts',(179.633179014945,504.823738140319,-35.3755796941561)) ;
#61233 = CARTESIAN_POINT('Ctrl Pts',(179.662438845217,504.825725098908,-35.3713075567878)) ;
#61234 = CARTESIAN_POINT('Ctrl Pts',(179.744420682284,504.831157517958,-35.3615588122423)) ;
#61235 = CARTESIAN_POINT('Ctrl Pts',(179.797312268705,504.8345175028,-35.3578150417454)) ;
#61236 = CARTESIAN_POINT('Ctrl Pts',(179.961213487743,504.844728458033,-35.3540530046583)) ;
#61237 = CARTESIAN_POINT('Ctrl Pts',(180.072108380191,504.851369896765,-35.362592520638)) ;
#61238 = CARTESIAN_POINT('Ctrl Pts',(180.252392080602,504.862705117642,-35.3947792286458)) ;
#61239 = CARTESIAN_POINT('Ctrl Pts',(180.322541431123,504.867251806807,-35.4120682142025)) ;
#61240 = CARTESIAN_POINT('Ctrl Pts',(180.415779168701,504.873616399834,-35.4415847181096)) ;
#61241 = CARTESIAN_POINT('Ctrl Pts',(180.440028900372,504.87530171097,-35.4498819413305)) ;
#61242 = CARTESIAN_POINT('Ctrl Pts',(180.464073449582,504.877005588434,-35.458733485193)) ;
#61243 = CARTESIAN_POINT('Origin',(29.888527625402,504.710565160562,-37.0221601717529)) ;
#61244 = CARTESIAN_POINT('Ctrl Pts',(30.4640904795472,504.369620557053,-35.4587397545496)) ;
#61245 = CARTESIAN_POINT('Ctrl Pts',(30.4818072267917,504.370851028822,-35.4652620575066)) ;
#61246 = CARTESIAN_POINT('Ctrl Pts',(30.4994121352201,504.372096230735,-35.4720851531116)) ;
#61247 = CARTESIAN_POINT('Ctrl Pts',(30.5461349865861,504.375471236898,-35.4911130913441)) ;
#61248 = CARTESIAN_POINT('Ctrl Pts',(30.5750232638434,504.377634739377,-35.503846723006)) ;
#61249 = CARTESIAN_POINT('Ctrl Pts',(30.7084207921841,504.387935871951,-35.56723141876)) ;
#61250 = CARTESIAN_POINT('Ctrl Pts',(30.807807336918,504.396492032086,-35.6278989566728)) ;
#61251 = CARTESIAN_POINT('Ctrl Pts',(30.9537451828525,504.409810285808,-35.7394168085837)) ;
#61252 = CARTESIAN_POINT('Ctrl Pts',(31.0048788466309,504.414656247058,-35.7836608378205)) ;
#61253 = CARTESIAN_POINT('Ctrl Pts',(31.094150352441,504.423406943605,-35.8709384745049)) ;
#61254 = CARTESIAN_POINT('Ctrl Pts',(31.1330228165377,504.42733768956,-35.9130746596511)) ;
#61255 = CARTESIAN_POINT('Ctrl Pts',(31.2023854262371,504.434606817046,-35.9965112568204)) ;
#61256 = CARTESIAN_POINT('Ctrl Pts',(31.2332894861913,504.437960144194,-36.0373787220969)) ;
#61257 = CARTESIAN_POINT('Ctrl Pts',(31.3414899318344,504.450237873685,-36.1950772960683)) ;
#61258 = CARTESIAN_POINT('Ctrl Pts',(31.4058400244181,504.458634702507,-36.3200695238254)) ;
#61259 = CARTESIAN_POINT('Ctrl Pts',(31.4713149728053,504.470375743832,-36.4997073047313)) ;
#61260 = CARTESIAN_POINT('Ctrl Pts',(31.4866085210478,504.47354464176,-36.548546939597)) ;
#61261 = CARTESIAN_POINT('Ctrl Pts',(31.509368349094,504.479233295625,-36.6349981986934)) ;
#61262 = CARTESIAN_POINT('Ctrl Pts',(31.5178287374945,504.481713681474,-36.6723082882773)) ;
#61263 = CARTESIAN_POINT('Ctrl Pts',(31.5307973189628,504.486331667881,-36.740267060104)) ;
#61264 = CARTESIAN_POINT('Ctrl Pts',(31.5357485560298,504.488446541567,-36.7708116897684)) ;
#61265 = CARTESIAN_POINT('Ctrl Pts',(31.5560816371796,504.499127512867,-36.9229558446275)) ;
#61266 = CARTESIAN_POINT('Ctrl Pts',(31.5588609984445,504.508175784895,-37.0458518849898)) ;
#61267 = CARTESIAN_POINT('Ctrl Pts',(31.5423903234936,504.521809135464,-37.2333685292144)) ;
#61268 = CARTESIAN_POINT('Ctrl Pts',(31.5327773935459,504.5265121807,-37.2984120089292)) ;
#61269 = CARTESIAN_POINT('Ctrl Pts',(31.5078027914526,504.535061250799,-37.4180051352628)) ;
#61270 = CARTESIAN_POINT('Ctrl Pts',(31.4934539865168,504.538930028759,-37.4726687920088)) ;
#61271 = CARTESIAN_POINT('Ctrl Pts',(31.4607546069237,504.546156970532,-37.575616289686)) ;
#61272 = CARTESIAN_POINT('Ctrl Pts',(31.4428836514145,504.549526461959,-37.62398212294)) ;
#61273 = CARTESIAN_POINT('Ctrl Pts',(31.3703229305544,504.561461240068,-37.795443819484)) ;
#61274 = CARTESIAN_POINT('Ctrl Pts',(31.3030123891598,504.5695536622,-37.9126210641733)) ;
#61275 = CARTESIAN_POINT('Ctrl Pts',(31.1905646628836,504.58106319146,-38.0628645200647)) ;
#61276 = CARTESIAN_POINT('Ctrl Pts',(31.1567962696498,504.584340083067,-38.1037607655317)) ;
#61277 = CARTESIAN_POINT('Ctrl Pts',(31.0948503770259,504.59018948277,-38.171885498301)) ;
#61278 = CARTESIAN_POINT('Ctrl Pts',(31.0675555457996,504.592719186309,-38.19985939045)) ;
#61279 = CARTESIAN_POINT('Ctrl Pts',(31.0171408119758,504.597367231119,-38.2480181786567)) ;
#61280 = CARTESIAN_POINT('Ctrl Pts',(30.9944001770837,504.599459194373,-38.2685713665322)) ;
#61281 = CARTESIAN_POINT('Ctrl Pts',(30.8859316669576,504.609376711437,-38.3613012386849)) ;
#61282 = CARTESIAN_POINT('Ctrl Pts',(30.7936320177673,504.617612868785,-38.4253337212463)) ;
#61283 = CARTESIAN_POINT('Ctrl Pts',(30.6335567869241,504.63090447705,-38.5139776708744)) ;
#61284 = CARTESIAN_POINT('Ctrl Pts',(30.5693638243277,504.636010132638,-38.5443466897619)) ;
#61285 = CARTESIAN_POINT('Ctrl Pts',(30.4488504973312,504.64512366722,-38.5922054866997)) ;
#61286 = CARTESIAN_POINT('Ctrl Pts',(30.3931638365256,504.64916373651,-38.6109797977536)) ;
#61287 = CARTESIAN_POINT('Ctrl Pts',(30.2882856003111,504.656474513121,-38.6402656589938)) ;
#61288 = CARTESIAN_POINT('Ctrl Pts',(30.2393875840542,504.659768086624,-38.6515680386249)) ;
#61289 = CARTESIAN_POINT('Ctrl Pts',(30.0972327074653,504.669073686927,-38.6777280030521)) ;
#61290 = CARTESIAN_POINT('Ctrl Pts',(30.0031278187236,504.674896606954,-38.6868921379273)) ;
#61291 = CARTESIAN_POINT('Ctrl Pts',(29.8038991865405,504.687079164596,-38.6893098239551)) ;
#61292 = CARTESIAN_POINT('Ctrl Pts',(29.6991802951144,504.693400835222,-38.6806814645055)) ;
#61293 = CARTESIAN_POINT('Ctrl Pts',(29.5604248691055,504.702411739959,-38.655931551754)) ;
#61294 = CARTESIAN_POINT('Ctrl Pts',(29.525089495292,504.704764620284,-38.6484358399948)) ;
#61295 = CARTESIAN_POINT('Ctrl Pts',(29.458998099112,504.709323786646,-38.6321545039943)) ;
#61296 = CARTESIAN_POINT('Ctrl Pts',(29.428198159912,504.71151712402,-38.6236199890625)) ;
#61297 = CARTESIAN_POINT('Ctrl Pts',(29.3611760464376,504.716415145603,-38.6029556946343)) ;
#61298 = CARTESIAN_POINT('Ctrl Pts',(29.3250852623283,504.719134399474,-38.5904542925922)) ;
#61299 = CARTESIAN_POINT('Ctrl Pts',(29.2052220738143,504.728376962964,-38.5442636730996)) ;
#61300 = CARTESIAN_POINT('Ctrl Pts',(29.1237635829594,504.735004858204,-38.5050094135889)) ;
#61301 = CARTESIAN_POINT('Ctrl Pts',(28.9737358103163,504.747560678263,-38.4170461880854)) ;
#61302 = CARTESIAN_POINT('Ctrl Pts',(28.904865239867,504.753487307483,-38.3693658628624)) ;
#61303 = CARTESIAN_POINT('Ctrl Pts',(28.8007541930881,504.7626710157,-38.2850289639115)) ;
#61304 = CARTESIAN_POINT('Ctrl Pts',(28.7631017392957,504.766048273813,-38.2515934381774)) ;
#61305 = CARTESIAN_POINT('Ctrl Pts',(28.68358132078,504.773337771596,-38.1742588931823)) ;
#61306 = CARTESIAN_POINT('Ctrl Pts',(28.6424787659963,504.777212502998,-38.1296757094903)) ;
#61307 = CARTESIAN_POINT('Ctrl Pts',(28.4948701589087,504.791753563263,-37.9509186692316)) ;
#61308 = CARTESIAN_POINT('Ctrl Pts',(28.4068720471786,504.801719284437,-37.8028989543274)) ;
#61309 = CARTESIAN_POINT('Ctrl Pts',(28.3306713993951,504.814878844816,-37.6135360615046)) ;
#61310 = CARTESIAN_POINT('Ctrl Pts',(28.3192823274698,504.817043101958,-37.5826156517476)) ;
#61311 = CARTESIAN_POINT('Ctrl Pts',(28.2978098136908,504.82160031745,-37.5185207020309)) ;
#61312 = CARTESIAN_POINT('Ctrl Pts',(28.2878305142513,504.823996765863,-37.485328839444)) ;
#61313 = CARTESIAN_POINT('Ctrl Pts',(28.2519775242662,504.833773376532,-37.3510233524459)) ;
#61314 = CARTESIAN_POINT('Ctrl Pts',(28.2345960258612,504.841443558282,-37.2478931395869)) ;
#61315 = CARTESIAN_POINT('Ctrl Pts',(28.2198204393433,504.856129917374,-37.0460990796966)) ;
#61316 = CARTESIAN_POINT('Ctrl Pts',(28.2212989741902,504.863128964229,-36.947922933889)) ;
#61317 = CARTESIAN_POINT('Ctrl Pts',(28.236573932299,504.873310251979,-36.8005240993064)) ;
#61318 = CARTESIAN_POINT('Ctrl Pts',(28.2439982782578,504.876686277838,-36.7508711585461)) ;
#61319 = CARTESIAN_POINT('Ctrl Pts',(28.2649251132639,504.883852817423,-36.6441351704651)) ;
#61320 = CARTESIAN_POINT('Ctrl Pts',(28.2792217584378,504.887612455738,-36.587276377783)) ;
#61321 = CARTESIAN_POINT('Ctrl Pts',(28.3172965947635,504.89574519811,-36.4637897806799)) ;
#61322 = CARTESIAN_POINT('Ctrl Pts',(28.3423789427392,504.900076169707,-36.3976846332995)) ;
#61323 = CARTESIAN_POINT('Ctrl Pts',(28.4182598676669,504.911287323251,-36.2305700188501)) ;
#61324 = CARTESIAN_POINT('Ctrl Pts',(28.4752587737452,504.918105330507,-36.1327974778647)) ;
#61325 = CARTESIAN_POINT('Ctrl Pts',(28.5596979907462,504.927438555201,-36.0168226005408)) ;
#61326 = CARTESIAN_POINT('Ctrl Pts',(28.5783780831064,504.929467190729,-35.992597208781)) ;
#61327 = CARTESIAN_POINT('Ctrl Pts',(28.6225395090025,504.934212130542,-35.9384758727604)) ;
#61328 = CARTESIAN_POINT('Ctrl Pts',(28.6484270923263,504.936952080011,-35.9089451857543)) ;
#61329 = CARTESIAN_POINT('Ctrl Pts',(28.7119488890555,504.943526749772,-35.8414513926158)) ;
#61330 = CARTESIAN_POINT('Ctrl Pts',(28.7504156532799,504.947395358522,-35.80432964191)) ;
#61331 = CARTESIAN_POINT('Ctrl Pts',(28.8910109427986,504.96099076579,-35.6811378833544)) ;
#61332 = CARTESIAN_POINT('Ctrl Pts',(29.0016582060664,504.97070963352,-35.6055248417994)) ;
#61333 = CARTESIAN_POINT('Ctrl Pts',(29.1659717199386,504.983489504468,-35.5201167017051)) ;
#61334 = CARTESIAN_POINT('Ctrl Pts',(29.2128684082581,504.986978200553,-35.498445211476)) ;
#61335 = CARTESIAN_POINT('Ctrl Pts',(29.3128978300854,504.994119221994,-35.4577491620444)) ;
#61336 = CARTESIAN_POINT('Ctrl Pts',(29.3661424689265,504.997752433225,-35.4391736330252)) ;
#61337 = CARTESIAN_POINT('Ctrl Pts',(29.4829858156303,505.005449635377,-35.4049502997174)) ;
#61338 = CARTESIAN_POINT('Ctrl Pts',(29.5467710357804,505.00948187133,-35.3902792518849)) ;
#61339 = CARTESIAN_POINT('Ctrl Pts',(29.7331360403668,505.021050937422,-35.3588240280395)) ;
#61340 = CARTESIAN_POINT('Ctrl Pts',(29.8569074724625,505.028460527986,-35.3518832920923)) ;
#61341 = CARTESIAN_POINT('Ctrl Pts',(30.0111009000491,505.038495321206,-35.3603887638529)) ;
#61342 = CARTESIAN_POINT('Ctrl Pts',(30.0418603211689,505.040539427872,-35.3629442760115)) ;
#61343 = CARTESIAN_POINT('Ctrl Pts',(30.1109129553052,505.045254007532,-35.3706178213031)) ;
#61344 = CARTESIAN_POINT('Ctrl Pts',(30.1491312633468,505.047945531556,-35.376215912461)) ;
#61345 = CARTESIAN_POINT('Ctrl Pts',(30.2814475543236,505.057474417214,-35.4003205988776)) ;
#61346 = CARTESIAN_POINT('Ctrl Pts',(30.3741140780086,505.064511658039,-35.4256158096493)) ;
#61347 = CARTESIAN_POINT('Ctrl Pts',(30.4640863420645,505.071468680575,-35.458738231369)) ;
#61348 = CARTESIAN_POINT('Ctrl Pts',(30.4640904799732,504.178934308784,-35.4587397547064)) ;
#61349 = CARTESIAN_POINT('Ctrl Pts',(30.4907011144323,504.180665101958,-35.4685362832436)) ;
#61350 = CARTESIAN_POINT('Ctrl Pts',(30.5170714890677,504.182393321346,-35.4790158374907)) ;
#61351 = CARTESIAN_POINT('Ctrl Pts',(30.6056643235233,504.188277764651,-35.5168731914104)) ;
#61352 = CARTESIAN_POINT('Ctrl Pts',(30.6664576028908,504.192452399163,-35.547372768982)) ;
#61353 = CARTESIAN_POINT('Ctrl Pts',(30.7749430871822,504.200360350362,-35.6103774131304)) ;
#61354 = CARTESIAN_POINT('Ctrl Pts',(30.8231369247307,504.204056835209,-35.6418097956032)) ;
#61355 = CARTESIAN_POINT('Ctrl Pts',(30.910970371616,504.211227626555,-35.705806787347)) ;
#61356 = CARTESIAN_POINT('Ctrl Pts',(30.9509197831789,504.214677510178,-35.7378326074416)) ;
#61357 = CARTESIAN_POINT('Ctrl Pts',(31.0955111224068,504.227942923774,-35.865112990807)) ;
#61358 = CARTESIAN_POINT('Ctrl Pts',(31.1893389281624,504.238260893217,-35.9717116928767)) ;
#61359 = CARTESIAN_POINT('Ctrl Pts',(31.2970019770797,504.25222851145,-36.1309059329223)) ;
#61360 = CARTESIAN_POINT('Ctrl Pts',(31.3235110651886,504.255898359007,-36.1742466747629)) ;
#61361 = CARTESIAN_POINT('Ctrl Pts',(31.366375972885,504.262191723867,-36.2521133151798)) ;
#61362 = CARTESIAN_POINT('Ctrl Pts',(31.3836028547328,504.264845741402,-36.2861176778182)) ;
#61363 = CARTESIAN_POINT('Ctrl Pts',(31.4127861562838,504.269545294304,-36.3489846440859)) ;
#61364 = CARTESIAN_POINT('Ctrl Pts',(31.4251251096603,504.271609424052,-36.3776466676352)) ;
#61365 = CARTESIAN_POINT('Ctrl Pts',(31.4755645661525,504.280470034501,-36.5045093805009)) ;
#61366 = CARTESIAN_POINT('Ctrl Pts',(31.5051137642256,504.28685660227,-36.6058622738222)) ;
#61367 = CARTESIAN_POINT('Ctrl Pts',(31.5387147580193,504.297780284296,-36.7816289284403)) ;
#61368 = CARTESIAN_POINT('Ctrl Pts',(31.5477281471907,504.302280659341,-36.8547520594954)) ;
#61369 = CARTESIAN_POINT('Ctrl Pts',(31.5552580151837,504.310668340292,-36.9880900742235)) ;
#61370 = CARTESIAN_POINT('Ctrl Pts',(31.55540420449,504.314507575305,-37.0480849560254)) ;
#61371 = CARTESIAN_POINT('Ctrl Pts',(31.5496982404839,504.321797888635,-37.1587422788779)) ;
#61372 = CARTESIAN_POINT('Ctrl Pts',(31.5447553096988,504.32521516324,-37.2093802441109)) ;
#61373 = CARTESIAN_POINT('Ctrl Pts',(31.5245676218829,504.334934620541,-37.3495161243687)) ;
#61374 = CARTESIAN_POINT('Ctrl Pts',(31.5043172307581,504.341389633905,-37.4381025199924)) ;
#61375 = CARTESIAN_POINT('Ctrl Pts',(31.4448062630143,504.35567833131,-37.6262474020342)) ;
#61376 = CARTESIAN_POINT('Ctrl Pts',(31.4029658153932,504.36352646484,-37.7245865547845)) ;
#61377 = CARTESIAN_POINT('Ctrl Pts',(31.3341699895455,504.373701781066,-37.8510561122995)) ;
#61378 = CARTESIAN_POINT('Ctrl Pts',(31.3152272053732,504.37629781547,-37.8832520369713)) ;
#61379 = CARTESIAN_POINT('Ctrl Pts',(31.2782180182557,504.380974069887,-37.9415747326819)) ;
#61380 = CARTESIAN_POINT('Ctrl Pts',(31.2604575940171,504.383068956177,-37.9678719856091)) ;
#61381 = CARTESIAN_POINT('Ctrl Pts',(31.1743298119563,504.392637318802,-38.0878610062847)) ;
#61382 = CARTESIAN_POINT('Ctrl Pts',(31.0970414817693,504.399618028477,-38.1747690329425)) ;
#61383 = CARTESIAN_POINT('Ctrl Pts',(30.961272612537,504.410855710863,-38.2986269216421)) ;
#61384 = CARTESIAN_POINT('Ctrl Pts',(30.9084663887144,504.415024194965,-38.3412026621245)) ;
#61385 = CARTESIAN_POINT('Ctrl Pts',(30.8063211535929,504.42292979897,-38.4137490700687)) ;
#61386 = CARTESIAN_POINT('Ctrl Pts',(30.7577365016669,504.426630812306,-38.4446014988423)) ;
#61387 = CARTESIAN_POINT('Ctrl Pts',(30.6626998312883,504.433838277046,-38.4982628230963)) ;
#61388 = CARTESIAN_POINT('Ctrl Pts',(30.6165908763741,504.43732162946,-38.5215415474714)) ;
#61389 = CARTESIAN_POINT('Ctrl Pts',(30.4437705063967,504.450373728195,-38.5989397397799)) ;
#61390 = CARTESIAN_POINT('Ctrl Pts',(30.3115842294009,504.460407264738,-38.6394225371948)) ;
#61391 = CARTESIAN_POINT('Ctrl Pts',(30.1246126224308,504.474206594011,-38.6721714552532)) ;
#61392 = CARTESIAN_POINT('Ctrl Pts',(30.0728688706349,504.477977406946,-38.6787507480919)) ;
#61393 = CARTESIAN_POINT('Ctrl Pts',(29.9822867808964,504.484416414237,-38.685970735421)) ;
#61394 = CARTESIAN_POINT('Ctrl Pts',(29.9435749109091,504.487116777064,-38.6877011601384)) ;
#61395 = CARTESIAN_POINT('Ctrl Pts',(29.8737630129181,504.491853884982,-38.6883845013247)) ;
#61396 = CARTESIAN_POINT('Ctrl Pts',(29.842689357502,504.493911516148,-38.6878193451084)) ;
#61397 = CARTESIAN_POINT('Ctrl Pts',(29.7041100929686,504.502922643108,-38.6814176055466)) ;
#61398 = CARTESIAN_POINT('Ctrl Pts',(29.5972914075657,504.509443756828,-38.6660375990937)) ;
#61399 = CARTESIAN_POINT('Ctrl Pts',(29.4221165524651,504.520455775701,-38.6231897395625)) ;
#61400 = CARTESIAN_POINT('Ctrl Pts',(29.3527489373109,504.524902935258,-38.6013293068749)) ;
#61401 = CARTESIAN_POINT('Ctrl Pts',(29.2295202282037,504.53321287539,-38.5534382064981)) ;
#61402 = CARTESIAN_POINT('Ctrl Pts',(29.1752099573159,504.537029566373,-38.5289049259005)) ;
#61403 = CARTESIAN_POINT('Ctrl Pts',(29.0776176967347,504.544265183361,-38.4783596755257)) ;
#61404 = CARTESIAN_POINT('Ctrl Pts',(29.0339792758185,504.54765031761,-38.453187099049)) ;
#61405 = CARTESIAN_POINT('Ctrl Pts',(28.9148868609788,504.557354038443,-38.3770979212853)) ;
#61406 = CARTESIAN_POINT('Ctrl Pts',(28.8423754253948,504.563828251882,-38.3219268716572)) ;
#61407 = CARTESIAN_POINT('Ctrl Pts',(28.6954838152663,504.578135134068,-38.1898758427256)) ;
#61408 = CARTESIAN_POINT('Ctrl Pts',(28.623247345394,504.585981263866,-38.111187502659)) ;
#61409 = CARTESIAN_POINT('Ctrl Pts',(28.5365293980443,504.596153456221,-37.9963520285435)) ;
#61410 = CARTESIAN_POINT('Ctrl Pts',(28.5150426212387,504.598748664611,-37.9658171489067)) ;
#61411 = CARTESIAN_POINT('Ctrl Pts',(28.4772641271797,504.603419285255,-37.9081020703248)) ;
#61412 = CARTESIAN_POINT('Ctrl Pts',(28.460688141321,504.605509544811,-37.8811318041395)) ;
#61413 = CARTESIAN_POINT('Ctrl Pts',(28.386715734315,504.615112203666,-37.7527088308068)) ;
#61414 = CARTESIAN_POINT('Ctrl Pts',(28.3392924273754,504.622124959081,-37.6458733421152)) ;
#61415 = CARTESIAN_POINT('Ctrl Pts',(28.2825984776944,504.63338753655,-37.4706225938849)) ;
#61416 = CARTESIAN_POINT('Ctrl Pts',(28.265724868551,504.637546213729,-37.4050925232578)) ;
#61417 = CARTESIAN_POINT('Ctrl Pts',(28.2419642768403,504.645437098255,-37.2823237836898)) ;
#61418 = CARTESIAN_POINT('Ctrl Pts',(28.2339743448999,504.64913349586,-37.2254043310153)) ;
#61419 = CARTESIAN_POINT('Ctrl Pts',(28.2244145514327,504.656336197896,-37.1167604938927)) ;
#61420 = CARTESIAN_POINT('Ctrl Pts',(28.2222827180057,504.659819652864,-37.0651534021609)) ;
#61421 = CARTESIAN_POINT('Ctrl Pts',(28.2232610291204,504.672845454525,-36.8761851121111)) ;
#61422 = CARTESIAN_POINT('Ctrl Pts',(28.2409551547823,504.682849220847,-36.7394719751709)) ;
#61423 = CARTESIAN_POINT('Ctrl Pts',(28.2882394629522,504.696626913346,-36.5559401494667)) ;
#61424 = CARTESIAN_POINT('Ctrl Pts',(28.3036402169593,504.700404727469,-36.5060052666149)) ;
#61425 = CARTESIAN_POINT('Ctrl Pts',(28.3345189341348,504.706853537362,-36.4203990176483)) ;
#61426 = CARTESIAN_POINT('Ctrl Pts',(28.3489463634585,504.709556820619,-36.3843908914333)) ;
#61427 = CARTESIAN_POINT('Ctrl Pts',(28.3771711069419,504.714296043972,-36.3205033510563)) ;
#61428 = CARTESIAN_POINT('Ctrl Pts',(28.3905154654764,504.716353027107,-36.2924475525481)) ;
#61429 = CARTESIAN_POINT('Ctrl Pts',(28.4536846769671,504.725379129408,-36.1686838939503)) ;
#61430 = CARTESIAN_POINT('Ctrl Pts',(28.5119579065753,504.731913573759,-36.0775658859773)) ;
#61431 = CARTESIAN_POINT('Ctrl Pts',(28.6235012799821,504.742936127844,-35.9356360680403)) ;
#61432 = CARTESIAN_POINT('Ctrl Pts',(28.6720405308344,504.747379793806,-35.8815531297736)) ;
#61433 = CARTESIAN_POINT('Ctrl Pts',(28.7665271136365,504.755685187347,-35.789189751515)) ;
#61434 = CARTESIAN_POINT('Ctrl Pts',(28.8113009889449,504.759500965598,-35.7498855707174)) ;
#61435 = CARTESIAN_POINT('Ctrl Pts',(28.8976650580656,504.766737110976,-35.681904430462)) ;
#61436 = CARTESIAN_POINT('Ctrl Pts',(28.9386405089888,504.770123808217,-35.6525589211314)) ;
#61437 = CARTESIAN_POINT('Ctrl Pts',(29.0577673824255,504.779878415715,-35.5751630419295)) ;
#61438 = CARTESIAN_POINT('Ctrl Pts',(29.138636417171,504.786405515967,-35.5316496523497)) ;
#61439 = CARTESIAN_POINT('Ctrl Pts',(29.2988974047154,504.799071204943,-35.4617727015263)) ;
#61440 = CARTESIAN_POINT('Ctrl Pts',(29.377515150584,504.805169540373,-35.4342876098999)) ;
#61441 = CARTESIAN_POINT('Ctrl Pts',(29.5061494292016,504.814734545311,-35.3998648546688)) ;
#61442 = CARTESIAN_POINT('Ctrl Pts',(29.555004743805,504.818274079265,-35.3891204419165)) ;
#61443 = CARTESIAN_POINT('Ctrl Pts',(29.6333991237245,504.823734147088,-35.3755457240655)) ;
#61444 = CARTESIAN_POINT('Ctrl Pts',(29.662651257049,504.825720307625,-35.3712786297883)) ;
#61445 = CARTESIAN_POINT('Ctrl Pts',(29.7447474034344,504.831159707993,-35.3615265866565)) ;
#61446 = CARTESIAN_POINT('Ctrl Pts',(29.7977620325855,504.834526901093,-35.3577865547951)) ;
#61447 = CARTESIAN_POINT('Ctrl Pts',(29.9616519833074,504.84473567362,-35.3540811318244)) ;
#61448 = CARTESIAN_POINT('Ctrl Pts',(30.072409488731,504.851369367733,-35.3626348727482)) ;
#61449 = CARTESIAN_POINT('Ctrl Pts',(30.2525156761033,504.862693904126,-35.394808733771)) ;
#61450 = CARTESIAN_POINT('Ctrl Pts',(30.322622955803,504.867238072286,-35.4120920768919)) ;
#61451 = CARTESIAN_POINT('Ctrl Pts',(30.4158119787388,504.873599448271,-35.4415957968915)) ;
#61452 = CARTESIAN_POINT('Ctrl Pts',(30.4400537646826,504.875284228122,-35.4498907971939)) ;
#61453 = CARTESIAN_POINT('Ctrl Pts',(30.4640904938027,504.876987562729,-35.4587397597976)) ;
#61454 = CARTESIAN_POINT('Origin',(29.8885276254015,502.164639880024,-37.0221601717529)) ;
#61455 = CARTESIAN_POINT('',(29.8869092437844,504.615879743148,-34.9674106288422)) ;
#61456 = CARTESIAN_POINT('Ctrl Pts',(31.5177152521424,504.164515898581,-38.2742565096501)) ;
#61457 = CARTESIAN_POINT('Ctrl Pts',(31.5148235489527,504.164756875326,-38.2780191011651)) ;
#61458 = CARTESIAN_POINT('Ctrl Pts',(31.5119187232967,504.164997289862,-38.281771789605)) ;
#61459 = CARTESIAN_POINT('Ctrl Pts',(31.4250406485552,504.172139640842,-38.393208136478)) ;
#61460 = CARTESIAN_POINT('Ctrl Pts',(31.3305490130783,504.178599631649,-38.4922704745298)) ;
#61461 = CARTESIAN_POINT('Ctrl Pts',(31.1532930766517,504.18999601998,-38.6444370332624)) ;
#61462 = CARTESIAN_POINT('Ctrl Pts',(31.0752852035322,504.194813416355,-38.7023440114372)) ;
#61463 = CARTESIAN_POINT('Ctrl Pts',(30.949737991717,504.202532357627,-38.7824221956525)) ;
#61464 = CARTESIAN_POINT('Ctrl Pts',(30.9049538153029,504.205278060223,-38.8086558989463)) ;
#61465 = CARTESIAN_POINT('Ctrl Pts',(30.8111129902634,504.211042858654,-38.8589546317743)) ;
#61466 = CARTESIAN_POINT('Ctrl Pts',(30.7619937126592,504.214066489737,-38.8828143119784)) ;
#61467 = CARTESIAN_POINT('Ctrl Pts',(30.5800826690271,504.225303492967,-38.962386093982)) ;
#61468 = CARTESIAN_POINT('Ctrl Pts',(30.4424977051433,504.233912094998,-39.0060530827161)) ;
#61469 = CARTESIAN_POINT('Ctrl Pts',(30.197888625853,504.24893002881,-39.0562401098375)) ;
#61470 = CARTESIAN_POINT('Ctrl Pts',(30.092779254595,504.255282823913,-39.0694681919765)) ;
#61471 = CARTESIAN_POINT('Ctrl Pts',(29.9543132818391,504.263178631244,-39.0761192898812)) ;
#61472 = CARTESIAN_POINT('Ctrl Pts',(29.9214791238713,504.265015593504,-39.0769084030974)) ;
#61473 = CARTESIAN_POINT('Ctrl Pts',(29.8560888868276,504.268584680553,-39.0769119187796)) ;
#61474 = CARTESIAN_POINT('Ctrl Pts',(29.8235422794873,504.27031687866,-39.0761402520766)) ;
#61475 = CARTESIAN_POINT('Ctrl Pts',(29.6961630925704,504.276969907332,-39.0700890533033)) ;
#61476 = CARTESIAN_POINT('Ctrl Pts',(29.6017171766313,504.281631194197,-39.0590106957116)) ;
#61477 = CARTESIAN_POINT('Ctrl Pts',(29.3501804194694,504.294061759902,-39.0116551863151)) ;
#61478 = CARTESIAN_POINT('Ctrl Pts',(29.1960529846797,504.301740650502,-38.963392708511)) ;
#61479 = CARTESIAN_POINT('Ctrl Pts',(29.000576079914,504.312781599337,-38.8759051151238)) ;
#61480 = CARTESIAN_POINT('Ctrl Pts',(28.9528795596217,504.315582142882,-38.8522941201617)) ;
#61481 = CARTESIAN_POINT('Ctrl Pts',(28.8597230943665,504.321298516359,-38.8015852483557)) ;
#61482 = CARTESIAN_POINT('Ctrl Pts',(28.8142868220569,504.324211328772,-38.7745295183716)) ;
#61483 = CARTESIAN_POINT('Ctrl Pts',(28.672155293724,504.333748773588,-38.6822887597222)) ;
#61484 = CARTESIAN_POINT('Ctrl Pts',(28.5799550021247,504.340612396311,-38.6106247733197)) ;
#61485 = CARTESIAN_POINT('Ctrl Pts',(28.3906925171473,504.356054008684,-38.4358061889736)) ;
#61486 = CARTESIAN_POINT('Ctrl Pts',(28.2971796642736,504.364653587044,-38.3296465469626)) ;
#61487 = CARTESIAN_POINT('Ctrl Pts',(28.1963986426728,504.374535187488,-38.1882456950988)) ;
#61488 = CARTESIAN_POINT('Ctrl Pts',(28.1781470982285,504.376353560173,-38.1613066476604)) ;
#61489 = CARTESIAN_POINT('Ctrl Pts',(28.1427778843342,504.379918632784,-38.1063341641738)) ;
#61490 = CARTESIAN_POINT('Ctrl Pts',(28.1256770795843,504.381664176009,-38.0783010876621)) ;
#61491 = CARTESIAN_POINT('Ctrl Pts',(28.0564219140068,504.388881012845,-37.9583994939058)) ;
#61492 = CARTESIAN_POINT('Ctrl Pts',(28.0107158627895,504.394026474673,-37.8629829110937)) ;
#61493 = CARTESIAN_POINT('Ctrl Pts',(27.9205134428556,504.406123512417,-37.6301597935089)) ;
#61494 = CARTESIAN_POINT('Ctrl Pts',(27.8827489167825,504.413041687382,-37.4907663634845)) ;
#61495 = CARTESIAN_POINT('Ctrl Pts',(27.8512031161613,504.423234806284,-37.2947089638861)) ;
#61496 = CARTESIAN_POINT('Ctrl Pts',(27.8446856426347,504.426094497572,-37.2405250451073)) ;
#61497 = CARTESIAN_POINT('Ctrl Pts',(27.8361919969776,504.431809923338,-37.1344407125451)) ;
#61498 = CARTESIAN_POINT('Ctrl Pts',(27.8340118596933,504.434656792618,-37.0825979546641)) ;
#61499 = CARTESIAN_POINT('Ctrl Pts',(27.8333907404359,504.443004252779,-36.933699146649)) ;
#61500 = CARTESIAN_POINT('Ctrl Pts',(27.8398597229981,504.44865278662,-36.8367718348499)) ;
#61501 = CARTESIAN_POINT('Ctrl Pts',(27.8718630661051,504.462548232292,-36.6053613124954)) ;
#61502 = CARTESIAN_POINT('Ctrl Pts',(27.904022200339,504.470893467997,-36.4722556065769)) ;
#61503 = CARTESIAN_POINT('Ctrl Pts',(27.9643312583325,504.481562027557,-36.299957102833)) ;
#61504 = CARTESIAN_POINT('Ctrl Pts',(27.9809634875001,504.484200708119,-36.2571055145642)) ;
#61505 = CARTESIAN_POINT('Ctrl Pts',(28.0104662349016,504.488387610518,-36.1880548465334)) ;
#61506 = CARTESIAN_POINT('Ctrl Pts',(28.0224804906909,504.489978912064,-36.1615123860689)) ;
#61507 = CARTESIAN_POINT('Ctrl Pts',(28.0540773742399,504.493892480927,-36.0954825385167)) ;
#61508 = CARTESIAN_POINT('Ctrl Pts',(28.0743723871633,504.496174775951,-36.0563545557368)) ;
#61509 = CARTESIAN_POINT('Ctrl Pts',(28.1255351294484,504.501482940851,-35.9650278341757)) ;
#61510 = CARTESIAN_POINT('Ctrl Pts',(28.1574857105561,504.504464093686,-35.9134825958934)) ;
#61511 = CARTESIAN_POINT('Ctrl Pts',(28.2846566893434,504.515445262384,-35.7272530740073)) ;
#61512 = CARTESIAN_POINT('Ctrl Pts',(28.393688025964,504.523270905339,-35.602780418299)) ;
#61513 = CARTESIAN_POINT('Ctrl Pts',(28.5569189335517,504.534531985956,-35.4563454578015)) ;
#61514 = CARTESIAN_POINT('Ctrl Pts',(28.5988398778898,504.537384910656,-35.4216408142721)) ;
#61515 = CARTESIAN_POINT('Ctrl Pts',(28.6833922257485,504.543098697741,-35.357123884478)) ;
#61516 = CARTESIAN_POINT('Ctrl Pts',(28.7258760073268,504.545951287438,-35.3271859281487)) ;
#61517 = CARTESIAN_POINT('Ctrl Pts',(28.851944265802,504.554381603345,-35.2453178548258)) ;
#61518 = CARTESIAN_POINT('Ctrl Pts',(28.9381730330999,504.56011285664,-35.1977436287525)) ;
#61519 = CARTESIAN_POINT('Ctrl Pts',(29.1557118326525,504.574373885363,-35.0973410652257)) ;
#61520 = CARTESIAN_POINT('Ctrl Pts',(29.2897146013487,504.583011428528,-35.0515332237529)) ;
#61521 = CARTESIAN_POINT('Ctrl Pts',(29.4687426135226,504.593694047923,-35.010299877618)) ;
#61522 = CARTESIAN_POINT('Ctrl Pts',(29.5104182485432,504.596120142491,-35.0020524700819)) ;
#61523 = CARTESIAN_POINT('Ctrl Pts',(29.5811185464928,504.600100505977,-34.9903262099202)) ;
#61524 = CARTESIAN_POINT('Ctrl Pts',(29.6100105628021,504.601687189038,-34.9861645957613)) ;
#61525 = CARTESIAN_POINT('Ctrl Pts',(29.6715541801972,504.604988205767,-34.9786346361948)) ;
#61526 = CARTESIAN_POINT('Ctrl Pts',(29.7042143846149,504.606695294684,-34.9754303519592)) ;
#61527 = CARTESIAN_POINT('Ctrl Pts',(29.7868420118162,504.610932294638,-34.9693178657169)) ;
#61528 = CARTESIAN_POINT('Ctrl Pts',(29.8368657604163,504.613422434739,-34.9674502061277)) ;
#61529 = CARTESIAN_POINT('Ctrl Pts',(29.8869100116458,504.615880093082,-34.9674108084909)) ;
#61530 = CARTESIAN_POINT('Ctrl Pts',(29.8869092286308,504.615880054629,-34.9674108091075)) ;
#61531 = CARTESIAN_POINT('Ctrl Pts',(29.9743151528632,504.620172534274,-34.9673419649612)) ;
#61532 = CARTESIAN_POINT('Ctrl Pts',(30.061638319728,504.624361881162,-34.9728503261362)) ;
#61533 = CARTESIAN_POINT('Ctrl Pts',(30.2214344170103,504.63219255041,-34.9932197654128)) ;
#61534 = CARTESIAN_POINT('Ctrl Pts',(30.2939642411405,504.635810289608,-35.0064602112025)) ;
#61535 = CARTESIAN_POINT('Ctrl Pts',(30.425659735867,504.642647313586,-35.0378979797031)) ;
#61536 = CARTESIAN_POINT('Ctrl Pts',(30.4850155008177,504.645832003589,-35.0549264318618)) ;
#61537 = CARTESIAN_POINT('Ctrl Pts',(30.5908536792851,504.651754221207,-35.0905208552764)) ;
#61538 = CARTESIAN_POINT('Ctrl Pts',(30.6375962064229,504.654458877904,-35.108162266111)) ;
#61539 = CARTESIAN_POINT('Ctrl Pts',(30.7487274051546,504.661125615687,-35.154799658217)) ;
#61540 = CARTESIAN_POINT('Ctrl Pts',(30.8123511196922,504.665142224397,-35.185443691651)) ;
#61541 = CARTESIAN_POINT('Ctrl Pts',(31.0019409790919,504.677723377999,-35.2891045421784)) ;
#61542 = CARTESIAN_POINT('Ctrl Pts',(31.121831933475,504.686584265912,-35.3722738701345)) ;
#61543 = CARTESIAN_POINT('Ctrl Pts',(31.2838060677299,504.699342497518,-35.5122270559041)) ;
#61544 = CARTESIAN_POINT('Ctrl Pts',(31.333421582142,504.703372433043,-35.5596339402745)) ;
#61545 = CARTESIAN_POINT('Ctrl Pts',(31.401818237834,504.708999622481,-35.6318711465972)) ;
#61546 = CARTESIAN_POINT('Ctrl Pts',(31.4225531129196,504.710715619432,-35.6547837498582)) ;
#61547 = CARTESIAN_POINT('Ctrl Pts',(31.4657496508298,504.714297294096,-35.7047373248478)) ;
#61548 = CARTESIAN_POINT('Ctrl Pts',(31.4880495041329,504.716152799631,-35.7319034690109)) ;
#61549 = CARTESIAN_POINT('Ctrl Pts',(31.593358102968,504.725021404996,-35.8671219264988)) ;
#61550 = CARTESIAN_POINT('Ctrl Pts',(31.6661831868102,504.731509519045,-35.9826849514427)) ;
#61551 = CARTESIAN_POINT('Ctrl Pts',(31.778293017743,504.743681266819,-36.2073227102153)) ;
#61552 = CARTESIAN_POINT('Ctrl Pts',(31.8208504252621,504.749309037469,-36.3141357762717)) ;
#61553 = CARTESIAN_POINT('Ctrl Pts',(31.8696406631956,504.757961556692,-36.4744579849168)) ;
#61554 = CARTESIAN_POINT('Ctrl Pts',(31.8830615941412,504.760745441822,-36.5255515500389)) ;
#61555 = CARTESIAN_POINT('Ctrl Pts',(31.9060456359246,504.766471640629,-36.6291456036399)) ;
#61556 = CARTESIAN_POINT('Ctrl Pts',(31.9155617208057,504.769413009454,-36.6816144397597)) ;
#61557 = CARTESIAN_POINT('Ctrl Pts',(31.9454256999068,504.781433213952,-36.8927495277647)) ;
#61558 = CARTESIAN_POINT('Ctrl Pts',(31.9492557443054,504.791034735987,-37.0531607336239)) ;
#61559 = CARTESIAN_POINT('Ctrl Pts',(31.9256039450413,504.806389351844,-37.3075750369586)) ;
#61560 = CARTESIAN_POINT('Ctrl Pts',(31.9101157301214,504.812103960265,-37.4020628904223)) ;
#61561 = CARTESIAN_POINT('Ctrl Pts',(31.8806027134349,504.81940071634,-37.5268338033386)) ;
#61562 = CARTESIAN_POINT('Ctrl Pts',(31.8723513646039,504.82122148254,-37.5583525758758)) ;
#61563 = CARTESIAN_POINT('Ctrl Pts',(31.8542977183121,504.82478662451,-37.6211764952282)) ;
#61564 = CARTESIAN_POINT('Ctrl Pts',(31.8444884026176,504.826530000501,-37.6524698798109)) ;
#61565 = CARTESIAN_POINT('Ctrl Pts',(31.7893531194999,504.835458551802,-37.8146523877921)) ;
#61566 = CARTESIAN_POINT('Ctrl Pts',(31.7316223416336,504.842062177886,-37.94095946727)) ;
#61567 = CARTESIAN_POINT('Ctrl Pts',(31.6181486770615,504.852940150495,-38.1347277298167)) ;
#61568 = CARTESIAN_POINT('Ctrl Pts',(31.5700842716764,504.857132155032,-38.206115626978)) ;
#61569 = CARTESIAN_POINT('Ctrl Pts',(31.5177151883675,504.861461047188,-38.2742565926321)) ;
#61570 = CARTESIAN_POINT('Ctrl Pts',(31.5177152522312,504.803366924184,-38.2742565095347)) ;
#61571 = CARTESIAN_POINT('Ctrl Pts',(31.518055454289,504.803339675502,-38.27381384952)) ;
#61572 = CARTESIAN_POINT('Ctrl Pts',(31.5183954781065,504.803312429802,-38.2733710480293)) ;
#61573 = CARTESIAN_POINT('Ctrl Pts',(31.6278180883491,504.794540871479,-38.1307533994567)) ;
#61574 = CARTESIAN_POINT('Ctrl Pts',(31.7178262718211,504.786071609238,-37.9749324629393)) ;
#61575 = CARTESIAN_POINT('Ctrl Pts',(31.8064571919854,504.774108590257,-37.7612553613457)) ;
#61576 = CARTESIAN_POINT('Ctrl Pts',(31.8245903385251,504.771356396023,-37.7123601691067)) ;
#61577 = CARTESIAN_POINT('Ctrl Pts',(31.8574845436478,504.76565699939,-37.6121216766635)) ;
#61578 = CARTESIAN_POINT('Ctrl Pts',(31.8721420816032,504.762708888452,-37.5607869959292)) ;
#61579 = CARTESIAN_POINT('Ctrl Pts',(31.9135740012181,504.752839934177,-37.3908781454159)) ;
#61580 = CARTESIAN_POINT('Ctrl Pts',(31.931829461122,504.745656491413,-37.2705072137826)) ;
#61581 = CARTESIAN_POINT('Ctrl Pts',(31.9473741596984,504.73057002732,-37.0196557489838)) ;
#61582 = CARTESIAN_POINT('Ctrl Pts',(31.9431040933741,504.722686426204,-36.8895910022409)) ;
#61583 = CARTESIAN_POINT('Ctrl Pts',(31.9223320987491,504.713364966716,-36.7276168785901)) ;
#61584 = CARTESIAN_POINT('Ctrl Pts',(31.9172675922358,504.711489515848,-36.6945463286282)) ;
#61585 = CARTESIAN_POINT('Ctrl Pts',(31.9058501141434,504.707930362346,-36.6304880935951)) ;
#61586 = CARTESIAN_POINT('Ctrl Pts',(31.8995849282361,504.706243281743,-36.5994951572382)) ;
#61587 = CARTESIAN_POINT('Ctrl Pts',(31.8751326170149,504.700446169061,-36.4914375426429)) ;
#61588 = CARTESIAN_POINT('Ctrl Pts',(31.8532082194561,504.696511771494,-36.4152843082838)) ;
#61589 = CARTESIAN_POINT('Ctrl Pts',(31.7658565660364,504.683639719898,-36.1668560123068)) ;
#61590 = CARTESIAN_POINT('Ctrl Pts',(31.6817022353868,504.674959848809,-36.0021439832749)) ;
#61591 = CARTESIAN_POINT('Ctrl Pts',(31.5471179687585,504.662740588675,-35.8081693594873)) ;
#61592 = CARTESIAN_POINT('Ctrl Pts',(31.5159023175279,504.659996309372,-35.7666337562143)) ;
#61593 = CARTESIAN_POINT('Ctrl Pts',(31.4493226785199,504.654288909477,-35.6847024350061)) ;
#61594 = CARTESIAN_POINT('Ctrl Pts',(31.4138826545651,504.651323752432,-35.6444208412975)) ;
#61595 = CARTESIAN_POINT('Ctrl Pts',(31.3306339529066,504.644504095972,-35.5569528916296)) ;
#61596 = CARTESIAN_POINT('Ctrl Pts',(31.2820073201595,504.640616945316,-35.5106324505666)) ;
#61597 = CARTESIAN_POINT('Ctrl Pts',(31.1289495665657,504.628696319042,-35.3785060219119)) ;
#61598 = CARTESIAN_POINT('Ctrl Pts',(31.0182463937016,504.620457396717,-35.3005394412097)) ;
#61599 = CARTESIAN_POINT('Ctrl Pts',(30.8488917454572,504.608925125323,-35.204677817596)) ;
#61600 = CARTESIAN_POINT('Ctrl Pts',(30.7958312837281,504.605452863158,-35.1776161687232)) ;
#61601 = CARTESIAN_POINT('Ctrl Pts',(30.7144288796586,504.600411297327,-35.1404638333113)) ;
#61602 = CARTESIAN_POINT('Ctrl Pts',(30.6869204004802,504.598755356804,-35.1286281849115)) ;
#61603 = CARTESIAN_POINT('Ctrl Pts',(30.6252205371183,504.595158362591,-35.1036655864817)) ;
#61604 = CARTESIAN_POINT('Ctrl Pts',(30.5909188484938,504.593233448648,-35.0908433033592)) ;
#61605 = CARTESIAN_POINT('Ctrl Pts',(30.5132768639043,504.58900425143,-35.0641625676601)) ;
#61606 = CARTESIAN_POINT('Ctrl Pts',(30.4697818309885,504.586722099753,-35.0508128627286)) ;
#61607 = CARTESIAN_POINT('Ctrl Pts',(30.3102779048337,504.578551617017,-35.0075960671411)) ;
#61608 = CARTESIAN_POINT('Ctrl Pts',(30.1921591688437,504.572863673324,-34.9864412659003)) ;
#61609 = CARTESIAN_POINT('Ctrl Pts',(29.9835043897067,504.562604900725,-34.9676462385594)) ;
#61610 = CARTESIAN_POINT('Ctrl Pts',(29.8937183611511,504.558125843547,-34.965459190854)) ;
#61611 = CARTESIAN_POINT('Ctrl Pts',(29.7530225855961,504.550810306761,-34.971246375075)) ;
#61612 = CARTESIAN_POINT('Ctrl Pts',(29.7020629906538,504.548100485852,-34.9752504693354)) ;
#61613 = CARTESIAN_POINT('Ctrl Pts',(29.596698643478,504.542347393465,-34.9874965832376)) ;
#61614 = CARTESIAN_POINT('Ctrl Pts',(29.5423698634712,504.539296670944,-34.9960323250186)) ;
#61615 = CARTESIAN_POINT('Ctrl Pts',(29.3750845272703,504.529626961228,-35.0292396050918)) ;
#61616 = CARTESIAN_POINT('Ctrl Pts',(29.2638314811684,504.522785926783,-35.061266247792)) ;
#61617 = CARTESIAN_POINT('Ctrl Pts',(29.0350649430583,504.508087502773,-35.1485755269603)) ;
#61618 = CARTESIAN_POINT('Ctrl Pts',(28.9188728071577,504.500237696303,-35.2059852861536)) ;
#61619 = CARTESIAN_POINT('Ctrl Pts',(28.7803530824693,504.490943534214,-35.2915336865619)) ;
#61620 = CARTESIAN_POINT('Ctrl Pts',(28.7522952996634,504.489065841819,-35.3098239759593)) ;
#61621 = CARTESIAN_POINT('Ctrl Pts',(28.6986673940265,504.48550611848,-35.346681835444)) ;
#61622 = CARTESIAN_POINT('Ctrl Pts',(28.6730544150619,504.483820562522,-35.3651689085796)) ;
#61623 = CARTESIAN_POINT('Ctrl Pts',(28.5851449218539,504.478049445089,-35.4317563831467)) ;
#61624 = CARTESIAN_POINT('Ctrl Pts',(28.5251886937477,504.47413725332,-35.4828421873308)) ;
#61625 = CARTESIAN_POINT('Ctrl Pts',(28.3345871126536,504.461242576263,-35.6651398318796)) ;
#61626 = CARTESIAN_POINT('Ctrl Pts',(28.2187641410032,504.452525603814,-35.8104983358359)) ;
#61627 = CARTESIAN_POINT('Ctrl Pts',(28.0973544399116,504.440259969451,-36.0139969402947)) ;
#61628 = CARTESIAN_POINT('Ctrl Pts',(28.0724490295943,504.437515996184,-36.0595842707441)) ;
#61629 = CARTESIAN_POINT('Ctrl Pts',(28.0253561422967,504.431805206114,-36.1541317303312)) ;
#61630 = CARTESIAN_POINT('Ctrl Pts',(28.0033093359974,504.428836168213,-36.2031164721737)) ;
#61631 = CARTESIAN_POINT('Ctrl Pts',(27.9580771506564,504.422012024509,-36.3151493027802)) ;
#61632 = CARTESIAN_POINT('Ctrl Pts',(27.9360140165513,504.418124462712,-36.3785821329784)) ;
#61633 = CARTESIAN_POINT('Ctrl Pts',(27.8788522900084,504.406168821206,-36.5731498245496)) ;
#61634 = CARTESIAN_POINT('Ctrl Pts',(27.853598022308,504.397893463499,-36.7067815836235)) ;
#61635 = CARTESIAN_POINT('Ctrl Pts',(27.8365293408457,504.386369138365,-36.9006179389331)) ;
#61636 = CARTESIAN_POINT('Ctrl Pts',(27.8338874974816,504.38293466512,-36.9595139539795)) ;
#61637 = CARTESIAN_POINT('Ctrl Pts',(27.8337274547556,504.377947841857,-37.0480613630741)) ;
#61638 = CARTESIAN_POINT('Ctrl Pts',(27.8343141637769,504.376310370602,-37.0776765652497)) ;
#61639 = CARTESIAN_POINT('Ctrl Pts',(27.8370603179552,504.372727553615,-37.14391591728)) ;
#61640 = CARTESIAN_POINT('Ctrl Pts',(27.8395603316326,504.370799329269,-37.1805140851523)) ;
#61641 = CARTESIAN_POINT('Ctrl Pts',(27.8473627635365,504.366561213734,-37.2624146340991)) ;
#61642 = CARTESIAN_POINT('Ctrl Pts',(27.8531962550742,504.364273560524,-37.3076472120647)) ;
#61643 = CARTESIAN_POINT('Ctrl Pts',(27.8799175670082,504.356059128149,-37.4716180204413)) ;
#61644 = CARTESIAN_POINT('Ctrl Pts',(27.9097359245385,504.350334210273,-37.5886510114655)) ;
#61645 = CARTESIAN_POINT('Ctrl Pts',(27.9790501523618,504.340073501606,-37.7862176954731)) ;
#61646 = CARTESIAN_POINT('Ctrl Pts',(28.0138591111613,504.335635127387,-37.8680348136569)) ;
#61647 = CARTESIAN_POINT('Ctrl Pts',(28.0768311937259,504.328365975392,-37.9929117547693)) ;
#61648 = CARTESIAN_POINT('Ctrl Pts',(28.1015008840197,504.325658279698,-38.037609528763)) ;
#61649 = CARTESIAN_POINT('Ctrl Pts',(28.1562403639933,504.319896474891,-38.1286053015315)) ;
#61650 = CARTESIAN_POINT('Ctrl Pts',(28.1865626300446,504.316834308049,-38.1747027098842)) ;
#61651 = CARTESIAN_POINT('Ctrl Pts',(28.2870125577057,504.307056071724,-38.3147890656886)) ;
#61652 = CARTESIAN_POINT('Ctrl Pts',(28.3633438674579,504.300110143312,-38.4040242422746)) ;
#61653 = CARTESIAN_POINT('Ctrl Pts',(28.5371863629811,504.285457836782,-38.5752042210906)) ;
#61654 = CARTESIAN_POINT('Ctrl Pts',(28.6355603256371,504.277767426526,-38.6556061117652)) ;
#61655 = CARTESIAN_POINT('Ctrl Pts',(28.7686590801501,504.268600732772,-38.7452465046634)) ;
#61656 = CARTESIAN_POINT('Ctrl Pts',(28.7970566316433,504.266710787157,-38.7633733810208)) ;
#61657 = CARTESIAN_POINT('Ctrl Pts',(28.8526763420077,504.263153847954,-38.7969810758505)) ;
#61658 = CARTESIAN_POINT('Ctrl Pts',(28.8798308692204,504.261482306544,-38.8125534513021)) ;
#61659 = CARTESIAN_POINT('Ctrl Pts',(28.9736421709229,504.255890950561,-38.8635395831377)) ;
#61660 = CARTESIAN_POINT('Ctrl Pts',(29.041894354526,504.25212994789,-38.8959017889211)) ;
#61661 = CARTESIAN_POINT('Ctrl Pts',(29.248364237253,504.241210692672,-38.9802088696638)) ;
#61662 = CARTESIAN_POINT('Ctrl Pts',(29.3905556206666,504.234238383345,-39.0211069554706)) ;
#61663 = CARTESIAN_POINT('Ctrl Pts',(29.5999831926082,504.223573199036,-39.0575890228591)) ;
#61664 = CARTESIAN_POINT('Ctrl Pts',(29.6645527094485,504.220238474504,-39.0657018596547)) ;
#61665 = CARTESIAN_POINT('Ctrl Pts',(29.7785069944165,504.214205655444,-39.074553801887)) ;
#61666 = CARTESIAN_POINT('Ctrl Pts',(29.8277374144049,504.211551793415,-39.0766012432058)) ;
#61667 = CARTESIAN_POINT('Ctrl Pts',(29.9413063160695,504.205301172694,-39.077238892392)) ;
#61668 = CARTESIAN_POINT('Ctrl Pts',(30.0055972247018,504.201667030928,-39.0745800969795)) ;
#61669 = CARTESIAN_POINT('Ctrl Pts',(30.1489717595916,504.193348731315,-39.061892298022)) ;
#61670 = CARTESIAN_POINT('Ctrl Pts',(30.2278094507371,504.188626390787,-39.0502687459828)) ;
#61671 = CARTESIAN_POINT('Ctrl Pts',(30.4381553867794,504.175744078493,-39.0066467437805)) ;
#61672 = CARTESIAN_POINT('Ctrl Pts',(30.5675134413197,504.167500694065,-38.9661917702435)) ;
#61673 = CARTESIAN_POINT('Ctrl Pts',(30.7243120763826,504.157724969001,-38.8995778782788)) ;
#61674 = CARTESIAN_POINT('Ctrl Pts',(30.7563054070292,504.155743969045,-38.8850060993159)) ;
#61675 = CARTESIAN_POINT('Ctrl Pts',(30.8155589582394,504.152122661215,-38.856160179725)) ;
#61676 = CARTESIAN_POINT('Ctrl Pts',(30.8429013725043,504.150472955122,-38.842081583614)) ;
#61677 = CARTESIAN_POINT('Ctrl Pts',(30.9285457798979,504.145344093845,-38.795522179738)) ;
#61678 = CARTESIAN_POINT('Ctrl Pts',(30.9855909658659,504.141984230631,-38.7608102471607)) ;
#61679 = CARTESIAN_POINT('Ctrl Pts',(31.1866293936743,504.129992369155,-38.6246368304838)) ;
#61680 = CARTESIAN_POINT('Ctrl Pts',(31.3191086112689,504.12172427263,-38.5075692674377)) ;
#61681 = CARTESIAN_POINT('Ctrl Pts',(31.4636786648758,504.110543446074,-38.3423072292991)) ;
#61682 = CARTESIAN_POINT('Ctrl Pts',(31.4912659857281,504.1082936835,-38.3086742357782)) ;
#61683 = CARTESIAN_POINT('Ctrl Pts',(31.5177642178171,504.106001566445,-38.2741927945048)) ;
#61684 = CARTESIAN_POINT('Origin',(179.888527625402,502.164639879998,-37.0221601717597)) ;
#61685 = CARTESIAN_POINT('Ctrl Pts',(181.517728902313,504.164526607599,-38.2742387482923)) ;
#61686 = CARTESIAN_POINT('Ctrl Pts',(181.440913164261,504.170928309153,-38.374191180086)) ;
#61687 = CARTESIAN_POINT('Ctrl Pts',(181.35506384574,504.176928754324,-38.4668625482387)) ;
#61688 = CARTESIAN_POINT('Ctrl Pts',(181.204907912824,504.186728917933,-38.6016770715163)) ;
#61689 = CARTESIAN_POINT('Ctrl Pts',(181.145816360762,504.190439335762,-38.6491066326943)) ;
#61690 = CARTESIAN_POINT('Ctrl Pts',(181.033260293955,504.197417411237,-38.7296481294601)) ;
#61691 = CARTESIAN_POINT('Ctrl Pts',(180.980636552643,504.200647192836,-38.7637758254983)) ;
#61692 = CARTESIAN_POINT('Ctrl Pts',(180.883452293891,504.206612952502,-38.8206637034777)) ;
#61693 = CARTESIAN_POINT('Ctrl Pts',(180.839464486277,504.209313228368,-38.8443041082496)) ;
#61694 = CARTESIAN_POINT('Ctrl Pts',(180.73251015871,504.215897768503,-38.8968565464999)) ;
#61695 = CARTESIAN_POINT('Ctrl Pts',(180.66886019815,504.219832450438,-38.9242307549692)) ;
#61696 = CARTESIAN_POINT('Ctrl Pts',(180.465331173095,504.232453396912,-38.999826165136)) ;
#61697 = CARTESIAN_POINT('Ctrl Pts',(180.321560766012,504.241459026997,-39.0361959147464)) ;
#61698 = CARTESIAN_POINT('Ctrl Pts',(180.106812157454,504.254388550514,-39.0664480224822)) ;
#61699 = CARTESIAN_POINT('Ctrl Pts',(180.038021849696,504.258446141896,-39.072626955555)) ;
#61700 = CARTESIAN_POINT('Ctrl Pts',(179.938131845848,504.2641020352,-39.0765442973059)) ;
#61701 = CARTESIAN_POINT('Ctrl Pts',(179.907191208821,504.265820788362,-39.0770584195075)) ;
#61702 = CARTESIAN_POINT('Ctrl Pts',(179.841166522842,504.269402347307,-39.0766638041493)) ;
#61703 = CARTESIAN_POINT('Ctrl Pts',(179.806094792212,504.271255225189,-39.0755557500163)) ;
#61704 = CARTESIAN_POINT('Ctrl Pts',(179.634610612812,504.280145333299,-39.0657366804744)) ;
#61705 = CARTESIAN_POINT('Ctrl Pts',(179.499260612516,504.286653222637,-39.0443267796173)) ;
#61706 = CARTESIAN_POINT('Ctrl Pts',(179.256309646013,504.298832240622,-38.9805781054524)) ;
#61707 = CARTESIAN_POINT('Ctrl Pts',(179.148219145409,504.304445777928,-38.9423269265333)) ;
#61708 = CARTESIAN_POINT('Ctrl Pts',(178.99575486251,504.31308179847,-38.8735763113426)) ;
#61709 = CARTESIAN_POINT('Ctrl Pts',(178.948483943041,504.315865097047,-38.8500283632146)) ;
#61710 = CARTESIAN_POINT('Ctrl Pts',(178.855395438623,504.32159179624,-38.7990898285438)) ;
#61711 = CARTESIAN_POINT('Ctrl Pts',(178.809633831471,504.324534331084,-38.7716825485577)) ;
#61712 = CARTESIAN_POINT('Ctrl Pts',(178.661238632831,504.334526305746,-38.6747688768215)) ;
#61713 = CARTESIAN_POINT('Ctrl Pts',(178.563840814428,504.341853162214,-38.5977715028224)) ;
#61714 = CARTESIAN_POINT('Ctrl Pts',(178.393637076305,504.355943085441,-38.4362220257068)) ;
#61715 = CARTESIAN_POINT('Ctrl Pts',(178.319587058913,504.362655105734,-38.3535864992456)) ;
#61716 = CARTESIAN_POINT('Ctrl Pts',(178.227362585419,504.371507105705,-38.2322272324966)) ;
#61717 = CARTESIAN_POINT('Ctrl Pts',(178.203179249806,504.373882736117,-38.1983119214529)) ;
#61718 = CARTESIAN_POINT('Ctrl Pts',(178.163793444985,504.377816283238,-38.1393642562015)) ;
#61719 = CARTESIAN_POINT('Ctrl Pts',(178.148067727621,504.379404068034,-38.1147041890701)) ;
#61720 = CARTESIAN_POINT('Ctrl Pts',(178.107364097086,504.383570437789,-38.0477645233996)) ;
#61721 = CARTESIAN_POINT('Ctrl Pts',(178.083366678306,504.386092698709,-38.004912672078)) ;
#61722 = CARTESIAN_POINT('Ctrl Pts',(177.998025423101,504.395483358698,-37.8388246028883)) ;
#61723 = CARTESIAN_POINT('Ctrl Pts',(177.947579870272,504.401985048399,-37.7103940374137)) ;
#61724 = CARTESIAN_POINT('Ctrl Pts',(177.885351094748,504.413236022972,-37.4888796374843)) ;
#61725 = CARTESIAN_POINT('Ctrl Pts',(177.866386046882,504.417841610328,-37.3983042318141)) ;
#61726 = CARTESIAN_POINT('Ctrl Pts',(177.846441135689,504.425316724334,-37.2556966914539)) ;
#61727 = CARTESIAN_POINT('Ctrl Pts',(177.841224186185,504.428049352477,-37.2043812530813)) ;
#61728 = CARTESIAN_POINT('Ctrl Pts',(177.834432741539,504.433834770224,-37.0978828472443)) ;
#61729 = CARTESIAN_POINT('Ctrl Pts',(177.833140556721,504.436894316832,-37.0427242136307)) ;
#61730 = CARTESIAN_POINT('Ctrl Pts',(177.836718001565,504.448944858561,-36.8301591850571)) ;
#61731 = CARTESIAN_POINT('Ctrl Pts',(177.857452810433,504.458423953639,-36.6735797595066)) ;
#61732 = CARTESIAN_POINT('Ctrl Pts',(177.911263524934,504.471671538578,-36.4596503776431)) ;
#61733 = CARTESIAN_POINT('Ctrl Pts',(177.929497424505,504.475447271999,-36.3991096166263)) ;
#61734 = CARTESIAN_POINT('Ctrl Pts',(177.9655117281,504.481775975183,-36.2968665391766)) ;
#61735 = CARTESIAN_POINT('Ctrl Pts',(177.981934223607,504.484369062807,-36.2547338184999)) ;
#61736 = CARTESIAN_POINT('Ctrl Pts',(178.011205183651,504.488511203235,-36.1863929626504)) ;
#61737 = CARTESIAN_POINT('Ctrl Pts',(178.023243498962,504.490101032807,-36.1598599183415)) ;
#61738 = CARTESIAN_POINT('Ctrl Pts',(178.05521750411,504.494050632914,-36.0931938066943)) ;
#61739 = CARTESIAN_POINT('Ctrl Pts',(178.075908005558,504.496368083601,-36.0534418427131)) ;
#61740 = CARTESIAN_POINT('Ctrl Pts',(178.164605420021,504.50552645065,-35.8958400356843)) ;
#61741 = CARTESIAN_POINT('Ctrl Pts',(178.242940964506,504.511965062077,-35.784196219905)) ;
#61742 = CARTESIAN_POINT('Ctrl Pts',(178.396348330988,504.523419415139,-35.6061102895555)) ;
#61743 = CARTESIAN_POINT('Ctrl Pts',(178.466284305852,504.528325858958,-35.535883756918)) ;
#61744 = CARTESIAN_POINT('Ctrl Pts',(178.580267068193,504.536147179058,-35.4368662155772)) ;
#61745 = CARTESIAN_POINT('Ctrl Pts',(178.620809020646,504.538897663563,-35.4042629262864)) ;
#61746 = CARTESIAN_POINT('Ctrl Pts',(178.706171672828,504.544653910776,-35.3407953024403)) ;
#61747 = CARTESIAN_POINT('Ctrl Pts',(178.751068485251,504.54766335062,-35.3101031261099)) ;
#61748 = CARTESIAN_POINT('Ctrl Pts',(178.937276180553,504.560093262962,-35.1933683108459)) ;
#61749 = CARTESIAN_POINT('Ctrl Pts',(179.087505572358,504.570071373715,-35.1227638647846)) ;
#61750 = CARTESIAN_POINT('Ctrl Pts',(179.32708243113,504.585209454714,-35.0436929019299)) ;
#61751 = CARTESIAN_POINT('Ctrl Pts',(179.411280315052,504.59037977148,-35.021712479621)) ;
#61752 = CARTESIAN_POINT('Ctrl Pts',(179.528230841388,504.597151750432,-34.9989892605366)) ;
#61753 = CARTESIAN_POINT('Ctrl Pts',(179.559980876531,504.59894931193,-34.9935912971791)) ;
#61754 = CARTESIAN_POINT('Ctrl Pts',(179.62474426433,504.602514977737,-34.984141241318)) ;
#61755 = CARTESIAN_POINT('Ctrl Pts',(179.657755137529,504.604280277299,-34.9801398079141)) ;
#61756 = CARTESIAN_POINT('Ctrl Pts',(179.823917863895,504.612969092488,-34.9640796485024)) ;
#61757 = CARTESIAN_POINT('Ctrl Pts',(179.957937769981,504.619359703623,-34.9642340272171)) ;
#61758 = CARTESIAN_POINT('Ctrl Pts',(180.173504743855,504.629850002885,-34.9855800162206)) ;
#61759 = CARTESIAN_POINT('Ctrl Pts',(180.255432393552,504.633884390789,-34.9987347141687)) ;
#61760 = CARTESIAN_POINT('Ctrl Pts',(180.400696273933,504.641348689964,-35.0311731383869)) ;
#61761 = CARTESIAN_POINT('Ctrl Pts',(180.464320305686,504.644728187107,-35.0486334452597)) ;
#61762 = CARTESIAN_POINT('Ctrl Pts',(180.574351535492,504.650837753467,-35.0846035066313)) ;
#61763 = CARTESIAN_POINT('Ctrl Pts',(180.621129735626,504.653522249129,-35.1018024419299)) ;
#61764 = CARTESIAN_POINT('Ctrl Pts',(180.727697206733,504.659861336601,-35.1454447190358)) ;
#61765 = CARTESIAN_POINT('Ctrl Pts',(180.786939439681,504.663554778688,-35.1730735488531)) ;
#61766 = CARTESIAN_POINT('Ctrl Pts',(180.978470201232,504.676066557894,-35.2737771131301)) ;
#61767 = CARTESIAN_POINT('Ctrl Pts',(181.104010017504,504.685251276406,-35.3586062399055)) ;
#61768 = CARTESIAN_POINT('Ctrl Pts',(181.274653865825,504.698626313589,-35.5036192872005)) ;
#61769 = CARTESIAN_POINT('Ctrl Pts',(181.327659970123,504.702924288147,-35.5537555068308)) ;
#61770 = CARTESIAN_POINT('Ctrl Pts',(181.399429990766,504.708826035816,-35.6292678656424)) ;
#61771 = CARTESIAN_POINT('Ctrl Pts',(181.42044973339,504.710565262194,-35.6524193208363)) ;
#61772 = CARTESIAN_POINT('Ctrl Pts',(181.463553326009,504.714138602677,-35.7021285112233)) ;
#61773 = CARTESIAN_POINT('Ctrl Pts',(181.48551199562,504.715964875973,-35.7287805774248)) ;
#61774 = CARTESIAN_POINT('Ctrl Pts',(181.593731484256,504.72506888717,-35.8670917293213)) ;
#61775 = CARTESIAN_POINT('Ctrl Pts',(181.669006722605,504.731772047075,-35.9868794797552)) ;
#61776 = CARTESIAN_POINT('Ctrl Pts',(181.780072730742,504.743955363404,-36.212123658951)) ;
#61777 = CARTESIAN_POINT('Ctrl Pts',(181.820721975699,504.749357624635,-36.3145416644425)) ;
#61778 = CARTESIAN_POINT('Ctrl Pts',(181.868557806522,504.757771508443,-36.4705239191078)) ;
#61779 = CARTESIAN_POINT('Ctrl Pts',(181.882161842062,504.760569876128,-36.5219162361649)) ;
#61780 = CARTESIAN_POINT('Ctrl Pts',(181.905323977497,504.766292051518,-36.6255000310409)) ;
#61781 = CARTESIAN_POINT('Ctrl Pts',(181.914883514516,504.769213319355,-36.6776491231629)) ;
#61782 = CARTESIAN_POINT('Ctrl Pts',(181.939492009862,504.77896197232,-36.8490247851047)) ;
#61783 = CARTESIAN_POINT('Ctrl Pts',(181.946103516199,504.786047048548,-36.9691959949358)) ;
#61784 = CARTESIAN_POINT('Ctrl Pts',(181.937761955812,504.80137204501,-37.2245696335507)) ;
#61785 = CARTESIAN_POINT('Ctrl Pts',(181.919975887731,504.809608289459,-37.3591359994321)) ;
#61786 = CARTESIAN_POINT('Ctrl Pts',(181.881529340343,504.819212584416,-37.5231957434927)) ;
#61787 = CARTESIAN_POINT('Ctrl Pts',(181.873201881488,504.821064985777,-37.5552275842933)) ;
#61788 = CARTESIAN_POINT('Ctrl Pts',(181.855220564076,504.824637147744,-37.6181136416478)) ;
#61789 = CARTESIAN_POINT('Ctrl Pts',(181.84560527541,504.826358000672,-37.6489687073554)) ;
#61790 = CARTESIAN_POINT('Ctrl Pts',(181.80667823877,504.832710206947,-37.7642376514148)) ;
#61791 = CARTESIAN_POINT('Ctrl Pts',(181.772596783725,504.837113637798,-37.8469432779841)) ;
#61792 = CARTESIAN_POINT('Ctrl Pts',(181.67307874025,504.848105449872,-38.0497930125789)) ;
#61793 = CARTESIAN_POINT('Ctrl Pts',(181.600877032597,504.854608447747,-38.1660466247542)) ;
#61794 = CARTESIAN_POINT('Ctrl Pts',(181.517728902317,504.861481368308,-38.2742387482878)) ;
#61795 = CARTESIAN_POINT('Ctrl Pts',(181.517728902323,504.803342258844,-38.2742387482803)) ;
#61796 = CARTESIAN_POINT('Ctrl Pts',(181.518028016694,504.803318300742,-38.2738495414643)) ;
#61797 = CARTESIAN_POINT('Ctrl Pts',(181.518326993276,504.803294344944,-38.2734602252776)) ;
#61798 = CARTESIAN_POINT('Ctrl Pts',(181.627767714738,504.794522084801,-38.1308448219171)) ;
#61799 = CARTESIAN_POINT('Ctrl Pts',(181.717819695322,504.786049499824,-37.9749595168889)) ;
#61800 = CARTESIAN_POINT('Ctrl Pts',(181.806476315796,504.774082118455,-37.7612059974817)) ;
#61801 = CARTESIAN_POINT('Ctrl Pts',(181.824609459599,504.771329674729,-37.7123068130391)) ;
#61802 = CARTESIAN_POINT('Ctrl Pts',(181.857506971475,504.765629080746,-37.6120482968176)) ;
#61803 = CARTESIAN_POINT('Ctrl Pts',(181.872166873395,504.762679991535,-37.5606973031445)) ;
#61804 = CARTESIAN_POINT('Ctrl Pts',(181.913635425447,504.752799861929,-37.3905989044251)) ;
#61805 = CARTESIAN_POINT('Ctrl Pts',(181.931895584619,504.745605303935,-37.2700491280813)) ;
#61806 = CARTESIAN_POINT('Ctrl Pts',(181.947356611009,504.730523974722,-37.0192871434651)) ;
#61807 = CARTESIAN_POINT('Ctrl Pts',(181.94308082157,504.722657547747,-36.889495447667)) ;
#61808 = CARTESIAN_POINT('Ctrl Pts',(181.922353731829,504.713349563908,-36.7277634461602)) ;
#61809 = CARTESIAN_POINT('Ctrl Pts',(181.917287616793,504.711472599095,-36.6946677947558)) ;
#61810 = CARTESIAN_POINT('Ctrl Pts',(181.905870401056,504.707912402934,-36.6305933326396)) ;
#61811 = CARTESIAN_POINT('Ctrl Pts',(181.899608710014,504.706225719172,-36.5996090117794)) ;
#61812 = CARTESIAN_POINT('Ctrl Pts',(181.875203730563,504.70043796528,-36.4917299682928)) ;
#61813 = CARTESIAN_POINT('Ctrl Pts',(181.853342369544,504.696511686355,-36.4157416647703)) ;
#61814 = CARTESIAN_POINT('Ctrl Pts',(181.766032252826,504.683632891777,-36.1671796841624)) ;
#61815 = CARTESIAN_POINT('Ctrl Pts',(181.681762985447,504.674940800863,-36.0021987516026)) ;
#61816 = CARTESIAN_POINT('Ctrl Pts',(181.546996452941,504.662706166569,-35.8080034781573)) ;
#61817 = CARTESIAN_POINT('Ctrl Pts',(181.515778358693,504.659961892883,-35.7664732167796)) ;
#61818 = CARTESIAN_POINT('Ctrl Pts',(181.449173072119,504.654252700115,-35.6845266298854)) ;
#61819 = CARTESIAN_POINT('Ctrl Pts',(181.413707839674,504.651285662178,-35.6442261211981)) ;
#61820 = CARTESIAN_POINT('Ctrl Pts',(181.330426191572,504.644463889159,-35.5567484845012)) ;
#61821 = CARTESIAN_POINT('Ctrl Pts',(181.281793787348,504.640576592862,-35.5104356700513)) ;
#61822 = CARTESIAN_POINT('Ctrl Pts',(181.12853432545,504.628641293187,-35.3781727513209)) ;
#61823 = CARTESIAN_POINT('Ctrl Pts',(181.017606262631,504.620387003001,-35.30010048392)) ;
#61824 = CARTESIAN_POINT('Ctrl Pts',(180.848201149098,504.608856792096,-35.2043208977969)) ;
#61825 = CARTESIAN_POINT('Ctrl Pts',(180.79534571144,504.6053993151,-35.1773851168643)) ;
#61826 = CARTESIAN_POINT('Ctrl Pts',(180.714440195643,504.600389570668,-35.1404737476219)) ;
#61827 = CARTESIAN_POINT('Ctrl Pts',(180.687219932894,504.598750833435,-35.1287594286665)) ;
#61828 = CARTESIAN_POINT('Ctrl Pts',(180.625958612455,504.595177921618,-35.103952062463)) ;
#61829 = CARTESIAN_POINT('Ctrl Pts',(180.591804811688,504.593260290426,-35.0911686224346)) ;
#61830 = CARTESIAN_POINT('Ctrl Pts',(180.514592305773,504.589052083592,-35.0645894294843)) ;
#61831 = CARTESIAN_POINT('Ctrl Pts',(180.471381841536,504.586783267168,-35.0512919397479)) ;
#61832 = CARTESIAN_POINT('Ctrl Pts',(180.314100324172,504.578721260657,-35.0085164763534)) ;
#61833 = CARTESIAN_POINT('Ctrl Pts',(180.197984746224,504.573123677812,-34.9874338794217)) ;
#61834 = CARTESIAN_POINT('Ctrl Pts',(179.989562315985,504.562884367147,-34.9678552236461)) ;
#61835 = CARTESIAN_POINT('Ctrl Pts',(179.897963378539,504.558321740006,-34.9653943885215)) ;
#61836 = CARTESIAN_POINT('Ctrl Pts',(179.755301446587,504.550909531777,-34.9710933981785)) ;
#61837 = CARTESIAN_POINT('Ctrl Pts',(179.704190277625,504.548193738326,-34.9750541082729)) ;
#61838 = CARTESIAN_POINT('Ctrl Pts',(179.598916875681,504.54244972914,-34.9871864247966)) ;
#61839 = CARTESIAN_POINT('Ctrl Pts',(179.544826574092,504.539415056052,-34.9956209271563)) ;
#61840 = CARTESIAN_POINT('Ctrl Pts',(179.425441148235,504.53252098311,-35.019154271756)) ;
#61841 = CARTESIAN_POINT('Ctrl Pts',(179.360419218725,504.528632480622,-35.0353079012343)) ;
#61842 = CARTESIAN_POINT('Ctrl Pts',(179.156270978218,504.516039286217,-35.0967552175052)) ;
#61843 = CARTESIAN_POINT('Ctrl Pts',(179.021144422686,504.507088525318,-35.1537309963188)) ;
#61844 = CARTESIAN_POINT('Ctrl Pts',(178.849805901742,504.495589521322,-35.2485997198334)) ;
#61845 = CARTESIAN_POINT('Ctrl Pts',(178.807279082472,504.492725907566,-35.2742008342211)) ;
#61846 = CARTESIAN_POINT('Ctrl Pts',(178.74132796563,504.48831890564,-35.3172324231881)) ;
#61847 = CARTESIAN_POINT('Ctrl Pts',(178.717278624554,504.486720843645,-35.3336632704159)) ;
#61848 = CARTESIAN_POINT('Ctrl Pts',(178.660466362811,504.482972048318,-35.3742766086214)) ;
#61849 = CARTESIAN_POINT('Ctrl Pts',(178.628058559032,504.48085094912,-35.3989310153388)) ;
#61850 = CARTESIAN_POINT('Ctrl Pts',(178.510467902888,504.473133906769,-35.4940357445329)) ;
#61851 = CARTESIAN_POINT('Ctrl Pts',(178.430274201759,504.467821699576,-35.5703634924208)) ;
#61852 = CARTESIAN_POINT('Ctrl Pts',(178.27277520858,504.45638458646,-35.7465568457832)) ;
#61853 = CARTESIAN_POINT('Ctrl Pts',(178.197738689864,504.450263196797,-35.8478310884731)) ;
#61854 = CARTESIAN_POINT('Ctrl Pts',(178.104869142975,504.44104583485,-36.0007007918042)) ;
#61855 = CARTESIAN_POINT('Ctrl Pts',(178.079072130116,504.438252376895,-36.0471283913144)) ;
#61856 = CARTESIAN_POINT('Ctrl Pts',(178.031434095232,504.432568707919,-36.1412800646791)) ;
#61857 = CARTESIAN_POINT('Ctrl Pts',(178.00956564923,504.429682293223,-36.1889451226498)) ;
#61858 = CARTESIAN_POINT('Ctrl Pts',(177.94729477266,504.420513207317,-36.3396281130938)) ;
#61859 = CARTESIAN_POINT('Ctrl Pts',(177.913375173728,504.41402135162,-36.4450967596812)) ;
#61860 = CARTESIAN_POINT('Ctrl Pts',(177.855400178598,504.398841192147,-36.6921708900916)) ;
#61861 = CARTESIAN_POINT('Ctrl Pts',(177.837350195796,504.390100604637,-36.8346122735709)) ;
#61862 = CARTESIAN_POINT('Ctrl Pts',(177.833519635185,504.379961133188,-37.0119064910454)) ;
#61863 = CARTESIAN_POINT('Ctrl Pts',(177.83363286823,504.378043815694,-37.0460521233854)) ;
#61864 = CARTESIAN_POINT('Ctrl Pts',(177.83547817841,504.374464050053,-37.1113756246714)) ;
#61865 = CARTESIAN_POINT('Ctrl Pts',(177.837069933862,504.372795816064,-37.1425465031698)) ;
#61866 = CARTESIAN_POINT('Ctrl Pts',(177.844791726139,504.367306501627,-37.2469830457464)) ;
#61867 = CARTESIAN_POINT('Ctrl Pts',(177.854143340816,504.36363476977,-37.3199591266994)) ;
#61868 = CARTESIAN_POINT('Ctrl Pts',(177.893866962334,504.35281746537,-37.5368793385124)) ;
#61869 = CARTESIAN_POINT('Ctrl Pts',(177.935785576385,504.345869198863,-37.6782137245616)) ;
#61870 = CARTESIAN_POINT('Ctrl Pts',(178.018009868928,504.335177442307,-37.8751369016024)) ;
#61871 = CARTESIAN_POINT('Ctrl Pts',(178.046545225707,504.331778264457,-37.9351254848763)) ;
#61872 = CARTESIAN_POINT('Ctrl Pts',(178.101343350485,504.325666389523,-38.0372571276467)) ;
#61873 = CARTESIAN_POINT('Ctrl Pts',(178.126322274646,504.323001277131,-38.08002650189)) ;
#61874 = CARTESIAN_POINT('Ctrl Pts',(178.18702404461,504.316764617251,-38.1758358404909)) ;
#61875 = CARTESIAN_POINT('Ctrl Pts',(178.223725018205,504.31315764344,-38.2281920927415)) ;
#61876 = CARTESIAN_POINT('Ctrl Pts',(178.310861191262,504.304933612228,-38.3409253500451)) ;
#61877 = CARTESIAN_POINT('Ctrl Pts',(178.362443030331,504.300280441195,-38.4002882820591)) ;
#61878 = CARTESIAN_POINT('Ctrl Pts',(178.513623239173,504.287309550931,-38.5553519931561)) ;
#61879 = CARTESIAN_POINT('Ctrl Pts',(178.619663512684,504.278895790228,-38.6442039587384)) ;
#61880 = CARTESIAN_POINT('Ctrl Pts',(178.762609281968,504.268994138379,-38.7413220174802)) ;
#61881 = CARTESIAN_POINT('Ctrl Pts',(178.791900328897,504.267034818895,-38.76015282612)) ;
#61882 = CARTESIAN_POINT('Ctrl Pts',(178.847840154085,504.263442816442,-38.7941380770124)) ;
#61883 = CARTESIAN_POINT('Ctrl Pts',(178.874375218896,504.261801502184,-38.8094573120819)) ;
#61884 = CARTESIAN_POINT('Ctrl Pts',(178.96030286957,504.256654423801,-38.8565350906304)) ;
#61885 = CARTESIAN_POINT('Ctrl Pts',(179.020922335966,504.253272027075,-38.8859721620507)) ;
#61886 = CARTESIAN_POINT('Ctrl Pts',(179.211230834465,504.24308241426,-38.9670849493294)) ;
#61887 = CARTESIAN_POINT('Ctrl Pts',(179.344816204064,504.236492319199,-39.0085747583076)) ;
#61888 = CARTESIAN_POINT('Ctrl Pts',(179.554135230827,504.225900001773,-39.0508688107427)) ;
#61889 = CARTESIAN_POINT('Ctrl Pts',(179.627425372828,504.222148885058,-39.0615966499812)) ;
#61890 = CARTESIAN_POINT('Ctrl Pts',(179.750587587933,504.215671034999,-39.0728763037185)) ;
#61891 = CARTESIAN_POINT('Ctrl Pts',(179.800189524387,504.213016184586,-39.075610900755)) ;
#61892 = CARTESIAN_POINT('Ctrl Pts',(179.908396181734,504.207103240459,-39.0776486663926)) ;
#61893 = CARTESIAN_POINT('Ctrl Pts',(179.966968790785,504.203824794166,-39.076247243386)) ;
#61894 = CARTESIAN_POINT('Ctrl Pts',(180.092828594785,504.196606627187,-39.0678448660369)) ;
#61895 = CARTESIAN_POINT('Ctrl Pts',(180.159991247105,504.192646753089,-39.0600195915755)) ;
#61896 = CARTESIAN_POINT('Ctrl Pts',(180.362318746089,504.180447566007,-39.02626597024)) ;
#61897 = CARTESIAN_POINT('Ctrl Pts',(180.495375183035,504.172030998369,-38.9900659627336)) ;
#61898 = CARTESIAN_POINT('Ctrl Pts',(180.668181903654,504.161180978865,-38.9238421250475)) ;
#61899 = CARTESIAN_POINT('Ctrl Pts',(180.711949044893,504.158443621116,-38.9053045910474)) ;
#61900 = CARTESIAN_POINT('Ctrl Pts',(180.781409624588,504.154161161521,-38.8729992385101)) ;
#61901 = CARTESIAN_POINT('Ctrl Pts',(180.807517941004,504.15256793519,-38.8601755591509)) ;
#61902 = CARTESIAN_POINT('Ctrl Pts',(180.871116499867,504.148727728224,-38.8272433925758)) ;
#61903 = CARTESIAN_POINT('Ctrl Pts',(180.908269665468,504.146515743246,-38.8065180416558)) ;
#61904 = CARTESIAN_POINT('Ctrl Pts',(180.993837159418,504.141434216021,-38.7552391119479)) ;
#61905 = CARTESIAN_POINT('Ctrl Pts',(181.04167168088,504.138603296537,-38.7237862290604)) ;
#61906 = CARTESIAN_POINT('Ctrl Pts',(181.210378483855,504.128435505628,-38.6024700488032)) ;
#61907 = CARTESIAN_POINT('Ctrl Pts',(181.322585764394,504.121276173305,-38.5013983472221)) ;
#61908 = CARTESIAN_POINT('Ctrl Pts',(181.455800306384,504.111119709196,-38.3518682265149)) ;
#61909 = CARTESIAN_POINT('Ctrl Pts',(181.487498334288,504.108555055911,-38.3135777294949)) ;
#61910 = CARTESIAN_POINT('Ctrl Pts',(181.517775728527,504.105934865979,-38.2741778157906)) ;
#61911 = CARTESIAN_POINT('Origin',(179.888527625407,535.710565160536,-48.5221601717598)) ;
#61912 = CARTESIAN_POINT('Ctrl Pts',(181.451956083968,536.286106171205,-48.8631290382246)) ;
#61913 = CARTESIAN_POINT('Ctrl Pts',(181.445401841449,536.303910444207,-48.8618925414681)) ;
#61914 = CARTESIAN_POINT('Ctrl Pts',(181.438543835126,536.321601758001,-48.8606411710218)) ;
#61915 = CARTESIAN_POINT('Ctrl Pts',(181.41945812941,536.368445833857,-48.8572568591724)) ;
#61916 = CARTESIAN_POINT('Ctrl Pts',(181.406702462457,536.397369164468,-48.8550902797562)) ;
#61917 = CARTESIAN_POINT('Ctrl Pts',(181.343426241339,536.530460296774,-48.8448105556143)) ;
#61918 = CARTESIAN_POINT('Ctrl Pts',(181.282959873888,536.629539463379,-48.8362823401656)) ;
#61919 = CARTESIAN_POINT('Ctrl Pts',(181.171658204911,536.775323279961,-48.8229818495332)) ;
#61920 = CARTESIAN_POINT('Ctrl Pts',(181.127358346787,536.826555328311,-48.8181274957693)) ;
#61921 = CARTESIAN_POINT('Ctrl Pts',(181.039987027751,536.915963358886,-48.8093647000216)) ;
#61922 = CARTESIAN_POINT('Ctrl Pts',(180.997819204767,536.954879094015,-48.8054300663977)) ;
#61923 = CARTESIAN_POINT('Ctrl Pts',(180.914350770737,537.024286967429,-48.798156968782)) ;
#61924 = CARTESIAN_POINT('Ctrl Pts',(180.873486662309,537.055196989528,-48.7948033931466)) ;
#61925 = CARTESIAN_POINT('Ctrl Pts',(180.715645399245,537.163525867764,-48.7825128141501)) ;
#61926 = CARTESIAN_POINT('Ctrl Pts',(180.590480353423,537.227958858901,-48.7741053222124)) ;
#61927 = CARTESIAN_POINT('Ctrl Pts',(180.410704605132,537.29344170527,-48.762355655858)) ;
#61928 = CARTESIAN_POINT('Ctrl Pts',(180.361917082431,537.308710533985,-48.7591900680543)) ;
#61929 = CARTESIAN_POINT('Ctrl Pts',(180.275541773772,537.331440621175,-48.7535062333762)) ;
#61930 = CARTESIAN_POINT('Ctrl Pts',(180.238254393896,537.339892570055,-48.7510272515709)) ;
#61931 = CARTESIAN_POINT('Ctrl Pts',(180.170299363026,537.352856047998,-48.7464093436077)) ;
#61932 = CARTESIAN_POINT('Ctrl Pts',(180.139735210229,537.357807947996,-48.74429300956)) ;
#61933 = CARTESIAN_POINT('Ctrl Pts',(179.987727526603,537.378107754513,-48.7336211306909)) ;
#61934 = CARTESIAN_POINT('Ctrl Pts',(179.864992040077,537.380889079062,-48.7245850571382)) ;
#61935 = CARTESIAN_POINT('Ctrl Pts',(179.677579684228,537.364463130775,-48.7109590783032)) ;
#61936 = CARTESIAN_POINT('Ctrl Pts',(179.612484000194,537.354851945904,-48.7062521308366)) ;
#61937 = CARTESIAN_POINT('Ctrl Pts',(179.492811896352,537.329872854313,-48.6976972489222)) ;
#61938 = CARTESIAN_POINT('Ctrl Pts',(179.438121068129,537.315521117356,-48.6938264852776)) ;
#61939 = CARTESIAN_POINT('Ctrl Pts',(179.33514120235,537.282816849689,-48.6865971965219)) ;
#61940 = CARTESIAN_POINT('Ctrl Pts',(179.286769577754,537.264946104945,-48.6832272746554)) ;
#61941 = CARTESIAN_POINT('Ctrl Pts',(179.115251273482,537.192369101227,-48.671288502312)) ;
#61942 = CARTESIAN_POINT('Ctrl Pts',(178.998028122189,537.125030674743,-48.6631930146316)) ;
#61943 = CARTESIAN_POINT('Ctrl Pts',(178.847759472658,537.012550643929,-48.6516808887462)) ;
#61944 = CARTESIAN_POINT('Ctrl Pts',(178.806875249398,536.978789074268,-48.6484047620819)) ;
#61945 = CARTESIAN_POINT('Ctrl Pts',(178.738765680519,536.916852876371,-48.6425563659384)) ;
#61946 = CARTESIAN_POINT('Ctrl Pts',(178.71079555728,536.889560130116,-48.6400268733404)) ;
#61947 = CARTESIAN_POINT('Ctrl Pts',(178.662632282902,536.8391381328,-48.6353781704473)) ;
#61948 = CARTESIAN_POINT('Ctrl Pts',(178.642071541905,536.816387463089,-48.6332852885324)) ;
#61949 = CARTESIAN_POINT('Ctrl Pts',(178.549411150272,536.707989706724,-48.6233743524902)) ;
#61950 = CARTESIAN_POINT('Ctrl Pts',(178.485437852139,536.615785632238,-48.6151467179976)) ;
#61951 = CARTESIAN_POINT('Ctrl Pts',(178.396802099555,536.455782669324,-48.6018597914381)) ;
#61952 = CARTESIAN_POINT('Ctrl Pts',(178.366406883428,536.391553010678,-48.5967507811819)) ;
#61953 = CARTESIAN_POINT('Ctrl Pts',(178.31851456452,536.270980796986,-48.5876322998191)) ;
#61954 = CARTESIAN_POINT('Ctrl Pts',(178.299730034168,536.215273403371,-48.5835905679914)) ;
#61955 = CARTESIAN_POINT('Ctrl Pts',(178.270432344023,536.110365552277,-48.5762775624481)) ;
#61956 = CARTESIAN_POINT('Ctrl Pts',(178.259126820571,536.061459177897,-48.5729833740857)) ;
#61957 = CARTESIAN_POINT('Ctrl Pts',(178.232962589701,535.919293550546,-48.5636769772334)) ;
#61958 = CARTESIAN_POINT('Ctrl Pts',(178.223796957473,535.825186275962,-48.557853867868)) ;
#61959 = CARTESIAN_POINT('Ctrl Pts',(178.221376978864,535.625950363706,-48.5456708139611)) ;
#61960 = CARTESIAN_POINT('Ctrl Pts',(178.230005028246,535.521226599191,-48.53934884585)) ;
#61961 = CARTESIAN_POINT('Ctrl Pts',(178.254756245185,535.382461903842,-48.5303373125597)) ;
#61962 = CARTESIAN_POINT('Ctrl Pts',(178.262252961617,535.347122083389,-48.5279841224477)) ;
#61963 = CARTESIAN_POINT('Ctrl Pts',(178.278538014051,535.281017240628,-48.5234239778264)) ;
#61964 = CARTESIAN_POINT('Ctrl Pts',(178.287075476337,535.25020836675,-48.5212299604185)) ;
#61965 = CARTESIAN_POINT('Ctrl Pts',(178.30774854546,535.183163191395,-48.5163301324382)) ;
#61966 = CARTESIAN_POINT('Ctrl Pts',(178.320256251134,535.147058456146,-48.5136097353657)) ;
#61967 = CARTESIAN_POINT('Ctrl Pts',(178.366486174142,535.027111182489,-48.5043603339154)) ;
#61968 = CARTESIAN_POINT('Ctrl Pts',(178.405783940426,534.945587344092,-48.4977266488301)) ;
#61969 = CARTESIAN_POINT('Ctrl Pts',(178.493675145285,534.795747387831,-48.4851855682641)) ;
#61970 = CARTESIAN_POINT('Ctrl Pts',(178.541193720555,534.727101837503,-48.4792784118901)) ;
#61971 = CARTESIAN_POINT('Ctrl Pts',(178.625345330398,534.62315430444,-48.4701100576345)) ;
#61972 = CARTESIAN_POINT('Ctrl Pts',(178.658791882695,534.585468346556,-48.4667301383124)) ;
#61973 = CARTESIAN_POINT('Ctrl Pts',(178.736071673144,534.505964667386,-48.4594429830431)) ;
#61974 = CARTESIAN_POINT('Ctrl Pts',(178.780580798885,534.464903785589,-48.4555728702336)) ;
#61975 = CARTESIAN_POINT('Ctrl Pts',(178.958787414233,534.317630590756,-48.4410694757553)) ;
#61976 = CARTESIAN_POINT('Ctrl Pts',(179.10624318588,534.229789053832,-48.4311323402834)) ;
#61977 = CARTESIAN_POINT('Ctrl Pts',(179.29526323438,534.153420779713,-48.4180006057553)) ;
#61978 = CARTESIAN_POINT('Ctrl Pts',(179.32645130277,534.141893394678,-48.4158186048797)) ;
#61979 = CARTESIAN_POINT('Ctrl Pts',(179.390488483832,534.120379481555,-48.4112673043479)) ;
#61980 = CARTESIAN_POINT('Ctrl Pts',(179.423343033481,534.11046006711,-48.4088962401272)) ;
#61981 = CARTESIAN_POINT('Ctrl Pts',(179.557139774496,534.074532848963,-48.3991601142111)) ;
#61982 = CARTESIAN_POINT('Ctrl Pts',(179.660110853324,534.057010448843,-48.3915011029027)) ;
#61983 = CARTESIAN_POINT('Ctrl Pts',(179.862707993671,534.041829151286,-48.3767506686075)) ;
#61984 = CARTESIAN_POINT('Ctrl Pts',(179.961854862796,534.04323927891,-48.3696797205071)) ;
#61985 = CARTESIAN_POINT('Ctrl Pts',(180.110228486116,534.058619666808,-48.3594307531145)) ;
#61986 = CARTESIAN_POINT('Ctrl Pts',(180.159897218995,534.066048611531,-48.3560535462152)) ;
#61987 = CARTESIAN_POINT('Ctrl Pts',(180.266667645582,534.08698870835,-48.3488844496936)) ;
#61988 = CARTESIAN_POINT('Ctrl Pts',(180.323544845949,534.101294624443,-48.3451234572799)) ;
#61989 = CARTESIAN_POINT('Ctrl Pts',(180.447084181674,534.13939855112,-48.3369868187775)) ;
#61990 = CARTESIAN_POINT('Ctrl Pts',(180.513222545071,534.164503324822,-48.3326533681225)) ;
#61991 = CARTESIAN_POINT('Ctrl Pts',(180.680225631726,534.240366806741,-48.3214482268071)) ;
#61992 = CARTESIAN_POINT('Ctrl Pts',(180.777867842923,534.297293941667,-48.3146381713659)) ;
#61993 = CARTESIAN_POINT('Ctrl Pts',(180.893743191954,534.381642909102,-48.3053136498849)) ;
#61994 = CARTESIAN_POINT('Ctrl Pts',(180.917981307947,534.400329422626,-48.3032841039066)) ;
#61995 = CARTESIAN_POINT('Ctrl Pts',(180.972107525708,534.444488057351,-48.2985389957307)) ;
#61996 = CARTESIAN_POINT('Ctrl Pts',(181.00163143216,534.470365211504,-48.2957998556565)) ;
#61997 = CARTESIAN_POINT('Ctrl Pts',(181.069101746028,534.533852611671,-48.2892279578467)) ;
#61998 = CARTESIAN_POINT('Ctrl Pts',(181.106208234236,534.572294134727,-48.2853613355198)) ;
#61999 = CARTESIAN_POINT('Ctrl Pts',(181.229501700653,534.712963394802,-48.2717564119641)) ;
#62000 = CARTESIAN_POINT('Ctrl Pts',(181.305202518358,534.823736110179,-48.2620257177712)) ;
#62001 = CARTESIAN_POINT('Ctrl Pts',(181.39066097337,534.988196008883,-48.2492352804052)) ;
#62002 = CARTESIAN_POINT('Ctrl Pts',(181.412327276743,535.035096845546,-48.2457464992169)) ;
#62003 = CARTESIAN_POINT('Ctrl Pts',(181.453019193062,535.13515229458,-48.2386040333602)) ;
#62004 = CARTESIAN_POINT('Ctrl Pts',(181.471593911735,535.188419461946,-48.2349695293695)) ;
#62005 = CARTESIAN_POINT('Ctrl Pts',(181.505816833914,535.305332469606,-48.2272682045055)) ;
#62006 = CARTESIAN_POINT('Ctrl Pts',(181.520485072712,535.369165421784,-48.2232332206311)) ;
#62007 = CARTESIAN_POINT('Ctrl Pts',(181.55186846701,535.555384353464,-48.2116735151591)) ;
#62008 = CARTESIAN_POINT('Ctrl Pts',(181.558789752985,535.678953015432,-48.2042749395757)) ;
#62009 = CARTESIAN_POINT('Ctrl Pts',(181.550311947402,535.832969013319,-48.194252299259)) ;
#62010 = CARTESIAN_POINT('Ctrl Pts',(181.547757461034,535.863751558768,-48.192206796657)) ;
#62011 = CARTESIAN_POINT('Ctrl Pts',(181.540088429022,535.932810408178,-48.1874920233069)) ;
#62012 = CARTESIAN_POINT('Ctrl Pts',(181.534496277019,535.971012136138,-48.1848018162824)) ;
#62013 = CARTESIAN_POINT('Ctrl Pts',(181.51039947183,536.103364346698,-48.1752708839214)) ;
#62014 = CARTESIAN_POINT('Ctrl Pts',(181.485096229393,536.196082005249,-48.1682298305151)) ;
#62015 = CARTESIAN_POINT('Ctrl Pts',(181.451957355136,536.286102718128,-48.1612691418708)) ;
#62016 = CARTESIAN_POINT('Ctrl Pts',(181.451956072328,536.286106202824,-49.0537499415271)) ;
#62017 = CARTESIAN_POINT('Ctrl Pts',(181.444652999706,536.305944634229,-49.0524601164881)) ;
#62018 = CARTESIAN_POINT('Ctrl Pts',(181.436969948344,536.325650536645,-49.0511716725108)) ;
#62019 = CARTESIAN_POINT('Ctrl Pts',(181.401722665985,536.411200822763,-49.0455280065106)) ;
#62020 = CARTESIAN_POINT('Ctrl Pts',(181.370324467744,536.475370143754,-49.0411597533643)) ;
#62021 = CARTESIAN_POINT('Ctrl Pts',(181.305647465685,536.588519950892,-49.0329685862384)) ;
#62022 = CARTESIAN_POINT('Ctrl Pts',(181.273690047954,536.638119483931,-49.0291894357721)) ;
#62023 = CARTESIAN_POINT('Ctrl Pts',(181.209813010097,536.726575040688,-49.0220066308013)) ;
#62024 = CARTESIAN_POINT('Ctrl Pts',(181.178634484178,536.765882404595,-49.0186354002201)) ;
#62025 = CARTESIAN_POINT('Ctrl Pts',(181.085945636468,536.872481132761,-49.0089363043924)) ;
#62026 = CARTESIAN_POINT('Ctrl Pts',(181.020626926734,536.936209896215,-49.0024509014762)) ;
#62027 = CARTESIAN_POINT('Ctrl Pts',(180.868614765786,537.061957551611,-48.9881600908592)) ;
#62028 = CARTESIAN_POINT('Ctrl Pts',(180.780507366938,537.121666028037,-48.980342893649)) ;
#62029 = CARTESIAN_POINT('Ctrl Pts',(180.65463160926,537.190439372448,-48.970204552058)) ;
#62030 = CARTESIAN_POINT('Ctrl Pts',(180.621356086709,537.207196714229,-48.9676152587733)) ;
#62031 = CARTESIAN_POINT('Ctrl Pts',(180.558838462443,537.236094385003,-48.9629524177518)) ;
#62032 = CARTESIAN_POINT('Ctrl Pts',(180.529760797672,537.248543118926,-48.9608641801791)) ;
#62033 = CARTESIAN_POINT('Ctrl Pts',(180.391697573253,537.303053895975,-48.9512479597624)) ;
#62034 = CARTESIAN_POINT('Ctrl Pts',(180.27882477886,537.334411235509,-48.9442228422084)) ;
#62035 = CARTESIAN_POINT('Ctrl Pts',(180.096912622584,537.364863107974,-48.9329483632415)) ;
#62036 = CARTESIAN_POINT('Ctrl Pts',(180.029624869013,537.371955112813,-48.9287911807169)) ;
#62037 = CARTESIAN_POINT('Ctrl Pts',(179.90470500665,537.377476825306,-48.9209023403871)) ;
#62038 = CARTESIAN_POINT('Ctrl Pts',(179.847227053245,537.37704325759,-48.9172064998977)) ;
#62039 = CARTESIAN_POINT('Ctrl Pts',(179.738370101123,537.370586985611,-48.9100060099322)) ;
#62040 = CARTESIAN_POINT('Ctrl Pts',(179.687024674893,537.365139205087,-48.9065242777309)) ;
#62041 = CARTESIAN_POINT('Ctrl Pts',(179.500305910478,537.336508301739,-48.8935053166676)) ;
#62042 = CARTESIAN_POINT('Ctrl Pts',(179.367707059889,537.299004414284,-48.8835069489898)) ;
#62043 = CARTESIAN_POINT('Ctrl Pts',(179.193147628988,537.225400735127,-48.8697376387081)) ;
#62044 = CARTESIAN_POINT('Ctrl Pts',(179.146031075378,537.20287199927,-48.8659626691381)) ;
#62045 = CARTESIAN_POINT('Ctrl Pts',(179.065899411207,537.159820659145,-48.8595178109888)) ;
#62046 = CARTESIAN_POINT('Ctrl Pts',(179.032398413199,537.14028613622,-48.8568157003346)) ;
#62047 = CARTESIAN_POINT('Ctrl Pts',(178.973261105123,537.102977998372,-48.8520719412159)) ;
#62048 = CARTESIAN_POINT('Ctrl Pts',(178.947387077376,537.085621851242,-48.8500095409117)) ;
#62049 = CARTESIAN_POINT('Ctrl Pts',(178.834923491124,537.005519484749,-48.8410421838967)) ;
#62050 = CARTESIAN_POINT('Ctrl Pts',(178.753994818018,536.935240637472,-48.8345618743026)) ;
#62051 = CARTESIAN_POINT('Ctrl Pts',(178.630138063676,536.804791151174,-48.8235765835784)) ;
#62052 = CARTESIAN_POINT('Ctrl Pts',(178.583451858269,536.748664888205,-48.8191130998566)) ;
#62053 = CARTESIAN_POINT('Ctrl Pts',(178.505516622669,536.641370883671,-48.8107782544506)) ;
#62054 = CARTESIAN_POINT('Ctrl Pts',(178.473062448466,536.591232938511,-48.8069534916042)) ;
#62055 = CARTESIAN_POINT('Ctrl Pts',(178.418293457785,536.495745312112,-48.7997066121985)) ;
#62056 = CARTESIAN_POINT('Ctrl Pts',(178.39521601073,536.450913618259,-48.7963186085098)) ;
#62057 = CARTESIAN_POINT('Ctrl Pts',(178.336353782971,536.322575784734,-48.7866241266458)) ;
#62058 = CARTESIAN_POINT('Ctrl Pts',(178.305316414915,536.237099286703,-48.7801631208431)) ;
#62059 = CARTESIAN_POINT('Ctrl Pts',(178.253256203703,536.046498800338,-48.7658526358325)) ;
#62060 = CARTESIAN_POINT('Ctrl Pts',(178.235086652117,535.940995749693,-48.7579883362068)) ;
#62061 = CARTESIAN_POINT('Ctrl Pts',(178.224362427726,535.797207742188,-48.7477950802033)) ;
#62062 = CARTESIAN_POINT('Ctrl Pts',(178.222837322931,535.75985133355,-48.745196186547)) ;
#62063 = CARTESIAN_POINT('Ctrl Pts',(178.222343869998,535.69080745543,-48.7405208954119)) ;
#62064 = CARTESIAN_POINT('Ctrl Pts',(178.223020334068,535.659142554616,-48.7384295397676)) ;
#62065 = CARTESIAN_POINT('Ctrl Pts',(178.230404250324,535.511204908019,-48.7288318244825)) ;
#62066 = CARTESIAN_POINT('Ctrl Pts',(178.248389465455,535.395808185701,-48.7218240282482)) ;
#62067 = CARTESIAN_POINT('Ctrl Pts',(178.295612571426,535.217869548388,-48.7105663841804)) ;
#62068 = CARTESIAN_POINT('Ctrl Pts',(178.316916691311,535.153640201641,-48.7064072989536)) ;
#62069 = CARTESIAN_POINT('Ctrl Pts',(178.36342938303,535.037563497842,-48.698515865777)) ;
#62070 = CARTESIAN_POINT('Ctrl Pts',(178.387537498471,534.985387040199,-48.6948193333161)) ;
#62071 = CARTESIAN_POINT('Ctrl Pts',(178.438341439578,534.888870314242,-48.6876157633278)) ;
#62072 = CARTESIAN_POINT('Ctrl Pts',(178.464502047986,534.844324712763,-48.684131552719)) ;
#62073 = CARTESIAN_POINT('Ctrl Pts',(178.569907934526,534.682553841477,-48.6708215229749)) ;
#62074 = CARTESIAN_POINT('Ctrl Pts',(178.661897798574,534.574374419796,-48.660498575176)) ;
#62075 = CARTESIAN_POINT('Ctrl Pts',(178.803485296674,534.445355900407,-48.6465828522548)) ;
#62076 = CARTESIAN_POINT('Ctrl Pts',(178.842065012611,534.413264898068,-48.6429605774959)) ;
#62077 = CARTESIAN_POINT('Ctrl Pts',(178.912190338064,534.360101021607,-48.6367340936556)) ;
#62078 = CARTESIAN_POINT('Ctrl Pts',(178.94311786213,534.338271877889,-48.634100274279)) ;
#62079 = CARTESIAN_POINT('Ctrl Pts',(179.001047698554,534.300273216161,-48.6294055322539)) ;
#62080 = CARTESIAN_POINT('Ctrl Pts',(179.027813286086,534.283780331266,-48.6273275451756)) ;
#62081 = CARTESIAN_POINT('Ctrl Pts',(179.157917175369,534.20860507297,-48.6175823518427)) ;
#62082 = CARTESIAN_POINT('Ctrl Pts',(179.266883086093,534.160325895569,-48.610440547418)) ;
#62083 = CARTESIAN_POINT('Ctrl Pts',(179.443825287085,534.103618447951,-48.5990757277951)) ;
#62084 = CARTESIAN_POINT('Ctrl Pts',(179.508748118981,534.08704908744,-48.5949546844974)) ;
#62085 = CARTESIAN_POINT('Ctrl Pts',(179.63063155382,534.063654758555,-48.5871182169442)) ;
#62086 = CARTESIAN_POINT('Ctrl Pts',(179.687286753632,534.055776605915,-48.583437285437)) ;
#62087 = CARTESIAN_POINT('Ctrl Pts',(179.795814145927,534.046341244903,-48.5762393202312)) ;
#62088 = CARTESIAN_POINT('Ctrl Pts',(179.847573567845,534.044264241712,-48.5727437584416)) ;
#62089 = CARTESIAN_POINT('Ctrl Pts',(180.034568195186,534.045477986089,-48.5598464440853)) ;
#62090 = CARTESIAN_POINT('Ctrl Pts',(180.169163967346,534.062817256202,-48.5500025875058)) ;
#62091 = CARTESIAN_POINT('Ctrl Pts',(180.351477600845,534.109303564848,-48.5363217538065)) ;
#62092 = CARTESIAN_POINT('Ctrl Pts',(180.402151257672,534.124831001583,-48.5324880718608)) ;
#62093 = CARTESIAN_POINT('Ctrl Pts',(180.488803868579,534.155973967457,-48.5259596796516)) ;
#62094 = CARTESIAN_POINT('Ctrl Pts',(180.525132849965,534.170493810251,-48.5232317045762)) ;
#62095 = CARTESIAN_POINT('Ctrl Pts',(180.589251907854,534.198778027206,-48.5184743512113)) ;
#62096 = CARTESIAN_POINT('Ctrl Pts',(180.617229312525,534.212062967201,-48.516422586656)) ;
#62097 = CARTESIAN_POINT('Ctrl Pts',(180.742393017326,534.275831332575,-48.5072931253819)) ;
#62098 = CARTESIAN_POINT('Ctrl Pts',(180.834839625239,534.335047927997,-48.5006664165278)) ;
#62099 = CARTESIAN_POINT('Ctrl Pts',(180.977346854394,534.447546447001,-48.4895790086613)) ;
#62100 = CARTESIAN_POINT('Ctrl Pts',(181.03092297632,534.495791339069,-48.485168003849)) ;
#62101 = CARTESIAN_POINT('Ctrl Pts',(181.122620489224,534.589811388457,-48.4769093360181)) ;
#62102 = CARTESIAN_POINT('Ctrl Pts',(181.161732696112,534.634450968694,-48.4731064116664)) ;
#62103 = CARTESIAN_POINT('Ctrl Pts',(181.229560756722,534.720750794004,-48.4658773324031)) ;
#62104 = CARTESIAN_POINT('Ctrl Pts',(181.258920868448,534.761816651075,-48.462483822048)) ;
#62105 = CARTESIAN_POINT('Ctrl Pts',(181.341294615768,534.888850300523,-48.4520836994211)) ;
#62106 = CARTESIAN_POINT('Ctrl Pts',(181.388397610983,534.978355510868,-48.4448672258863)) ;
#62107 = CARTESIAN_POINT('Ctrl Pts',(181.45648639386,535.142297088654,-48.4319750445597)) ;
#62108 = CARTESIAN_POINT('Ctrl Pts',(181.480953159586,535.214979947161,-48.4263675132201)) ;
#62109 = CARTESIAN_POINT('Ctrl Pts',(181.512473276413,535.335519004315,-48.4174345830246)) ;
#62110 = CARTESIAN_POINT('Ctrl Pts',(181.522603784557,535.382456640829,-48.4140444255247)) ;
#62111 = CARTESIAN_POINT('Ctrl Pts',(181.535686926608,535.458970665944,-48.4087253486124)) ;
#62112 = CARTESIAN_POINT('Ctrl Pts',(181.539899835167,535.488295862052,-48.4067387604865)) ;
#62113 = CARTESIAN_POINT('Ctrl Pts',(181.549578645045,535.571351609852,-48.4012463685222)) ;
#62114 = CARTESIAN_POINT('Ctrl Pts',(181.553218199038,535.625256866763,-48.3978298650265)) ;
#62115 = CARTESIAN_POINT('Ctrl Pts',(181.556289051666,535.788596880453,-48.3876709276972)) ;
#62116 = CARTESIAN_POINT('Ctrl Pts',(181.54757277394,535.897882975501,-48.3811197798381)) ;
#62117 = CARTESIAN_POINT('Ctrl Pts',(181.515501205169,536.076165957159,-48.3699036379122)) ;
#62118 = CARTESIAN_POINT('Ctrl Pts',(181.498244779974,536.145899165917,-48.3653807724651)) ;
#62119 = CARTESIAN_POINT('Ctrl Pts',(181.468896035144,536.238421419071,-48.3590621823926)) ;
#62120 = CARTESIAN_POINT('Ctrl Pts',(181.460696278165,536.262363870131,-48.3573978200419)) ;
#62121 = CARTESIAN_POINT('Ctrl Pts',(181.451956078709,536.28610618549,-48.355715363061)) ;
#62122 = CARTESIAN_POINT('Origin',(179.888527625416,585.710565160536,-48.5221601717598)) ;
#62123 = CARTESIAN_POINT('Ctrl Pts',(181.45195815568,586.286100543496,-48.8631342200737)) ;
#62124 = CARTESIAN_POINT('Ctrl Pts',(181.445395417149,586.303928093434,-48.8618961238889)) ;
#62125 = CARTESIAN_POINT('Ctrl Pts',(181.438528122193,586.321642385202,-48.8606431156781)) ;
#62126 = CARTESIAN_POINT('Ctrl Pts',(181.419427296626,586.368518069373,-48.8572563811899)) ;
#62127 = CARTESIAN_POINT('Ctrl Pts',(181.406666054341,586.39745010849,-48.8550890352828)) ;
#62128 = CARTESIAN_POINT('Ctrl Pts',(181.343417378162,586.530462932121,-48.8448147933775)) ;
#62129 = CARTESIAN_POINT('Ctrl Pts',(181.283002087658,586.629463725066,-48.8362937062396)) ;
#62130 = CARTESIAN_POINT('Ctrl Pts',(181.171755641747,586.775207597148,-48.8229978111714)) ;
#62131 = CARTESIAN_POINT('Ctrl Pts',(181.127441967481,586.826464164859,-48.8181413755912)) ;
#62132 = CARTESIAN_POINT('Ctrl Pts',(181.040047552031,586.915906154756,-48.8093755878045)) ;
#62133 = CARTESIAN_POINT('Ctrl Pts',(180.99787200679,586.954832615455,-48.8054399988221)) ;
#62134 = CARTESIAN_POINT('Ctrl Pts',(180.914395907013,587.024251727405,-48.7981659313724)) ;
#62135 = CARTESIAN_POINT('Ctrl Pts',(180.873532736041,587.055163244635,-48.7948123002097)) ;
#62136 = CARTESIAN_POINT('Ctrl Pts',(180.715655128551,587.163525002694,-48.7825184509087)) ;
#62137 = CARTESIAN_POINT('Ctrl Pts',(180.590445938783,587.227979253165,-48.774108240018)) ;
#62138 = CARTESIAN_POINT('Ctrl Pts',(180.410634822879,587.293464258157,-48.762356370403)) ;
#62139 = CARTESIAN_POINT('Ctrl Pts',(180.361860493631,587.308726833761,-48.7591916229672)) ;
#62140 = CARTESIAN_POINT('Ctrl Pts',(180.275504485808,587.331449378907,-48.7535090170231)) ;
#62141 = CARTESIAN_POINT('Ctrl Pts',(180.238222929237,587.33989917927,-48.751030397237)) ;
#62142 = CARTESIAN_POINT('Ctrl Pts',(180.170269341545,587.352861282907,-48.7464125459367)) ;
#62143 = CARTESIAN_POINT('Ctrl Pts',(180.139700671585,587.357813298877,-48.7442958734795)) ;
#62144 = CARTESIAN_POINT('Ctrl Pts',(179.987725477292,587.378105106976,-48.7336261613859)) ;
#62145 = CARTESIAN_POINT('Ctrl Pts',(179.865028084288,587.380886821715,-48.7245929831802)) ;
#62146 = CARTESIAN_POINT('Ctrl Pts',(179.677640701921,587.36447138691,-48.7109687723047)) ;
#62147 = CARTESIAN_POINT('Ctrl Pts',(179.612532850842,587.3548606239,-48.7062609154197)) ;
#62148 = CARTESIAN_POINT('Ctrl Pts',(179.492842393294,587.329880523963,-48.6977046826171)) ;
#62149 = CARTESIAN_POINT('Ctrl Pts',(179.43814528453,587.315528132511,-48.6938334596435)) ;
#62150 = CARTESIAN_POINT('Ctrl Pts',(179.335158039324,587.282822812466,-48.6866036349422)) ;
#62151 = CARTESIAN_POINT('Ctrl Pts',(179.286785175313,587.26495218045,-48.683233620141)) ;
#62152 = CARTESIAN_POINT('Ctrl Pts',(179.115253043243,587.192371220558,-48.671293872118)) ;
#62153 = CARTESIAN_POINT('Ctrl Pts',(178.998018526856,587.125025886462,-48.663197625617)) ;
#62154 = CARTESIAN_POINT('Ctrl Pts',(178.84774373324,587.012537920548,-48.6516848633598)) ;
#62155 = CARTESIAN_POINT('Ctrl Pts',(178.806862571575,586.978778116054,-48.6484089329801)) ;
#62156 = CARTESIAN_POINT('Ctrl Pts',(178.738756907588,586.916844477785,-48.6425607993073)) ;
#62157 = CARTESIAN_POINT('Ctrl Pts',(178.710787785175,586.889552328761,-48.6400313659057)) ;
#62158 = CARTESIAN_POINT('Ctrl Pts',(178.662623663881,586.839128846284,-48.6353825280805)) ;
#62159 = CARTESIAN_POINT('Ctrl Pts',(178.642061242138,586.816375930667,-48.6332894402456)) ;
#62160 = CARTESIAN_POINT('Ctrl Pts',(178.549416667474,586.707994274046,-48.6233800000476)) ;
#62161 = CARTESIAN_POINT('Ctrl Pts',(178.485456818061,586.615811900013,-48.6151542993375)) ;
#62162 = CARTESIAN_POINT('Ctrl Pts',(178.396822941643,586.455825344801,-48.6018684335083)) ;
#62163 = CARTESIAN_POINT('Ctrl Pts',(178.366421779789,586.391587352801,-48.596758660419)) ;
#62164 = CARTESIAN_POINT('Ctrl Pts',(178.318521859579,586.271001776633,-48.5876390544956)) ;
#62165 = CARTESIAN_POINT('Ctrl Pts',(178.299735014943,586.21528968548,-48.5835969449305)) ;
#62166 = CARTESIAN_POINT('Ctrl Pts',(178.270434656485,586.11037515806,-48.5762834346059)) ;
#62167 = CARTESIAN_POINT('Ctrl Pts',(178.259128428237,586.061466924438,-48.5729891081358)) ;
#62168 = CARTESIAN_POINT('Ctrl Pts',(178.232963221671,585.919298844015,-48.5636825260079)) ;
#62169 = CARTESIAN_POINT('Ctrl Pts',(178.223797245764,585.825190974939,-48.557859367918)) ;
#62170 = CARTESIAN_POINT('Ctrl Pts',(178.22137675862,585.625953374547,-48.5456761923845)) ;
#62171 = CARTESIAN_POINT('Ctrl Pts',(178.230004741034,585.521228521675,-48.5393541532479)) ;
#62172 = CARTESIAN_POINT('Ctrl Pts',(178.254756216032,585.382461959764,-48.5303424845386)) ;
#62173 = CARTESIAN_POINT('Ctrl Pts',(178.26225310819,585.347121347018,-48.5279892366432)) ;
#62174 = CARTESIAN_POINT('Ctrl Pts',(178.278538896352,585.281013784409,-48.5234288901615)) ;
#62175 = CARTESIAN_POINT('Ctrl Pts',(178.287076979221,585.250202999452,-48.5212347256081)) ;
#62176 = CARTESIAN_POINT('Ctrl Pts',(178.307751910826,585.183152866943,-48.5163345054779)) ;
#62177 = CARTESIAN_POINT('Ctrl Pts',(178.320260961917,585.147045123671,-48.5136138596793)) ;
#62178 = CARTESIAN_POINT('Ctrl Pts',(178.366499301835,585.027079748457,-48.5043629778704)) ;
#62179 = CARTESIAN_POINT('Ctrl Pts',(178.405806400911,584.945541844804,-48.4977280397341)) ;
#62180 = CARTESIAN_POINT('Ctrl Pts',(178.493729271822,584.795661767691,-48.4851833753854)) ;
#62181 = CARTESIAN_POINT('Ctrl Pts',(178.541272145921,584.726991521092,-48.4792739398857)) ;
#62182 = CARTESIAN_POINT('Ctrl Pts',(178.625453742743,584.62302852524,-48.4701038447424)) ;
#62183 = CARTESIAN_POINT('Ctrl Pts',(178.658901939437,584.585348205591,-48.4667242798575)) ;
#62184 = CARTESIAN_POINT('Ctrl Pts',(178.736214594653,584.505825972784,-48.4594350348387)) ;
#62185 = CARTESIAN_POINT('Ctrl Pts',(178.780758089445,584.464744206344,-48.455562626252)) ;
#62186 = CARTESIAN_POINT('Ctrl Pts',(178.959201873152,584.317325055665,-48.4410427013598)) ;
#62187 = CARTESIAN_POINT('Ctrl Pts',(179.106897446745,584.229416393242,-48.4310931826386)) ;
#62188 = CARTESIAN_POINT('Ctrl Pts',(179.296062549795,584.153119208356,-48.4179493718058)) ;
#62189 = CARTESIAN_POINT('Ctrl Pts',(179.327135949902,584.141650947657,-48.4157749251129)) ;
#62190 = CARTESIAN_POINT('Ctrl Pts',(179.391202653044,584.120152722041,-48.4112206507534)) ;
#62191 = CARTESIAN_POINT('Ctrl Pts',(179.424206587051,584.110206027197,-48.4088383029963)) ;
#62192 = CARTESIAN_POINT('Ctrl Pts',(179.558225010919,584.074309879143,-48.3990843113958)) ;
#62193 = CARTESIAN_POINT('Ctrl Pts',(179.661262958337,584.056848209297,-48.3914204243538)) ;
#62194 = CARTESIAN_POINT('Ctrl Pts',(179.863536560141,584.041839676472,-48.3766955582062)) ;
#62195 = CARTESIAN_POINT('Ctrl Pts',(179.96228948806,584.04328162874,-48.3696536971554)) ;
#62196 = CARTESIAN_POINT('Ctrl Pts',(180.110276131934,584.058625983096,-48.3594314119205)) ;
#62197 = CARTESIAN_POINT('Ctrl Pts',(180.159947212651,584.066056782849,-48.3560540289076)) ;
#62198 = CARTESIAN_POINT('Ctrl Pts',(180.266728468062,584.087002546081,-48.3488841559948)) ;
#62199 = CARTESIAN_POINT('Ctrl Pts',(180.323613961205,584.101312976819,-48.3451225870087)) ;
#62200 = CARTESIAN_POINT('Ctrl Pts',(180.447179470846,584.139431521646,-48.3369841059589)) ;
#62201 = CARTESIAN_POINT('Ctrl Pts',(180.513335099721,584.164547884762,-48.3326494265749)) ;
#62202 = CARTESIAN_POINT('Ctrl Pts',(180.680285102839,584.240404310523,-48.321447250591)) ;
#62203 = CARTESIAN_POINT('Ctrl Pts',(180.7778639742,584.297297199941,-48.3146411259093)) ;
#62204 = CARTESIAN_POINT('Ctrl Pts',(180.893689803835,584.38160239818,-48.30532097844)) ;
#62205 = CARTESIAN_POINT('Ctrl Pts',(180.917933084389,584.400291403845,-48.3032910877185)) ;
#62206 = CARTESIAN_POINT('Ctrl Pts',(180.972056869607,584.444445034939,-48.2985463549472)) ;
#62207 = CARTESIAN_POINT('Ctrl Pts',(181.0015738731,584.470313890453,-48.2958079822345)) ;
#62208 = CARTESIAN_POINT('Ctrl Pts',(181.069021994091,584.533773710968,-48.2892386090915)) ;
#62209 = CARTESIAN_POINT('Ctrl Pts',(181.106114365626,584.572194870677,-48.2853737720822)) ;
#62210 = CARTESIAN_POINT('Ctrl Pts',(181.229463972879,584.712900760287,-48.2717640399015)) ;
#62211 = CARTESIAN_POINT('Ctrl Pts',(181.305217422334,584.823746490405,-48.2620265180577)) ;
#62212 = CARTESIAN_POINT('Ctrl Pts',(181.390704991926,584.988287792071,-48.2492303228113)) ;
#62213 = CARTESIAN_POINT('Ctrl Pts',(181.412367059358,585.035186857292,-48.245741817317)) ;
#62214 = CARTESIAN_POINT('Ctrl Pts',(181.453055904458,585.13525110279,-48.2385989756737)) ;
#62215 = CARTESIAN_POINT('Ctrl Pts',(181.471630510021,585.188529314956,-48.2349638650926)) ;
#62216 = CARTESIAN_POINT('Ctrl Pts',(181.50585425358,585.305477954741,-48.2272604845742)) ;
#62217 = CARTESIAN_POINT('Ctrl Pts',(181.520521678923,585.369335839379,-48.2232240970912)) ;
#62218 = CARTESIAN_POINT('Ctrl Pts',(181.551870665631,585.555485732305,-48.2116689419256)) ;
#62219 = CARTESIAN_POINT('Ctrl Pts',(181.558782590793,585.678956048735,-48.204275786974)) ;
#62220 = CARTESIAN_POINT('Ctrl Pts',(181.550318332245,585.832884809784,-48.1942591949648)) ;
#62221 = CARTESIAN_POINT('Ctrl Pts',(181.547764491754,585.863677390899,-48.1922131102694)) ;
#62222 = CARTESIAN_POINT('Ctrl Pts',(181.540098764288,585.932730875518,-48.1874988546373)) ;
#62223 = CARTESIAN_POINT('Ctrl Pts',(181.534510895044,585.970917420704,-48.1848098243074)) ;
#62224 = CARTESIAN_POINT('Ctrl Pts',(181.510419429662,586.103290542427,-48.1752777881762)) ;
#62225 = CARTESIAN_POINT('Ctrl Pts',(181.485110124035,586.196043274498,-48.1682341296462)) ;
#62226 = CARTESIAN_POINT('Ctrl Pts',(181.451959398854,586.286097166427,-48.1612709156719)) ;
#62227 = CARTESIAN_POINT('Ctrl Pts',(181.451958155526,586.286100543914,-49.0537403040458)) ;
#62228 = CARTESIAN_POINT('Ctrl Pts',(181.442367045837,586.312154604425,-49.0520465268598)) ;
#62229 = CARTESIAN_POINT('Ctrl Pts',(181.432121158642,586.337978443246,-49.0503552040013)) ;
#62230 = CARTESIAN_POINT('Ctrl Pts',(181.394454146755,586.426391658561,-49.0444887226731)) ;
#62231 = CARTESIAN_POINT('Ctrl Pts',(181.36384202225,586.487526345688,-49.0402953049949)) ;
#62232 = CARTESIAN_POINT('Ctrl Pts',(181.300623160239,586.596493277071,-49.0323589745846)) ;
#62233 = CARTESIAN_POINT('Ctrl Pts',(181.269112464359,586.644838511793,-49.0286536151324)) ;
#62234 = CARTESIAN_POINT('Ctrl Pts',(181.20506708751,586.73276501538,-49.0214791337567)) ;
#62235 = CARTESIAN_POINT('Ctrl Pts',(181.173090421842,586.772669727805,-49.0180352194983)) ;
#62236 = CARTESIAN_POINT('Ctrl Pts',(181.045386686211,586.917818712398,-49.0047277504003)) ;
#62237 = CARTESIAN_POINT('Ctrl Pts',(180.938167836179,587.012111900912,-48.9943543232183)) ;
#62238 = CARTESIAN_POINT('Ctrl Pts',(180.77850569482,587.119833939444,-48.9803618603223)) ;
#62239 = CARTESIAN_POINT('Ctrl Pts',(180.735436557747,587.146129635776,-48.9767187236512)) ;
#62240 = CARTESIAN_POINT('Ctrl Pts',(180.657977597534,587.188720591738,-48.9704631244622)) ;
#62241 = CARTESIAN_POINT('Ctrl Pts',(180.624098116846,587.205868935525,-48.9678206681173)) ;
#62242 = CARTESIAN_POINT('Ctrl Pts',(180.561256328243,587.235023240386,-48.9631255841729)) ;
#62243 = CARTESIAN_POINT('Ctrl Pts',(180.53248750204,587.247397015689,-48.9610551831426)) ;
#62244 = CARTESIAN_POINT('Ctrl Pts',(180.391846290724,587.303245000643,-48.9512392153902)) ;
#62245 = CARTESIAN_POINT('Ctrl Pts',(180.275831654044,587.335361323865,-48.9440332098066)) ;
#62246 = CARTESIAN_POINT('Ctrl Pts',(180.091559152841,587.365491014052,-48.9326153625952)) ;
#62247 = CARTESIAN_POINT('Ctrl Pts',(180.025176612528,587.372289398275,-48.9285112382682)) ;
#62248 = CARTESIAN_POINT('Ctrl Pts',(179.901573398395,587.377490501998,-48.9207000501558)) ;
#62249 = CARTESIAN_POINT('Ctrl Pts',(179.844498083288,587.376959616676,-48.9170269918634)) ;
#62250 = CARTESIAN_POINT('Ctrl Pts',(179.735888500295,587.37036569637,-48.9098376558024)) ;
#62251 = CARTESIAN_POINT('Ctrl Pts',(179.684389951565,587.364821273548,-48.9063424581797)) ;
#62252 = CARTESIAN_POINT('Ctrl Pts',(179.50018944562,587.336257913998,-48.893486501548)) ;
#62253 = CARTESIAN_POINT('Ctrl Pts',(179.370153955682,587.299577166926,-48.8836886288801)) ;
#62254 = CARTESIAN_POINT('Ctrl Pts',(179.196977890182,587.22718490761,-48.8700421522576)) ;
#62255 = CARTESIAN_POINT('Ctrl Pts',(179.148982901137,587.204369289545,-48.8661983357896)) ;
#62256 = CARTESIAN_POINT('Ctrl Pts',(179.067625799373,587.160810119648,-48.859655666143)) ;
#62257 = CARTESIAN_POINT('Ctrl Pts',(179.033753333724,587.141107642177,-48.8569233855499)) ;
#62258 = CARTESIAN_POINT('Ctrl Pts',(178.974361948848,587.103697949959,-48.8521586859097)) ;
#62259 = CARTESIAN_POINT('Ctrl Pts',(178.948586800191,587.086439142605,-48.850103824995)) ;
#62260 = CARTESIAN_POINT('Ctrl Pts',(178.834401945849,587.005274691068,-48.8409993708825)) ;
#62261 = CARTESIAN_POINT('Ctrl Pts',(178.751905171419,586.933491905227,-48.8343959081399)) ;
#62262 = CARTESIAN_POINT('Ctrl Pts',(178.627491283675,586.801687413218,-48.8233257170684)) ;
#62263 = CARTESIAN_POINT('Ctrl Pts',(178.58143371168,586.746067414824,-48.8189073122065)) ;
#62264 = CARTESIAN_POINT('Ctrl Pts',(178.504311454519,586.639557009385,-48.8106376494352)) ;
#62265 = CARTESIAN_POINT('Ctrl Pts',(178.472093520653,586.589651834192,-48.8068313364632)) ;
#62266 = CARTESIAN_POINT('Ctrl Pts',(178.417532366746,586.494323749243,-48.7995971454438)) ;
#62267 = CARTESIAN_POINT('Ctrl Pts',(178.394462227524,586.449396804079,-48.7962020175189)) ;
#62268 = CARTESIAN_POINT('Ctrl Pts',(178.332902696884,586.31479994524,-48.786034767644)) ;
#62269 = CARTESIAN_POINT('Ctrl Pts',(178.300210156406,586.222727714971,-48.7790724057875)) ;
#62270 = CARTESIAN_POINT('Ctrl Pts',(178.24953364727,586.02709734253,-48.7644060715532)) ;
#62271 = CARTESIAN_POINT('Ctrl Pts',(178.232898034086,585.923606423054,-48.7567170633223)) ;
#62272 = CARTESIAN_POINT('Ctrl Pts',(178.223788995917,585.784254712189,-48.7468898710452)) ;
#62273 = CARTESIAN_POINT('Ctrl Pts',(178.2226068193,585.749207279291,-48.7444639976611)) ;
#62274 = CARTESIAN_POINT('Ctrl Pts',(178.222460322143,585.681036389742,-48.7398667560257)) ;
#62275 = CARTESIAN_POINT('Ctrl Pts',(178.223376160584,585.647930394898,-48.7376912221731)) ;
#62276 = CARTESIAN_POINT('Ctrl Pts',(178.235112625915,585.443939353843,-48.7245176558765)) ;
#62277 = CARTESIAN_POINT('Ctrl Pts',(178.271237097301,585.275526077541,-48.7145486788468)) ;
#62278 = CARTESIAN_POINT('Ctrl Pts',(178.354107592696,585.058795222922,-48.6999919552509)) ;
#62279 = CARTESIAN_POINT('Ctrl Pts',(178.378898080143,585.003270210825,-48.6961054971068)) ;
#62280 = CARTESIAN_POINT('Ctrl Pts',(178.429836563856,584.904123752046,-48.6887778830967)) ;
#62281 = CARTESIAN_POINT('Ctrl Pts',(178.455054280415,584.860106137367,-48.6853738374054)) ;
#62282 = CARTESIAN_POINT('Ctrl Pts',(178.561582772263,584.692393615485,-48.6717467517413)) ;
#62283 = CARTESIAN_POINT('Ctrl Pts',(178.657205466419,584.578627161155,-48.6609542442595)) ;
#62284 = CARTESIAN_POINT('Ctrl Pts',(178.80360883029,584.445251161344,-48.6465667609292)) ;
#62285 = CARTESIAN_POINT('Ctrl Pts',(178.842168195389,584.413182836259,-48.6429467251942)) ;
#62286 = CARTESIAN_POINT('Ctrl Pts',(178.912262244202,584.360049409252,-48.6367234201416)) ;
#62287 = CARTESIAN_POINT('Ctrl Pts',(178.943180031159,584.338229414607,-48.6340905778274)) ;
#62288 = CARTESIAN_POINT('Ctrl Pts',(179.001108605256,584.300234666821,-48.6293961419528)) ;
#62289 = CARTESIAN_POINT('Ctrl Pts',(179.027883497909,584.28373775712,-48.6273175512703)) ;
#62290 = CARTESIAN_POINT('Ctrl Pts',(179.157926532345,584.208607252175,-48.6175774891948)) ;
#62291 = CARTESIAN_POINT('Ctrl Pts',(179.266812928399,584.160360557507,-48.6104404346335)) ;
#62292 = CARTESIAN_POINT('Ctrl Pts',(179.443693055667,584.103653972866,-48.5990792733714)) ;
#62293 = CARTESIAN_POINT('Ctrl Pts',(179.508639704786,584.087073388664,-48.5949567190845)) ;
#62294 = CARTESIAN_POINT('Ctrl Pts',(179.630560220302,584.063665472465,-48.5871178953679)) ;
#62295 = CARTESIAN_POINT('Ctrl Pts',(179.687228202661,584.055783271736,-48.5834361639714)) ;
#62296 = CARTESIAN_POINT('Ctrl Pts',(179.79577160293,584.046343517895,-48.5762371771017)) ;
#62297 = CARTESIAN_POINT('Ctrl Pts',(179.847534112949,584.044265114454,-48.57274142944)) ;
#62298 = CARTESIAN_POINT('Ctrl Pts',(180.034557113231,584.045474966471,-48.5598422314382)) ;
#62299 = CARTESIAN_POINT('Ctrl Pts',(180.169178146,584.062817604246,-48.5499964691717)) ;
#62300 = CARTESIAN_POINT('Ctrl Pts',(180.351509828747,584.109313062743,-48.5363141986945)) ;
#62301 = CARTESIAN_POINT('Ctrl Pts',(180.402177987646,584.124839841457,-48.5324809233746)) ;
#62302 = CARTESIAN_POINT('Ctrl Pts',(180.488823509572,584.155981592902,-48.5259530604896)) ;
#62303 = CARTESIAN_POINT('Ctrl Pts',(180.52515078838,584.170501267112,-48.5232252152166)) ;
#62304 = CARTESIAN_POINT('Ctrl Pts',(180.589272508025,584.198787475713,-48.5184676721755)) ;
#62305 = CARTESIAN_POINT('Ctrl Pts',(180.617254126349,584.212074933187,-48.5164156067623)) ;
#62306 = CARTESIAN_POINT('Ctrl Pts',(180.742381452353,584.27582783167,-48.5072888127749)) ;
#62307 = CARTESIAN_POINT('Ctrl Pts',(180.834791665601,584.335018464639,-48.500664618126)) ;
#62308 = CARTESIAN_POINT('Ctrl Pts',(180.97728528003,584.447492319991,-48.4895788123734)) ;
#62309 = CARTESIAN_POINT('Ctrl Pts',(181.030877204606,584.495747206756,-48.485166742301)) ;
#62310 = CARTESIAN_POINT('Ctrl Pts',(181.122596725458,584.589784719551,-48.4769063994183)) ;
#62311 = CARTESIAN_POINT('Ctrl Pts',(181.161716030833,584.634430728337,-48.4731028998787)) ;
#62312 = CARTESIAN_POINT('Ctrl Pts',(181.229553247931,584.720740420858,-48.4658729695989)) ;
#62313 = CARTESIAN_POINT('Ctrl Pts',(181.25891591204,584.761809283354,-48.4624792060419)) ;
#62314 = CARTESIAN_POINT('Ctrl Pts',(181.341261194128,584.888798207312,-48.4520827394775)) ;
#62315 = CARTESIAN_POINT('Ctrl Pts',(181.38834236011,584.978250184839,-48.4448705192446)) ;
#62316 = CARTESIAN_POINT('Ctrl Pts',(181.45644186305,585.142168860621,-48.4319797407391)) ;
#62317 = CARTESIAN_POINT('Ctrl Pts',(181.480926438181,585.214887932324,-48.4263692302537)) ;
#62318 = CARTESIAN_POINT('Ctrl Pts',(181.512464138701,585.335477694045,-48.4174323641217)) ;
#62319 = CARTESIAN_POINT('Ctrl Pts',(181.522598529847,585.382428474779,-48.4140411988247)) ;
#62320 = CARTESIAN_POINT('Ctrl Pts',(181.535685102336,585.458958414956,-48.4087209712909)) ;
#62321 = CARTESIAN_POINT('Ctrl Pts',(181.539898578278,585.48828617496,-48.4067341949588)) ;
#62322 = CARTESIAN_POINT('Ctrl Pts',(181.549578169499,585.571345527602,-48.40124154138)) ;
#62323 = CARTESIAN_POINT('Ctrl Pts',(181.553217974826,585.625251824746,-48.3978249627858)) ;
#62324 = CARTESIAN_POINT('Ctrl Pts',(181.55628927666,585.788594905675,-48.3876658151951)) ;
#62325 = CARTESIAN_POINT('Ctrl Pts',(181.547572900447,585.897883036014,-48.3811145423157)) ;
#62326 = CARTESIAN_POINT('Ctrl Pts',(181.515500295583,586.076170512365,-48.3698980979893)) ;
#62327 = CARTESIAN_POINT('Ctrl Pts',(181.498242999368,586.145906175836,-48.3653750592674)) ;
#62328 = CARTESIAN_POINT('Ctrl Pts',(181.468894521793,586.23842569739,-48.3590566210714)) ;
#62329 = CARTESIAN_POINT('Ctrl Pts',(181.46069644486,586.262363153745,-48.3573926027051)) ;
#62330 = CARTESIAN_POINT('Ctrl Pts',(181.45195815042,586.286100557784,-48.3557104975402)) ;
#62331 = CARTESIAN_POINT('Origin',(29.8885276254069,535.710565160562,-48.522160171753)) ;
#62332 = CARTESIAN_POINT('Ctrl Pts',(31.4519498095241,536.286123215158,-48.8631108318347)) ;
#62333 = CARTESIAN_POINT('Ctrl Pts',(31.4454204319241,536.303859347433,-48.8618790238479)) ;
#62334 = CARTESIAN_POINT('Ctrl Pts',(31.4385896048817,536.321483393227,-48.8606324540074)) ;
#62335 = CARTESIAN_POINT('Ctrl Pts',(31.4195487156195,536.368233484221,-48.8572553542794)) ;
#62336 = CARTESIAN_POINT('Ctrl Pts',(31.4068100232744,536.397129905838,-48.8550911380751)) ;
#62337 = CARTESIAN_POINT('Ctrl Pts',(31.3434502247697,536.530457439493,-48.8447948905069)) ;
#62338 = CARTESIAN_POINT('Ctrl Pts',(31.2828288436453,536.629773665628,-48.8362451218479)) ;
#62339 = CARTESIAN_POINT('Ctrl Pts',(31.1713604166045,536.775676648282,-48.8229308955179)) ;
#62340 = CARTESIAN_POINT('Ctrl Pts',(31.1271033933445,536.826833134008,-48.8180829824099)) ;
#62341 = CARTESIAN_POINT('Ctrl Pts',(31.0398039156606,536.916136337417,-48.8093294678809)) ;
#62342 = CARTESIAN_POINT('Ctrl Pts',(30.9976603212316,536.955018864236,-48.8053978137976)) ;
#62343 = CARTESIAN_POINT('Ctrl Pts',(30.9142162610716,537.024391960484,-48.7981277594601)) ;
#62344 = CARTESIAN_POINT('Ctrl Pts',(30.8733495719742,537.055297371613,-48.794774374771)) ;
#62345 = CARTESIAN_POINT('Ctrl Pts',(30.7156180138062,537.16352740695,-48.7824936744457)) ;
#62346 = CARTESIAN_POINT('Ctrl Pts',(30.5905858503303,537.227896599009,-48.7740943799516)) ;
#62347 = CARTESIAN_POINT('Ctrl Pts',(30.4109162759848,537.293373274499,-48.7623513479098)) ;
#62348 = CARTESIAN_POINT('Ctrl Pts',(30.3620887671397,537.308661068351,-48.7591832191955)) ;
#62349 = CARTESIAN_POINT('Ctrl Pts',(30.2756551508876,537.33141398117,-48.7534956830553)) ;
#62350 = CARTESIAN_POINT('Ctrl Pts',(30.2383503147815,537.339872410809,-48.7510156211688)) ;
#62351 = CARTESIAN_POINT('Ctrl Pts',(30.1703921943881,537.352839841649,-48.7463976368524)) ;
#62352 = CARTESIAN_POINT('Ctrl Pts',(30.1398428321677,537.357791256459,-48.7442824094505)) ;
#62353 = CARTESIAN_POINT('Ctrl Pts',(29.987731379682,537.37811640213,-48.7336036163793)) ;
#62354 = CARTESIAN_POINT('Ctrl Pts',(29.8648738658647,537.380896271859,-48.7245582714606)) ;
#62355 = CARTESIAN_POINT('Ctrl Pts',(29.6773821562647,537.364436380474,-48.7109266828766)) ;
#62356 = CARTESIAN_POINT('Ctrl Pts',(29.6123260643387,537.354823869722,-48.706222695061)) ;
#62357 = CARTESIAN_POINT('Ctrl Pts',(29.4927138369646,537.329848175287,-48.6976722198205)) ;
#62358 = CARTESIAN_POINT('Ctrl Pts',(29.4380435956142,537.315498654276,-48.6938029609648)) ;
#62359 = CARTESIAN_POINT('Ctrl Pts',(29.3350882176055,537.282798068093,-48.6865754484628)) ;
#62360 = CARTESIAN_POINT('Ctrl Pts',(29.2867209456151,537.264927143662,-48.6832058505681)) ;
#62361 = CARTESIAN_POINT('Ctrl Pts',(29.1152457585742,537.192362540044,-48.6712701212747)) ;
#62362 = CARTESIAN_POINT('Ctrl Pts',(28.998057623687,537.1250453891,-48.6631769723867)) ;
#62363 = CARTESIAN_POINT('Ctrl Pts',(28.8478081536067,537.012589980382,-48.651666825322)) ;
#62364 = CARTESIAN_POINT('Ctrl Pts',(28.8069147261988,536.978823177535,-48.6483901126609)) ;
#62365 = CARTESIAN_POINT('Ctrl Pts',(28.7387935325007,536.916879526409,-48.6425409460339)) ;
#62366 = CARTESIAN_POINT('Ctrl Pts',(28.7108205091927,536.889585160937,-48.640011290118)) ;
#62367 = CARTESIAN_POINT('Ctrl Pts',(28.6626605689291,536.839168600924,-48.6353630801209)) ;
#62368 = CARTESIAN_POINT('Ctrl Pts',(28.6421055286096,536.816425509455,-48.6332708921402)) ;
#62369 = CARTESIAN_POINT('Ctrl Pts',(28.549392551664,536.707974202544,-48.6233549760745)) ;
#62370 = CARTESIAN_POINT('Ctrl Pts',(28.4853744705787,536.615697813506,-48.6151208936581)) ;
#62371 = CARTESIAN_POINT('Ctrl Pts',(28.3967325088784,536.455640164154,-48.6018304252883)) ;
#62372 = CARTESIAN_POINT('Ctrl Pts',(28.3663571120631,536.391438263774,-48.5967239532406)) ;
#62373 = CARTESIAN_POINT('Ctrl Pts',(28.318490152092,536.270910588629,-48.5876092144972)) ;
#62374 = CARTESIAN_POINT('Ctrl Pts',(28.2997133518178,536.215218872086,-48.5835687403659)) ;
#62375 = CARTESIAN_POINT('Ctrl Pts',(28.2704246069845,536.110333400511,-48.5762574203631)) ;
#62376 = CARTESIAN_POINT('Ctrl Pts',(28.259121460215,536.061433331987,-48.5729636965277)) ;
#62377 = CARTESIAN_POINT('Ctrl Pts',(28.2329604690923,535.91927585596,-48.5636579051796)) ;
#62378 = CARTESIAN_POINT('Ctrl Pts',(28.2237959757104,535.825170423279,-48.5578349424046)) ;
#62379 = CARTESIAN_POINT('Ctrl Pts',(28.2213777302767,535.625940040585,-48.5456522682261)) ;
#62380 = CARTESIAN_POINT('Ctrl Pts',(28.2300060161302,535.521219947478,-48.5393305262647)) ;
#62381 = CARTESIAN_POINT('Ctrl Pts',(28.2547562692319,535.382462152631,-48.5303194648317)) ;
#62382 = CARTESIAN_POINT('Ctrl Pts',(28.2622522500082,535.347125600081,-48.5279665035358)) ;
#62383 = CARTESIAN_POINT('Ctrl Pts',(28.2785345438782,535.28103077109,-48.5234070892657)) ;
#62384 = CARTESIAN_POINT('Ctrl Pts',(28.2870698025533,535.250228593131,-48.521213582298)) ;
#62385 = CARTESIAN_POINT('Ctrl Pts',(28.3077363051077,535.183200708031,-48.5163151105162)) ;
#62386 = CARTESIAN_POINT('Ctrl Pts',(28.3202392904089,535.147106435088,-48.5135955718699)) ;
#62387 = CARTESIAN_POINT('Ctrl Pts',(28.3664397794752,535.027222173313,-48.5043512989633)) ;
#62388 = CARTESIAN_POINT('Ctrl Pts',(28.405704959675,534.945747298854,-48.4977219557218)) ;
#62389 = CARTESIAN_POINT('Ctrl Pts',(28.4934975528425,534.796026881753,-48.4851916210285)) ;
#62390 = CARTESIAN_POINT('Ctrl Pts',(28.54094623985,534.727449032701,-48.4792907597104)) ;
#62391 = CARTESIAN_POINT('Ctrl Pts',(28.6250116790044,534.62354155731,-48.4701270667798)) ;
#62392 = CARTESIAN_POINT('Ctrl Pts',(28.6584532530235,534.585838145977,-48.4667460351904)) ;
#62393 = CARTESIAN_POINT('Ctrl Pts',(28.7356312282708,534.506392334471,-48.4594653505644)) ;
#62394 = CARTESIAN_POINT('Ctrl Pts',(28.7800337381957,534.465396515331,-48.4556023595078)) ;
#62395 = CARTESIAN_POINT('Ctrl Pts',(28.8843572636623,534.379091212892,-48.4471069074285)) ;
#62396 = CARTESIAN_POINT('Ctrl Pts',(28.9453102389704,534.335238677291,-48.4425257259063)) ;
#62397 = CARTESIAN_POINT('Ctrl Pts',(29.0949855695054,534.242200691369,-48.4317667231819)) ;
#62398 = CARTESIAN_POINT('Ctrl Pts',(29.1856389041805,534.196714042877,-48.4256155216174)) ;
#62399 = CARTESIAN_POINT('Ctrl Pts',(29.3090086461524,534.148292666523,-48.4170224739412)) ;
#62400 = CARTESIAN_POINT('Ctrl Pts',(29.3384886336853,534.137671469888,-48.4149521926076)) ;
#62401 = CARTESIAN_POINT('Ctrl Pts',(29.4036597539175,534.116247595698,-48.4103055797973)) ;
#62402 = CARTESIAN_POINT('Ctrl Pts',(29.4394467489295,534.105800020707,-48.4077136888816)) ;
#62403 = CARTESIAN_POINT('Ctrl Pts',(29.5788803365027,534.070122923199,-48.3975380933083)) ;
#62404 = CARTESIAN_POINT('Ctrl Pts',(29.6845063342131,534.053668596351,-48.3896855205373)) ;
#62405 = CARTESIAN_POINT('Ctrl Pts',(29.8813784485332,534.042121123562,-48.3754021542157)) ;
#62406 = CARTESIAN_POINT('Ctrl Pts',(29.9720738372828,534.044197455524,-48.3689563092193)) ;
#62407 = CARTESIAN_POINT('Ctrl Pts',(30.1119849461126,534.058859300089,-48.3592958865846)) ;
#62408 = CARTESIAN_POINT('Ctrl Pts',(30.1615495460964,534.066325093203,-48.3559270262173)) ;
#62409 = CARTESIAN_POINT('Ctrl Pts',(30.2685177041821,534.087409153804,-48.348746804829)) ;
#62410 = CARTESIAN_POINT('Ctrl Pts',(30.3256873163134,534.101863643287,-48.3449677232646)) ;
#62411 = CARTESIAN_POINT('Ctrl Pts',(30.4502107481799,534.140478632447,-48.3367674456449)) ;
#62412 = CARTESIAN_POINT('Ctrl Pts',(30.5170165955757,534.166006242255,-48.3323900406877)) ;
#62413 = CARTESIAN_POINT('Ctrl Pts',(30.6824974099923,534.24175983126,-48.3212747043782)) ;
#62414 = CARTESIAN_POINT('Ctrl Pts',(30.7781710719915,534.297658692539,-48.3145903065853)) ;
#62415 = CARTESIAN_POINT('Ctrl Pts',(30.89246928846,534.380676967541,-48.3054068684597)) ;
#62416 = CARTESIAN_POINT('Ctrl Pts',(30.9168412750927,534.399431150226,-48.3033692886197)) ;
#62417 = CARTESIAN_POINT('Ctrl Pts',(30.9707476966025,534.443340014193,-48.2986496486544)) ;
#62418 = CARTESIAN_POINT('Ctrl Pts',(30.9999477732322,534.468870957812,-48.2959456836003)) ;
#62419 = CARTESIAN_POINT('Ctrl Pts',(31.0663987464412,534.53119484749,-48.289488103178)) ;
#62420 = CARTESIAN_POINT('Ctrl Pts',(31.1028596158002,534.568771895611,-48.2857020423812)) ;
#62421 = CARTESIAN_POINT('Ctrl Pts',(31.2279575461114,534.710480065302,-48.2719588210758)) ;
#62422 = CARTESIAN_POINT('Ctrl Pts',(31.3054876975347,534.823727772674,-48.2619993719887)) ;
#62423 = CARTESIAN_POINT('Ctrl Pts',(31.3919382314065,534.990872532076,-48.24902413267)) ;
#62424 = CARTESIAN_POINT('Ctrl Pts',(31.4134391968092,535.03762634286,-48.2455520136143)) ;
#62425 = CARTESIAN_POINT('Ctrl Pts',(31.454065443006,535.137961759983,-48.2383995061277)) ;
#62426 = CARTESIAN_POINT('Ctrl Pts',(31.4726807808057,535.191678584579,-48.2347403570559)) ;
#62427 = CARTESIAN_POINT('Ctrl Pts',(31.5070335174782,535.310054343029,-48.2269553265335)) ;
#62428 = CARTESIAN_POINT('Ctrl Pts',(31.5217179082243,535.374915461387,-48.2228632113497)) ;
#62429 = CARTESIAN_POINT('Ctrl Pts',(31.5519263648473,535.558791651747,-48.2114628275883)) ;
#62430 = CARTESIAN_POINT('Ctrl Pts',(31.5585322927592,535.678834988884,-48.2042620913468)) ;
#62431 = CARTESIAN_POINT('Ctrl Pts',(31.5505560086946,535.829694152295,-48.1944607941727)) ;
#62432 = CARTESIAN_POINT('Ctrl Pts',(31.5480328185513,535.860806461547,-48.1923970588143)) ;
#62433 = CARTESIAN_POINT('Ctrl Pts',(31.54053205366,535.929336850383,-48.1877251296333)) ;
#62434 = CARTESIAN_POINT('Ctrl Pts',(31.5351541337926,535.966690612461,-48.1850996528049)) ;
#62435 = CARTESIAN_POINT('Ctrl Pts',(31.5113175405677,536.099990816266,-48.1755200396746)) ;
#62436 = CARTESIAN_POINT('Ctrl Pts',(31.4856974378523,536.194451838716,-48.1683484248333)) ;
#62437 = CARTESIAN_POINT('Ctrl Pts',(31.451951253523,536.286119292724,-48.161260329976)) ;
#62438 = CARTESIAN_POINT('Ctrl Pts',(31.4519498093678,536.286123215583,-49.053781357604)) ;
#62439 = CARTESIAN_POINT('Ctrl Pts',(31.4421205686183,536.312822960126,-49.0520449154176)) ;
#62440 = CARTESIAN_POINT('Ctrl Pts',(31.4316037221729,536.339280832236,-49.0503110614434)) ;
#62441 = CARTESIAN_POINT('Ctrl Pts',(31.3937051203419,536.427928965283,-49.0444228981946)) ;
#62442 = CARTESIAN_POINT('Ctrl Pts',(31.3632095023766,536.488692706009,-49.0402501160774)) ;
#62443 = CARTESIAN_POINT('Ctrl Pts',(31.3002108353399,536.597138557633,-49.0323447179619)) ;
#62444 = CARTESIAN_POINT('Ctrl Pts',(31.2687782099982,536.645321263705,-49.0286488811754)) ;
#62445 = CARTESIAN_POINT('Ctrl Pts',(31.2047763014379,536.733142823493,-49.0214786452748)) ;
#62446 = CARTESIAN_POINT('Ctrl Pts',(31.1727448169078,536.773090852571,-49.0180286330047)) ;
#62447 = CARTESIAN_POINT('Ctrl Pts',(31.045525067889,536.917582596926,-49.0047712786818)) ;
#62448 = CARTESIAN_POINT('Ctrl Pts',(30.9390154262382,537.011331975432,-48.9944625987745)) ;
#62449 = CARTESIAN_POINT('Ctrl Pts',(30.7799073340656,537.118961076065,-48.9805020290253)) ;
#62450 = CARTESIAN_POINT('Ctrl Pts',(30.736545836289,537.145487669707,-48.9768303167691)) ;
#62451 = CARTESIAN_POINT('Ctrl Pts',(30.6586460790295,537.188376554804,-48.9705341909782)) ;
#62452 = CARTESIAN_POINT('Ctrl Pts',(30.6246301766632,537.205611172816,-48.9678792523042)) ;
#62453 = CARTESIAN_POINT('Ctrl Pts',(30.5617479321509,537.234803998063,-48.963178571334)) ;
#62454 = CARTESIAN_POINT('Ctrl Pts',(30.5330825030713,537.247145373332,-48.9611142101719)) ;
#62455 = CARTESIAN_POINT('Ctrl Pts',(30.4062318452574,537.29758362935,-48.9522545644049)) ;
#62456 = CARTESIAN_POINT('Ctrl Pts',(30.3048952988687,537.327132303877,-48.9458690541033)) ;
#62457 = CARTESIAN_POINT('Ctrl Pts',(30.1291327364573,537.360742121137,-48.9349458198824)) ;
#62458 = CARTESIAN_POINT('Ctrl Pts',(30.0559966536166,537.369760128288,-48.930444779145)) ;
#62459 = CARTESIAN_POINT('Ctrl Pts',(29.9226393734231,537.377294919229,-48.9220561003875)) ;
#62460 = CARTESIAN_POINT('Ctrl Pts',(29.8626383459254,537.377442512114,-48.9182165652561)) ;
#62461 = CARTESIAN_POINT('Ctrl Pts',(29.7519770257693,537.371738297544,-48.9109261301689)) ;
#62462 = CARTESIAN_POINT('Ctrl Pts',(29.7013411892077,537.366796578201,-48.9075090647033)) ;
#62463 = CARTESIAN_POINT('Ctrl Pts',(29.5613095774384,537.346627004707,-48.8977970203768)) ;
#62464 = CARTESIAN_POINT('Ctrl Pts',(29.4728222904853,537.326409953065,-48.8913497197765)) ;
#62465 = CARTESIAN_POINT('Ctrl Pts',(29.2846788589956,537.266942440775,-48.877062579661)) ;
#62466 = CARTESIAN_POINT('Ctrl Pts',(29.1862519074647,537.225079489781,-48.8692076446659)) ;
#62467 = CARTESIAN_POINT('Ctrl Pts',(29.0596865745791,537.156239416906,-48.8590246154616)) ;
#62468 = CARTESIAN_POINT('Ctrl Pts',(29.0274759559766,537.137289427105,-48.8564273766625)) ;
#62469 = CARTESIAN_POINT('Ctrl Pts',(28.9691398590744,537.100273251785,-48.8517500090167)) ;
#62470 = CARTESIAN_POINT('Ctrl Pts',(28.9428432952346,537.082514045143,-48.8496551588635)) ;
#62471 = CARTESIAN_POINT('Ctrl Pts',(28.8228277652379,536.996371012458,-48.8400846281266)) ;
#62472 = CARTESIAN_POINT('Ctrl Pts',(28.7358964591998,536.919060786394,-48.8331020510572)) ;
#62473 = CARTESIAN_POINT('Ctrl Pts',(28.6120290203898,536.783271594557,-48.8218629018146)) ;
#62474 = CARTESIAN_POINT('Ctrl Pts',(28.5694611510534,536.730472224843,-48.8176949640231)) ;
#62475 = CARTESIAN_POINT('Ctrl Pts',(28.4969242682058,536.628336572284,-48.8097900613749)) ;
#62476 = CARTESIAN_POINT('Ctrl Pts',(28.4660742189961,536.579754065192,-48.8060891793899)) ;
#62477 = CARTESIAN_POINT('Ctrl Pts',(28.4124117211227,536.484712618079,-48.7988812822438)) ;
#62478 = CARTESIAN_POINT('Ctrl Pts',(28.3891303541027,536.438596229111,-48.79539733326)) ;
#62479 = CARTESIAN_POINT('Ctrl Pts',(28.3117554211104,536.265815650094,-48.7823481043735)) ;
#62480 = CARTESIAN_POINT('Ctrl Pts',(28.2712856127787,536.133682124281,-48.7723185326411)) ;
#62481 = CARTESIAN_POINT('Ctrl Pts',(28.2385286580393,535.946741599366,-48.7585210768233)) ;
#62482 = CARTESIAN_POINT('Ctrl Pts',(28.2319437995907,535.894973950611,-48.7547483986554)) ;
#62483 = CARTESIAN_POINT('Ctrl Pts',(28.2247186035574,535.80435638508,-48.7483067016716)) ;
#62484 = CARTESIAN_POINT('Ctrl Pts',(28.2229870553385,535.76563313255,-48.7456054799053)) ;
#62485 = CARTESIAN_POINT('Ctrl Pts',(28.2223032057972,535.695809024691,-48.7408674607804)) ;
#62486 = CARTESIAN_POINT('Ctrl Pts',(28.2228682259566,535.664734565818,-48.7388097405462)) ;
#62487 = CARTESIAN_POINT('Ctrl Pts',(28.2292703114838,535.526135406332,-48.7297971737671)) ;
#62488 = CARTESIAN_POINT('Ctrl Pts',(28.244654448591,535.419297890581,-48.7232748848117)) ;
#62489 = CARTESIAN_POINT('Ctrl Pts',(28.2875103192788,535.244113187678,-48.7122620083713)) ;
#62490 = CARTESIAN_POINT('Ctrl Pts',(28.3093700686501,535.17475338164,-48.7078152279912)) ;
#62491 = CARTESIAN_POINT('Ctrl Pts',(28.3572599854346,535.051533722027,-48.6995057005265)) ;
#62492 = CARTESIAN_POINT('Ctrl Pts',(28.3817935899067,534.997224954907,-48.6956890215672)) ;
#62493 = CARTESIAN_POINT('Ctrl Pts',(28.4323434189617,534.89962725477,-48.6884528302141)) ;
#62494 = CARTESIAN_POINT('Ctrl Pts',(28.4575210253998,534.855982290588,-48.6850670821177)) ;
#62495 = CARTESIAN_POINT('Ctrl Pts',(28.5337123354556,534.736737625771,-48.6753505723693)) ;
#62496 = CARTESIAN_POINT('Ctrl Pts',(28.589003469921,534.664096461363,-48.6688633113024)) ;
#62497 = CARTESIAN_POINT('Ctrl Pts',(28.7211304162431,534.517221958731,-48.6545527618538)) ;
#62498 = CARTESIAN_POINT('Ctrl Pts',(28.799733098023,534.445096067159,-48.6467170500542)) ;
#62499 = CARTESIAN_POINT('Ctrl Pts',(28.9144493430178,534.358485740725,-48.6365565910861)) ;
#62500 = CARTESIAN_POINT('Ctrl Pts',(28.9449669730364,534.337014608568,-48.6339631071992)) ;
#62501 = CARTESIAN_POINT('Ctrl Pts',(29.0026784291749,534.299243107175,-48.6292931361974)) ;
#62502 = CARTESIAN_POINT('Ctrl Pts',(29.0296637178229,534.282660515776,-48.6272019168331)) ;
#62503 = CARTESIAN_POINT('Ctrl Pts',(29.1579836052175,534.208762064253,-48.6176079360074)) ;
#62504 = CARTESIAN_POINT('Ctrl Pts',(29.2646857390792,534.161392511465,-48.610603227281)) ;
#62505 = CARTESIAN_POINT('Ctrl Pts',(29.4398334887716,534.104698864893,-48.599346790951)) ;
#62506 = CARTESIAN_POINT('Ctrl Pts',(29.5054045485285,534.087805567345,-48.595185547943)) ;
#62507 = CARTESIAN_POINT('Ctrl Pts',(29.6282356498718,534.064021358175,-48.5872907661045)) ;
#62508 = CARTESIAN_POINT('Ctrl Pts',(29.6851755961976,534.056024397277,-48.5835931198444)) ;
#62509 = CARTESIAN_POINT('Ctrl Pts',(29.7938399477841,534.04645705887,-48.5763891853042)) ;
#62510 = CARTESIAN_POINT('Ctrl Pts',(29.8454467967628,534.044322519761,-48.572905819667)) ;
#62511 = CARTESIAN_POINT('Ctrl Pts',(30.0344919646107,534.045291275285,-48.559874997899)) ;
#62512 = CARTESIAN_POINT('Ctrl Pts',(30.1712819879578,534.062997633868,-48.5498654329698)) ;
#62513 = CARTESIAN_POINT('Ctrl Pts',(30.354861364568,534.110310902991,-48.5360839772566)) ;
#62514 = CARTESIAN_POINT('Ctrl Pts',(30.4047726488978,534.125707882412,-48.5323079446873)) ;
#62515 = CARTESIAN_POINT('Ctrl Pts',(30.490346221921,534.156578956215,-48.5258616200494)) ;
#62516 = CARTESIAN_POINT('Ctrl Pts',(30.5263448359197,534.171003999066,-48.5231590718303)) ;
#62517 = CARTESIAN_POINT('Ctrl Pts',(30.5902304062684,534.199229808851,-48.5184200337856)) ;
#62518 = CARTESIAN_POINT('Ctrl Pts',(30.6182933053543,534.212578675798,-48.5163625553282)) ;
#62519 = CARTESIAN_POINT('Ctrl Pts',(30.7419759751355,534.275712845991,-48.5073424179834)) ;
#62520 = CARTESIAN_POINT('Ctrl Pts',(30.8330148628258,534.333929549948,-48.5008134722058)) ;
#62521 = CARTESIAN_POINT('Ctrl Pts',(30.9749136575361,534.445418049187,-48.4897945293355)) ;
#62522 = CARTESIAN_POINT('Ctrl Pts',(31.0290298718726,534.49397753817,-48.4853486686103)) ;
#62523 = CARTESIAN_POINT('Ctrl Pts',(31.121438346133,534.588498110605,-48.4770399616097)) ;
#62524 = CARTESIAN_POINT('Ctrl Pts',(31.1607563698252,534.633283390558,-48.4732231409905)) ;
#62525 = CARTESIAN_POINT('Ctrl Pts',(31.2287526516097,534.719660932539,-48.4659857941293)) ;
#62526 = CARTESIAN_POINT('Ctrl Pts',(31.2581007393871,534.760637355124,-48.4625989939174)) ;
#62527 = CARTESIAN_POINT('Ctrl Pts',(31.3354475186327,534.879681277916,-48.4528511260399)) ;
#62528 = CARTESIAN_POINT('Ctrl Pts',(31.3789234103375,534.96045798176,-48.4463313835402)) ;
#62529 = CARTESIAN_POINT('Ctrl Pts',(31.4488258018835,535.120687430415,-48.4336674869897)) ;
#62530 = CARTESIAN_POINT('Ctrl Pts',(31.476347860618,535.199377132828,-48.4275632007741)) ;
#62531 = CARTESIAN_POINT('Ctrl Pts',(31.5108055247004,535.328109887804,-48.4179905323981)) ;
#62532 = CARTESIAN_POINT('Ctrl Pts',(31.5215571408749,535.376988614597,-48.4144491906886)) ;
#62533 = CARTESIAN_POINT('Ctrl Pts',(31.535137920552,535.455409534496,-48.408987186366)) ;
#62534 = CARTESIAN_POINT('Ctrl Pts',(31.5394058780599,535.484664384523,-48.4070008085166)) ;
#62535 = CARTESIAN_POINT('Ctrl Pts',(31.5491582978217,535.566754525897,-48.4015617422502)) ;
#62536 = CARTESIAN_POINT('Ctrl Pts',(31.5528988245009,535.619760350806,-48.3981950541164)) ;
#62537 = CARTESIAN_POINT('Ctrl Pts',(31.556609044588,535.783653537267,-48.387985950332)) ;
#62538 = CARTESIAN_POINT('Ctrl Pts',(31.5480563565674,535.894423330942,-48.381351556632)) ;
#62539 = CARTESIAN_POINT('Ctrl Pts',(31.5158807242769,536.074546829631,-48.3700259558492)) ;
#62540 = CARTESIAN_POINT('Ctrl Pts',(31.4985962826607,536.144659280053,-48.3654814587207)) ;
#62541 = CARTESIAN_POINT('Ctrl Pts',(31.4690916639415,536.237850375347,-48.3591199242599)) ;
#62542 = CARTESIAN_POINT('Ctrl Pts',(31.4607976500271,536.26208930646,-48.3574353418366)) ;
#62543 = CARTESIAN_POINT('Ctrl Pts',(31.4519498042747,536.286123229417,-48.3557322092704)) ;
#62544 = CARTESIAN_POINT('Origin',(29.8885276254157,585.710565160562,-48.522160171753)) ;
#62545 = CARTESIAN_POINT('Ctrl Pts',(31.451951903833,586.286117526255,-48.8631174034081)) ;
#62546 = CARTESIAN_POINT('Ctrl Pts',(31.445414274508,586.303876272495,-48.8618840380574)) ;
#62547 = CARTESIAN_POINT('Ctrl Pts',(31.4385744286486,586.321522643009,-48.8606358738028)) ;
#62548 = CARTESIAN_POINT('Ctrl Pts',(31.419518555509,586.36830420647,-48.8572563572135)) ;
#62549 = CARTESIAN_POINT('Ctrl Pts',(31.4067741013603,586.39720983254,-48.8550913335529)) ;
#62550 = CARTESIAN_POINT('Ctrl Pts',(31.3434426454872,586.530457434389,-48.8448006684502)) ;
#62551 = CARTESIAN_POINT('Ctrl Pts',(31.2828738267999,586.629693428051,-48.8362581932297)) ;
#62552 = CARTESIAN_POINT('Ctrl Pts',(31.1714618048038,586.775556366407,-48.8229485875785)) ;
#62553 = CARTESIAN_POINT('Ctrl Pts',(31.1271901091252,586.826738668564,-48.8180984699313)) ;
#62554 = CARTESIAN_POINT('Ctrl Pts',(31.0398659904931,586.916077711557,-48.809341775052)) ;
#62555 = CARTESIAN_POINT('Ctrl Pts',(30.9977140564705,586.954971606289,-48.8054090976715)) ;
#62556 = CARTESIAN_POINT('Ctrl Pts',(30.9142615818459,587.024356587802,-48.7981379971501)) ;
#62557 = CARTESIAN_POINT('Ctrl Pts',(30.8733957523154,587.055263559717,-48.7947845459238)) ;
#62558 = CARTESIAN_POINT('Ctrl Pts',(30.7156269223439,587.163527102585,-48.7825004886115)) ;
#62559 = CARTESIAN_POINT('Ctrl Pts',(30.5905496439846,587.227917914789,-48.7740984093909)) ;
#62560 = CARTESIAN_POINT('Ctrl Pts',(30.4108440838895,587.293396616897,-48.7623531259073)) ;
#62561 = CARTESIAN_POINT('Ctrl Pts',(30.3620302084178,587.308677942517,-48.759185862631)) ;
#62562 = CARTESIAN_POINT('Ctrl Pts',(30.2756164453555,587.331423077509,-48.7534995852661)) ;
#62563 = CARTESIAN_POINT('Ctrl Pts',(30.2383175334423,587.33987930196,-48.7510198891862)) ;
#62564 = CARTESIAN_POINT('Ctrl Pts',(30.1703602760856,587.352845416816,-48.7464019168162)) ;
#62565 = CARTESIAN_POINT('Ctrl Pts',(30.1398057068966,587.357797017178,-48.7442863000492)) ;
#62566 = CARTESIAN_POINT('Ctrl Pts',(29.9877304410739,587.378113357972,-48.7336099174467)) ;
#62567 = CARTESIAN_POINT('Ctrl Pts',(29.8649155294811,587.380893766487,-48.7245678091076)) ;
#62568 = CARTESIAN_POINT('Ctrl Pts',(29.6774514396149,587.364445766459,-48.7109381722721)) ;
#62569 = CARTESIAN_POINT('Ctrl Pts',(29.6123814452612,587.354833717225,-48.7062331452597)) ;
#62570 = CARTESIAN_POINT('Ctrl Pts',(29.4927481734006,587.329856819,-48.6976811214779)) ;
#62571 = CARTESIAN_POINT('Ctrl Pts',(29.4380706841677,587.315506510809,-48.6938113330393)) ;
#62572 = CARTESIAN_POINT('Ctrl Pts',(29.3351066489178,587.282804603572,-48.6865831930285)) ;
#62573 = CARTESIAN_POINT('Ctrl Pts',(29.2867378096245,587.264933721043,-48.6832134788407)) ;
#62574 = CARTESIAN_POINT('Ctrl Pts',(29.1152476886922,587.192364817326,-48.671276695858)) ;
#62575 = CARTESIAN_POINT('Ctrl Pts',(28.9980474770585,587.125040331794,-48.663182740517)) ;
#62576 = CARTESIAN_POINT('Ctrl Pts',(28.84779135783,587.012576410687,-48.6516719089149)) ;
#62577 = CARTESIAN_POINT('Ctrl Pts',(28.8069010735547,586.978811385645,-48.6483953959183)) ;
#62578 = CARTESIAN_POINT('Ctrl Pts',(28.7387838345676,586.916870248669,-48.6425464901203)) ;
#62579 = CARTESIAN_POINT('Ctrl Pts',(28.7108117873238,586.889576413327,-48.6400168881208)) ;
#62580 = CARTESIAN_POINT('Ctrl Pts',(28.6626506075018,586.83915787209,-48.6353684987152)) ;
#62581 = CARTESIAN_POINT('Ctrl Pts',(28.6420935377327,586.816412087286,-48.6332760642411)) ;
#62582 = CARTESIAN_POINT('Ctrl Pts',(28.5493991477983,586.70797970938,-48.6233619092092)) ;
#62583 = CARTESIAN_POINT('Ctrl Pts',(28.4853969049893,586.615728900754,-48.6151301082404)) ;
#62584 = CARTESIAN_POINT('Ctrl Pts',(28.3967571336742,586.455690593489,-48.6018408934074)) ;
#62585 = CARTESIAN_POINT('Ctrl Pts',(28.3663747245201,586.391478871241,-48.5967335237128)) ;
#62586 = CARTESIAN_POINT('Ctrl Pts',(28.3184987900759,586.270935432396,-48.5876174612283)) ;
#62587 = CARTESIAN_POINT('Ctrl Pts',(28.2997192532535,586.215238164086,-48.5835765421571)) ;
#62588 = CARTESIAN_POINT('Ctrl Pts',(28.2704273385842,586.110344754646,-48.5762646252609)) ;
#62589 = CARTESIAN_POINT('Ctrl Pts',(28.259123348422,586.061442440133,-48.5729707365131)) ;
#62590 = CARTESIAN_POINT('Ctrl Pts',(28.2329612179784,585.919282092521,-48.5636647331985)) ;
#62591 = CARTESIAN_POINT('Ctrl Pts',(28.2237963249913,585.825176036673,-48.5578417212622)) ;
#62592 = CARTESIAN_POINT('Ctrl Pts',(28.2213774626171,585.625943716043,-48.5456589164728)) ;
#62593 = CARTESIAN_POINT('Ctrl Pts',(28.2300056645136,585.521222313689,-48.5393370956589)) ;
#62594 = CARTESIAN_POINT('Ctrl Pts',(28.2547562756177,585.382461980831,-48.5303258642098)) ;
#62595 = CARTESIAN_POINT('Ctrl Pts',(28.2622525376537,585.347124186651,-48.5279728170235)) ;
#62596 = CARTESIAN_POINT('Ctrl Pts',(28.2785358516811,585.281025679962,-48.5234131361376)) ;
#62597 = CARTESIAN_POINT('Ctrl Pts',(28.2870719106186,585.250221083006,-48.5212194454555)) ;
#62598 = CARTESIAN_POINT('Ctrl Pts',(28.3077407921973,585.183186959741,-48.5163204859633)) ;
#62599 = CARTESIAN_POINT('Ctrl Pts',(28.3202454848325,585.147088915202,-48.5136006387902)) ;
#62600 = CARTESIAN_POINT('Ctrl Pts',(28.3664566130891,585.027181913957,-48.5043545186396)) ;
#62601 = CARTESIAN_POINT('Ctrl Pts',(28.4057335667357,584.94568936655,-48.4977236111895)) ;
#62602 = CARTESIAN_POINT('Ctrl Pts',(28.4935581090456,584.795932053103,-48.485189927585)) ;
#62603 = CARTESIAN_POINT('Ctrl Pts',(28.5410274421894,584.727335442535,-48.4792872991504)) ;
#62604 = CARTESIAN_POINT('Ctrl Pts',(28.6251184481247,584.623417601101,-48.4701223348718)) ;
#62605 = CARTESIAN_POINT('Ctrl Pts',(28.6585617390161,584.585719641628,-48.4667416485274)) ;
#62606 = CARTESIAN_POINT('Ctrl Pts',(28.7357727542759,584.506254866704,-48.4594588549308)) ;
#62607 = CARTESIAN_POINT('Ctrl Pts',(28.7802097380882,584.465237936564,-48.4555935583331)) ;
#62608 = CARTESIAN_POINT('Ctrl Pts',(28.8846519841829,584.378863586232,-48.4470900730299)) ;
#62609 = CARTESIAN_POINT('Ctrl Pts',(28.9456941544283,584.334970228841,-48.4425033676714)) ;
#62610 = CARTESIAN_POINT('Ctrl Pts',(29.095284272208,584.242055365075,-48.431752711962)) ;
#62611 = CARTESIAN_POINT('Ctrl Pts',(29.1857337121211,584.196685595261,-48.4256148653484)) ;
#62612 = CARTESIAN_POINT('Ctrl Pts',(29.308895433532,584.148334388459,-48.4170364395786)) ;
#62613 = CARTESIAN_POINT('Ctrl Pts',(29.3383877677785,584.137706469837,-48.4149653444503)) ;
#62614 = CARTESIAN_POINT('Ctrl Pts',(29.4035476772101,584.11628225571,-48.4103196186268)) ;
#62615 = CARTESIAN_POINT('Ctrl Pts',(29.4393104057071,584.10583874822,-48.4077295406124)) ;
#62616 = CARTESIAN_POINT('Ctrl Pts',(29.5785795201811,584.070188940319,-48.3975660997385)) ;
#62617 = CARTESIAN_POINT('Ctrl Pts',(29.6840607939237,584.053732638662,-48.3897242915992)) ;
#62618 = CARTESIAN_POINT('Ctrl Pts',(29.8809666072766,584.042113179148,-48.3754372096816)) ;
#62619 = CARTESIAN_POINT('Ctrl Pts',(29.9718429293535,584.044176114987,-48.3689779597763)) ;
#62620 = CARTESIAN_POINT('Ctrl Pts',(30.1119402854631,584.058853043998,-48.3593044710473)) ;
#62621 = CARTESIAN_POINT('Ctrl Pts',(30.1615120803415,584.066318656834,-48.3559350558121)) ;
#62622 = CARTESIAN_POINT('Ctrl Pts',(30.2684818203681,584.08740096651,-48.348754602551)) ;
#62623 = CARTESIAN_POINT('Ctrl Pts',(30.3256460785242,584.101852652511,-48.3449758032274)) ;
#62624 = CARTESIAN_POINT('Ctrl Pts',(30.4501491659698,584.140457359066,-48.3367767317666)) ;
#62625 = CARTESIAN_POINT('Ctrl Pts',(30.5169405733026,584.165976078781,-48.3324002121253)) ;
#62626 = CARTESIAN_POINT('Ctrl Pts',(30.6824466268293,584.241729411495,-48.3212832619082)) ;
#62627 = CARTESIAN_POINT('Ctrl Pts',(30.7781559128771,584.297646062732,-48.3145965096427)) ;
#62628 = CARTESIAN_POINT('Ctrl Pts',(30.8924838136642,584.380687968153,-48.3054103738149)) ;
#62629 = CARTESIAN_POINT('Ctrl Pts',(30.9168543912333,584.399441473042,-48.3033728420633)) ;
#62630 = CARTESIAN_POINT('Ctrl Pts',(30.9707692336124,584.443358012326,-48.2986523179648)) ;
#62631 = CARTESIAN_POINT('Ctrl Pts',(30.9999785026842,584.468898061059,-48.2959473720544)) ;
#62632 = CARTESIAN_POINT('Ctrl Pts',(31.0664577942132,584.531252549733,-48.2894866498209)) ;
#62633 = CARTESIAN_POINT('Ctrl Pts',(31.1029364879462,584.568852341852,-48.2856983870331)) ;
#62634 = CARTESIAN_POINT('Ctrl Pts',(31.2279978609192,584.710543075024,-48.271957567134)) ;
#62635 = CARTESIAN_POINT('Ctrl Pts',(31.3054875040584,584.823737638272,-48.2620029832366)) ;
#62636 = CARTESIAN_POINT('Ctrl Pts',(31.3919167571382,584.990827162992,-48.2490314326713)) ;
#62637 = CARTESIAN_POINT('Ctrl Pts',(31.4134220282484,585.037586891647,-48.2455587370126)) ;
#62638 = CARTESIAN_POINT('Ctrl Pts',(31.4540496185314,585.137919422736,-48.238406203904)) ;
#62639 = CARTESIAN_POINT('Ctrl Pts',(31.4726634996755,585.191626850893,-48.2347475537479)) ;
#62640 = CARTESIAN_POINT('Ctrl Pts',(31.5070119830165,585.309971010306,-48.226964295642)) ;
#62641 = CARTESIAN_POINT('Ctrl Pts',(31.5216952390433,585.374809568827,-48.222873409492)) ;
#62642 = CARTESIAN_POINT('Ctrl Pts',(31.5519254659926,585.558728309999,-48.2114699996543)) ;
#62643 = CARTESIAN_POINT('Ctrl Pts',(31.5585372407686,585.678839707607,-48.2042653578465)) ;
#62644 = CARTESIAN_POINT('Ctrl Pts',(31.5505511352172,585.829760711676,-48.194459660826)) ;
#62645 = CARTESIAN_POINT('Ctrl Pts',(31.5480271865968,585.86086753712,-48.1923962024582)) ;
#62646 = CARTESIAN_POINT('Ctrl Pts',(31.5405221375054,585.929415790313,-48.1877228879381)) ;
#62647 = CARTESIAN_POINT('Ctrl Pts',(31.5351387999145,585.966792651816,-48.1850956588018)) ;
#62648 = CARTESIAN_POINT('Ctrl Pts',(31.5112957067943,586.100070682857,-48.1755171306818)) ;
#62649 = CARTESIAN_POINT('Ctrl Pts',(31.4856838387136,586.194487787323,-48.1683488037984)) ;
#62650 = CARTESIAN_POINT('Ctrl Pts',(31.4519532733313,586.286113806151,-48.1612639293305)) ;
#62651 = CARTESIAN_POINT('Ctrl Pts',(31.4519519036772,586.286117526679,-49.0537704297648)) ;
#62652 = CARTESIAN_POINT('Ctrl Pts',(31.421888077714,586.367782581286,-49.0484597996442)) ;
#62653 = CARTESIAN_POINT('Ctrl Pts',(31.3854244428663,586.44709620345,-49.0431716762742)) ;
#62654 = CARTESIAN_POINT('Ctrl Pts',(31.3130425560406,586.576615087064,-49.033878018227)) ;
#62655 = CARTESIAN_POINT('Ctrl Pts',(31.2803461721985,586.628238848599,-49.0299782559106)) ;
#62656 = CARTESIAN_POINT('Ctrl Pts',(31.2156925895508,586.718889554863,-49.0226674544353)) ;
#62657 = CARTESIAN_POINT('Ctrl Pts',(31.1846563998223,586.758484131325,-49.0192959156207)) ;
#62658 = CARTESIAN_POINT('Ctrl Pts',(31.0546535773857,586.909711023892,-49.0056355997136)) ;
#62659 = CARTESIAN_POINT('Ctrl Pts',(30.9426962060906,587.0092223164,-48.9947606263072)) ;
#62660 = CARTESIAN_POINT('Ctrl Pts',(30.7774075023683,587.12051796513,-48.980283192767)) ;
#62661 = CARTESIAN_POINT('Ctrl Pts',(30.734533338749,587.146653362595,-48.9766582859475)) ;
#62662 = CARTESIAN_POINT('Ctrl Pts',(30.6573775015316,587.189029753654,-48.9704291484922)) ;
#62663 = CARTESIAN_POINT('Ctrl Pts',(30.6235983888595,587.206111630206,-48.9677952116997)) ;
#62664 = CARTESIAN_POINT('Ctrl Pts',(30.5608394961429,587.235207520903,-48.9631070895318)) ;
#62665 = CARTESIAN_POINT('Ctrl Pts',(30.5320490588203,587.247581059817,-48.9610355313183)) ;
#62666 = CARTESIAN_POINT('Ctrl Pts',(30.3916611088348,587.303280178125,-48.9512388317041)) ;
#62667 = CARTESIAN_POINT('Ctrl Pts',(30.2759473600757,587.335310846125,-48.9440495531446)) ;
#62668 = CARTESIAN_POINT('Ctrl Pts',(30.0919257833265,587.365448569377,-48.9326459202487)) ;
#62669 = CARTESIAN_POINT('Ctrl Pts',(30.0254808689942,587.372266915703,-48.9285377892994)) ;
#62670 = CARTESIAN_POINT('Ctrl Pts',(29.9017875197256,587.377489738618,-48.9207207309675)) ;
#62671 = CARTESIAN_POINT('Ctrl Pts',(29.8446850354306,587.376965472036,-48.9170459215576)) ;
#62672 = CARTESIAN_POINT('Ctrl Pts',(29.736049637312,587.370380450138,-48.9098548858993)) ;
#62673 = CARTESIAN_POINT('Ctrl Pts',(29.6845523622667,587.364841250242,-48.9063598316317)) ;
#62674 = CARTESIAN_POINT('Ctrl Pts',(29.5002524777121,587.336281214402,-48.8934972606977)) ;
#62675 = CARTESIAN_POINT('Ctrl Pts',(29.3701198079592,587.29957445332,-48.8836918630579)) ;
#62676 = CARTESIAN_POINT('Ctrl Pts',(29.1968897407221,587.227143495319,-48.8700407225077)) ;
#62677 = CARTESIAN_POINT('Ctrl Pts',(29.1489272394888,587.204340498131,-48.8661994840422)) ;
#62678 = CARTESIAN_POINT('Ctrl Pts',(29.06761643464,587.16080436013,-48.8596605593172)) ;
#62679 = CARTESIAN_POINT('Ctrl Pts',(29.0337586969931,587.141110381612,-48.8569294932786)) ;
#62680 = CARTESIAN_POINT('Ctrl Pts',(28.974393253501,587.103718173652,-48.8521669165994)) ;
#62681 = CARTESIAN_POINT('Ctrl Pts',(28.9486295188721,587.086468003505,-48.8501129820764)) ;
#62682 = CARTESIAN_POINT('Ctrl Pts',(28.8561505308132,587.020737934175,-48.8427393643579)) ;
#62683 = CARTESIAN_POINT('Ctrl Pts',(28.7925708362745,586.968037745833,-48.8376588523299)) ;
#62684 = CARTESIAN_POINT('Ctrl Pts',(28.6710461307095,586.85105862289,-48.82733849245)) ;
#62685 = CARTESIAN_POINT('Ctrl Pts',(28.6136785386213,586.786551045327,-48.8221145311418)) ;
#62686 = CARTESIAN_POINT('Ctrl Pts',(28.5224275940193,586.666345239656,-48.8126989284406)) ;
#62687 = CARTESIAN_POINT('Ctrl Pts',(28.4863360466501,586.612564081683,-48.8085843937042)) ;
#62688 = CARTESIAN_POINT('Ctrl Pts',(28.4279568623936,586.513566449864,-48.8010610254608)) ;
#62689 = CARTESIAN_POINT('Ctrl Pts',(28.404418967938,586.469181383288,-48.7977051784176)) ;
#62690 = CARTESIAN_POINT('Ctrl Pts',(28.3480024142957,586.350089594821,-48.7887071723738)) ;
#62691 = CARTESIAN_POINT('Ctrl Pts',(28.3185478323463,586.273920507988,-48.7829530214212)) ;
#62692 = CARTESIAN_POINT('Ctrl Pts',(28.2669922487746,586.104626910196,-48.7702109246683)) ;
#62693 = CARTESIAN_POINT('Ctrl Pts',(28.2470882004441,586.011126920369,-48.7631999164279)) ;
#62694 = CARTESIAN_POINT('Ctrl Pts',(28.2304679835342,585.877661701334,-48.7535126220154)) ;
#62695 = CARTESIAN_POINT('Ctrl Pts',(28.227004525409,585.838723128789,-48.7507259943334)) ;
#62696 = CARTESIAN_POINT('Ctrl Pts',(28.2231776958819,585.767296041769,-48.7457251098162)) ;
#62697 = CARTESIAN_POINT('Ctrl Pts',(28.2223884530683,585.734847620626,-48.7434951728177)) ;
#62698 = CARTESIAN_POINT('Ctrl Pts',(28.2227240337122,585.666442687974,-48.7389096624418)) ;
#62699 = CARTESIAN_POINT('Ctrl Pts',(28.2240639783314,585.630504682275,-48.736565180261)) ;
#62700 = CARTESIAN_POINT('Ctrl Pts',(28.2378119829954,585.43341528436,-48.7239246318286)) ;
#62701 = CARTESIAN_POINT('Ctrl Pts',(28.2724559474573,585.274676180999,-48.7144649842797)) ;
#62702 = CARTESIAN_POINT('Ctrl Pts',(28.3512561311783,585.065438731575,-48.7004641075677)) ;
#62703 = CARTESIAN_POINT('Ctrl Pts',(28.3762965010787,585.008747985914,-48.6965108910803)) ;
#62704 = CARTESIAN_POINT('Ctrl Pts',(28.4273717777081,584.90861218639,-48.6891317848915)) ;
#62705 = CARTESIAN_POINT('Ctrl Pts',(28.4523417666481,584.86470808054,-48.6857478278277)) ;
#62706 = CARTESIAN_POINT('Ctrl Pts',(28.5596588195656,584.694501603386,-48.6719682983997)) ;
#62707 = CARTESIAN_POINT('Ctrl Pts',(28.6569732335752,584.578517479455,-48.6609732722238)) ;
#62708 = CARTESIAN_POINT('Ctrl Pts',(28.8052809840315,584.443837473444,-48.6464230819893)) ;
#62709 = CARTESIAN_POINT('Ctrl Pts',(28.8435227762707,584.412109223283,-48.642837843674)) ;
#62710 = CARTESIAN_POINT('Ctrl Pts',(28.9131194039447,584.359436159431,-48.6366646784877)) ;
#62711 = CARTESIAN_POINT('Ctrl Pts',(28.9438748394614,584.337756919394,-48.6340477808887)) ;
#62712 = CARTESIAN_POINT('Ctrl Pts',(29.0017071522415,584.299856403518,-48.6293638583321)) ;
#62713 = CARTESIAN_POINT('Ctrl Pts',(29.028558958392,584.283328746974,-48.627280734223)) ;
#62714 = CARTESIAN_POINT('Ctrl Pts',(29.1579455116045,584.208667712314,-48.6175964913183)) ;
#62715 = CARTESIAN_POINT('Ctrl Pts',(29.2660028768451,584.160753273113,-48.6105096961675)) ;
#62716 = CARTESIAN_POINT('Ctrl Pts',(29.442221951244,584.104051306547,-48.5991886678688)) ;
#62717 = CARTESIAN_POINT('Ctrl Pts',(29.5074019498371,584.087352992751,-48.5950517058598)) ;
#62718 = CARTESIAN_POINT('Ctrl Pts',(29.6296597897424,584.063803169192,-48.5871922612557)) ;
#62719 = CARTESIAN_POINT('Ctrl Pts',(29.6864264019397,584.055877426931,-48.5835048295577)) ;
#62720 = CARTESIAN_POINT('Ctrl Pts',(29.7949988572825,584.046388953304,-48.5763051782396)) ;
#62721 = CARTESIAN_POINT('Ctrl Pts',(29.8466900049273,584.044288276869,-48.5728150229549)) ;
#62722 = CARTESIAN_POINT('Ctrl Pts',(30.0345413500177,584.045400398924,-48.5598619412075)) ;
#62723 = CARTESIAN_POINT('Ctrl Pts',(30.1700582728422,584.062893874096,-48.5499485511959)) ;
#62724 = CARTESIAN_POINT('Ctrl Pts',(30.3529006932756,584.109726391023,-48.536225666219)) ;
#62725 = CARTESIAN_POINT('Ctrl Pts',(30.4032513462971,584.125198553051,-48.5324164110218)) ;
#62726 = CARTESIAN_POINT('Ctrl Pts',(30.4894467492368,584.156225994577,-48.5259227950453)) ;
#62727 = CARTESIAN_POINT('Ctrl Pts',(30.5256357001918,584.17070543898,-48.5232055973716)) ;
#62728 = CARTESIAN_POINT('Ctrl Pts',(30.5896520775957,584.198962751141,-48.5184562772016)) ;
#62729 = CARTESIAN_POINT('Ctrl Pts',(30.6176620905825,584.212272669135,-48.5164023509664)) ;
#62730 = CARTESIAN_POINT('Ctrl Pts',(30.7422349836639,584.275789097501,-48.5073165282251)) ;
#62731 = CARTESIAN_POINT('Ctrl Pts',(30.8341215230322,584.334608235735,-48.5007286935346)) ;
#62732 = CARTESIAN_POINT('Ctrl Pts',(30.9763833581684,584.446702867174,-48.489668800352)) ;
#62733 = CARTESIAN_POINT('Ctrl Pts',(31.0301709562402,584.495070409924,-48.4852441815845)) ;
#62734 = CARTESIAN_POINT('Ctrl Pts',(31.1221461897108,584.589284357062,-48.476966073771)) ;
#62735 = CARTESIAN_POINT('Ctrl Pts',(31.1613383716971,584.633979402702,-48.4731578284577)) ;
#62736 = CARTESIAN_POINT('Ctrl Pts',(31.22922902557,584.720303373162,-48.4659260123143)) ;
#62737 = CARTESIAN_POINT('Ctrl Pts',(31.2585820130292,584.761329328733,-48.4625355183699)) ;
#62738 = CARTESIAN_POINT('Ctrl Pts',(31.337393397172,584.882768649674,-48.4525926100329)) ;
#62739 = CARTESIAN_POINT('Ctrl Pts',(31.3819343939489,584.96612572113,-48.4458671290233)) ;
#62740 = CARTESIAN_POINT('Ctrl Pts',(31.4512199610634,585.127354135424,-48.4331435908763)) ;
#62741 = CARTESIAN_POINT('Ctrl Pts',(31.4777714568495,585.204159432916,-48.427195361869)) ;
#62742 = CARTESIAN_POINT('Ctrl Pts',(31.5113096004686,585.330335151134,-48.4178223601859)) ;
#62743 = CARTESIAN_POINT('Ctrl Pts',(31.5218711356606,585.37862203405,-48.4143271422184)) ;
#62744 = CARTESIAN_POINT('Ctrl Pts',(31.5353000636259,585.456456457616,-48.4089090160608)) ;
#62745 = CARTESIAN_POINT('Ctrl Pts',(31.5395513003226,585.48572785121,-48.4069228541789)) ;
#62746 = CARTESIAN_POINT('Ctrl Pts',(31.5493436735007,585.568615969838,-48.4014340330348)) ;
#62747 = CARTESIAN_POINT('Ctrl Pts',(31.5530664315368,585.622409624868,-48.398020883997)) ;
#62748 = CARTESIAN_POINT('Ctrl Pts',(31.55643863621,585.786309141962,-48.3878199607563)) ;
#62749 = CARTESIAN_POINT('Ctrl Pts',(31.547797451983,585.896279176642,-48.3812304434282)) ;
#62750 = CARTESIAN_POINT('Ctrl Pts',(31.5156784419345,586.075410171445,-48.3699638980023)) ;
#62751 = CARTESIAN_POINT('Ctrl Pts',(31.4984095576746,586.145317801445,-48.3654311046471)) ;
#62752 = CARTESIAN_POINT('Ctrl Pts',(31.4689881640764,586.238152638679,-48.3590924580401)) ;
#62753 = CARTESIAN_POINT('Ctrl Pts',(31.4607434316487,586.262236314981,-48.3574184609264)) ;
#62754 = CARTESIAN_POINT('Ctrl Pts',(31.4519518985791,586.286117540527,-48.355726152802)) ;
#62755 = CARTESIAN_POINT('Origin',(179.888527625407,535.710565160536,-51.0680854522974)) ;
#62756 = CARTESIAN_POINT('Ctrl Pts',(178.636454050031,537.339770280938,-49.0681970943831)) ;
#62757 = CARTESIAN_POINT('Ctrl Pts',(178.542327710974,537.267432488475,-49.0621684907212)) ;
#62758 = CARTESIAN_POINT('Ctrl Pts',(178.454647768142,537.187075486664,-49.0564967090507)) ;
#62759 = CARTESIAN_POINT('Ctrl Pts',(178.296795779322,537.015004255062,-49.0451737686981)) ;
#62760 = CARTESIAN_POINT('Ctrl Pts',(178.226433855834,536.924077643581,-49.0395455094629)) ;
#62761 = CARTESIAN_POINT('Ctrl Pts',(178.135310039735,536.783419696863,-49.0308913314428)) ;
#62762 = CARTESIAN_POINT('Ctrl Pts',(178.108307493668,536.737991246653,-49.028106053429)) ;
#62763 = CARTESIAN_POINT('Ctrl Pts',(178.057607625607,536.644683744705,-49.022374987254)) ;
#62764 = CARTESIAN_POINT('Ctrl Pts',(178.033966845089,536.596820840721,-49.0194300557263)) ;
#62765 = CARTESIAN_POINT('Ctrl Pts',(177.962776448962,536.437333645756,-49.0095833748824)) ;
#62766 = CARTESIAN_POINT('Ctrl Pts',(177.923246874237,536.322426621875,-49.0024193971002)) ;
#62767 = CARTESIAN_POINT('Ctrl Pts',(177.866987766582,536.095360924845,-48.9883797828834)) ;
#62768 = CARTESIAN_POINT('Ctrl Pts',(177.848931848885,535.983955093438,-48.9815479914339)) ;
#62769 = CARTESIAN_POINT('Ctrl Pts',(177.836804776698,535.829720497406,-48.9725576625325)) ;
#62770 = CARTESIAN_POINT('Ctrl Pts',(177.834796270281,535.787718764495,-48.9701579616603)) ;
#62771 = CARTESIAN_POINT('Ctrl Pts',(177.83357816501,535.716455883667,-48.9662014726683)) ;
#62772 = CARTESIAN_POINT('Ctrl Pts',(177.833702239804,535.687225142105,-48.9646136316033)) ;
#62773 = CARTESIAN_POINT('Ctrl Pts',(177.835692606149,535.609445264445,-48.9604736885088)) ;
#62774 = CARTESIAN_POINT('Ctrl Pts',(177.838656619331,535.560944270059,-48.9579761577606)) ;
#62775 = CARTESIAN_POINT('Ctrl Pts',(177.8565806548,535.375778778729,-48.9486128266382)) ;
#62776 = CARTESIAN_POINT('Ctrl Pts',(177.883518922326,535.240634029496,-48.9421178793161)) ;
#62777 = CARTESIAN_POINT('Ctrl Pts',(177.950998588688,535.020170561269,-48.9308475096296)) ;
#62778 = CARTESIAN_POINT('Ctrl Pts',(177.984259739123,534.933117475896,-48.9262118917525)) ;
#62779 = CARTESIAN_POINT('Ctrl Pts',(178.04495061424,534.80178355098,-48.9187028320399)) ;
#62780 = CARTESIAN_POINT('Ctrl Pts',(178.068351768507,534.755777531711,-48.9159688748401)) ;
#62781 = CARTESIAN_POINT('Ctrl Pts',(178.120244690292,534.662613248668,-48.9101884388951)) ;
#62782 = CARTESIAN_POINT('Ctrl Pts',(178.14895075701,534.615622587636,-48.9071355627331)) ;
#62783 = CARTESIAN_POINT('Ctrl Pts',(178.267581401577,534.437890957758,-48.895025771416)) ;
#62784 = CARTESIAN_POINT('Ctrl Pts',(178.370631361474,534.316598532573,-48.8854704416936)) ;
#62785 = CARTESIAN_POINT('Ctrl Pts',(178.532510892978,534.165520463416,-48.8721722636474)) ;
#62786 = CARTESIAN_POINT('Ctrl Pts',(178.580384473297,534.124782478099,-48.8684188322932)) ;
#62787 = CARTESIAN_POINT('Ctrl Pts',(178.665657526472,534.058713124868,-48.8621216119247)) ;
#62788 = CARTESIAN_POINT('Ctrl Pts',(178.702163908397,534.03230172305,-48.8595381348249)) ;
#62789 = CARTESIAN_POINT('Ctrl Pts',(178.763657146783,533.990823251127,-48.8554058869055)) ;
#62790 = CARTESIAN_POINT('Ctrl Pts',(178.788144971627,533.975052538786,-48.8538167890008)) ;
#62791 = CARTESIAN_POINT('Ctrl Pts',(178.851230495965,533.93629652699,-48.8498621324231)) ;
#62792 = CARTESIAN_POINT('Ctrl Pts',(178.890260028631,533.914047165523,-48.8475392796793)) ;
#62793 = CARTESIAN_POINT('Ctrl Pts',(179.05036044178,533.829609950303,-48.8383745189989)) ;
#62794 = CARTESIAN_POINT('Ctrl Pts',(179.17674740049,533.778237287736,-48.8319339113943)) ;
#62795 = CARTESIAN_POINT('Ctrl Pts',(179.402040691413,533.71179406825,-48.8204859190186)) ;
#62796 = CARTESIAN_POINT('Ctrl Pts',(179.498672341653,533.690722193766,-48.8155887901258)) ;
#62797 = CARTESIAN_POINT('Ctrl Pts',(179.64791508429,533.669289151764,-48.8077777470804)) ;
#62798 = CARTESIAN_POINT('Ctrl Pts',(179.699651023047,533.663853868523,-48.8050272740284)) ;
#62799 = CARTESIAN_POINT('Ctrl Pts',(179.805824777175,533.656759330293,-48.7992684846683)) ;
#62800 = CARTESIAN_POINT('Ctrl Pts',(179.860233484665,533.655289804287,-48.7962563727491)) ;
#62801 = CARTESIAN_POINT('Ctrl Pts',(180.060831435104,533.65783858587,-48.7849090068978)) ;
#62802 = CARTESIAN_POINT('Ctrl Pts',(180.206395009497,533.675295226187,-48.7761617775762)) ;
#62803 = CARTESIAN_POINT('Ctrl Pts',(180.418356560313,533.724019094757,-48.7630829499242)) ;
#62804 = CARTESIAN_POINT('Ctrl Pts',(180.486986681768,533.743605190038,-48.758800857569)) ;
#62805 = CARTESIAN_POINT('Ctrl Pts',(180.600415187797,533.782464218616,-48.7517703501032)) ;
#62806 = CARTESIAN_POINT('Ctrl Pts',(180.645799812939,533.799833179317,-48.7489710346728)) ;
#62807 = CARTESIAN_POINT('Ctrl Pts',(180.717440523858,533.830204730404,-48.7446213841963)) ;
#62808 = CARTESIAN_POINT('Ctrl Pts',(180.744105244593,533.842186404612,-48.743019913562)) ;
#62809 = CARTESIAN_POINT('Ctrl Pts',(180.808484487784,533.87278260655,-48.7391991236654)) ;
#62810 = CARTESIAN_POINT('Ctrl Pts',(180.845898957911,533.891992650726,-48.7370132501454)) ;
#62811 = CARTESIAN_POINT('Ctrl Pts',(181.000076963651,533.977231923506,-48.7280453755306)) ;
#62812 = CARTESIAN_POINT('Ctrl Pts',(181.110827040934,534.053466505995,-48.7216838029734)) ;
#62813 = CARTESIAN_POINT('Ctrl Pts',(181.269343003033,534.187177494918,-48.7116001408561)) ;
#62814 = CARTESIAN_POINT('Ctrl Pts',(181.322755927236,534.237354603126,-48.7080023363249)) ;
#62815 = CARTESIAN_POINT('Ctrl Pts',(181.415897884025,534.334730027453,-48.70119524651)) ;
#62816 = CARTESIAN_POINT('Ctrl Pts',(181.456400456788,534.381070506793,-48.6980198342083)) ;
#62817 = CARTESIAN_POINT('Ctrl Pts',(181.525934523147,534.468230711574,-48.692104578938)) ;
#62818 = CARTESIAN_POINT('Ctrl Pts',(181.555669429729,534.508427971447,-48.6893969376608)) ;
#62819 = CARTESIAN_POINT('Ctrl Pts',(181.624023351724,534.608252295365,-48.6827023965866)) ;
#62820 = CARTESIAN_POINT('Ctrl Pts',(181.661071639527,534.668871785708,-48.6786597196493)) ;
#62821 = CARTESIAN_POINT('Ctrl Pts',(181.763938740653,534.858619681276,-48.6660864400596)) ;
#62822 = CARTESIAN_POINT('Ctrl Pts',(181.819309924628,534.992894583591,-48.6572660636923)) ;
#62823 = CARTESIAN_POINT('Ctrl Pts',(181.879379417516,535.197541619153,-48.6445552557715)) ;
#62824 = CARTESIAN_POINT('Ctrl Pts',(181.895367130346,535.26415639492,-48.6405325459092)) ;
#62825 = CARTESIAN_POINT('Ctrl Pts',(181.913699937431,535.361811682268,-48.634912396563)) ;
#62826 = CARTESIAN_POINT('Ctrl Pts',(181.918714878817,535.392301082679,-48.6331966618825)) ;
#62827 = CARTESIAN_POINT('Ctrl Pts',(181.927966025126,535.457728881311,-48.629613135694)) ;
#62828 = CARTESIAN_POINT('Ctrl Pts',(181.931996191779,535.492685115481,-48.627755627963)) ;
#62829 = CARTESIAN_POINT('Ctrl Pts',(181.947227091345,535.663174854721,-48.6188993033526)) ;
#62830 = CARTESIAN_POINT('Ctrl Pts',(181.945852949278,535.799500654536,-48.6124229137948)) ;
#62831 = CARTESIAN_POINT('Ctrl Pts',(181.922365983171,536.013530295561,-48.6019847066371)) ;
#62832 = CARTESIAN_POINT('Ctrl Pts',(181.909159696295,536.091788707267,-48.5981130198768)) ;
#62833 = CARTESIAN_POINT('Ctrl Pts',(181.877106418538,536.231806048838,-48.5908917623806)) ;
#62834 = CARTESIAN_POINT('Ctrl Pts',(181.859810998182,536.293813363811,-48.5875861792547)) ;
#62835 = CARTESIAN_POINT('Ctrl Pts',(181.824006354894,536.402232700357,-48.5815496659751)) ;
#62836 = CARTESIAN_POINT('Ctrl Pts',(181.80666045951,536.448974073297,-48.5788594790524)) ;
#62837 = CARTESIAN_POINT('Ctrl Pts',(181.762036317524,536.557003540419,-48.5724143353593)) ;
#62838 = CARTESIAN_POINT('Ctrl Pts',(181.7334239354,536.617675355295,-48.5686154819313)) ;
#62839 = CARTESIAN_POINT('Ctrl Pts',(181.63271996048,536.806663580111,-48.5562035521406)) ;
#62840 = CARTESIAN_POINT('Ctrl Pts',(181.549801374464,536.928678549378,-48.5472607754822)) ;
#62841 = CARTESIAN_POINT('Ctrl Pts',(181.407306384613,537.096437276941,-48.5341137218446)) ;
#62842 = CARTESIAN_POINT('Ctrl Pts',(181.357092275105,537.149540529168,-48.5298080754178)) ;
#62843 = CARTESIAN_POINT('Ctrl Pts',(181.281485390623,537.221407412791,-48.5238984437335)) ;
#62844 = CARTESIAN_POINT('Ctrl Pts',(181.258326345418,537.242435756466,-48.5221585157646)) ;
#62845 = CARTESIAN_POINT('Ctrl Pts',(181.208618406476,537.285541064528,-48.5185850498275)) ;
#62846 = CARTESIAN_POINT('Ctrl Pts',(181.181975882962,537.307493676342,-48.5167593004295)) ;
#62847 = CARTESIAN_POINT('Ctrl Pts',(181.043600486761,537.415774257984,-48.5076503615033)) ;
#62848 = CARTESIAN_POINT('Ctrl Pts',(180.923726042842,537.491099983794,-48.5009428001874)) ;
#62849 = CARTESIAN_POINT('Ctrl Pts',(180.698429482008,537.602164841813,-48.4887570785792)) ;
#62850 = CARTESIAN_POINT('Ctrl Pts',(180.596058661144,537.642788524634,-48.4833572372502)) ;
#62851 = CARTESIAN_POINT('Ctrl Pts',(180.440124522023,537.690606352748,-48.4749459309971)) ;
#62852 = CARTESIAN_POINT('Ctrl Pts',(180.388730237061,537.704209792353,-48.4721474456496)) ;
#62853 = CARTESIAN_POINT('Ctrl Pts',(180.285135981776,537.727371919115,-48.4664246655478)) ;
#62854 = CARTESIAN_POINT('Ctrl Pts',(180.232978296029,537.736931535074,-48.4635028946538)) ;
#62855 = CARTESIAN_POINT('Ctrl Pts',(180.061413179173,537.761561294265,-48.4537433732945)) ;
#62856 = CARTESIAN_POINT('Ctrl Pts',(179.941058030172,537.768162804701,-48.4466469575906)) ;
#62857 = CARTESIAN_POINT('Ctrl Pts',(179.685782989789,537.759747996101,-48.4313271939612)) ;
#62858 = CARTESIAN_POINT('Ctrl Pts',(179.551496092749,537.741985659295,-48.4231086697372)) ;
#62859 = CARTESIAN_POINT('Ctrl Pts',(179.387676844545,537.703613770197,-48.413518022559)) ;
#62860 = CARTESIAN_POINT('Ctrl Pts',(179.355618173539,537.695282286733,-48.4116639825675)) ;
#62861 = CARTESIAN_POINT('Ctrl Pts',(179.292723724043,537.677303095676,-48.4080911972685)) ;
#62862 = CARTESIAN_POINT('Ctrl Pts',(179.26188651879,537.66769610399,-48.4063712621669)) ;
#62863 = CARTESIAN_POINT('Ctrl Pts',(179.147036168478,537.628922584521,-48.4000418752808)) ;
#62864 = CARTESIAN_POINT('Ctrl Pts',(179.06471211879,537.595037439013,-48.3956580320164)) ;
#62865 = CARTESIAN_POINT('Ctrl Pts',(178.861732865358,537.495636268589,-48.3846614012211)) ;
#62866 = CARTESIAN_POINT('Ctrl Pts',(178.745034004208,537.423215937803,-48.3781367500008)) ;
#62867 = CARTESIAN_POINT('Ctrl Pts',(178.636454050035,537.339770280941,-48.3712393117967)) ;
#62868 = CARTESIAN_POINT('Ctrl Pts',(178.636454050048,537.339770280952,-48.4293891818575)) ;
#62869 = CARTESIAN_POINT('Ctrl Pts',(178.636971408351,537.340167880156,-48.4294210284128)) ;
#62870 = CARTESIAN_POINT('Ctrl Pts',(178.637488959893,537.340565235887,-48.4294528708969)) ;
#62871 = CARTESIAN_POINT('Ctrl Pts',(178.780097725288,537.449946708084,-48.4382225368371)) ;
#62872 = CARTESIAN_POINT('Ctrl Pts',(178.935813278076,537.539881613079,-48.4466864846988)) ;
#62873 = CARTESIAN_POINT('Ctrl Pts',(179.149382963027,537.628476018642,-48.4586434944128)) ;
#62874 = CARTESIAN_POINT('Ctrl Pts',(179.19829007531,537.646614839493,-48.4613963560147)) ;
#62875 = CARTESIAN_POINT('Ctrl Pts',(179.298549919782,537.679517489769,-48.4670969686892)) ;
#62876 = CARTESIAN_POINT('Ctrl Pts',(179.349893935389,537.69417801563,-48.4700456192522)) ;
#62877 = CARTESIAN_POINT('Ctrl Pts',(179.519851071119,537.735621469847,-48.4799174054492)) ;
#62878 = CARTESIAN_POINT('Ctrl Pts',(179.640262191138,537.753879282824,-48.4871033321921)) ;
#62879 = CARTESIAN_POINT('Ctrl Pts',(179.89110237037,537.769408324738,-48.5021891641325)) ;
#62880 = CARTESIAN_POINT('Ctrl Pts',(180.021114633496,537.76513718705,-48.5100694564814)) ;
#62881 = CARTESIAN_POINT('Ctrl Pts',(180.183045563217,537.744373440327,-48.5193885071454)) ;
#62882 = CARTESIAN_POINT('Ctrl Pts',(180.216124256574,537.739308041724,-48.521264432017)) ;
#62883 = CARTESIAN_POINT('Ctrl Pts',(180.280196624903,537.727888342959,-48.5248243783715)) ;
#62884 = CARTESIAN_POINT('Ctrl Pts',(180.311195563918,537.721621945074,-48.5265117823724)) ;
#62885 = CARTESIAN_POINT('Ctrl Pts',(180.419294269943,537.697159832723,-48.5323110754626)) ;
#62886 = CARTESIAN_POINT('Ctrl Pts',(180.495481631618,537.675223071724,-48.5362471587008)) ;
#62887 = CARTESIAN_POINT('Ctrl Pts',(180.743906180651,537.587856790418,-48.5491190278353)) ;
#62888 = CARTESIAN_POINT('Ctrl Pts',(180.908584110323,537.503713271122,-48.5577974545466)) ;
#62889 = CARTESIAN_POINT('Ctrl Pts',(181.102539616882,537.369140397392,-48.5700155075771)) ;
#62890 = CARTESIAN_POINT('Ctrl Pts',(181.144084836481,537.337916496415,-48.5727604521371)) ;
#62891 = CARTESIAN_POINT('Ctrl Pts',(181.226037430217,537.271316176251,-48.5784694697332)) ;
#62892 = CARTESIAN_POINT('Ctrl Pts',(181.266330419729,537.235863460076,-48.581435588996)) ;
#62893 = CARTESIAN_POINT('Ctrl Pts',(181.353808703011,537.152596646698,-48.5882564558795)) ;
#62894 = CARTESIAN_POINT('Ctrl Pts',(181.400128732297,537.1039653957,-48.5921438162043)) ;
#62895 = CARTESIAN_POINT('Ctrl Pts',(181.53230899464,536.950828532717,-48.6040700566887)) ;
#62896 = CARTESIAN_POINT('Ctrl Pts',(181.610315525784,536.840040140144,-48.6123146745958)) ;
#62897 = CARTESIAN_POINT('Ctrl Pts',(181.70614253534,536.670672330255,-48.6238455357941)) ;
#62898 = CARTESIAN_POINT('Ctrl Pts',(181.733153573353,536.617695803122,-48.6273117274549)) ;
#62899 = CARTESIAN_POINT('Ctrl Pts',(181.770259725125,536.536384764315,-48.6323471814532)) ;
#62900 = CARTESIAN_POINT('Ctrl Pts',(181.782092367469,536.508880071567,-48.6340027366087)) ;
#62901 = CARTESIAN_POINT('Ctrl Pts',(181.807064850906,536.447148879245,-48.6376012347852)) ;
#62902 = CARTESIAN_POINT('Ctrl Pts',(181.819897969242,536.412811280288,-48.6395279238708)) ;
#62903 = CARTESIAN_POINT('Ctrl Pts',(181.846605937451,536.335066409508,-48.6437621246174)) ;
#62904 = CARTESIAN_POINT('Ctrl Pts',(181.859969572937,536.291503686283,-48.6460474120062)) ;
#62905 = CARTESIAN_POINT('Ctrl Pts',(181.903291734283,536.131488033617,-48.6542426215403)) ;
#62906 = CARTESIAN_POINT('Ctrl Pts',(181.924464708046,536.01291003996,-48.659950998467)) ;
#62907 = CARTESIAN_POINT('Ctrl Pts',(181.943090230063,535.804143040914,-48.6702165823836)) ;
#62908 = CARTESIAN_POINT('Ctrl Pts',(181.945215475097,535.714712803232,-48.6746791616568)) ;
#62909 = CARTESIAN_POINT('Ctrl Pts',(181.939396636824,535.574389554094,-48.68197639383)) ;
#62910 = CARTESIAN_POINT('Ctrl Pts',(181.935377235313,535.523446093756,-48.6846857933659)) ;
#62911 = CARTESIAN_POINT('Ctrl Pts',(181.923090441906,535.418019053855,-48.6904432295553)) ;
#62912 = CARTESIAN_POINT('Ctrl Pts',(181.914521731202,535.363612522553,-48.6934989588403)) ;
#62913 = CARTESIAN_POINT('Ctrl Pts',(181.881078947393,535.195521010333,-48.7032176551853)) ;
#62914 = CARTESIAN_POINT('Ctrl Pts',(181.848732447318,535.083570532672,-48.7101061513494)) ;
#62915 = CARTESIAN_POINT('Ctrl Pts',(181.761288957932,534.855501686841,-48.7247698132129)) ;
#62916 = CARTESIAN_POINT('Ctrl Pts',(181.704422434309,534.740566048844,-48.7325330824152)) ;
#62917 = CARTESIAN_POINT('Ctrl Pts',(181.619591387979,534.603070477832,-48.7417581963727)) ;
#62918 = CARTESIAN_POINT('Ctrl Pts',(181.601251361125,534.574913838014,-48.7436425089385)) ;
#62919 = CARTESIAN_POINT('Ctrl Pts',(181.56438689509,534.52124340208,-48.7472050893983)) ;
#62920 = CARTESIAN_POINT('Ctrl Pts',(181.545950176528,534.495681972897,-48.7488872653828)) ;
#62921 = CARTESIAN_POINT('Ctrl Pts',(181.480047069673,534.408605392416,-48.7546034202228)) ;
#62922 = CARTESIAN_POINT('Ctrl Pts',(181.429681854904,534.349360116707,-48.7584687418977)) ;
#62923 = CARTESIAN_POINT('Ctrl Pts',(181.273963861487,534.185942174509,-48.7695102238633)) ;
#62924 = CARTESIAN_POINT('Ctrl Pts',(181.160573000626,534.090130181396,-48.7765146665075)) ;
#62925 = CARTESIAN_POINT('Ctrl Pts',(180.984912313923,533.971594213003,-48.7871719685216)) ;
#62926 = CARTESIAN_POINT('Ctrl Pts',(180.930319458856,533.938349581176,-48.790455091714)) ;
#62927 = CARTESIAN_POINT('Ctrl Pts',(180.830786329668,533.883928308802,-48.7964528939476)) ;
#62928 = CARTESIAN_POINT('Ctrl Pts',(180.786459782168,533.861735557778,-48.7991275880171)) ;
#62929 = CARTESIAN_POINT('Ctrl Pts',(180.680817007635,533.813539615423,-48.8055292643042)) ;
#62930 = CARTESIAN_POINT('Ctrl Pts',(180.618955979563,533.788872837457,-48.8092993194072)) ;
#62931 = CARTESIAN_POINT('Ctrl Pts',(180.389830696127,533.710173452179,-48.8233338555193)) ;
#62932 = CARTESIAN_POINT('Ctrl Pts',(180.217041684975,533.674653078495,-48.8341250616248)) ;
#62933 = CARTESIAN_POINT('Ctrl Pts',(179.989017568001,533.657590038913,-48.8475964982882)) ;
#62934 = CARTESIAN_POINT('Ctrl Pts',(179.936041739681,533.655681131174,-48.8506661055594)) ;
#62935 = CARTESIAN_POINT('Ctrl Pts',(179.853655294818,533.655900858353,-48.8552882948924)) ;
#62936 = CARTESIAN_POINT('Ctrl Pts',(179.824266671069,533.656609860909,-48.856905972248)) ;
#62937 = CARTESIAN_POINT('Ctrl Pts',(179.755849666641,533.659730669324,-48.860591705264)) ;
#62938 = CARTESIAN_POINT('Ctrl Pts',(179.716856847382,533.662625925228,-48.8626355136992)) ;
#62939 = CARTESIAN_POINT('Ctrl Pts',(179.568071522617,533.677953338839,-48.8702955296407)) ;
#62940 = CARTESIAN_POINT('Ctrl Pts',(179.459258029982,533.698120245836,-48.8756148325543)) ;
#62941 = CARTESIAN_POINT('Ctrl Pts',(179.228026559658,533.760594960374,-48.8872078832518)) ;
#62942 = CARTESIAN_POINT('Ctrl Pts',(179.106919887448,533.80590482709,-48.89347780094)) ;
#62943 = CARTESIAN_POINT('Ctrl Pts',(178.943213025649,533.885411792385,-48.9028593082998)) ;
#62944 = CARTESIAN_POINT('Ctrl Pts',(178.896471964068,533.910390337433,-48.9056474956303)) ;
#62945 = CARTESIAN_POINT('Ctrl Pts',(178.805490493409,533.963631240722,-48.9113271240036)) ;
#62946 = CARTESIAN_POINT('Ctrl Pts',(178.761264010578,533.99183784831,-48.9142150947648)) ;
#62947 = CARTESIAN_POINT('Ctrl Pts',(178.626669037012,534.085110493024,-48.9234270354854)) ;
#62948 = CARTESIAN_POINT('Ctrl Pts',(178.540486606791,534.155840212777,-48.9299639722328)) ;
#62949 = CARTESIAN_POINT('Ctrl Pts',(178.358085762492,534.332152980644,-48.9451470628023)) ;
#62950 = CARTESIAN_POINT('Ctrl Pts',(178.266268253122,534.441490734593,-48.9538406640168)) ;
#62951 = CARTESIAN_POINT('Ctrl Pts',(178.16730741226,534.587813506215,-48.9639471366811)) ;
#62952 = CARTESIAN_POINT('Ctrl Pts',(178.148833270806,534.616657410548,-48.9658716624541)) ;
#62953 = CARTESIAN_POINT('Ctrl Pts',(178.115042963914,534.672437679025,-48.9694461467811)) ;
#62954 = CARTESIAN_POINT('Ctrl Pts',(178.099598845633,534.699283587368,-48.9711026825243)) ;
#62955 = CARTESIAN_POINT('Ctrl Pts',(178.050707002889,534.788897992079,-48.9764573449579)) ;
#62956 = CARTESIAN_POINT('Ctrl Pts',(178.019907961577,534.853058713529,-48.9800162413306)) ;
#62957 = CARTESIAN_POINT('Ctrl Pts',(177.930404605978,535.067362316777,-48.9914230800628)) ;
#62958 = CARTESIAN_POINT('Ctrl Pts',(177.886015249744,535.222814075474,-48.9990057158956)) ;
#62959 = CARTESIAN_POINT('Ctrl Pts',(177.850398961521,535.442584475366,-49.0102419279424)) ;
#62960 = CARTESIAN_POINT('Ctrl Pts',(177.843290433788,535.503717489371,-49.0134140804978)) ;
#62961 = CARTESIAN_POINT('Ctrl Pts',(177.83544145771,535.614289026611,-49.0192895888663)) ;
#62962 = CARTESIAN_POINT('Ctrl Pts',(177.833721894218,535.663610719697,-49.0219592191754)) ;
#62963 = CARTESIAN_POINT('Ctrl Pts',(177.833858254744,535.781406596256,-49.0284696142769)) ;
#62964 = CARTESIAN_POINT('Ctrl Pts',(177.837359097982,535.849816219465,-49.0323600333312)) ;
#62965 = CARTESIAN_POINT('Ctrl Pts',(177.857248770573,536.045905170736,-49.0438188647945)) ;
#62966 = CARTESIAN_POINT('Ctrl Pts',(177.882220800885,536.172381287622,-49.0516067850136)) ;
#62967 = CARTESIAN_POINT('Ctrl Pts',(177.941698773642,536.372603416275,-49.0641531800656)) ;
#62968 = CARTESIAN_POINT('Ctrl Pts',(177.969038821971,536.448130014332,-49.068932319098)) ;
#62969 = CARTESIAN_POINT('Ctrl Pts',(178.014183418213,536.553175701456,-49.0754770465997)) ;
#62970 = CARTESIAN_POINT('Ctrl Pts',(178.028415695389,536.584145522984,-49.077392895849)) ;
#62971 = CARTESIAN_POINT('Ctrl Pts',(178.057235292496,536.642955988185,-49.0809840392975)) ;
#62972 = CARTESIAN_POINT('Ctrl Pts',(178.071703392011,536.670843303878,-49.0826649097805)) ;
#62973 = CARTESIAN_POINT('Ctrl Pts',(178.122411753081,536.763331824808,-49.0882002710017)) ;
#62974 = CARTESIAN_POINT('Ctrl Pts',(178.16150626327,536.82630797845,-49.0919048209158)) ;
#62975 = CARTESIAN_POINT('Ctrl Pts',(178.297112211223,537.020483729812,-49.10354519564)) ;
#62976 = CARTESIAN_POINT('Ctrl Pts',(178.40582557567,537.142376886713,-49.1112419490159)) ;
#62977 = CARTESIAN_POINT('Ctrl Pts',(178.562993620517,537.281286422608,-49.1219018392419)) ;
#62978 = CARTESIAN_POINT('Ctrl Pts',(178.599258286014,537.311186851907,-49.1243301742461)) ;
#62979 = CARTESIAN_POINT('Ctrl Pts',(178.63651424806,537.339816542443,-49.1268080620001)) ;
#62980 = CARTESIAN_POINT('Origin',(29.8885276254068,535.710565160562,-51.0680854522906)) ;
#62981 = CARTESIAN_POINT('',(31.9432771690465,535.708946382626,-48.6168383787018)) ;
#62982 = CARTESIAN_POINT('Ctrl Pts',(28.6364362889498,537.339756631099,-49.0682055192064)) ;
#62983 = CARTESIAN_POINT('Ctrl Pts',(28.6324425150367,537.336687274423,-49.0679497338304)) ;
#62984 = CARTESIAN_POINT('Ctrl Pts',(28.6284598996157,537.333603134144,-49.0676945819357)) ;
#62985 = CARTESIAN_POINT('Ctrl Pts',(28.51677826253,537.246457910494,-49.0605360378214)) ;
#62986 = CARTESIAN_POINT('Ctrl Pts',(28.4177123018037,537.151873699214,-49.0540733584487)) ;
#62987 = CARTESIAN_POINT('Ctrl Pts',(28.2657666768744,536.97468919814,-49.042685031261)) ;
#62988 = CARTESIAN_POINT('Ctrl Pts',(28.2080430766881,536.89687532036,-49.0378797303259)) ;
#62989 = CARTESIAN_POINT('Ctrl Pts',(28.1281316220551,536.771552535011,-49.0301745650768)) ;
#62990 = CARTESIAN_POINT('Ctrl Pts',(28.1019109186819,536.72677792836,-49.0274294076523)) ;
#62991 = CARTESIAN_POINT('Ctrl Pts',(28.0516125755643,536.632912548862,-49.0216629927892)) ;
#62992 = CARTESIAN_POINT('Ctrl Pts',(28.0277438456033,536.583757304117,-49.0186370725674)) ;
#62993 = CARTESIAN_POINT('Ctrl Pts',(27.9483571866116,536.402187847095,-49.0074208738758)) ;
#62994 = CARTESIAN_POINT('Ctrl Pts',(27.9047996613618,536.265015932918,-48.9988384691246)) ;
#62995 = CARTESIAN_POINT('Ctrl Pts',(27.8545262406192,536.020546151499,-48.9838273769015)) ;
#62996 = CARTESIAN_POINT('Ctrl Pts',(27.8412358140034,535.915136749459,-48.9774553494339)) ;
#62997 = CARTESIAN_POINT('Ctrl Pts',(27.8345687442573,535.776361161162,-48.9695417164412)) ;
#62998 = CARTESIAN_POINT('Ctrl Pts',(27.8337793709737,535.743521102824,-48.9677043882939)) ;
#62999 = CARTESIAN_POINT('Ctrl Pts',(27.8337759013759,535.67812415242,-48.9641348791646)) ;
#63000 = CARTESIAN_POINT('Ctrl Pts',(27.8345476296576,535.645576735634,-48.962402611237)) ;
#63001 = CARTESIAN_POINT('Ctrl Pts',(27.8405969987939,535.518241148965,-48.9557517569802)) ;
#63002 = CARTESIAN_POINT('Ctrl Pts',(27.851667278428,535.423839206406,-48.9510924372246)) ;
#63003 = CARTESIAN_POINT('Ctrl Pts',(27.8990110077315,535.172277947907,-48.9386604529326)) ;
#63004 = CARTESIAN_POINT('Ctrl Pts',(27.9472912575291,535.018085829451,-48.9309784834429)) ;
#63005 = CARTESIAN_POINT('Ctrl Pts',(28.0348116369868,534.822553301613,-48.9199338804978)) ;
#63006 = CARTESIAN_POINT('Ctrl Pts',(28.0584231785513,534.774859517256,-48.9171333661)) ;
#63007 = CARTESIAN_POINT('Ctrl Pts',(28.1091407291144,534.681693853697,-48.9114161674706)) ;
#63008 = CARTESIAN_POINT('Ctrl Pts',(28.1362057121994,534.636246274519,-48.9085024603027)) ;
#63009 = CARTESIAN_POINT('Ctrl Pts',(28.2286148084511,534.493871405869,-48.8989480131398)) ;
#63010 = CARTESIAN_POINT('Ctrl Pts',(28.30047605584,534.401466254605,-48.8920668280111)) ;
#63011 = CARTESIAN_POINT('Ctrl Pts',(28.4752737908205,534.212401433728,-48.876633558149)) ;
#63012 = CARTESIAN_POINT('Ctrl Pts',(28.581113391671,534.119196927386,-48.8680620072579)) ;
#63013 = CARTESIAN_POINT('Ctrl Pts',(28.7221750027698,534.018619385244,-48.8582014538988)) ;
#63014 = CARTESIAN_POINT('Ctrl Pts',(28.7491495677121,534.000338016805,-48.8563802461583)) ;
#63015 = CARTESIAN_POINT('Ctrl Pts',(28.8041220381912,533.964960046678,-48.8528144706223)) ;
#63016 = CARTESIAN_POINT('Ctrl Pts',(28.8321173586955,533.947876783207,-48.8510708699381)) ;
#63017 = CARTESIAN_POINT('Ctrl Pts',(28.9499475578021,533.879790849504,-48.8439769161771)) ;
#63018 = CARTESIAN_POINT('Ctrl Pts',(29.0431628404374,533.83492400264,-48.8389371565802)) ;
#63019 = CARTESIAN_POINT('Ctrl Pts',(29.2767405583929,533.743465911539,-48.8267790113076)) ;
#63020 = CARTESIAN_POINT('Ctrl Pts',(29.4194970411273,533.704631513566,-48.8197028533382)) ;
#63021 = CARTESIAN_POINT('Ctrl Pts',(29.6187965722154,533.672872678016,-48.8093352506182)) ;
#63022 = CARTESIAN_POINT('Ctrl Pts',(29.6727287167303,533.666457628644,-48.8064870501227)) ;
#63023 = CARTESIAN_POINT('Ctrl Pts',(29.7787379813608,533.658090293649,-48.8007724108854)) ;
#63024 = CARTESIAN_POINT('Ctrl Pts',(29.830760445896,533.655968096278,-48.7979137395599)) ;
#63025 = CARTESIAN_POINT('Ctrl Pts',(29.9824955487993,533.65554544796,-48.7894009621829)) ;
#63026 = CARTESIAN_POINT('Ctrl Pts',(30.0820626933322,533.662523190496,-48.7835877643077)) ;
#63027 = CARTESIAN_POINT('Ctrl Pts',(30.3151523885225,533.696009649856,-48.769562464539)) ;
#63028 = CARTESIAN_POINT('Ctrl Pts',(30.4473363445353,533.72860262887,-48.7612678171605)) ;
#63029 = CARTESIAN_POINT('Ctrl Pts',(30.6171791367185,533.788837952158,-48.7507588141903)) ;
#63030 = CARTESIAN_POINT('Ctrl Pts',(30.6585320936462,533.805030538939,-48.7482151736987)) ;
#63031 = CARTESIAN_POINT('Ctrl Pts',(30.7260980516117,533.834046583491,-48.7441218990153)) ;
#63032 = CARTESIAN_POINT('Ctrl Pts',(30.7526162537398,533.846108877327,-48.74253395379)) ;
#63033 = CARTESIAN_POINT('Ctrl Pts',(30.819970134706,533.878492087609,-48.738545449447)) ;
#63034 = CARTESIAN_POINT('Ctrl Pts',(30.8604005153898,533.899614972793,-48.7361898069779)) ;
#63035 = CARTESIAN_POINT('Ctrl Pts',(30.955898902664,533.953628603919,-48.7306414550289)) ;
#63036 = CARTESIAN_POINT('Ctrl Pts',(31.010195932004,533.987785849383,-48.7274994543444)) ;
#63037 = CARTESIAN_POINT('Ctrl Pts',(31.1981508725158,534.118683852124,-48.7163686221103)) ;
#63038 = CARTESIAN_POINT('Ctrl Pts',(31.3216407479201,534.228882736553,-48.7085137277512)) ;
#63039 = CARTESIAN_POINT('Ctrl Pts',(31.4655997208718,534.392368978522,-48.6972711351371)) ;
#63040 = CARTESIAN_POINT('Ctrl Pts',(31.4990198184368,534.433415293354,-48.6944828469524)) ;
#63041 = CARTESIAN_POINT('Ctrl Pts',(31.5627846218381,534.518218501526,-48.6887591937053)) ;
#63042 = CARTESIAN_POINT('Ctrl Pts',(31.5930870619016,534.561955817211,-48.6858253189656)) ;
#63043 = CARTESIAN_POINT('Ctrl Pts',(31.6856910679613,534.707364593144,-48.6761112697115)) ;
#63044 = CARTESIAN_POINT('Ctrl Pts',(31.7408456107136,534.81328088647,-48.6690796140408)) ;
#63045 = CARTESIAN_POINT('Ctrl Pts',(31.8384573846933,535.048627739519,-48.6537975852015)) ;
#63046 = CARTESIAN_POINT('Ctrl Pts',(31.8778850749625,535.178730600246,-48.6455482266552)) ;
#63047 = CARTESIAN_POINT('Ctrl Pts',(31.9106149382367,535.344162998822,-48.6359380080728)) ;
#63048 = CARTESIAN_POINT('Ctrl Pts',(31.9162416944623,535.376703532573,-48.6340900384243)) ;
#63049 = CARTESIAN_POINT('Ctrl Pts',(31.9258295824852,535.441404932666,-48.6305183482567)) ;
#63050 = CARTESIAN_POINT('Ctrl Pts',(31.9298192211171,535.473551783346,-48.6287938333755)) ;
#63051 = CARTESIAN_POINT('Ctrl Pts',(31.9398089868692,535.573287498696,-48.6235614691451)) ;
#63052 = CARTESIAN_POINT('Ctrl Pts',(31.9432235565964,535.64109270422,-48.6201703425734)) ;
#63053 = CARTESIAN_POINT('Ctrl Pts',(31.9432769883604,535.708947154935,-48.6168380267463)) ;
#63054 = CARTESIAN_POINT('Ctrl Pts',(31.9432769877401,535.708946367384,-48.6168380654227)) ;
#63055 = CARTESIAN_POINT('Ctrl Pts',(31.9433994816354,535.864429017549,-48.6092023486022)) ;
#63056 = CARTESIAN_POINT('Ctrl Pts',(31.9258746531393,536.019420798674,-48.6018725754436)) ;
#63057 = CARTESIAN_POINT('Ctrl Pts',(31.8766814814539,536.233389829389,-48.5908301659164)) ;
#63058 = CARTESIAN_POINT('Ctrl Pts',(31.859417119639,536.295111929032,-48.5875377078832)) ;
#63059 = CARTESIAN_POINT('Ctrl Pts',(31.8236473630234,536.403235796962,-48.581514804191)) ;
#63060 = CARTESIAN_POINT('Ctrl Pts',(31.8062804514816,536.44995984631,-48.5788242838928)) ;
#63061 = CARTESIAN_POINT('Ctrl Pts',(31.7614976556292,536.5582169947,-48.5723623498924)) ;
#63062 = CARTESIAN_POINT('Ctrl Pts',(31.7327221843561,536.619121888355,-48.5685461748127)) ;
#63063 = CARTESIAN_POINT('Ctrl Pts',(31.6298850923612,536.811687078903,-48.5558881187871)) ;
#63064 = CARTESIAN_POINT('Ctrl Pts',(31.5442977966927,536.936620651887,-48.5466946167372)) ;
#63065 = CARTESIAN_POINT('Ctrl Pts',(31.4004416894612,537.103745188659,-48.5335453159337)) ;
#63066 = CARTESIAN_POINT('Ctrl Pts',(31.3524180486736,537.154123674196,-48.5294550128805)) ;
#63067 = CARTESIAN_POINT('Ctrl Pts',(31.2794410996137,537.223283600136,-48.5237657056771)) ;
#63068 = CARTESIAN_POINT('Ctrl Pts',(31.2564728611837,537.244085171439,-48.522044267435)) ;
#63069 = CARTESIAN_POINT('Ctrl Pts',(31.2065821095409,537.287256036464,-48.5184648764438)) ;
#63070 = CARTESIAN_POINT('Ctrl Pts',(31.1795418673164,537.309472377918,-48.5166165292592)) ;
#63071 = CARTESIAN_POINT('Ctrl Pts',(31.0435489340074,537.415503873464,-48.50768938979)) ;
#63072 = CARTESIAN_POINT('Ctrl Pts',(30.926934016215,537.488938109116,-48.501147638137)) ;
#63073 = CARTESIAN_POINT('Ctrl Pts',(30.7017056914125,537.601002973052,-48.4889493883153)) ;
#63074 = CARTESIAN_POINT('Ctrl Pts',(30.595514389154,537.643226552039,-48.4833532886448)) ;
#63075 = CARTESIAN_POINT('Ctrl Pts',(30.4358719594056,537.69177648773,-48.4747370646156)) ;
#63076 = CARTESIAN_POINT('Ctrl Pts',(30.384798153687,537.705182674746,-48.4719540982873)) ;
#63077 = CARTESIAN_POINT('Ctrl Pts',(30.2811864843987,537.728153412873,-48.4662266093179)) ;
#63078 = CARTESIAN_POINT('Ctrl Pts',(30.2286792967238,537.737666396398,-48.4632828832545)) ;
#63079 = CARTESIAN_POINT('Ctrl Pts',(30.017917873202,537.767431832564,-48.4512830000069)) ;
#63080 = CARTESIAN_POINT('Ctrl Pts',(29.8579320127544,537.771266737994,-48.4417077840596)) ;
#63081 = CARTESIAN_POINT('Ctrl Pts',(29.6036802310208,537.747732561675,-48.4263631350217)) ;
#63082 = CARTESIAN_POINT('Ctrl Pts',(29.5089433938644,537.732224836442,-48.4206330006412)) ;
#63083 = CARTESIAN_POINT('Ctrl Pts',(29.383919780426,537.702657086295,-48.4133213628132)) ;
#63084 = CARTESIAN_POINT('Ctrl Pts',(29.3523905594172,537.694404028775,-48.4114999668074)) ;
#63085 = CARTESIAN_POINT('Ctrl Pts',(29.289560406237,537.67635014148,-48.4079344305652)) ;
#63086 = CARTESIAN_POINT('Ctrl Pts',(29.2582710338655,537.666542978867,-48.406191258963)) ;
#63087 = CARTESIAN_POINT('Ctrl Pts',(29.0960265949812,537.611391948595,-48.3972592222333)) ;
#63088 = CARTESIAN_POINT('Ctrl Pts',(28.969658196228,537.553630041063,-48.3906526202095)) ;
#63089 = CARTESIAN_POINT('Ctrl Pts',(28.775882258398,537.440133668493,-48.3797737830095)) ;
#63090 = CARTESIAN_POINT('Ctrl Pts',(28.7045376370665,537.392094934182,-48.3755841735163)) ;
#63091 = CARTESIAN_POINT('Ctrl Pts',(28.6364362059859,537.339756567338,-48.3712578505663)) ;
#63092 = CARTESIAN_POINT('Ctrl Pts',(28.6364362890811,537.3397566312,-48.4293659750649)) ;
#63093 = CARTESIAN_POINT('Ctrl Pts',(28.6369341345453,537.340139243068,-48.4293966207162)) ;
#63094 = CARTESIAN_POINT('Ctrl Pts',(28.6374321589537,537.340521629481,-48.4294272625968)) ;
#63095 = CARTESIAN_POINT('Ctrl Pts',(28.7800462888248,537.44991782317,-48.4381976533586)) ;
#63096 = CARTESIAN_POINT('Ctrl Pts',(28.9357932715107,537.539874897829,-48.4466631603452)) ;
#63097 = CARTESIAN_POINT('Ctrl Pts',(29.1493914937462,537.628479096233,-48.4586217370792)) ;
#63098 = CARTESIAN_POINT('Ctrl Pts',(29.1982914004728,537.646615103932,-48.4613741865881)) ;
#63099 = CARTESIAN_POINT('Ctrl Pts',(29.2985341710519,537.679512495968,-48.4670738079441)) ;
#63100 = CARTESIAN_POINT('Ctrl Pts',(29.3498682754265,537.69417077506,-48.4700218739289)) ;
#63101 = CARTESIAN_POINT('Ctrl Pts',(29.5197401231057,537.735596653561,-48.4798886385651)) ;
#63102 = CARTESIAN_POINT('Ctrl Pts',(29.6400734380034,537.753851770086,-48.4870697365803)) ;
#63103 = CARTESIAN_POINT('Ctrl Pts',(29.890948668675,537.769415700826,-48.5021575738849)) ;
#63104 = CARTESIAN_POINT('Ctrl Pts',(30.0210758289075,537.765146895875,-48.5100450976257)) ;
#63105 = CARTESIAN_POINT('Ctrl Pts',(30.1831069739731,537.744364345731,-48.5193697278809)) ;
#63106 = CARTESIAN_POINT('Ctrl Pts',(30.2161734596322,537.739299894654,-48.5212449249387)) ;
#63107 = CARTESIAN_POINT('Ctrl Pts',(30.2802337054626,537.727881144985,-48.5248041479331)) ;
#63108 = CARTESIAN_POINT('Ctrl Pts',(30.3112326378434,537.721614154638,-48.5264915296209)) ;
#63109 = CARTESIAN_POINT('Ctrl Pts',(30.4193712226151,537.697140916015,-48.5322929018191)) ;
#63110 = CARTESIAN_POINT('Ctrl Pts',(30.4955972493127,537.675189013209,-48.5362308872873)) ;
#63111 = CARTESIAN_POINT('Ctrl Pts',(30.7439778340765,537.587816240299,-48.549100545008)) ;
#63112 = CARTESIAN_POINT('Ctrl Pts',(30.9085813624795,537.503706560625,-48.5577755381623)) ;
#63113 = CARTESIAN_POINT('Ctrl Pts',(31.1024713760036,537.369190175353,-48.5699889667854)) ;
#63114 = CARTESIAN_POINT('Ctrl Pts',(31.1440135884473,537.337971291506,-48.5727335794584)) ;
#63115 = CARTESIAN_POINT('Ctrl Pts',(31.2259504847639,537.27139003543,-48.5784411871001)) ;
#63116 = CARTESIAN_POINT('Ctrl Pts',(31.2662314798376,537.235952166069,-48.5814061958917)) ;
#63117 = CARTESIAN_POINT('Ctrl Pts',(31.3537013792073,537.152705633824,-48.5882257457261)) ;
#63118 = CARTESIAN_POINT('Ctrl Pts',(31.4000241652538,537.104078763425,-48.5921129488544)) ;
#63119 = CARTESIAN_POINT('Ctrl Pts',(31.532130969245,536.951050407056,-48.6040313840824)) ;
#63120 = CARTESIAN_POINT('Ctrl Pts',(31.610081524474,536.84038136237,-48.612267924402)) ;
#63121 = CARTESIAN_POINT('Ctrl Pts',(31.7059545915688,536.671036217124,-48.6238002968767)) ;
#63122 = CARTESIAN_POINT('Ctrl Pts',(31.7330344859247,536.617946572958,-48.6272746542249)) ;
#63123 = CARTESIAN_POINT('Ctrl Pts',(31.770204887291,536.536510033042,-48.6323184695661)) ;
#63124 = CARTESIAN_POINT('Ctrl Pts',(31.7820428516438,536.508997847162,-48.6339746771135)) ;
#63125 = CARTESIAN_POINT('Ctrl Pts',(31.8070057707924,536.447300556583,-48.6375715962633)) ;
#63126 = CARTESIAN_POINT('Ctrl Pts',(31.8198265633701,536.41300534071,-48.6394961948287)) ;
#63127 = CARTESIAN_POINT('Ctrl Pts',(31.8465031839903,536.335382547397,-48.6437244550515)) ;
#63128 = CARTESIAN_POINT('Ctrl Pts',(31.8598507509704,536.291900369335,-48.6460060016628)) ;
#63129 = CARTESIAN_POINT('Ctrl Pts',(31.9030471562376,536.132501638755,-48.6541713204406)) ;
#63130 = CARTESIAN_POINT('Ctrl Pts',(31.9241989758048,536.014478360057,-48.6598549254506)) ;
#63131 = CARTESIAN_POINT('Ctrl Pts',(31.9430323379677,535.805828438005,-48.6701129849498)) ;
#63132 = CARTESIAN_POINT('Ctrl Pts',(31.9452321466234,535.715949847246,-48.6745963046339)) ;
#63133 = CARTESIAN_POINT('Ctrl Pts',(31.9394476928602,535.575151268958,-48.6819168956853)) ;
#63134 = CARTESIAN_POINT('Ctrl Pts',(31.935444950985,535.524181471041,-48.6846271532407)) ;
#63135 = CARTESIAN_POINT('Ctrl Pts',(31.9232023026646,535.41881509033,-48.6903801553537)) ;
#63136 = CARTESIAN_POINT('Ctrl Pts',(31.9146700888374,535.364494303113,-48.6934303048282)) ;
#63137 = CARTESIAN_POINT('Ctrl Pts',(31.8814923869037,535.197316851374,-48.7030933440012)) ;
#63138 = CARTESIAN_POINT('Ctrl Pts',(31.8495080041542,535.08615953212,-48.7099277833718)) ;
#63139 = CARTESIAN_POINT('Ctrl Pts',(31.7622215685892,534.857317338191,-48.7246294358381)) ;
#63140 = CARTESIAN_POINT('Ctrl Pts',(31.7047468601355,534.74097130568,-48.7324896348168)) ;
#63141 = CARTESIAN_POINT('Ctrl Pts',(31.619111806607,534.602324927815,-48.7417921002564)) ;
#63142 = CARTESIAN_POINT('Ctrl Pts',(31.6008272848172,534.574278139409,-48.7436690093868)) ;
#63143 = CARTESIAN_POINT('Ctrl Pts',(31.5639681048963,534.520651299094,-48.7472285686689)) ;
#63144 = CARTESIAN_POINT('Ctrl Pts',(31.5454729735806,534.495029041029,-48.7489146878207)) ;
#63145 = CARTESIAN_POINT('Ctrl Pts',(31.478769457113,534.406974371609,-48.7546952049357)) ;
#63146 = CARTESIAN_POINT('Ctrl Pts',(31.4275605618832,534.346894424055,-48.7586153935346)) ;
#63147 = CARTESIAN_POINT('Ctrl Pts',(31.2452598331507,534.156402940385,-48.7715048480354)) ;
#63148 = CARTESIAN_POINT('Ctrl Pts',(31.100087052131,534.04075517695,-48.7802110641077)) ;
#63149 = CARTESIAN_POINT('Ctrl Pts',(30.8968010888553,533.919453643736,-48.7924637012187)) ;
#63150 = CARTESIAN_POINT('Ctrl Pts',(30.8512036997583,533.894539288516,-48.7952082236486)) ;
#63151 = CARTESIAN_POINT('Ctrl Pts',(30.7566582376927,533.84744164903,-48.8009187729786)) ;
#63152 = CARTESIAN_POINT('Ctrl Pts',(30.707686431377,533.825397247532,-48.8038869570241)) ;
#63153 = CARTESIAN_POINT('Ctrl Pts',(30.5956643458089,533.780160627255,-48.8107102818242)) ;
#63154 = CARTESIAN_POINT('Ctrl Pts',(30.5322287080541,533.758091959801,-48.8145979272861)) ;
#63155 = CARTESIAN_POINT('Ctrl Pts',(30.3377825727375,533.70095309641,-48.8265458852118)) ;
#63156 = CARTESIAN_POINT('Ctrl Pts',(30.2042809237263,533.675702165735,-48.8348129996362)) ;
#63157 = CARTESIAN_POINT('Ctrl Pts',(30.0104620705288,533.658586862171,-48.8463374070203)) ;
#63158 = CARTESIAN_POINT('Ctrl Pts',(29.9514522259461,533.655930259869,-48.8497788664516)) ;
#63159 = CARTESIAN_POINT('Ctrl Pts',(29.862778450047,533.65576290418,-48.8547730708599)) ;
#63160 = CARTESIAN_POINT('Ctrl Pts',(29.8331510395665,533.65634774999,-48.8564113135559)) ;
#63161 = CARTESIAN_POINT('Ctrl Pts',(29.7669271382415,533.659089140959,-48.8599934643313)) ;
#63162 = CARTESIAN_POINT('Ctrl Pts',(29.7303565076276,533.661584245061,-48.8619203514904)) ;
#63163 = CARTESIAN_POINT('Ctrl Pts',(29.6485352682143,533.669370640701,-48.8661546058384)) ;
#63164 = CARTESIAN_POINT('Ctrl Pts',(29.6033541592041,533.675191010724,-48.868439803436)) ;
#63165 = CARTESIAN_POINT('Ctrl Pts',(29.4397931584769,533.701815382174,-48.8766340387472)) ;
#63166 = CARTESIAN_POINT('Ctrl Pts',(29.3231049050991,533.731490330573,-48.8823421003453)) ;
#63167 = CARTESIAN_POINT('Ctrl Pts',(29.1255303987832,533.800648702973,-48.8925983927261)) ;
#63168 = CARTESIAN_POINT('Ctrl Pts',(29.0433982438944,533.83554521826,-48.8970516434834)) ;
#63169 = CARTESIAN_POINT('Ctrl Pts',(28.9181967859105,533.898642697004,-48.9043377886449)) ;
#63170 = CARTESIAN_POINT('Ctrl Pts',(28.8734731992443,533.923313404962,-48.9070463441136)) ;
#63171 = CARTESIAN_POINT('Ctrl Pts',(28.782495903055,533.978015763905,-48.9128055638768)) ;
#63172 = CARTESIAN_POINT('Ctrl Pts',(28.7364393900242,534.008294486009,-48.9158640837821)) ;
#63173 = CARTESIAN_POINT('Ctrl Pts',(28.5968448723203,534.108329479567,-48.9256045307346)) ;
#63174 = CARTESIAN_POINT('Ctrl Pts',(28.5080007968297,534.184215561842,-48.9325135703255)) ;
#63175 = CARTESIAN_POINT('Ctrl Pts',(28.3363244911219,534.358163329451,-48.9471897982566)) ;
#63176 = CARTESIAN_POINT('Ctrl Pts',(28.2552406649746,534.457288384783,-48.9549440754408)) ;
#63177 = CARTESIAN_POINT('Ctrl Pts',(28.1651226857596,534.591189234342,-48.9641622118551)) ;
#63178 = CARTESIAN_POINT('Ctrl Pts',(28.1470435395733,534.619528713667,-48.9660475985244)) ;
#63179 = CARTESIAN_POINT('Ctrl Pts',(28.1134540115264,534.675145102815,-48.9696032458967)) ;
#63180 = CARTESIAN_POINT('Ctrl Pts',(28.0978575945542,534.702357842372,-48.9712777588851)) ;
#63181 = CARTESIAN_POINT('Ctrl Pts',(28.0464988262082,534.796923280355,-48.9769119178478)) ;
#63182 = CARTESIAN_POINT('Ctrl Pts',(28.0138625654261,534.86590868834,-48.9807092093426)) ;
#63183 = CARTESIAN_POINT('Ctrl Pts',(27.9295186082834,535.073321377053,-48.9916672182404)) ;
#63184 = CARTESIAN_POINT('Ctrl Pts',(27.8888064204059,535.215679883322,-48.9986472242326)) ;
#63185 = CARTESIAN_POINT('Ctrl Pts',(27.8527272342222,535.424769497181,-49.0093009088516)) ;
#63186 = CARTESIAN_POINT('Ctrl Pts',(27.8447565767471,535.488841886332,-49.0126121056994)) ;
#63187 = CARTESIAN_POINT('Ctrl Pts',(27.8360411363504,535.602292071308,-49.018621250477)) ;
#63188 = CARTESIAN_POINT('Ctrl Pts',(27.8340357012717,535.651521140232,-49.0212764843941)) ;
#63189 = CARTESIAN_POINT('Ctrl Pts',(27.8334920706155,535.765581350514,-49.0275576199013)) ;
#63190 = CARTESIAN_POINT('Ctrl Pts',(27.8362496176875,535.830363180296,-49.0312223608911)) ;
#63191 = CARTESIAN_POINT('Ctrl Pts',(27.8493044253744,535.975294799131,-49.0396387495613)) ;
#63192 = CARTESIAN_POINT('Ctrl Pts',(27.8612762282024,536.055185266311,-49.0444303922878)) ;
#63193 = CARTESIAN_POINT('Ctrl Pts',(27.9067613413416,536.27108303815,-49.0576690138394)) ;
#63194 = CARTESIAN_POINT('Ctrl Pts',(27.9495207150067,536.404707790326,-49.0662027057441)) ;
#63195 = CARTESIAN_POINT('Ctrl Pts',(28.0185405257698,536.562740188445,-49.0760279359963)) ;
#63196 = CARTESIAN_POINT('Ctrl Pts',(28.032255570223,536.592216121502,-49.0778468905781)) ;
#63197 = CARTESIAN_POINT('Ctrl Pts',(28.0611434151041,536.650635032118,-49.08140578559)) ;
#63198 = CARTESIAN_POINT('Ctrl Pts',(28.0763185331564,536.679566137274,-49.0831452063993)) ;
#63199 = CARTESIAN_POINT('Ctrl Pts',(28.1391848763923,536.792772324395,-49.089906784842)) ;
#63200 = CARTESIAN_POINT('Ctrl Pts',(28.1921209509982,536.873999898044,-49.0946614201394)) ;
#63201 = CARTESIAN_POINT('Ctrl Pts',(28.3293440963686,537.055167643582,-49.1057178054702)) ;
#63202 = CARTESIAN_POINT('Ctrl Pts',(28.4178107731256,537.151398051176,-49.1119736958817)) ;
#63203 = CARTESIAN_POINT('Ctrl Pts',(28.554053713274,537.273883161158,-49.1212418129166)) ;
#63204 = CARTESIAN_POINT('Ctrl Pts',(28.5946501464557,537.307645068652,-49.1239612214735)) ;
#63205 = CARTESIAN_POINT('Ctrl Pts',(28.636499183292,537.339804965697,-49.1267434461298)) ;
#63206 = CARTESIAN_POINT('Origin',(29.8885276254155,585.710565160562,-51.0680854522906)) ;
#63207 = CARTESIAN_POINT('Ctrl Pts',(27.8735990520585,585.307997890694,-48.9453612460011)) ;
#63208 = CARTESIAN_POINT('Ctrl Pts',(27.8828319451009,585.261785440258,-48.9430764260291)) ;
#63209 = CARTESIAN_POINT('Ctrl Pts',(27.8936579797779,585.215873972431,-48.940800625095)) ;
#63210 = CARTESIAN_POINT('Ctrl Pts',(27.9347516972393,585.065070751935,-48.9332117860105)) ;
#63211 = CARTESIAN_POINT('Ctrl Pts',(27.9717770230872,584.962255467665,-48.92784200937)) ;
#63212 = CARTESIAN_POINT('Ctrl Pts',(28.0384706308186,584.814993064186,-48.9194872141135)) ;
#63213 = CARTESIAN_POINT('Ctrl Pts',(28.0619826295612,584.767966110018,-48.9167139106165)) ;
#63214 = CARTESIAN_POINT('Ctrl Pts',(28.1130495345266,584.674927375609,-48.9109820561371)) ;
#63215 = CARTESIAN_POINT('Ctrl Pts',(28.140654051435,584.62898979262,-48.908023163243)) ;
#63216 = CARTESIAN_POINT('Ctrl Pts',(28.25590551563,584.453151570968,-48.8961604357202)) ;
#63217 = CARTESIAN_POINT('Ctrl Pts',(28.3564845074397,584.332387613501,-48.8867614008555)) ;
#63218 = CARTESIAN_POINT('Ctrl Pts',(28.5404134475904,584.156821291141,-48.8714760146908)) ;
#63219 = CARTESIAN_POINT('Ctrl Pts',(28.6157669081412,584.094515943848,-48.8656341455121)) ;
#63220 = CARTESIAN_POINT('Ctrl Pts',(28.7218404423022,584.018848949306,-48.8582168333091)) ;
#63221 = CARTESIAN_POINT('Ctrl Pts',(28.7488595555702,584.00053016038,-48.8563920678079)) ;
#63222 = CARTESIAN_POINT('Ctrl Pts',(28.8038317937748,583.965141364442,-48.8528254229299)) ;
#63223 = CARTESIAN_POINT('Ctrl Pts',(28.8317795338927,583.948080260942,-48.8510842726652)) ;
#63224 = CARTESIAN_POINT('Ctrl Pts',(28.9805311904364,583.86208383587,-48.8421258450719)) ;
#63225 = CARTESIAN_POINT('Ctrl Pts',(29.1077080427244,583.804870949162,-48.8354958606823)) ;
#63226 = CARTESIAN_POINT('Ctrl Pts',(29.3164592093386,583.73539949144,-48.8248356009852)) ;
#63227 = CARTESIAN_POINT('Ctrl Pts',(29.3946545399406,583.714411338987,-48.820891855375)) ;
#63228 = CARTESIAN_POINT('Ctrl Pts',(29.5375992007793,583.68495925355,-48.8135627439636)) ;
#63229 = CARTESIAN_POINT('Ctrl Pts',(29.6019008912608,583.67486526629,-48.810224167102)) ;
#63230 = CARTESIAN_POINT('Ctrl Pts',(29.7161079886277,583.662455767892,-48.8041554036916)) ;
#63231 = CARTESIAN_POINT('Ctrl Pts',(29.7658226386929,583.658877197722,-48.8014681105815)) ;
#63232 = CARTESIAN_POINT('Ctrl Pts',(29.8818194143827,583.654758492743,-48.7950728714387)) ;
#63233 = CARTESIAN_POINT('Ctrl Pts',(29.9480922703889,583.655610974656,-48.7913234000719)) ;
#63234 = CARTESIAN_POINT('Ctrl Pts',(30.1613217624503,583.668677305342,-48.7789552567645)) ;
#63235 = CARTESIAN_POINT('Ctrl Pts',(30.3070337244956,583.693496225898,-48.7699997001851)) ;
#63236 = CARTESIAN_POINT('Ctrl Pts',(30.5201616922284,583.753900882992,-48.7567619853803)) ;
#63237 = CARTESIAN_POINT('Ctrl Pts',(30.5903670728376,583.777971065631,-48.7523863572617)) ;
#63238 = CARTESIAN_POINT('Ctrl Pts',(30.6881942252481,583.81754788722,-48.7464057891474)) ;
#63239 = CARTESIAN_POINT('Ctrl Pts',(30.7169959342009,583.829974367012,-48.7446604082429)) ;
#63240 = CARTESIAN_POINT('Ctrl Pts',(30.776733898433,583.857387403823,-48.7410894368781)) ;
#63241 = CARTESIAN_POINT('Ctrl Pts',(30.8076006084095,583.872500052541,-48.7392710751644)) ;
#63242 = CARTESIAN_POINT('Ctrl Pts',(30.9643078236209,583.95416085008,-48.7301062112254)) ;
#63243 = CARTESIAN_POINT('Ctrl Pts',(31.08337668112,584.03288708128,-48.7233476818017)) ;
#63244 = CARTESIAN_POINT('Ctrl Pts',(31.2793757498751,584.19401049874,-48.7110370886051)) ;
#63245 = CARTESIAN_POINT('Ctrl Pts',(31.3594962772446,584.27159173016,-48.7055656014119)) ;
#63246 = CARTESIAN_POINT('Ctrl Pts',(31.4676760674295,584.394866718269,-48.6970930090278)) ;
#63247 = CARTESIAN_POINT('Ctrl Pts',(31.5008820584609,584.435777060235,-48.6943148732855)) ;
#63248 = CARTESIAN_POINT('Ctrl Pts',(31.5645546291345,584.520695390366,-48.6885847556892)) ;
#63249 = CARTESIAN_POINT('Ctrl Pts',(31.5949468372883,584.564707708841,-48.6856329809055)) ;
#63250 = CARTESIAN_POINT('Ctrl Pts',(31.7082083532369,584.743242369691,-48.6737082586726)) ;
#63251 = CARTESIAN_POINT('Ctrl Pts',(31.7771541839664,584.885928113124,-48.6642293704264)) ;
#63252 = CARTESIAN_POINT('Ctrl Pts',(31.8608933388827,585.126491965216,-48.6489198893472)) ;
#63253 = CARTESIAN_POINT('Ctrl Pts',(31.8862189720269,585.220054905014,-48.6431314359125)) ;
#63254 = CARTESIAN_POINT('Ctrl Pts',(31.911132813277,585.347068647145,-48.6357643033073)) ;
#63255 = CARTESIAN_POINT('Ctrl Pts',(31.9166485219174,585.379223371689,-48.633940884459)) ;
#63256 = CARTESIAN_POINT('Ctrl Pts',(31.9261678452045,585.443929675183,-48.63037338205)) ;
#63257 = CARTESIAN_POINT('Ctrl Pts',(31.930162588974,585.476473087068,-48.628630178473)) ;
#63258 = CARTESIAN_POINT('Ctrl Pts',(31.9399954942879,585.576276100018,-48.6234023185067)) ;
#63259 = CARTESIAN_POINT('Ctrl Pts',(31.9433001626235,585.643742882456,-48.6200309199534)) ;
#63260 = CARTESIAN_POINT('Ctrl Pts',(31.9432268809865,585.862142072657,-48.6093098625096)) ;
#63261 = CARTESIAN_POINT('Ctrl Pts',(31.9265570734146,586.012561161177,-48.6021883339017)) ;
#63262 = CARTESIAN_POINT('Ctrl Pts',(31.8791982766796,586.223933774399,-48.5913218257441)) ;
#63263 = CARTESIAN_POINT('Ctrl Pts',(31.8617617266439,586.287334633891,-48.5879525832714)) ;
#63264 = CARTESIAN_POINT('Ctrl Pts',(31.8258196602408,586.397135777016,-48.5818536579686)) ;
#63265 = CARTESIAN_POINT('Ctrl Pts',(31.8086049423566,586.443901463165,-48.5791688934032)) ;
#63266 = CARTESIAN_POINT('Ctrl Pts',(31.7648496519996,586.55062944245,-48.5728179108504)) ;
#63267 = CARTESIAN_POINT('Ctrl Pts',(31.7371060415975,586.610036573832,-48.5691122456167)) ;
#63268 = CARTESIAN_POINT('Ctrl Pts',(31.6683752720788,586.740545806259,-48.5605811907351)) ;
#63269 = CARTESIAN_POINT('Ctrl Pts',(31.625873047702,586.810722795197,-48.5557143506426)) ;
#63270 = CARTESIAN_POINT('Ctrl Pts',(31.5019234464376,586.990210141892,-48.5426325634253)) ;
#63271 = CARTESIAN_POINT('Ctrl Pts',(31.413602052318,587.0942881016,-48.5343477697469)) ;
#63272 = CARTESIAN_POINT('Ctrl Pts',(31.2918750230757,587.211799269043,-48.5247059847297)) ;
#63273 = CARTESIAN_POINT('Ctrl Pts',(31.2675689369299,587.234157335596,-48.5228579173838)) ;
#63274 = CARTESIAN_POINT('Ctrl Pts',(31.2183674720407,587.277272892066,-48.5192856052886)) ;
#63275 = CARTESIAN_POINT('Ctrl Pts',(31.1934990656334,587.298046468125,-48.5175605810797)) ;
#63276 = CARTESIAN_POINT('Ctrl Pts',(31.0969248872281,587.37491495707,-48.5111173943664)) ;
#63277 = CARTESIAN_POINT('Ctrl Pts',(31.0220055134937,587.426815492891,-48.5066362620309)) ;
#63278 = CARTESIAN_POINT('Ctrl Pts',(30.8084278084011,587.5546651062,-48.4945322749571)) ;
#63279 = CARTESIAN_POINT('Ctrl Pts',(30.6640884365156,587.619864514387,-48.4870182239858)) ;
#63280 = CARTESIAN_POINT('Ctrl Pts',(30.461216012842,587.684662981642,-48.4761035926813)) ;
#63281 = CARTESIAN_POINT('Ctrl Pts',(30.4080735160824,587.699309868848,-48.4732194884917)) ;
#63282 = CARTESIAN_POINT('Ctrl Pts',(30.3041724313787,587.723497724343,-48.4674975042467)) ;
#63283 = CARTESIAN_POINT('Ctrl Pts',(30.2535163502199,587.733296150955,-48.4646706110966)) ;
#63284 = CARTESIAN_POINT('Ctrl Pts',(30.1109173362283,587.755348132967,-48.4565926048347)) ;
#63285 = CARTESIAN_POINT('Ctrl Pts',(30.0184430545465,587.763298232305,-48.4512109170444)) ;
#63286 = CARTESIAN_POINT('Ctrl Pts',(29.7881874387505,587.767470850485,-48.4375458956304)) ;
#63287 = CARTESIAN_POINT('Ctrl Pts',(29.6507208797945,587.756139860824,-48.4291382587002)) ;
#63288 = CARTESIAN_POINT('Ctrl Pts',(29.4673457254583,587.722279197781,-48.418199947024)) ;
#63289 = CARTESIAN_POINT('Ctrl Pts',(29.419599086166,587.71168842582,-48.4153815054089)) ;
#63290 = CARTESIAN_POINT('Ctrl Pts',(29.3439784790511,587.692059110938,-48.411013048576)) ;
#63291 = CARTESIAN_POINT('Ctrl Pts',(29.3158444361789,587.684111794925,-48.4094108937611)) ;
#63292 = CARTESIAN_POINT('Ctrl Pts',(29.2479414463373,587.66335584115,-48.4056037101182)) ;
#63293 = CARTESIAN_POINT('Ctrl Pts',(29.2083769251862,587.649930420049,-48.4034312895463)) ;
#63294 = CARTESIAN_POINT('Ctrl Pts',(29.0649387296169,587.596327198067,-48.3956329475004)) ;
#63295 = CARTESIAN_POINT('Ctrl Pts',(28.9639642494161,587.548929494315,-48.3902876589681)) ;
#63296 = CARTESIAN_POINT('Ctrl Pts',(28.7605616866109,587.432432512032,-48.3789415175016)) ;
#63297 = CARTESIAN_POINT('Ctrl Pts',(28.6595147948651,587.361824738476,-48.3729455374816)) ;
#63298 = CARTESIAN_POINT('Ctrl Pts',(28.5245997117867,587.248271804966,-48.3638584784995)) ;
#63299 = CARTESIAN_POINT('Ctrl Pts',(28.4851572127738,587.212361374696,-48.3610527891648)) ;
#63300 = CARTESIAN_POINT('Ctrl Pts',(28.4095418356387,587.137934913229,-48.3553365899688)) ;
#63301 = CARTESIAN_POINT('Ctrl Pts',(28.3733689587353,587.099477274376,-48.3524296095634)) ;
#63302 = CARTESIAN_POINT('Ctrl Pts',(28.2637347117484,586.973533130021,-48.3430345374575)) ;
#63303 = CARTESIAN_POINT('Ctrl Pts',(28.1960723420737,586.881303856626,-48.3363197263494)) ;
#63304 = CARTESIAN_POINT('Ctrl Pts',(28.0647700036677,586.666976164258,-48.3212673541831)) ;
#63305 = CARTESIAN_POINT('Ctrl Pts',(28.0050033170084,586.543123266581,-48.3129077669416)) ;
#63306 = CARTESIAN_POINT('Ctrl Pts',(27.9460310373271,586.381334024594,-48.303041472131)) ;
#63307 = CARTESIAN_POINT('Ctrl Pts',(27.9348807829284,586.348129439641,-48.3010707738538)) ;
#63308 = CARTESIAN_POINT('Ctrl Pts',(27.9154793199297,586.285053645666,-48.2974500155675)) ;
#63309 = CARTESIAN_POINT('Ctrl Pts',(27.9070448732466,586.255251131039,-48.2957915775275)) ;
#63310 = CARTESIAN_POINT('Ctrl Pts',(27.8819134032908,586.158122291074,-48.2905239125927)) ;
#63311 = CARTESIAN_POINT('Ctrl Pts',(27.8679490942094,586.090133423294,-48.2870460380664)) ;
#63312 = CARTESIAN_POINT('Ctrl Pts',(27.8347763925141,585.87348791356,-48.2762644177513)) ;
#63313 = CARTESIAN_POINT('Ctrl Pts',(27.828363726723,585.723379597226,-48.2692008448875)) ;
#63314 = CARTESIAN_POINT('Ctrl Pts',(27.8428558433911,585.505966301211,-48.2583071991447)) ;
#63315 = CARTESIAN_POINT('Ctrl Pts',(27.8507581869572,585.438300178,-48.2548284056049)) ;
#63316 = CARTESIAN_POINT('Ctrl Pts',(27.8655401484261,585.35004119791,-48.2501155276743)) ;
#63317 = CARTESIAN_POINT('Ctrl Pts',(27.869405730716,585.328986290629,-48.2489781223699)) ;
#63318 = CARTESIAN_POINT('Ctrl Pts',(27.8735990532433,585.307997884764,-48.2478302996211)) ;
#63319 = CARTESIAN_POINT('Ctrl Pts',(27.8735990519255,585.30799789136,-48.3063633758768)) ;
#63320 = CARTESIAN_POINT('Ctrl Pts',(27.8690228437001,585.330902716012,-48.3075791955719)) ;
#63321 = CARTESIAN_POINT('Ctrl Pts',(27.8648370620205,585.353886230142,-48.3087777345022)) ;
#63322 = CARTESIAN_POINT('Ctrl Pts',(27.8390652940413,585.510503910103,-48.3168292564892)) ;
#63323 = CARTESIAN_POINT('Ctrl Pts',(27.8303373251784,585.645923443368,-48.3232401464756)) ;
#63324 = CARTESIAN_POINT('Ctrl Pts',(27.8384534431231,585.881794760119,-48.3347322963557)) ;
#63325 = CARTESIAN_POINT('Ctrl Pts',(27.8492967927589,585.981966326658,-48.3397132810064)) ;
#63326 = CARTESIAN_POINT('Ctrl Pts',(27.8767835625487,586.131961236808,-48.3476078620855)) ;
#63327 = CARTESIAN_POINT('Ctrl Pts',(27.8880629202371,586.182612978086,-48.3503494002897)) ;
#63328 = CARTESIAN_POINT('Ctrl Pts',(27.9148999336193,586.284740695226,-48.3560593161279)) ;
#63329 = CARTESIAN_POINT('Ctrl Pts',(27.9305853769514,586.336141047699,-48.3590301089257)) ;
#63330 = CARTESIAN_POINT('Ctrl Pts',(28.0041461221571,586.547182336332,-48.3716558018206)) ;
#63331 = CARTESIAN_POINT('Ctrl Pts',(28.0796746256448,586.699936179463,-48.3819088839737)) ;
#63332 = CARTESIAN_POINT('Ctrl Pts',(28.2195680883585,586.912104584204,-48.3971489536296)) ;
#63333 = CARTESIAN_POINT('Ctrl Pts',(28.2703364620774,586.979652496502,-48.4021628299502)) ;
#63334 = CARTESIAN_POINT('Ctrl Pts',(28.3458498138865,587.068196646234,-48.4087753481411)) ;
#63335 = CARTESIAN_POINT('Ctrl Pts',(28.367144985269,587.092018480801,-48.4105583281068)) ;
#63336 = CARTESIAN_POINT('Ctrl Pts',(28.4115786577177,587.139449722224,-48.4140988523607)) ;
#63337 = CARTESIAN_POINT('Ctrl Pts',(28.4347483876723,587.163016726596,-48.4158535092086)) ;
#63338 = CARTESIAN_POINT('Ctrl Pts',(28.5152613527078,587.241052220625,-48.4216904835596)) ;
#63339 = CARTESIAN_POINT('Ctrl Pts',(28.5751797018589,587.292769400038,-48.4256068227319)) ;
#63340 = CARTESIAN_POINT('Ctrl Pts',(28.7800497785067,587.449919877474,-48.4382057697603)) ;
#63341 = CARTESIAN_POINT('Ctrl Pts',(28.9357954566398,587.539875874447,-48.4466712248569)) ;
#63342 = CARTESIAN_POINT('Ctrl Pts',(29.1493943090872,587.628480243647,-48.4586298525516)) ;
#63343 = CARTESIAN_POINT('Ctrl Pts',(29.1982964077967,587.646616950942,-48.4613824294678)) ;
#63344 = CARTESIAN_POINT('Ctrl Pts',(29.2985454382891,587.679515985023,-48.4670824176221)) ;
#63345 = CARTESIAN_POINT('Ctrl Pts',(29.3498836496353,587.694175061945,-48.4700307273956)) ;
#63346 = CARTESIAN_POINT('Ctrl Pts',(29.5197955539668,587.735608946595,-48.4798998520205)) ;
#63347 = CARTESIAN_POINT('Ctrl Pts',(29.6401659782254,587.753865198461,-48.4870832547293)) ;
#63348 = CARTESIAN_POINT('Ctrl Pts',(29.8910236896231,587.769412130909,-48.5021700893767)) ;
#63349 = CARTESIAN_POINT('Ctrl Pts',(30.0210952415389,587.765142155608,-48.5100541145676)) ;
#63350 = CARTESIAN_POINT('Ctrl Pts',(30.1830775202678,587.744368702829,-48.5193760254863)) ;
#63351 = CARTESIAN_POINT('Ctrl Pts',(30.2161495560777,587.739303846438,-48.5212515552003)) ;
#63352 = CARTESIAN_POINT('Ctrl Pts',(30.2802145057086,587.727884859259,-48.5248110660856)) ;
#63353 = CARTESIAN_POINT('Ctrl Pts',(30.3112126400379,587.721618344097,-48.5264984170095)) ;
#63354 = CARTESIAN_POINT('Ctrl Pts',(30.4193240139567,587.697152442163,-48.532298366769)) ;
#63355 = CARTESIAN_POINT('Ctrl Pts',(30.4955244199026,587.675210415306,-48.5362350923644)) ;
#63356 = CARTESIAN_POINT('Ctrl Pts',(30.7439283858594,587.587843422684,-48.5491059307094)) ;
#63357 = CARTESIAN_POINT('Ctrl Pts',(30.908576037651,587.503714459816,-48.557782942845)) ;
#63358 = CARTESIAN_POINT('Ctrl Pts',(31.1025033561642,587.369166800985,-48.5699989843105)) ;
#63359 = CARTESIAN_POINT('Ctrl Pts',(31.1440457843143,587.337946485946,-48.5727436769571)) ;
#63360 = CARTESIAN_POINT('Ctrl Pts',(31.2259880310742,587.271358123653,-48.5784518041368)) ;
#63361 = CARTESIAN_POINT('Ctrl Pts',(31.266273824805,587.235914186997,-48.581417268506)) ;
#63362 = CARTESIAN_POINT('Ctrl Pts',(31.3537467349999,587.152659559672,-48.5882373460527)) ;
#63363 = CARTESIAN_POINT('Ctrl Pts',(31.4000681015528,587.104031113529,-48.5921246004308)) ;
#63364 = CARTESIAN_POINT('Ctrl Pts',(31.5322058028293,586.950957186232,-48.6040463371314)) ;
#63365 = CARTESIAN_POINT('Ctrl Pts',(31.6101800892929,586.84023768012,-48.6122863132611)) ;
#63366 = CARTESIAN_POINT('Ctrl Pts',(31.7060343973457,586.670881816087,-48.6238181605086)) ;
#63367 = CARTESIAN_POINT('Ctrl Pts',(31.7330857332409,586.617838816955,-48.6272891512746)) ;
#63368 = CARTESIAN_POINT('Ctrl Pts',(31.7702293329091,586.536454196947,-48.6323295091933)) ;
#63369 = CARTESIAN_POINT('Ctrl Pts',(31.7820649612693,586.508945264748,-48.6339854382212)) ;
#63370 = CARTESIAN_POINT('Ctrl Pts',(31.8070315711429,586.447234262973,-48.6375829953204)) ;
#63371 = CARTESIAN_POINT('Ctrl Pts',(31.8198573330843,586.412921674962,-48.6395084525387)) ;
#63372 = CARTESIAN_POINT('Ctrl Pts',(31.8465466046069,586.335248895486,-48.6437391508926)) ;
#63373 = CARTESIAN_POINT('Ctrl Pts',(31.8599006469411,586.291733757156,-48.6460222327522)) ;
#63374 = CARTESIAN_POINT('Ctrl Pts',(31.9031482904717,586.132082169862,-48.6541998254054)) ;
#63375 = CARTESIAN_POINT('Ctrl Pts',(31.9243086278689,586.013831499553,-48.6598936094312)) ;
#63376 = CARTESIAN_POINT('Ctrl Pts',(31.9430560449183,585.805137605915,-48.6701546020348)) ;
#63377 = CARTESIAN_POINT('Ctrl Pts',(31.9452252036312,585.715446883614,-48.6746292400956)) ;
#63378 = CARTESIAN_POINT('Ctrl Pts',(31.9394273758999,585.574848092713,-48.6819400183033)) ;
#63379 = CARTESIAN_POINT('Ctrl Pts',(31.9354181095184,585.523889967366,-48.6846498826931)) ;
#63380 = CARTESIAN_POINT('Ctrl Pts',(31.9231581134606,585.418500244412,-48.6904046266792)) ;
#63381 = CARTESIAN_POINT('Ctrl Pts',(31.9146113726914,585.364144952808,-48.6934570295856)) ;
#63382 = CARTESIAN_POINT('Ctrl Pts',(31.8813274578258,585.196599033984,-48.7031425264944)) ;
#63383 = CARTESIAN_POINT('Ctrl Pts',(31.8491976755306,585.085121853984,-48.7099987741587)) ;
#63384 = CARTESIAN_POINT('Ctrl Pts',(31.7618473796161,584.856588605335,-48.7246853652262)) ;
#63385 = CARTESIAN_POINT('Ctrl Pts',(31.7046165347513,584.740808679616,-48.7325066943848)) ;
#63386 = CARTESIAN_POINT('Ctrl Pts',(31.6193039812691,584.602623578027,-48.7417782112384)) ;
#63387 = CARTESIAN_POINT('Ctrl Pts',(31.6009968757251,584.574532278801,-48.743658131563)) ;
#63388 = CARTESIAN_POINT('Ctrl Pts',(31.564135806747,584.520888379468,-48.7472188962191)) ;
#63389 = CARTESIAN_POINT('Ctrl Pts',(31.5456647166443,584.495291354427,-48.7489033896821)) ;
#63390 = CARTESIAN_POINT('Ctrl Pts',(31.4792960486314,584.407646868004,-48.7546569552136)) ;
#63391 = CARTESIAN_POINT('Ctrl Pts',(31.4284408198576,584.347917075783,-48.7585541613219)) ;
#63392 = CARTESIAN_POINT('Ctrl Pts',(31.2461032371271,584.157044787966,-48.7714616286157)) ;
#63393 = CARTESIAN_POINT('Ctrl Pts',(31.1003368320949,584.040848178069,-48.7802013217019)) ;
#63394 = CARTESIAN_POINT('Ctrl Pts',(30.8963609148751,583.91920677185,-48.792495130875)) ;
#63395 = CARTESIAN_POINT('Ctrl Pts',(30.8507831878443,583.894317270325,-48.795238442322)) ;
#63396 = CARTESIAN_POINT('Ctrl Pts',(30.7562128637324,583.847232878694,-48.8009504752684)) ;
#63397 = CARTESIAN_POINT('Ctrl Pts',(30.7071940154448,583.825182060003,-48.8039215382368)) ;
#63398 = CARTESIAN_POINT('Ctrl Pts',(30.5951231463654,583.779962696501,-48.8107479231404)) ;
#63399 = CARTESIAN_POINT('Ctrl Pts',(30.5316876920127,583.757913907858,-48.8146356004414)) ;
#63400 = CARTESIAN_POINT('Ctrl Pts',(30.3368011223745,583.700703582632,-48.8266105337954)) ;
#63401 = CARTESIAN_POINT('Ctrl Pts',(30.2028394406781,583.675449026812,-48.8349061745544)) ;
#63402 = CARTESIAN_POINT('Ctrl Pts',(30.0096246377573,583.658567824103,-48.8463896495128)) ;
#63403 = CARTESIAN_POINT('Ctrl Pts',(29.9516866572799,583.655967981502,-48.8497677902681)) ;
#63404 = CARTESIAN_POINT('Ctrl Pts',(29.8636999550514,583.655745975151,-48.8547258247118)) ;
#63405 = CARTESIAN_POINT('Ctrl Pts',(29.8336871087152,583.656327775443,-48.8563859616068)) ;
#63406 = CARTESIAN_POINT('Ctrl Pts',(29.7671110994842,583.659078834743,-48.8599873619322)) ;
#63407 = CARTESIAN_POINT('Ctrl Pts',(29.7305731984307,583.661568119779,-48.8619126603701)) ;
#63408 = CARTESIAN_POINT('Ctrl Pts',(29.6488461600364,583.669335506126,-48.8661423306649)) ;
#63409 = CARTESIAN_POINT('Ctrl Pts',(29.6037261636613,583.675140322987,-48.8684246141494)) ;
#63410 = CARTESIAN_POINT('Ctrl Pts',(29.4406495549682,583.701650174253,-48.8765949855997)) ;
#63411 = CARTESIAN_POINT('Ctrl Pts',(29.3243685952474,583.731156027315,-48.8822831449036)) ;
#63412 = CARTESIAN_POINT('Ctrl Pts',(29.126784185655,583.800130410762,-48.8925342947638)) ;
#63413 = CARTESIAN_POINT('Ctrl Pts',(29.0442790184281,583.835130255024,-48.897005152448)) ;
#63414 = CARTESIAN_POINT('Ctrl Pts',(28.9186937752864,583.898375876284,-48.9043114003962)) ;
#63415 = CARTESIAN_POINT('Ctrl Pts',(28.8739400100024,583.923047596241,-48.907020956715)) ;
#63416 = CARTESIAN_POINT('Ctrl Pts',(28.7829843422024,583.977706208729,-48.9127771452116)) ;
#63417 = CARTESIAN_POINT('Ctrl Pts',(28.7369756716019,584.007933853613,-48.915831396764)) ;
#63418 = CARTESIAN_POINT('Ctrl Pts',(28.5979521401743,584.107486581062,-48.9255279598643)) ;
#63419 = CARTESIAN_POINT('Ctrl Pts',(28.5095622067334,584.182856292733,-48.9323942184793)) ;
#63420 = CARTESIAN_POINT('Ctrl Pts',(28.337296920253,584.356935707098,-48.9470991196433)) ;
#63421 = CARTESIAN_POINT('Ctrl Pts',(28.2554111077127,584.456944982158,-48.9549286022389)) ;
#63422 = CARTESIAN_POINT('Ctrl Pts',(28.1647351501012,584.591788832908,-48.9642070074243)) ;
#63423 = CARTESIAN_POINT('Ctrl Pts',(28.1467139496469,584.620057762267,-48.9660868586587)) ;
#63424 = CARTESIAN_POINT('Ctrl Pts',(28.1131460555267,584.675670902665,-48.9696409850396)) ;
#63425 = CARTESIAN_POINT('Ctrl Pts',(28.0975200670127,584.70295516496,-48.971319153325)) ;
#63426 = CARTESIAN_POINT('Ctrl Pts',(28.0456916234135,584.798469928606,-48.9770072326492)) ;
#63427 = CARTESIAN_POINT('Ctrl Pts',(28.0127105198681,584.868380767047,-48.9808502668949)) ;
#63428 = CARTESIAN_POINT('Ctrl Pts',(27.9355998469476,585.058990289846,-48.9909079132612)) ;
#63429 = CARTESIAN_POINT('Ctrl Pts',(27.8987327219357,585.182198904562,-48.9969997855251)) ;
#63430 = CARTESIAN_POINT('Ctrl Pts',(27.873599044712,585.307997927464,-49.0033678610064)) ;
#63431 = CARTESIAN_POINT('Origin',(179.888527625416,585.710565160536,-51.0680854522974)) ;
#63432 = CARTESIAN_POINT('Ctrl Pts',(178.636459914524,587.339774787883,-49.0681958067691)) ;
#63433 = CARTESIAN_POINT('Ctrl Pts',(178.522689824047,587.252341068882,-49.0609089955289)) ;
#63434 = CARTESIAN_POINT('Ctrl Pts',(178.418390122109,587.153232145152,-49.0541378047761)) ;
#63435 = CARTESIAN_POINT('Ctrl Pts',(178.263316915004,586.971436619688,-49.0424708890543)) ;
#63436 = CARTESIAN_POINT('Ctrl Pts',(178.206516730537,586.894602127817,-49.0377266465304)) ;
#63437 = CARTESIAN_POINT('Ctrl Pts',(178.127449532883,586.77041603943,-49.0300912475289)) ;
#63438 = CARTESIAN_POINT('Ctrl Pts',(178.101297597512,586.725694763998,-49.0273491424362)) ;
#63439 = CARTESIAN_POINT('Ctrl Pts',(178.051005767729,586.631713724577,-49.021575057535)) ;
#63440 = CARTESIAN_POINT('Ctrl Pts',(178.027092924293,586.58238010058,-49.0185377642252)) ;
#63441 = CARTESIAN_POINT('Ctrl Pts',(177.940642160745,586.384206873234,-49.0062942105506)) ;
#63442 = CARTESIAN_POINT('Ctrl Pts',(177.893768281776,586.229189329091,-48.9965660400011)) ;
#63443 = CARTESIAN_POINT('Ctrl Pts',(177.854678192988,586.0093725406,-48.9831611277426)) ;
#63444 = CARTESIAN_POINT('Ctrl Pts',(177.846599334791,585.947965532311,-48.9794652477825)) ;
#63445 = CARTESIAN_POINT('Ctrl Pts',(177.837487294457,585.841805777013,-48.9732488868553)) ;
#63446 = CARTESIAN_POINT('Ctrl Pts',(177.835119794265,585.797210488457,-48.9706899204887)) ;
#63447 = CARTESIAN_POINT('Ctrl Pts',(177.833611346328,585.723437875262,-48.9665810771249)) ;
#63448 = CARTESIAN_POINT('Ctrl Pts',(177.833635366424,585.694297698019,-48.9649921358541)) ;
#63449 = CARTESIAN_POINT('Ctrl Pts',(177.835281913436,585.619799203005,-48.9610139143282)) ;
#63450 = CARTESIAN_POINT('Ctrl Pts',(177.837786954949,585.574478011413,-48.9586687963965)) ;
#63451 = CARTESIAN_POINT('Ctrl Pts',(177.853814028621,585.3935360709,-48.9494781205464)) ;
#63452 = CARTESIAN_POINT('Ctrl Pts',(177.879310822462,585.25932244537,-48.9430298320477)) ;
#63453 = CARTESIAN_POINT('Ctrl Pts',(177.945645425027,585.034698538346,-48.9316092583279)) ;
#63454 = CARTESIAN_POINT('Ctrl Pts',(177.980056095126,584.942892878263,-48.9267512485983)) ;
#63455 = CARTESIAN_POINT('Ctrl Pts',(178.042531888474,584.806687457151,-48.9189858219906)) ;
#63456 = CARTESIAN_POINT('Ctrl Pts',(178.065966781665,584.760319675901,-48.916238143136)) ;
#63457 = CARTESIAN_POINT('Ctrl Pts',(178.117532437603,584.667233005862,-48.9104776963002)) ;
#63458 = CARTESIAN_POINT('Ctrl Pts',(178.145816310086,584.620646628206,-48.9074607853636)) ;
#63459 = CARTESIAN_POINT('Ctrl Pts',(178.266774481441,584.438183718587,-48.8950746231816)) ;
#63460 = CARTESIAN_POINT('Ctrl Pts',(178.373746595138,584.31254505927,-48.8851563924031)) ;
#63461 = CARTESIAN_POINT('Ctrl Pts',(178.558831940002,584.141625852043,-48.8700354875747)) ;
#63462 = CARTESIAN_POINT('Ctrl Pts',(178.626881298135,584.086400061102,-48.8648260157736)) ;
#63463 = CARTESIAN_POINT('Ctrl Pts',(178.724517861708,584.017013502868,-48.8580161973399)) ;
#63464 = CARTESIAN_POINT('Ctrl Pts',(178.751222167727,583.998965739427,-48.8562168865875)) ;
#63465 = CARTESIAN_POINT('Ctrl Pts',(178.80627834916,583.963614600199,-48.8526517590939)) ;
#63466 = CARTESIAN_POINT('Ctrl Pts',(178.834647057342,583.946355482336,-48.8508885711469)) ;
#63467 = CARTESIAN_POINT('Ctrl Pts',(178.979752297396,583.862825547564,-48.8421723516118)) ;
#63468 = CARTESIAN_POINT('Ctrl Pts',(179.102376273154,583.807412948333,-48.8357574399702)) ;
#63469 = CARTESIAN_POINT('Ctrl Pts',(179.344054085458,583.725580796474,-48.823399720558)) ;
#63470 = CARTESIAN_POINT('Ctrl Pts',(179.461759004591,583.696991396647,-48.8174947155024)) ;
#63471 = CARTESIAN_POINT('Ctrl Pts',(179.633719296693,583.670986157263,-48.8085216136563)) ;
#63472 = CARTESIAN_POINT('Ctrl Pts',(179.686437232935,583.665090012014,-48.8057280772725)) ;
#63473 = CARTESIAN_POINT('Ctrl Pts',(179.792320510631,583.657380911096,-48.8000024926176)) ;
#63474 = CARTESIAN_POINT('Ctrl Pts',(179.845445508399,583.655579867296,-48.7970723574146)) ;
#63475 = CARTESIAN_POINT('Ctrl Pts',(180.060926335081,583.656633792174,-48.7849335265143)) ;
#63476 = CARTESIAN_POINT('Ctrl Pts',(180.222587067262,583.676666557783,-48.7751812275339)) ;
#63477 = CARTESIAN_POINT('Ctrl Pts',(180.471670050796,583.738048384186,-48.7597680186341)) ;
#63478 = CARTESIAN_POINT('Ctrl Pts',(180.561514710261,583.766865389574,-48.7541406330392)) ;
#63479 = CARTESIAN_POINT('Ctrl Pts',(180.679291883315,583.81379215604,-48.7469266060518)) ;
#63480 = CARTESIAN_POINT('Ctrl Pts',(180.709226004425,583.826550719338,-48.7451084662837)) ;
#63481 = CARTESIAN_POINT('Ctrl Pts',(180.768790643142,583.853627757196,-48.7415404569656)) ;
#63482 = CARTESIAN_POINT('Ctrl Pts',(180.798405516458,583.867957768318,-48.7397918942574)) ;
#63483 = CARTESIAN_POINT('Ctrl Pts',(180.964286668989,583.953199439178,-48.7300732103009)) ;
#63484 = CARTESIAN_POINT('Ctrl Pts',(181.092620945734,584.038511801579,-48.722820078209)) ;
#63485 = CARTESIAN_POINT('Ctrl Pts',(181.266798320066,584.184845340799,-48.7117627085179)) ;
#63486 = CARTESIAN_POINT('Ctrl Pts',(181.320735472359,584.235359807794,-48.7081372771924)) ;
#63487 = CARTESIAN_POINT('Ctrl Pts',(181.414609481846,584.333287916784,-48.7012880526855)) ;
#63488 = CARTESIAN_POINT('Ctrl Pts',(181.455346038366,584.379814425805,-48.6980991100151)) ;
#63489 = CARTESIAN_POINT('Ctrl Pts',(181.525108527616,584.467143560612,-48.6921715423448)) ;
#63490 = CARTESIAN_POINT('Ctrl Pts',(181.554858950221,584.507305576374,-48.6894660025777)) ;
#63491 = CARTESIAN_POINT('Ctrl Pts',(181.623006311283,584.606682601377,-48.6828008938031)) ;
#63492 = CARTESIAN_POINT('Ctrl Pts',(181.65987240215,584.666865477177,-48.6787869761349)) ;
#63493 = CARTESIAN_POINT('Ctrl Pts',(181.763135641178,584.856725704305,-48.6662039900775)) ;
#63494 = CARTESIAN_POINT('Ctrl Pts',(181.81890660503,584.99165820294,-48.6573377394081)) ;
#63495 = CARTESIAN_POINT('Ctrl Pts',(181.87928210976,585.197145618763,-48.6445728069065)) ;
#63496 = CARTESIAN_POINT('Ctrl Pts',(181.895313275056,585.263893045385,-48.6405415153138)) ;
#63497 = CARTESIAN_POINT('Ctrl Pts',(181.913680446364,585.361697291086,-48.6349124431078)) ;
#63498 = CARTESIAN_POINT('Ctrl Pts',(181.91869925795,585.392200109153,-48.6331958475187)) ;
#63499 = CARTESIAN_POINT('Ctrl Pts',(181.92795281846,585.457624697237,-48.6296123162934)) ;
#63500 = CARTESIAN_POINT('Ctrl Pts',(181.931982999312,585.4925641147,-48.6277555916354)) ;
#63501 = CARTESIAN_POINT('Ctrl Pts',(181.947236975738,585.663182508792,-48.6188920450278)) ;
#63502 = CARTESIAN_POINT('Ctrl Pts',(181.945855938037,585.799656253923,-48.6124091025634)) ;
#63503 = CARTESIAN_POINT('Ctrl Pts',(181.922326698606,586.013781540776,-48.6019658601517)) ;
#63504 = CARTESIAN_POINT('Ctrl Pts',(181.909119525765,586.091991740365,-48.598096296473)) ;
#63505 = CARTESIAN_POINT('Ctrl Pts',(181.877070329413,586.23194127789,-48.5908781356076)) ;
#63506 = CARTESIAN_POINT('Ctrl Pts',(181.859776295897,586.293928463719,-48.5875734407832)) ;
#63507 = CARTESIAN_POINT('Ctrl Pts',(181.823970948016,586.40233213641,-48.5815375256033)) ;
#63508 = CARTESIAN_POINT('Ctrl Pts',(181.806620827009,586.449077359126,-48.5788469790017)) ;
#63509 = CARTESIAN_POINT('Ctrl Pts',(181.761973727089,586.557145164089,-48.5723991884735)) ;
#63510 = CARTESIAN_POINT('Ctrl Pts',(181.733339478999,586.617849994804,-48.5685979421081)) ;
#63511 = CARTESIAN_POINT('Ctrl Pts',(181.632601722606,586.806849982821,-48.556183876341)) ;
#63512 = CARTESIAN_POINT('Ctrl Pts',(181.549677715302,586.928845632812,-48.547241692017)) ;
#63513 = CARTESIAN_POINT('Ctrl Pts',(181.407207624141,587.09654285752,-48.5340987047981)) ;
#63514 = CARTESIAN_POINT('Ctrl Pts',(181.357024989695,587.149606648158,-48.5297961754443)) ;
#63515 = CARTESIAN_POINT('Ctrl Pts',(181.281454639671,587.221435715396,-48.5238896250166)) ;
#63516 = CARTESIAN_POINT('Ctrl Pts',(181.258296910142,587.242462029363,-48.5221498622642)) ;
#63517 = CARTESIAN_POINT('Ctrl Pts',(181.208581063148,587.28557262162,-48.5185759543543)) ;
#63518 = CARTESIAN_POINT('Ctrl Pts',(181.181928866263,587.307532011327,-48.5167496317691)) ;
#63519 = CARTESIAN_POINT('Ctrl Pts',(181.043599643916,587.415768600393,-48.5076442549347)) ;
#63520 = CARTESIAN_POINT('Ctrl Pts',(180.923790899984,587.491056305203,-48.5009400328627)) ;
#63521 = CARTESIAN_POINT('Ctrl Pts',(180.698526771038,587.602125994094,-48.4887557721398)) ;
#63522 = CARTESIAN_POINT('Ctrl Pts',(180.596112403444,587.642771595279,-48.4833537154891)) ;
#63523 = CARTESIAN_POINT('Ctrl Pts',(180.440126484713,587.690605967853,-48.474939652445)) ;
#63524 = CARTESIAN_POINT('Ctrl Pts',(180.388726357869,587.704210926344,-48.4721408598607)) ;
#63525 = CARTESIAN_POINT('Ctrl Pts',(180.285120463092,587.727375122811,-48.4664174503528)) ;
#63526 = CARTESIAN_POINT('Ctrl Pts',(180.23295699744,587.736935306598,-48.46349535866)) ;
#63527 = CARTESIAN_POINT('Ctrl Pts',(180.0613123979,587.761574140313,-48.4537313138675)) ;
#63528 = CARTESIAN_POINT('Ctrl Pts',(179.940882315252,587.76817161978,-48.4466303077961)) ;
#63529 = CARTESIAN_POINT('Ctrl Pts',(179.685650283496,587.75972720534,-48.4313129222973)) ;
#63530 = CARTESIAN_POINT('Ctrl Pts',(179.551480027487,587.741975269937,-48.4231018376695)) ;
#63531 = CARTESIAN_POINT('Ctrl Pts',(179.38776014391,587.703634904507,-48.4135168793249)) ;
#63532 = CARTESIAN_POINT('Ctrl Pts',(179.355689312904,587.695301590795,-48.4116621103499)) ;
#63533 = CARTESIAN_POINT('Ctrl Pts',(179.292788168715,587.677322521817,-48.4080889064942)) ;
#63534 = CARTESIAN_POINT('Ctrl Pts',(179.26195620651,587.667718319085,-48.4063692453072)) ;
#63535 = CARTESIAN_POINT('Ctrl Pts',(179.147243409052,587.628996148952,-48.4000473936535)) ;
#63536 = CARTESIAN_POINT('Ctrl Pts',(179.065045314335,587.595176417414,-48.3956700578852)) ;
#63537 = CARTESIAN_POINT('Ctrl Pts',(178.862019777161,587.495813986433,-48.3846717806871)) ;
#63538 = CARTESIAN_POINT('Ctrl Pts',(178.745170702555,587.423320370498,-48.3781399215745)) ;
#63539 = CARTESIAN_POINT('Ctrl Pts',(178.636459914529,587.339774787887,-48.3712343220044)) ;
#63540 = CARTESIAN_POINT('Ctrl Pts',(178.636459914542,587.339774787898,-48.4293959864656)) ;
#63541 = CARTESIAN_POINT('Ctrl Pts',(178.636986385796,587.340179387555,-48.4294283938969)) ;
#63542 = CARTESIAN_POINT('Ctrl Pts',(178.637513057153,587.340583735086,-48.4294607971127)) ;
#63543 = CARTESIAN_POINT('Ctrl Pts',(178.780119962262,587.449959164934,-48.4382301728603)) ;
#63544 = CARTESIAN_POINT('Ctrl Pts',(178.9358216619,587.539884349372,-48.4466934278485)) ;
#63545 = CARTESIAN_POINT('Ctrl Pts',(179.149377938323,587.628474150212,-48.4586496940449)) ;
#63546 = CARTESIAN_POINT('Ctrl Pts',(179.198287363263,587.646613939987,-48.4614026870224)) ;
#63547 = CARTESIAN_POINT('Ctrl Pts',(179.298552188786,587.6795182441,-48.4671035874245)) ;
#63548 = CARTESIAN_POINT('Ctrl Pts',(179.349898874392,587.694179430637,-48.4700523947607)) ;
#63549 = CARTESIAN_POINT('Ctrl Pts',(179.519877132353,587.735627344895,-48.4799254234614)) ;
#63550 = CARTESIAN_POINT('Ctrl Pts',(179.640307299081,587.753885882769,-48.4871125309897)) ;
#63551 = CARTESIAN_POINT('Ctrl Pts',(179.891138871261,587.769406518002,-48.5021978670502)) ;
#63552 = CARTESIAN_POINT('Ctrl Pts',(180.021122982765,587.765134883684,-48.5100763857469)) ;
#63553 = CARTESIAN_POINT('Ctrl Pts',(180.183029478466,587.744375820552,-48.5193940738666)) ;
#63554 = CARTESIAN_POINT('Ctrl Pts',(180.216111276431,587.739310188868,-48.5212701829362)) ;
#63555 = CARTESIAN_POINT('Ctrl Pts',(180.280186931822,587.727890227682,-48.5248303227102)) ;
#63556 = CARTESIAN_POINT('Ctrl Pts',(180.311186074878,587.721623942164,-48.5265177421839)) ;
#63557 = CARTESIAN_POINT('Ctrl Pts',(180.419277045108,587.697164106773,-48.5323166307148)) ;
#63558 = CARTESIAN_POINT('Ctrl Pts',(180.495456715961,587.675230437209,-48.536252332983)) ;
#63559 = CARTESIAN_POINT('Ctrl Pts',(180.743893023261,587.587864663703,-48.5491247834839)) ;
#63560 = CARTESIAN_POINT('Ctrl Pts',(180.908588464011,587.503712761536,-48.5578040218231)) ;
#63561 = CARTESIAN_POINT('Ctrl Pts',(181.102559876962,587.36912563149,-48.5700232054645)) ;
#63562 = CARTESIAN_POINT('Ctrl Pts',(181.144106331474,587.337899977141,-48.5727682676786)) ;
#63563 = CARTESIAN_POINT('Ctrl Pts',(181.22606380259,587.271293763494,-48.5784777140493)) ;
#63564 = CARTESIAN_POINT('Ctrl Pts',(181.26636025404,587.235836702338,-48.5814441526807)) ;
#63565 = CARTESIAN_POINT('Ctrl Pts',(181.353841079801,587.15256377485,-48.5882654064029)) ;
#63566 = CARTESIAN_POINT('Ctrl Pts',(181.400160421775,587.103931045937,-48.5921528202506)) ;
#63567 = CARTESIAN_POINT('Ctrl Pts',(181.532362375625,586.95076192346,-48.6040813560957)) ;
#63568 = CARTESIAN_POINT('Ctrl Pts',(181.610385325454,586.839938278577,-48.6123283390582)) ;
#63569 = CARTESIAN_POINT('Ctrl Pts',(181.706197873556,586.670565058768,-48.6238586293729)) ;
#63570 = CARTESIAN_POINT('Ctrl Pts',(181.733187936688,586.617623274548,-48.6273223138455)) ;
#63571 = CARTESIAN_POINT('Ctrl Pts',(181.770274577796,586.536350819265,-48.6323551986297)) ;
#63572 = CARTESIAN_POINT('Ctrl Pts',(181.782105644378,586.508848474542,-48.6340105513203)) ;
#63573 = CARTESIAN_POINT('Ctrl Pts',(181.807080991506,586.447107481161,-48.6376094994863)) ;
#63574 = CARTESIAN_POINT('Ctrl Pts',(181.819917790566,586.412757439296,-48.6395367988921)) ;
#63575 = CARTESIAN_POINT('Ctrl Pts',(181.846635156415,586.334976552407,-48.6437727439833)) ;
#63576 = CARTESIAN_POINT('Ctrl Pts',(181.860003628662,586.291390001165,-48.646059132509)) ;
#63577 = CARTESIAN_POINT('Ctrl Pts',(181.903363414394,586.131191237845,-48.6542631907058)) ;
#63578 = CARTESIAN_POINT('Ctrl Pts',(181.924542793204,586.012448485831,-48.6599789005873)) ;
#63579 = CARTESIAN_POINT('Ctrl Pts',(181.943107302616,585.803643157367,-48.6702468529653)) ;
#63580 = CARTESIAN_POINT('Ctrl Pts',(181.945210561466,585.71434246134,-48.6747034291552)) ;
#63581 = CARTESIAN_POINT('Ctrl Pts',(181.939380969133,585.574156434677,-48.6819939094418)) ;
#63582 = CARTESIAN_POINT('Ctrl Pts',(181.935356419543,585.523220455332,-48.6847030665649)) ;
#63583 = CARTESIAN_POINT('Ctrl Pts',(181.923056094147,585.417775264734,-48.6904618170837)) ;
#63584 = CARTESIAN_POINT('Ctrl Pts',(181.914476361646,585.363343471826,-48.6935191872863)) ;
#63585 = CARTESIAN_POINT('Ctrl Pts',(181.880953857306,585.194979441117,-48.7032544617348)) ;
#63586 = CARTESIAN_POINT('Ctrl Pts',(181.848498568229,585.082792307793,-48.7101590874652)) ;
#63587 = CARTESIAN_POINT('Ctrl Pts',(181.761008228129,584.854955107566,-48.7248112828564)) ;
#63588 = CARTESIAN_POINT('Ctrl Pts',(181.704323616753,584.74044106589,-48.7325455574979)) ;
#63589 = CARTESIAN_POINT('Ctrl Pts',(181.619732999493,584.603290776368,-48.7417474150512)) ;
#63590 = CARTESIAN_POINT('Ctrl Pts',(181.601376933468,584.575102190356,-48.7436338706688)) ;
#63591 = CARTESIAN_POINT('Ctrl Pts',(181.564510817635,584.521418669305,-48.7471973382189)) ;
#63592 = CARTESIAN_POINT('Ctrl Pts',(181.546090854515,584.49587453644,-48.7488783845597)) ;
#63593 = CARTESIAN_POINT('Ctrl Pts',(181.480410139887,584.409068774605,-48.7545766846394)) ;
#63594 = CARTESIAN_POINT('Ctrl Pts',(181.430278388951,584.350054412464,-48.7584267985489)) ;
#63595 = CARTESIAN_POINT('Ctrl Pts',(181.27490476644,584.186800623008,-48.7694526822597)) ;
#63596 = CARTESIAN_POINT('Ctrl Pts',(181.161596854038,584.090937153969,-48.7764545529917)) ;
#63597 = CARTESIAN_POINT('Ctrl Pts',(180.985874239071,583.972193801001,-48.7871167467605)) ;
#63598 = CARTESIAN_POINT('Ctrl Pts',(180.931129520611,583.938818904161,-48.7904089452608)) ;
#63599 = CARTESIAN_POINT('Ctrl Pts',(180.831445558496,583.884268596496,-48.7964156207729)) ;
#63600 = CARTESIAN_POINT('Ctrl Pts',(180.787129616573,583.862061107398,-48.7990895235555)) ;
#63601 = CARTESIAN_POINT('Ctrl Pts',(180.681710573235,583.813920899863,-48.8054772419058)) ;
#63602 = CARTESIAN_POINT('Ctrl Pts',(180.62007072229,583.789304654493,-48.8092334701202)) ;
#63603 = CARTESIAN_POINT('Ctrl Pts',(180.4778445923,583.740343394327,-48.8179444675618)) ;
#63604 = CARTESIAN_POINT('Ctrl Pts',(180.396736848833,583.717881101102,-48.8229444977197)) ;
#63605 = CARTESIAN_POINT('Ctrl Pts',(180.187165467769,583.67347121718,-48.8357998319232)) ;
#63606 = CARTESIAN_POINT('Ctrl Pts',(180.057562166302,583.658647193278,-48.8437012290412)) ;
#63607 = CARTESIAN_POINT('Ctrl Pts',(179.89399027169,583.655550361919,-48.8530372674224)) ;
#63608 = CARTESIAN_POINT('Ctrl Pts',(179.860545511911,583.655733547046,-48.8549116000563)) ;
#63609 = CARTESIAN_POINT('Ctrl Pts',(179.795417971214,583.657680861198,-48.8584746829691)) ;
#63610 = CARTESIAN_POINT('Ctrl Pts',(179.763742952266,583.659362514779,-48.8601665525464)) ;
#63611 = CARTESIAN_POINT('Ctrl Pts',(179.651856244361,583.66790420828,-48.8660362043115)) ;
#63612 = CARTESIAN_POINT('Ctrl Pts',(179.572015914379,583.678743371446,-48.8700320578551)) ;
#63613 = CARTESIAN_POINT('Ctrl Pts',(179.314517779207,583.72925344417,-48.8828505384156)) ;
#63614 = CARTESIAN_POINT('Ctrl Pts',(179.141477145102,583.787807317399,-48.8914351977625)) ;
#63615 = CARTESIAN_POINT('Ctrl Pts',(178.931781998375,583.891406220177,-48.9035367927947)) ;
#63616 = CARTESIAN_POINT('Ctrl Pts',(178.886056600082,583.916198242564,-48.9062831764253)) ;
#63617 = CARTESIAN_POINT('Ctrl Pts',(178.79529151434,583.969963319822,-48.9119847847951)) ;
#63618 = CARTESIAN_POINT('Ctrl Pts',(178.750345892354,583.99901570397,-48.9149415781133)) ;
#63619 = CARTESIAN_POINT('Ctrl Pts',(178.651772409613,584.068333547866,-48.9217452744036)) ;
#63620 = CARTESIAN_POINT('Ctrl Pts',(178.59888008603,584.109535480401,-48.9256249255071)) ;
#63621 = CARTESIAN_POINT('Ctrl Pts',(178.447004424898,584.240259080228,-48.9374369453836)) ;
#63622 = CARTESIAN_POINT('Ctrl Pts',(178.354630428038,584.336903872117,-48.9455694340703)) ;
#63623 = CARTESIAN_POINT('Ctrl Pts',(178.234368692083,584.490104303318,-48.957129339582)) ;
#63624 = CARTESIAN_POINT('Ctrl Pts',(178.198641097553,584.540073278791,-48.9607168460511)) ;
#63625 = CARTESIAN_POINT('Ctrl Pts',(178.148814213497,584.616809983714,-48.9658775253391)) ;
#63626 = CARTESIAN_POINT('Ctrl Pts',(178.132980879125,584.64240825046,-48.9675438884388)) ;
#63627 = CARTESIAN_POINT('Ctrl Pts',(178.099434896374,584.699405719882,-48.9711217962482)) ;
#63628 = CARTESIAN_POINT('Ctrl Pts',(178.081975211821,584.730940269057,-48.9730190562814)) ;
#63629 = CARTESIAN_POINT('Ctrl Pts',(178.044865471298,584.802335688029,-48.9771699064271)) ;
#63630 = CARTESIAN_POINT('Ctrl Pts',(178.025660463273,584.842407764215,-48.9794027107795)) ;
#63631 = CARTESIAN_POINT('Ctrl Pts',(177.962314334052,584.986383483853,-48.9871914348485)) ;
#63632 = CARTESIAN_POINT('Ctrl Pts',(177.925448305642,585.093266179804,-48.9925637057962)) ;
#63633 = CARTESIAN_POINT('Ctrl Pts',(177.873877502783,585.295414575354,-49.0027427539056)) ;
#63634 = CARTESIAN_POINT('Ctrl Pts',(177.856724572656,585.389724127318,-49.0074980246381)) ;
#63635 = CARTESIAN_POINT('Ctrl Pts',(177.840570104518,585.535912044658,-49.0151215943738)) ;
#63636 = CARTESIAN_POINT('Ctrl Pts',(177.836845866824,585.587134834643,-49.0178380996845)) ;
#63637 = CARTESIAN_POINT('Ctrl Pts',(177.833157123241,585.6921582474,-49.0235264691367)) ;
#63638 = CARTESIAN_POINT('Ctrl Pts',(177.833379065138,585.745925210263,-49.0265021679117)) ;
#63639 = CARTESIAN_POINT('Ctrl Pts',(177.838608917974,585.866481774079,-49.033327514973)) ;
#63640 = CARTESIAN_POINT('Ctrl Pts',(177.844774267554,585.933158046879,-49.0372090984667)) ;
#63641 = CARTESIAN_POINT('Ctrl Pts',(177.873441696996,586.13506393026,-49.0492495174707)) ;
#63642 = CARTESIAN_POINT('Ctrl Pts',(177.906220531692,586.268441399001,-49.0576232844682)) ;
#63643 = CARTESIAN_POINT('Ctrl Pts',(177.971353722208,586.452038896113,-49.0691718657179)) ;
#63644 = CARTESIAN_POINT('Ctrl Pts',(177.992972818926,586.505682845048,-49.0725442484097)) ;
#63645 = CARTESIAN_POINT('Ctrl Pts',(178.029191244183,586.585644459333,-49.0774950847042)) ;
#63646 = CARTESIAN_POINT('Ctrl Pts',(178.042151912039,586.612669753336,-49.0791537483355)) ;
#63647 = CARTESIAN_POINT('Ctrl Pts',(178.072414417961,586.672384959256,-49.0827751211145)) ;
#63648 = CARTESIAN_POINT('Ctrl Pts',(178.090015742585,586.704909103596,-49.0847210505373)) ;
#63649 = CARTESIAN_POINT('Ctrl Pts',(178.13146668355,586.776797264857,-49.0890010652727)) ;
#63650 = CARTESIAN_POINT('Ctrl Pts',(178.15578028774,586.815871072237,-49.0913127622947)) ;
#63651 = CARTESIAN_POINT('Ctrl Pts',(178.282026089867,587.004339213792,-49.1025487914152)) ;
#63652 = CARTESIAN_POINT('Ctrl Pts',(178.402054396407,587.140634833927,-49.111026667567)) ;
#63653 = CARTESIAN_POINT('Ctrl Pts',(178.570257765251,587.287254992632,-49.1224071453578)) ;
#63654 = CARTESIAN_POINT('Ctrl Pts',(178.602987478482,587.314052749122,-49.1245976179241)) ;
#63655 = CARTESIAN_POINT('Ctrl Pts',(178.636519276311,587.33982040643,-49.1268280924949)) ;
#63656 = CARTESIAN_POINT('Origin',(212.388527625421,616.21056516053,-47.0221601717612)) ;
#63657 = CARTESIAN_POINT('',(212.388527625421,616.71056516053,-47.0221601717612)) ;
#63658 = CARTESIAN_POINT('',(212.388527625421,616.21056516053,-47.5221601717612)) ;
#63659 = CARTESIAN_POINT('Origin',(212.388527625421,616.21056516053,-47.0221601717612)) ;
#63660 = CARTESIAN_POINT('',(205.668527625421,616.710565160531,-47.0221601717609)) ;
#63661 = CARTESIAN_POINT('',(212.388527625421,616.71056516053,-47.0221601717612)) ;
#63662 = CARTESIAN_POINT('',(205.668527625421,616.210565160531,-47.5221601717609)) ;
#63663 = CARTESIAN_POINT('Origin',(205.668527625421,616.210565160531,-47.0221601717609)) ;
#63664 = CARTESIAN_POINT('',(212.388527625421,616.21056516053,-47.5221601717612)) ;
#63665 = CARTESIAN_POINT('Origin',(-0.61147237455117,767.719724025967,-21.5221601717515)) ;
#63666 = CARTESIAN_POINT('',(-2.61147237459719,505.710565160568,-21.5221601717515)) ;
#63667 = CARTESIAN_POINT('',(-0.611472374577598,505.710565160568,-19.5221601717515)) ;
#63668 = CARTESIAN_POINT('Origin',(-0.611472374597194,505.710565160567,-21.5221601717515)) ;
#63669 = CARTESIAN_POINT('',(-2.61147237459754,503.710565160568,-21.5221601717515)) ;
#63670 = CARTESIAN_POINT('',(-2.6114723745971,506.210565160568,-21.5221601717515)) ;
#63671 = CARTESIAN_POINT('',(-0.611472374577924,503.710565160567,-19.5221601717515)) ;
#63672 = CARTESIAN_POINT('Origin',(-0.611472374597545,503.710565160567,-21.5221601717515)) ;
#63673 = CARTESIAN_POINT('',(-0.611472374577774,504.632344420872,-19.5221601717515)) ;
#63674 = CARTESIAN_POINT('Origin',(210.388527625449,767.719724025931,-21.5221601717611)) ;
#63675 = CARTESIAN_POINT('',(210.388527625403,505.71056516053,-19.5221601717611)) ;
#63676 = CARTESIAN_POINT('',(212.388527625403,505.71056516053,-21.5221601717612)) ;
#63677 = CARTESIAN_POINT('Origin',(210.388527625403,505.71056516053,-21.5221601717611)) ;
#63678 = CARTESIAN_POINT('',(210.388527625403,503.71056516053,-19.5221601717611)) ;
#63679 = CARTESIAN_POINT('',(210.388527625403,506.21056516053,-19.5221601717611)) ;
#63680 = CARTESIAN_POINT('',(212.388527625402,503.71056516053,-21.5221601717612)) ;
#63681 = CARTESIAN_POINT('Origin',(210.388527625403,503.71056516053,-21.5221601717611)) ;
#63682 = CARTESIAN_POINT('',(212.388527625422,616.21056516053,-21.5221601717612)) ;
#63683 = CARTESIAN_POINT('Origin',(210.388527625376,354.70143701573,-21.5221601717611)) ;
#63684 = CARTESIAN_POINT('',(212.388527625422,616.71056516053,-21.5221601717612)) ;
#63685 = CARTESIAN_POINT('',(210.388527625422,616.71056516053,-19.5221601717611)) ;
#63686 = CARTESIAN_POINT('Origin',(210.388527625422,616.71056516053,-21.5221601717611)) ;
#63687 = CARTESIAN_POINT('',(212.388527625423,618.71056516053,-21.5221601717612)) ;
#63688 = CARTESIAN_POINT('',(212.388527625422,616.21056516053,-21.5221601717612)) ;
#63689 = CARTESIAN_POINT('',(210.388527625423,618.71056516053,-19.5221601717611)) ;
#63690 = CARTESIAN_POINT('Origin',(210.388527625423,618.71056516053,-21.5221601717611)) ;
#63691 = CARTESIAN_POINT('',(210.388527625423,618.71056516053,-19.5221601717611)) ;
#63692 = CARTESIAN_POINT('Origin',(-0.611472374623716,354.701437015767,-21.5221601717516)) ;
#63693 = CARTESIAN_POINT('',(-0.611472374559485,616.710565160567,-19.5221601717515)) ;
#63694 = CARTESIAN_POINT('',(-2.6114723745777,616.710565160568,-21.5221601717514)) ;
#63695 = CARTESIAN_POINT('Origin',(-0.611472374577692,616.710565160567,-21.5221601717515)) ;
#63696 = CARTESIAN_POINT('',(-0.611472374559158,618.710565160567,-19.5221601717515)) ;
#63697 = CARTESIAN_POINT('',(-0.611472374577774,504.632344420872,-19.5221601717515)) ;
#63698 = CARTESIAN_POINT('',(-2.61147237457735,618.710565160568,-21.5221601717514)) ;
#63699 = CARTESIAN_POINT('Origin',(-0.611472374577341,618.710565160567,-21.5221601717515)) ;
#63700 = CARTESIAN_POINT('',(-2.61147237457735,618.710565160568,-21.5221601717514)) ;
#63701 = CARTESIAN_POINT('Origin',(212.388527625421,618.21056516053,-49.5221601717612)) ;
#63702 = CARTESIAN_POINT('',(212.388527625402,506.210565160531,-47.5221601717613)) ;
#63703 = CARTESIAN_POINT('',(212.388527625411,561.21056516053,-47.5221601717613)) ;
#63704 = CARTESIAN_POINT('',(212.388527625402,505.71056516053,-47.0221601717613)) ;
#63705 = CARTESIAN_POINT('Origin',(212.388527625402,506.21056516053,-47.0221601717613)) ;
#63706 = CARTESIAN_POINT('',(212.388527625403,505.71056516053,-24.5221601717612)) ;
#63707 = CARTESIAN_POINT('',(212.388527625401,503.71056516053,-47.5221601717613)) ;
#63708 = CARTESIAN_POINT('',(212.388527625402,503.71056516053,-24.5221601717612)) ;
#63709 = CARTESIAN_POINT('',(212.388527625402,505.71056516053,-49.5221601717612)) ;
#63710 = CARTESIAN_POINT('Origin',(212.388527625402,505.71056516053,-47.5221601717612)) ;
#63711 = CARTESIAN_POINT('',(212.388527625421,616.71056516053,-49.5221601717612)) ;
#63712 = CARTESIAN_POINT('',(212.388527625411,561.21056516053,-49.5221601717612)) ;
#63713 = CARTESIAN_POINT('',(212.388527625421,618.71056516053,-47.5221601717612)) ;
#63714 = CARTESIAN_POINT('Origin',(212.388527625421,616.71056516053,-47.5221601717612)) ;
#63715 = CARTESIAN_POINT('',(212.388527625421,618.71056516053,-49.5221601717612)) ;
#63716 = CARTESIAN_POINT('',(212.388527625421,616.71056516053,-49.5221601717612)) ;
#63717 = CARTESIAN_POINT('Origin',(-0.611472374624711,355.600165159967,-47.5221601717515)) ;
#63718 = CARTESIAN_POINT('',(-2.6114723745982,506.335123681177,-47.5221601717515)) ;
#63719 = CARTESIAN_POINT('',(-0.611472374598311,506.335123681177,-49.5221601717515)) ;
#63720 = CARTESIAN_POINT('Origin',(-0.611472374598233,506.335123681177,-47.5221601717515)) ;
#63721 = CARTESIAN_POINT('',(-2.61147237457892,616.077123681177,-47.5221601717515)) ;
#63722 = CARTESIAN_POINT('',(-2.61147237459866,503.710565160568,-47.5221601717515)) ;
#63723 = CARTESIAN_POINT('',(-0.611472374579034,616.077123681177,-49.5221601717515)) ;
#63724 = CARTESIAN_POINT('Origin',(-0.611472374578956,616.077123681177,-47.5221601717515)) ;
#63725 = CARTESIAN_POINT('',(-0.611472374598421,505.710565160567,-49.5221601717515)) ;
#63726 = CARTESIAN_POINT('Origin',(0.388527625421986,503.131344420871,-46.5221601717516)) ;
#63727 = CARTESIAN_POINT('',(-0.611472374577496,506.335123681177,-46.5221601717516)) ;
#63728 = CARTESIAN_POINT('',(0.388527629159234,506.335123681176,-47.5221601717516)) ;
#63729 = CARTESIAN_POINT('Origin',(0.388527625422509,506.335123681176,-46.5221601717516)) ;
#63730 = CARTESIAN_POINT('',(0.388527629276449,616.077123681176,-47.5221601717516)) ;
#63731 = CARTESIAN_POINT('',(0.388527625421941,503.131344420871,-47.5221601717516)) ;
#63732 = CARTESIAN_POINT('',(-0.611472374559588,616.077123681177,-46.5221601717516)) ;
#63733 = CARTESIAN_POINT('Origin',(0.388527625440417,616.077123681176,-46.5221601717516)) ;
#63734 = CARTESIAN_POINT('',(-0.611472374578019,503.131344420871,-46.5221601717516)) ;
#63735 = CARTESIAN_POINT('Origin',(212.388527625404,505.71056516053,0.477839828238782)) ;
#63736 = CARTESIAN_POINT('',(104.888527625403,505.710565160549,-19.5221601717563)) ;
#63737 = CARTESIAN_POINT('',(205.668527625402,505.710565160531,-47.022160171761)) ;
#63738 = CARTESIAN_POINT('',(212.388527625402,505.71056516053,-47.0221601717613)) ;
#63739 = CARTESIAN_POINT('',(205.668527625403,505.710565160531,-28.5221601717609)) ;
#63740 = CARTESIAN_POINT('',(205.668527625403,505.710565160531,-24.5221601717609)) ;
#63741 = CARTESIAN_POINT('',(201.668527625403,505.710565160532,-28.5221601717607)) ;
#63742 = CARTESIAN_POINT('Origin',(203.668527625403,505.710565160532,-28.5221601717608)) ;
#63743 = CARTESIAN_POINT('',(201.668527625402,505.710565160532,-47.0221601717608)) ;
#63744 = CARTESIAN_POINT('',(201.668527625403,505.710565160532,-24.5221601717607)) ;
#63745 = CARTESIAN_POINT('',(197.688527625402,505.710565160533,-47.0221601717606)) ;
#63746 = CARTESIAN_POINT('',(212.388527625402,505.71056516053,-47.0221601717613)) ;
#63747 = CARTESIAN_POINT('',(197.688527625403,505.710565160533,-28.5221601717605)) ;
#63748 = CARTESIAN_POINT('',(197.688527625403,505.710565160533,-24.5221601717606)) ;
#63749 = CARTESIAN_POINT('',(193.688527625403,505.710565160533,-28.5221601717604)) ;
#63750 = CARTESIAN_POINT('Origin',(195.688527625403,505.710565160533,-28.5221601717604)) ;
#63751 = CARTESIAN_POINT('',(193.688527625402,505.710565160533,-47.0221601717604)) ;
#63752 = CARTESIAN_POINT('',(193.688527625403,505.710565160533,-24.5221601717604)) ;
#63753 = CARTESIAN_POINT('',(0.388527634349991,505.710565160567,-47.0221601717516)) ;
#63754 = CARTESIAN_POINT('',(212.388527625402,505.71056516053,-47.0221601717613)) ;
#63755 = CARTESIAN_POINT('',(0.388527634349961,505.710565160567,-43.4900362557631)) ;
#63756 = CARTESIAN_POINT('',(0.388527634349982,505.710565160567,-24.0060982137622)) ;
#63757 = CARTESIAN_POINT('',(-2.61147237459819,505.710565160568,-43.4900362557631)) ;
#63758 = CARTESIAN_POINT('',(103.388527625413,505.710565160549,-43.4900362557631)) ;
#63759 = CARTESIAN_POINT('',(-2.6114723745962,505.710565160568,0.47783982824855)) ;
#63760 = CARTESIAN_POINT('',(174.388527625403,505.710565160537,-25.7721601717595)) ;
#63761 = CARTESIAN_POINT('',(171.638527625403,505.710565160537,-25.7721601717594)) ;
#63762 = CARTESIAN_POINT('',(156.063527625403,505.71056516054,-25.7721601717586)) ;
#63763 = CARTESIAN_POINT('',(171.638527625403,505.710565160537,-24.1221601717594)) ;
#63764 = CARTESIAN_POINT('',(171.638527625403,505.710565160537,-24.1221601717594)) ;
#63765 = CARTESIAN_POINT('',(87.7385276254027,505.710565160552,-24.1221601717556)) ;
#63766 = CARTESIAN_POINT('',(171.638527625403,505.710565160537,-24.1221601717594)) ;
#63767 = CARTESIAN_POINT('',(87.7385276254026,505.710565160552,-25.7721601717556)) ;
#63768 = CARTESIAN_POINT('',(87.7385276254026,505.710565160552,-25.7721601717556)) ;
#63769 = CARTESIAN_POINT('',(84.9885276254027,505.710565160552,-25.7721601717554)) ;
#63770 = CARTESIAN_POINT('',(156.063527625403,505.71056516054,-25.7721601717586)) ;
#63771 = CARTESIAN_POINT('',(84.9885276254021,505.710565160552,-38.1221601717554)) ;
#63772 = CARTESIAN_POINT('',(84.9885276254033,505.710565160552,-11.8221601717554)) ;
#63773 = CARTESIAN_POINT('',(89.9885276254019,505.710565358999,-43.122160465752)) ;
#63774 = CARTESIAN_POINT('Origin',(89.9885276254021,505.710565160552,-38.1221601717556)) ;
#63775 = CARTESIAN_POINT('',(169.388527625402,505.71056496209,-43.1221604706556)) ;
#63776 = CARTESIAN_POINT('',(158.688527625402,505.710565160539,-43.1221607671016)) ;
#63777 = CARTESIAN_POINT('',(174.388527625402,505.710565160537,-38.1221601717595)) ;
#63778 = CARTESIAN_POINT('Origin',(169.388527625402,505.710565160538,-38.1221601717593)) ;
#63779 = CARTESIAN_POINT('',(174.388527625402,505.710565160537,-37.2221601717595)) ;
#63780 = CARTESIAN_POINT('',(174.388527625403,505.710565160537,-20.8221601717595)) ;
#63781 = CARTESIAN_POINT('',(173.388527625402,505.710565160537,-37.2221601717594)) ;
#63782 = CARTESIAN_POINT('',(192.888527625402,505.710565160533,-37.2221601717603)) ;
#63783 = CARTESIAN_POINT('',(173.388527625402,505.710565160537,-30.2221601717594)) ;
#63784 = CARTESIAN_POINT('',(173.388527625403,505.710565160537,-14.8721601717594)) ;
#63785 = CARTESIAN_POINT('',(174.388527625402,505.710565160537,-30.2221601717595)) ;
#63786 = CARTESIAN_POINT('',(191.888527625402,505.710565160534,-30.2221601717603)) ;
#63787 = CARTESIAN_POINT('',(174.388527625403,505.710565160537,-20.8221601717595)) ;
#63788 = CARTESIAN_POINT('',(181.555483800253,505.711440212721,-36.9689456432537)) ;
#63789 = CARTESIAN_POINT('Ctrl Pts',(179.0652954453,505.710565160536,-38.9047876814238)) ;
#63790 = CARTESIAN_POINT('Ctrl Pts',(179.135329608435,505.710565160536,-38.9278865069327)) ;
#63791 = CARTESIAN_POINT('Ctrl Pts',(179.206482466064,505.710565160536,-38.9468076688786)) ;
#63792 = CARTESIAN_POINT('Ctrl Pts',(179.278413970453,505.710565160536,-38.9616687602152)) ;
#63793 = CARTESIAN_POINT('Ctrl Pts',(179.351549896252,505.710565160536,-38.9767786857272)) ;
#63794 = CARTESIAN_POINT('Ctrl Pts',(179.425491802793,505.710565160536,-38.9876912772755)) ;
#63795 = CARTESIAN_POINT('Ctrl Pts',(179.499885702151,505.710565160536,-38.9944761516692)) ;
#63796 = CARTESIAN_POINT('Ctrl Pts',(179.574328731058,505.710565160536,-39.0012655067774)) ;
#63797 = CARTESIAN_POINT('Ctrl Pts',(179.649225397864,505.710565160536,-39.003921398964)) ;
#63798 = CARTESIAN_POINT('Ctrl Pts',(179.724208634386,505.710565160536,-39.0024636129629)) ;
#63799 = CARTESIAN_POINT('Ctrl Pts',(179.740738841685,505.710565160536,-39.0021422410681)) ;
#63800 = CARTESIAN_POINT('Ctrl Pts',(179.757273173814,505.710565160536,-39.0016207653068)) ;
#63801 = CARTESIAN_POINT('Ctrl Pts',(179.77380753891,505.710565160536,-39.0008990928722)) ;
#63802 = CARTESIAN_POINT('Ctrl Pts',(179.789271528614,505.710565160536,-39.0002241389182)) ;
#63803 = CARTESIAN_POINT('Ctrl Pts',(179.804735546905,505.710565160536,-38.9993740682518)) ;
#63804 = CARTESIAN_POINT('Ctrl Pts',(179.8201961877,505.710565160536,-38.9983487214072)) ;
#63805 = CARTESIAN_POINT('Ctrl Pts',(179.834565840625,505.710565160536,-38.9973957286767)) ;
#63806 = CARTESIAN_POINT('Ctrl Pts',(179.848934755005,505.710565160536,-38.996291021292)) ;
#63807 = CARTESIAN_POINT('Ctrl Pts',(179.863277860849,505.710565160536,-38.9950366924248)) ;
#63808 = CARTESIAN_POINT('Ctrl Pts',(179.936253785416,505.710565160536,-38.988654824384)) ;
#63809 = CARTESIAN_POINT('Ctrl Pts',(180.008688241705,505.710565160536,-38.9783969957027)) ;
#63810 = CARTESIAN_POINT('Ctrl Pts',(180.080246709531,505.710565160536,-38.9643329201609)) ;
#63811 = CARTESIAN_POINT('Ctrl Pts',(180.150714553706,505.710565160536,-38.9504831953995)) ;
#63812 = CARTESIAN_POINT('Ctrl Pts',(180.2203338107,505.710565160536,-38.9329419325712)) ;
#63813 = CARTESIAN_POINT('Ctrl Pts',(180.288765667339,505.710565160536,-38.9117300713281)) ;
#63814 = CARTESIAN_POINT('Ctrl Pts',(180.346723590668,505.710565160536,-38.8937648211074)) ;
#63815 = CARTESIAN_POINT('Ctrl Pts',(180.403829740812,505.710565160536,-38.8731657442259)) ;
#63816 = CARTESIAN_POINT('Ctrl Pts',(180.459860091428,505.710565160536,-38.8499225511445)) ;
#63817 = CARTESIAN_POINT('Ctrl Pts',(180.48291298549,505.710565160536,-38.8403594686033)) ;
#63818 = CARTESIAN_POINT('Ctrl Pts',(180.505783535886,505.710565160536,-38.8303485561633)) ;
#63819 = CARTESIAN_POINT('Ctrl Pts',(180.528455065064,505.710565160536,-38.8198881408891)) ;
#63820 = CARTESIAN_POINT('Ctrl Pts',(180.539030130832,505.710565160536,-38.8150089120284)) ;
#63821 = CARTESIAN_POINT('Ctrl Pts',(180.549561885266,505.710565160536,-38.810031875954)) ;
#63822 = CARTESIAN_POINT('Ctrl Pts',(180.560048582672,505.710565160536,-38.8049568234658)) ;
#63823 = CARTESIAN_POINT('Ctrl Pts',(180.570864466054,505.710565160536,-38.7997224609455)) ;
#63824 = CARTESIAN_POINT('Ctrl Pts',(180.581624773649,505.710565160536,-38.794387503373)) ;
#63825 = CARTESIAN_POINT('Ctrl Pts',(180.592324290572,505.710565160536,-38.7889539836172)) ;
#63826 = CARTESIAN_POINT('Ctrl Pts',(180.65367541487,505.710565160536,-38.7577981334676)) ;
#63827 = CARTESIAN_POINT('Ctrl Pts',(180.713069228249,505.710565160536,-38.7233860504585)) ;
#63828 = CARTESIAN_POINT('Ctrl Pts',(180.77020178144,505.710565160536,-38.6857410806322)) ;
#63829 = CARTESIAN_POINT('Ctrl Pts',(180.822348458373,505.710565160536,-38.6513813335176)) ;
#63830 = CARTESIAN_POINT('Ctrl Pts',(180.872611488785,505.710565160536,-38.6143276859924)) ;
#63831 = CARTESIAN_POINT('Ctrl Pts',(180.92073330326,505.710565160536,-38.5745706438288)) ;
#63832 = CARTESIAN_POINT('Ctrl Pts',(180.97729284033,505.710565160536,-38.5278425658338)) ;
#63833 = CARTESIAN_POINT('Ctrl Pts',(181.030895815755,505.710565160536,-38.477379095277)) ;
#63834 = CARTESIAN_POINT('Ctrl Pts',(181.081338141313,505.710565160536,-38.4235564497692)) ;
#63835 = CARTESIAN_POINT('Ctrl Pts',(181.092527765842,505.710565160536,-38.4116169686347)) ;
#63836 = CARTESIAN_POINT('Ctrl Pts',(181.103561628948,505.710565160536,-38.399512111087)) ;
#63837 = CARTESIAN_POINT('Ctrl Pts',(181.114437100065,505.710565160536,-38.3872458806828)) ;
#63838 = CARTESIAN_POINT('Ctrl Pts',(181.125083675749,505.710565160536,-38.3752378169457)) ;
#63839 = CARTESIAN_POINT('Ctrl Pts',(181.135581757719,505.710565160536,-38.3630709576335)) ;
#63840 = CARTESIAN_POINT('Ctrl Pts',(181.145909005854,505.710565160536,-38.3507731755607)) ;
#63841 = CARTESIAN_POINT('Ctrl Pts',(181.190002102132,505.710565160536,-38.2982667109303)) ;
#63842 = CARTESIAN_POINT('Ctrl Pts',(181.231048772417,505.710565160536,-38.2433074480089)) ;
#63843 = CARTESIAN_POINT('Ctrl Pts',(181.268934008565,505.710565160536,-38.1862332430176)) ;
#63844 = CARTESIAN_POINT('Ctrl Pts',(181.306814639129,505.710565160536,-38.1291659763522)) ;
#63845 = CARTESIAN_POINT('Ctrl Pts',(181.341534914382,505.710565160536,-38.0699831659733)) ;
#63846 = CARTESIAN_POINT('Ctrl Pts',(181.372931677357,505.710565160536,-38.0090034068331)) ;
#63847 = CARTESIAN_POINT('Ctrl Pts',(181.395884966156,505.710565160536,-37.9644228230484)) ;
#63848 = CARTESIAN_POINT('Ctrl Pts',(181.417060969264,505.710565160535,-37.9188813736391)) ;
#63849 = CARTESIAN_POINT('Ctrl Pts',(181.436378199941,505.710565160536,-37.8725021900714)) ;
#63850 = CARTESIAN_POINT('Ctrl Pts',(181.444366168592,505.710565160536,-37.8533236923572)) ;
#63851 = CARTESIAN_POINT('Ctrl Pts',(181.452036113095,505.710565160536,-37.8340019566088)) ;
#63852 = CARTESIAN_POINT('Ctrl Pts',(181.459381478451,505.710565160536,-37.8145457892129)) ;
#63853 = CARTESIAN_POINT('Ctrl Pts',(181.464832557486,505.710565160536,-37.8001071464708)) ;
#63854 = CARTESIAN_POINT('Ctrl Pts',(181.470104871676,505.710565160536,-37.7855944696366)) ;
#63855 = CARTESIAN_POINT('Ctrl Pts',(181.475195571295,505.710565160535,-37.771011398043)) ;
#63856 = CARTESIAN_POINT('Ctrl Pts',(181.479480142813,505.710565160535,-37.7587376011455)) ;
#63857 = CARTESIAN_POINT('Ctrl Pts',(181.483633257897,505.710565160536,-37.746421893323)) ;
#63858 = CARTESIAN_POINT('Ctrl Pts',(181.487652624753,505.710565160536,-37.7340700270267)) ;
#63859 = CARTESIAN_POINT('Ctrl Pts',(181.508028361165,505.710565160536,-37.6714536048839)) ;
#63860 = CARTESIAN_POINT('Ctrl Pts',(181.524981102548,505.710565160535,-37.6078787529545)) ;
#63861 = CARTESIAN_POINT('Ctrl Pts',(181.538343022134,505.710565160536,-37.5436364340069)) ;
#63862 = CARTESIAN_POINT('Ctrl Pts',(181.547803658224,505.710565160536,-37.4981509633619)) ;
#63863 = CARTESIAN_POINT('Ctrl Pts',(181.555463195809,505.710565160536,-37.452330761803)) ;
#63864 = CARTESIAN_POINT('Ctrl Pts',(181.56124651201,505.710565160536,-37.4062815313059)) ;
#63865 = CARTESIAN_POINT('Ctrl Pts',(181.563093934278,505.710565160536,-37.3915715671793)) ;
#63866 = CARTESIAN_POINT('Ctrl Pts',(181.56475002009,505.710565160536,-37.3768360133949)) ;
#63867 = CARTESIAN_POINT('Ctrl Pts',(181.566211327952,505.710565160536,-37.3620856413917)) ;
#63868 = CARTESIAN_POINT('Ctrl Pts',(181.572427964596,505.710565160536,-37.2993352070323)) ;
#63869 = CARTESIAN_POINT('Ctrl Pts',(181.575112940977,505.710565160536,-37.2364324486792)) ;
#63870 = CARTESIAN_POINT('Ctrl Pts',(181.574097520804,505.710565160536,-37.1736438710465)) ;
#63871 = CARTESIAN_POINT('Ctrl Pts',(181.573151572664,505.710565160536,-37.1151511014797)) ;
#63872 = CARTESIAN_POINT('Ctrl Pts',(181.568993905684,505.710565160536,-37.0567569444679)) ;
#63873 = CARTESIAN_POINT('Ctrl Pts',(181.561449401405,505.710565160536,-36.9986897046275)) ;
#63874 = CARTESIAN_POINT('Ctrl Pts',(181.560161212776,505.710565160536,-36.9887749964758)) ;
#63875 = CARTESIAN_POINT('Ctrl Pts',(181.558774192941,505.710565160536,-36.9788698606881)) ;
#63876 = CARTESIAN_POINT('Ctrl Pts',(181.557288983751,505.710565160535,-36.9689754712777)) ;
#63877 = CARTESIAN_POINT('Ctrl Pts',(181.553679372624,505.711440212721,-36.969003246307)) ;
#63878 = CARTESIAN_POINT('Ctrl Pts',(181.553434896476,505.711148528659,-36.9613449801169)) ;
#63879 = CARTESIAN_POINT('Ctrl Pts',(181.553137587331,505.710856844597,-36.9536884005284)) ;
#63880 = CARTESIAN_POINT('Ctrl Pts',(181.552787473488,505.710565160536,-36.9460342363074)) ;
#63881 = CARTESIAN_POINT('Ctrl Pts',(179.569297170772,505.710565160536,-35.3870308445087)) ;
#63882 = CARTESIAN_POINT('Ctrl Pts',(179.505455887236,505.710565160536,-35.3919881983916)) ;
#63883 = CARTESIAN_POINT('Ctrl Pts',(179.442183898045,505.710565160536,-35.4009213613684)) ;
#63884 = CARTESIAN_POINT('Ctrl Pts',(179.379716462264,505.710565160536,-35.4135293431981)) ;
#63885 = CARTESIAN_POINT('Ctrl Pts',(179.317249026483,505.710565160536,-35.4261373250277)) ;
#63886 = CARTESIAN_POINT('Ctrl Pts',(179.255585363968,505.710565160536,-35.4424204680216)) ;
#63887 = CARTESIAN_POINT('Ctrl Pts',(179.194950373845,505.710565160536,-35.4621332783491)) ;
#63888 = CARTESIAN_POINT('Ctrl Pts',(179.140136352604,505.710565160536,-35.4799536556892)) ;
#63889 = CARTESIAN_POINT('Ctrl Pts',(179.086162428757,505.710565160536,-35.5005776890217)) ;
#63890 = CARTESIAN_POINT('Ctrl Pts',(179.033195548199,505.710565160536,-35.5238594749927)) ;
#63891 = CARTESIAN_POINT('Ctrl Pts',(179.006578591245,505.710565160536,-35.5355590557208)) ;
#63892 = CARTESIAN_POINT('Ctrl Pts',(178.980216000577,505.710565160536,-35.5479302990645)) ;
#63893 = CARTESIAN_POINT('Ctrl Pts',(178.954129652167,505.710565160536,-35.5609576253808)) ;
#63894 = CARTESIAN_POINT('Ctrl Pts',(178.942328077973,505.710565160536,-35.5668512428259)) ;
#63895 = CARTESIAN_POINT('Ctrl Pts',(178.930581721253,505.710565160536,-35.572880003767)) ;
#63896 = CARTESIAN_POINT('Ctrl Pts',(178.918911283598,505.710565160536,-35.579032359671)) ;
#63897 = CARTESIAN_POINT('Ctrl Pts',(178.859681619721,505.710565160536,-35.6102567218602)) ;
#63898 = CARTESIAN_POINT('Ctrl Pts',(178.802297253821,505.710565160536,-35.6447138932495)) ;
#63899 = CARTESIAN_POINT('Ctrl Pts',(178.74699869452,505.710565160536,-35.6821359841794)) ;
#63900 = CARTESIAN_POINT('Ctrl Pts',(178.690694275589,505.710565160536,-35.7202387686217)) ;
#63901 = CARTESIAN_POINT('Ctrl Pts',(178.636551275762,505.710565160536,-35.7614156281894)) ;
#63902 = CARTESIAN_POINT('Ctrl Pts',(178.584831529575,505.710565160536,-35.805436907624)) ;
#63903 = CARTESIAN_POINT('Ctrl Pts',(178.541450424535,505.710565160536,-35.84236074983)) ;
#63904 = CARTESIAN_POINT('Ctrl Pts',(178.499774013886,505.710565160536,-35.8812868352562)) ;
#63905 = CARTESIAN_POINT('Ctrl Pts',(178.459968650475,505.710565160536,-35.9221049529937)) ;
#63906 = CARTESIAN_POINT('Ctrl Pts',(178.441578208832,505.710565160536,-35.9409632963904)) ;
#63907 = CARTESIAN_POINT('Ctrl Pts',(178.423587340823,505.710565160536,-35.9602258002509)) ;
#63908 = CARTESIAN_POINT('Ctrl Pts',(178.406013633541,505.710565160536,-35.9798830591776)) ;
#63909 = CARTESIAN_POINT('Ctrl Pts',(178.398443666251,505.710565160536,-35.9883505273504)) ;
#63910 = CARTESIAN_POINT('Ctrl Pts',(178.390951571984,505.710565160536,-35.9968908681941)) ;
#63911 = CARTESIAN_POINT('Ctrl Pts',(178.383547395181,505.710565160536,-36.0054929611087)) ;
#63912 = CARTESIAN_POINT('Ctrl Pts',(178.33772699916,505.710565160536,-36.0587266040186)) ;
#63913 = CARTESIAN_POINT('Ctrl Pts',(178.295182788124,505.710565160536,-36.1144199624445)) ;
#63914 = CARTESIAN_POINT('Ctrl Pts',(178.25618213975,505.710565160536,-36.1723214142079)) ;
#63915 = CARTESIAN_POINT('Ctrl Pts',(178.221114088011,505.710565160536,-36.22438442318)) ;
#63916 = CARTESIAN_POINT('Ctrl Pts',(178.188910651079,505.710565160536,-36.2782336378472)) ;
#63917 = CARTESIAN_POINT('Ctrl Pts',(178.159784940565,505.710565160536,-36.3337168679626)) ;
#63918 = CARTESIAN_POINT('Ctrl Pts',(178.128216735146,505.710565160536,-36.393852946179)) ;
#63919 = CARTESIAN_POINT('Ctrl Pts',(178.10026275254,505.710565160536,-36.4559086037906)) ;
#63920 = CARTESIAN_POINT('Ctrl Pts',(178.075864414872,505.710565160536,-36.519565756551)) ;
#63921 = CARTESIAN_POINT('Ctrl Pts',(178.066551119335,505.710565160536,-36.5438648659713)) ;
#63922 = CARTESIAN_POINT('Ctrl Pts',(178.057756368665,505.710565160536,-36.5683976281922)) ;
#63923 = CARTESIAN_POINT('Ctrl Pts',(178.049478616365,505.710565160536,-36.5931473112284)) ;
#63924 = CARTESIAN_POINT('Ctrl Pts',(178.045832898525,505.710565160536,-36.6040476568441)) ;
#63925 = CARTESIAN_POINT('Ctrl Pts',(178.042287878707,505.710565160536,-36.6149891360053)) ;
#63926 = CARTESIAN_POINT('Ctrl Pts',(178.038847045237,505.710565160536,-36.6259579956453)) ;
#63927 = CARTESIAN_POINT('Ctrl Pts',(178.01790405103,505.710565160536,-36.6927211115773)) ;
#63928 = CARTESIAN_POINT('Ctrl Pts',(178.000777075959,505.710565160536,-36.7606143234727)) ;
#63929 = CARTESIAN_POINT('Ctrl Pts',(177.987357778769,505.710565160536,-36.8292734696092)) ;
#63930 = CARTESIAN_POINT('Ctrl Pts',(177.973630974354,505.710565160536,-36.8995059606954)) ;
#63931 = CARTESIAN_POINT('Ctrl Pts',(177.963783447185,505.710565160536,-36.9705407196561)) ;
#63932 = CARTESIAN_POINT('Ctrl Pts',(177.957745517187,505.710565160536,-37.0420198942905)) ;
#63933 = CARTESIAN_POINT('Ctrl Pts',(177.953182960546,505.710565160536,-37.0960330714913)) ;
#63934 = CARTESIAN_POINT('Ctrl Pts',(177.95079664825,505.710565160536,-37.1503007792799)) ;
#63935 = CARTESIAN_POINT('Ctrl Pts',(177.950574798142,505.710565160536,-37.2046756703304)) ;
#63936 = CARTESIAN_POINT('Ctrl Pts',(177.950437322557,505.710565160536,-37.2383705827585)) ;
#63937 = CARTESIAN_POINT('Ctrl Pts',(177.951131314102,505.710565160536,-37.2721067525419)) ;
#63938 = CARTESIAN_POINT('Ctrl Pts',(177.952657081778,505.710565160536,-37.3058495799569)) ;
#63939 = CARTESIAN_POINT('Ctrl Pts',(177.953240450954,505.710565160536,-37.3187509709948)) ;
#63940 = CARTESIAN_POINT('Ctrl Pts',(177.953945590571,505.710565160536,-37.3316556206205)) ;
#63941 = CARTESIAN_POINT('Ctrl Pts',(177.954772122753,505.710565160536,-37.3445541442168)) ;
#63942 = CARTESIAN_POINT('Ctrl Pts',(177.95967870594,505.710565160536,-37.4211242770651)) ;
#63943 = CARTESIAN_POINT('Ctrl Pts',(177.968845134531,505.710565160536,-37.4972918701055)) ;
#63944 = CARTESIAN_POINT('Ctrl Pts',(177.982203495705,505.710565160536,-37.5726433698151)) ;
#63945 = CARTESIAN_POINT('Ctrl Pts',(177.992222266586,505.710565160536,-37.6291569945974)) ;
#63946 = CARTESIAN_POINT('Ctrl Pts',(178.004600133923,505.710565160536,-37.6852122341676)) ;
#63947 = CARTESIAN_POINT('Ctrl Pts',(178.019329553784,505.710565160536,-37.7406380121571)) ;
#63948 = CARTESIAN_POINT('Ctrl Pts',(178.024555821147,505.710565160536,-37.7603040911526)) ;
#63949 = CARTESIAN_POINT('Ctrl Pts',(178.030078307587,505.710565160536,-37.7798909242228)) ;
#63950 = CARTESIAN_POINT('Ctrl Pts',(178.035897233864,505.710565160536,-37.7993908321457)) ;
#63951 = CARTESIAN_POINT('Ctrl Pts',(178.040304327293,505.710565160536,-37.8141595217615)) ;
#63952 = CARTESIAN_POINT('Ctrl Pts',(178.044880075823,505.710565160536,-37.8288734635663)) ;
#63953 = CARTESIAN_POINT('Ctrl Pts',(178.049621681044,505.710565160536,-37.8435217616764)) ;
#63954 = CARTESIAN_POINT('Ctrl Pts',(178.072814492169,505.710565160536,-37.9151715923815)) ;
#63955 = CARTESIAN_POINT('Ctrl Pts',(178.099987870132,505.710565160536,-37.9853065120389)) ;
#63956 = CARTESIAN_POINT('Ctrl Pts',(178.1311097997,505.710565160536,-38.053547573471)) ;
#63957 = CARTESIAN_POINT('Ctrl Pts',(178.156254670014,505.710565160536,-38.1086827358345)) ;
#63958 = CARTESIAN_POINT('Ctrl Pts',(178.18397801006,505.710565160536,-38.1625820233426)) ;
#63959 = CARTESIAN_POINT('Ctrl Pts',(178.214287553404,505.710565160536,-38.2150417422617)) ;
#63960 = CARTESIAN_POINT('Ctrl Pts',(178.220262521689,505.710565160536,-38.2253832097409)) ;
#63961 = CARTESIAN_POINT('Ctrl Pts',(178.226338061256,505.710565160578,-38.235668711766)) ;
#63962 = CARTESIAN_POINT('Ctrl Pts',(178.232512830637,505.710565160538,-38.2458977135592)) ;
#63963 = CARTESIAN_POINT('',(31.555447115217,505.711420702611,-36.9690600226526)) ;
#63964 = CARTESIAN_POINT('Ctrl Pts',(29.0652954452959,505.710565160562,-38.9047876814153)) ;
#63965 = CARTESIAN_POINT('Ctrl Pts',(29.1351327058573,505.710565160562,-38.9278215640738)) ;
#63966 = CARTESIAN_POINT('Ctrl Pts',(29.2060816765201,505.710565160562,-38.9467022836268)) ;
#63967 = CARTESIAN_POINT('Ctrl Pts',(29.2778052840572,505.710565160562,-38.9615463226794)) ;
#63968 = CARTESIAN_POINT('Ctrl Pts',(29.3511852087307,505.710565160562,-38.9767331559262)) ;
#63969 = CARTESIAN_POINT('Ctrl Pts',(29.4253770054866,505.710565160562,-38.987694611082)) ;
#63970 = CARTESIAN_POINT('Ctrl Pts',(29.5000231783554,505.710565160562,-38.9945008791182)) ;
#63971 = CARTESIAN_POINT('Ctrl Pts',(29.5628201759124,505.710565160562,-39.0002267345883)) ;
#63972 = CARTESIAN_POINT('Ctrl Pts',(29.6259391294217,505.710565160562,-39.0030108311892)) ;
#63973 = CARTESIAN_POINT('Ctrl Pts',(29.6891607397903,505.710565160562,-39.00286714337)) ;
#63974 = CARTESIAN_POINT('Ctrl Pts',(29.7173582483808,505.710565160562,-39.0028030570791)) ;
#63975 = CARTESIAN_POINT('Ctrl Pts',(29.7455760540432,505.710565160562,-39.0021562353623)) ;
#63976 = CARTESIAN_POINT('Ctrl Pts',(29.7737939403674,505.710565160562,-39.000926394963)) ;
#63977 = CARTESIAN_POINT('Ctrl Pts',(29.789259057995,505.710565160562,-39.0002523676379)) ;
#63978 = CARTESIAN_POINT('Ctrl Pts',(29.8047241901967,505.710565160562,-38.9994032025605)) ;
#63979 = CARTESIAN_POINT('Ctrl Pts',(29.8201859307895,505.710565160562,-38.9983787384855)) ;
#63980 = CARTESIAN_POINT('Ctrl Pts',(29.8345524038282,505.710565160562,-38.9974268446529)) ;
#63981 = CARTESIAN_POINT('Ctrl Pts',(29.8489181231788,505.710565160562,-38.9963233055562)) ;
#63982 = CARTESIAN_POINT('Ctrl Pts',(29.8632580326653,505.710565160562,-38.9950702105724)) ;
#63983 = CARTESIAN_POINT('Ctrl Pts',(29.9362310424626,505.710565160562,-38.9886934539679)) ;
#63984 = CARTESIAN_POINT('Ctrl Pts',(30.0086623333364,505.710565160562,-38.9784410223258)) ;
#63985 = CARTESIAN_POINT('Ctrl Pts',(30.0802175001885,505.710565160562,-38.9643824410455)) ;
#63986 = CARTESIAN_POINT('Ctrl Pts',(30.15068071892,505.710565160562,-38.950538396913)) ;
#63987 = CARTESIAN_POINT('Ctrl Pts',(30.2202952517954,505.710565160562,-38.9330030533077)) ;
#63988 = CARTESIAN_POINT('Ctrl Pts',(30.288722414559,505.710565160562,-38.9117971678137)) ;
#63989 = CARTESIAN_POINT('Ctrl Pts',(30.3466769629711,505.710565160562,-38.8938367926082)) ;
#63990 = CARTESIAN_POINT('Ctrl Pts',(30.40377974218,505.710565160562,-38.87324257691)) ;
#63991 = CARTESIAN_POINT('Ctrl Pts',(30.4598067999162,505.710565160562,-38.8500041179199)) ;
#63992 = CARTESIAN_POINT('Ctrl Pts',(30.4828591313975,505.710565160562,-38.8404426545591)) ;
#63993 = CARTESIAN_POINT('Ctrl Pts',(30.5057291199309,505.710565160562,-38.8304333089539)) ;
#63994 = CARTESIAN_POINT('Ctrl Pts',(30.52840009156,505.710565160562,-38.8199743998416)) ;
#63995 = CARTESIAN_POINT('Ctrl Pts',(30.5389784366907,505.710565160562,-38.8150942406631)) ;
#63996 = CARTESIAN_POINT('Ctrl Pts',(30.5495134424306,505.710565160562,-38.8101161955752)) ;
#63997 = CARTESIAN_POINT('Ctrl Pts',(30.5600033616957,505.710565160562,-38.8050400542981)) ;
#63998 = CARTESIAN_POINT('Ctrl Pts',(30.5708146480521,505.710565160562,-38.799808401361)) ;
#63999 = CARTESIAN_POINT('Ctrl Pts',(30.5815703870052,505.710565160562,-38.7944762261743)) ;
#64000 = CARTESIAN_POINT('Ctrl Pts',(30.5922653929186,505.710565160562,-38.7890455472562)) ;
#64001 = CARTESIAN_POINT('Ctrl Pts',(30.6536123337932,505.710565160562,-38.7578949764942)) ;
#64002 = CARTESIAN_POINT('Ctrl Pts',(30.7130021980142,505.710565160562,-38.7234879257198)) ;
#64003 = CARTESIAN_POINT('Ctrl Pts',(30.7701311541928,505.710565160562,-38.6858475731534)) ;
#64004 = CARTESIAN_POINT('Ctrl Pts',(30.8222745637724,505.710565160562,-38.6514920299774)) ;
#64005 = CARTESIAN_POINT('Ctrl Pts',(30.8725346189327,505.710565160562,-38.6144422392586)) ;
#64006 = CARTESIAN_POINT('Ctrl Pts',(30.9206538443866,505.710565160562,-38.5746885745686)) ;
#64007 = CARTESIAN_POINT('Ctrl Pts',(30.9747624901138,505.710565160562,-38.5299867544796)) ;
#64008 = CARTESIAN_POINT('Ctrl Pts',(31.0261650707763,505.710565160562,-38.4818651599855)) ;
#64009 = CARTESIAN_POINT('Ctrl Pts',(31.0746839447929,505.710565160562,-38.4306536883031)) ;
#64010 = CARTESIAN_POINT('Ctrl Pts',(31.0881297831313,505.710565160562,-38.4164616613184)) ;
#64011 = CARTESIAN_POINT('Ctrl Pts',(31.1013538653161,505.710565160562,-38.4020322344394)) ;
#64012 = CARTESIAN_POINT('Ctrl Pts',(31.1143517243842,505.710565160562,-38.3873722484095)) ;
#64013 = CARTESIAN_POINT('Ctrl Pts',(31.1249977190283,505.710565160562,-38.3753648761231)) ;
#64014 = CARTESIAN_POINT('Ctrl Pts',(31.1354952461008,505.710565160562,-38.3631986878532)) ;
#64015 = CARTESIAN_POINT('Ctrl Pts',(31.1458219666048,505.710565160562,-38.3509015553636)) ;
#64016 = CARTESIAN_POINT('Ctrl Pts',(31.1899669478989,505.710565160562,-38.2983333965264)) ;
#64017 = CARTESIAN_POINT('Ctrl Pts',(31.2310585244121,505.710565160562,-38.2433060254466)) ;
#64018 = CARTESIAN_POINT('Ctrl Pts',(31.2689811923208,505.710565160562,-38.1861585964737)) ;
#64019 = CARTESIAN_POINT('Ctrl Pts',(31.3068004310769,505.710565160562,-38.1291670296929)) ;
#64020 = CARTESIAN_POINT('Ctrl Pts',(31.3414683117142,505.710565160562,-38.0700658327551)) ;
#64021 = CARTESIAN_POINT('Ctrl Pts',(31.3728222915957,505.710565160562,-38.0091723393296)) ;
#64022 = CARTESIAN_POINT('Ctrl Pts',(31.3957833184136,505.710565160562,-37.9645790487536)) ;
#64023 = CARTESIAN_POINT('Ctrl Pts',(31.4169661685957,505.710565160562,-37.9190241163557)) ;
#64024 = CARTESIAN_POINT('Ctrl Pts',(31.4362892673506,505.710565160562,-37.8726308157318)) ;
#64025 = CARTESIAN_POINT('Ctrl Pts',(31.4442773849114,505.710565160562,-37.8534519488161)) ;
#64026 = CARTESIAN_POINT('Ctrl Pts',(31.4519474920606,505.710565160562,-37.8341298171632)) ;
#64027 = CARTESIAN_POINT('Ctrl Pts',(31.4592930323279,505.710565160562,-37.8146732297774)) ;
#64028 = CARTESIAN_POINT('Ctrl Pts',(31.4647427469936,505.710565160562,-37.8002382330635)) ;
#64029 = CARTESIAN_POINT('Ctrl Pts',(31.470013801544,505.710565160562,-37.7857292295818)) ;
#64030 = CARTESIAN_POINT('Ctrl Pts',(31.4751033480087,505.710565160562,-37.7711498567442)) ;
#64031 = CARTESIAN_POINT('Ctrl Pts',(31.4793889286833,505.710565160562,-37.7588735018837)) ;
#64032 = CARTESIAN_POINT('Ctrl Pts',(31.4835430111578,505.710565160562,-37.7465552026881)) ;
#64033 = CARTESIAN_POINT('Ctrl Pts',(31.4875632978035,505.710565160562,-37.7342007273561)) ;
#64034 = CARTESIAN_POINT('Ctrl Pts',(31.5079397140028,505.710565160562,-37.6715833188298)) ;
#64035 = CARTESIAN_POINT('Ctrl Pts',(31.5248932906129,505.710565160562,-37.6080072908746)) ;
#64036 = CARTESIAN_POINT('Ctrl Pts',(31.5382561567857,505.710565160562,-37.5437636875823)) ;
#64037 = CARTESIAN_POINT('Ctrl Pts',(31.5477173363443,505.710565160562,-37.4982779169113)) ;
#64038 = CARTESIAN_POINT('Ctrl Pts',(31.5553775214832,505.710565160562,-37.4524573699572)) ;
#64039 = CARTESIAN_POINT('Ctrl Pts',(31.5611615768446,505.710565160562,-37.4064077734896)) ;
#64040 = CARTESIAN_POINT('Ctrl Pts',(31.5643673337055,505.710565160562,-37.380885229082)) ;
#64041 = CARTESIAN_POINT('Ctrl Pts',(31.5669968524272,505.710565160562,-37.3552836260987)) ;
#64042 = CARTESIAN_POINT('Ctrl Pts',(31.569032642096,505.710565160562,-37.329672801237)) ;
#64043 = CARTESIAN_POINT('Ctrl Pts',(31.5740111853602,505.710565160562,-37.2670412820962)) ;
#64044 = CARTESIAN_POINT('Ctrl Pts',(31.5754510607237,505.710565160562,-37.2043032363127)) ;
#64045 = CARTESIAN_POINT('Ctrl Pts',(31.5731765569328,505.710565160562,-37.1417251266716)) ;
#64046 = CARTESIAN_POINT('Ctrl Pts',(31.5714400801884,505.710565160562,-37.0939496810844)) ;
#64047 = CARTESIAN_POINT('Ctrl Pts',(31.5675377050921,505.710565160562,-37.0462674954266)) ;
#64048 = CARTESIAN_POINT('Ctrl Pts',(31.5613718805554,505.710565160562,-36.9988040978121)) ;
#64049 = CARTESIAN_POINT('Ctrl Pts',(31.5600838674012,505.710565160562,-36.988889206445)) ;
#64050 = CARTESIAN_POINT('Ctrl Pts',(31.558697022611,505.710565160562,-36.9789838905892)) ;
#64051 = CARTESIAN_POINT('Ctrl Pts',(31.5572119880889,505.710565160562,-36.9690893241484)) ;
#64052 = CARTESIAN_POINT('Ctrl Pts',(31.5536829752598,505.711420702611,-36.9691162197847)) ;
#64053 = CARTESIAN_POINT('Ctrl Pts',(31.5534444962862,505.711135521928,-36.9616298895976)) ;
#64054 = CARTESIAN_POINT('Ctrl Pts',(31.553155530141,505.710850341245,-36.9541451676964)) ;
#64055 = CARTESIAN_POINT('Ctrl Pts',(31.5528161031074,505.710565160562,-36.9466627348581)) ;
#64056 = CARTESIAN_POINT('Ctrl Pts',(29.5692971707754,505.710565160562,-35.3870308445009)) ;
#64057 = CARTESIAN_POINT('Ctrl Pts',(29.5072625869895,505.710565160562,-35.3918479059347)) ;
#64058 = CARTESIAN_POINT('Ctrl Pts',(29.4457654429815,505.710565160562,-35.4004180593316)) ;
#64059 = CARTESIAN_POINT('Ctrl Pts',(29.3850217861476,505.710565160562,-35.4124646102939)) ;
#64060 = CARTESIAN_POINT('Ctrl Pts',(29.3220357794238,505.710565160562,-35.4249558592481)) ;
#64061 = CARTESIAN_POINT('Ctrl Pts',(29.2598592126282,505.710565160562,-35.4411849077502)) ;
#64062 = CARTESIAN_POINT('Ctrl Pts',(29.1987222577426,505.710565160562,-35.460899523258)) ;
#64063 = CARTESIAN_POINT('Ctrl Pts',(29.1426079052272,505.710565160562,-35.4789945181164)) ;
#64064 = CARTESIAN_POINT('Ctrl Pts',(29.0873687600192,505.710565160562,-35.5000267520628)) ;
#64065 = CARTESIAN_POINT('Ctrl Pts',(29.0331835132918,505.710565160562,-35.5238397755035)) ;
#64066 = CARTESIAN_POINT('Ctrl Pts',(29.0065636304015,505.710565160562,-35.5355385299346)) ;
#64067 = CARTESIAN_POINT('Ctrl Pts',(28.9801981719153,505.710565160562,-35.5479089719437)) ;
#64068 = CARTESIAN_POINT('Ctrl Pts',(28.9541090217123,505.710565160562,-35.5609355344341)) ;
#64069 = CARTESIAN_POINT('Ctrl Pts',(28.9423122115306,505.710565160562,-35.5668257947079)) ;
#64070 = CARTESIAN_POINT('Ctrl Pts',(28.9305705845767,505.710565160562,-35.572851063511)) ;
#64071 = CARTESIAN_POINT('Ctrl Pts',(28.9189048179306,505.710565160562,-35.5789998089842)) ;
#64072 = CARTESIAN_POINT('Ctrl Pts',(28.8596712661301,505.710565160562,-35.6102203917833)) ;
#64073 = CARTESIAN_POINT('Ctrl Pts',(28.8022832597293,505.710565160562,-35.6446737270167)) ;
#64074 = CARTESIAN_POINT('Ctrl Pts',(28.7469813608305,505.710565160562,-35.6820920937285)) ;
#64075 = CARTESIAN_POINT('Ctrl Pts',(28.6906751156464,505.710565160562,-35.7201900211489)) ;
#64076 = CARTESIAN_POINT('Ctrl Pts',(28.6365304804,505.710565160562,-35.7613619677535)) ;
#64077 = CARTESIAN_POINT('Ctrl Pts',(28.5848093271771,505.710565160562,-35.8053784761555)) ;
#64078 = CARTESIAN_POINT('Ctrl Pts',(28.541430437791,505.710565160562,-35.8422954265743)) ;
#64079 = CARTESIAN_POINT('Ctrl Pts',(28.4997561367543,505.710565160562,-35.8812144066662)) ;
#64080 = CARTESIAN_POINT('Ctrl Pts',(28.4599527622968,505.710565160562,-35.9220253479791)) ;
#64081 = CARTESIAN_POINT('Ctrl Pts',(28.4415595226414,505.710565160562,-35.9408841868178)) ;
#64082 = CARTESIAN_POINT('Ctrl Pts',(28.423565992348,505.710565160563,-35.9601473342408)) ;
#64083 = CARTESIAN_POINT('Ctrl Pts',(28.4059897676973,505.710565160563,-35.9798053930658)) ;
#64084 = CARTESIAN_POINT('Ctrl Pts',(28.3984223584326,505.710565160563,-35.9882691319765)) ;
#64085 = CARTESIAN_POINT('Ctrl Pts',(28.3909327876458,505.710565160563,-35.9968056872066)) ;
#64086 = CARTESIAN_POINT('Ctrl Pts',(28.3835310782131,505.710565160563,-36.0054039637556)) ;
#64087 = CARTESIAN_POINT('Ctrl Pts',(28.3377108760982,505.710565160563,-36.0586315016502)) ;
#64088 = CARTESIAN_POINT('Ctrl Pts',(28.2951669675323,505.710565160563,-36.1143190826752)) ;
#64089 = CARTESIAN_POINT('Ctrl Pts',(28.2561667463011,505.710565160563,-36.1722153095195)) ;
#64090 = CARTESIAN_POINT('Ctrl Pts',(28.2211039769088,505.710565160563,-36.2242663488837)) ;
#64091 = CARTESIAN_POINT('Ctrl Pts',(28.188905123424,505.710565160563,-36.2781035417552)) ;
#64092 = CARTESIAN_POINT('Ctrl Pts',(28.1597832202372,505.710565160563,-36.333574922188)) ;
#64093 = CARTESIAN_POINT('Ctrl Pts',(28.1282157438182,505.710565160563,-36.3937046287703)) ;
#64094 = CARTESIAN_POINT('Ctrl Pts',(28.1002623563384,505.710565160563,-36.4557545291069)) ;
#64095 = CARTESIAN_POINT('Ctrl Pts',(28.0758644739581,505.710565160563,-36.5194064672103)) ;
#64096 = CARTESIAN_POINT('Ctrl Pts',(28.0665506287128,505.710565160563,-36.5437054736492)) ;
#64097 = CARTESIAN_POINT('Ctrl Pts',(28.0577553884762,505.710565160563,-36.568238248327)) ;
#64098 = CARTESIAN_POINT('Ctrl Pts',(28.0494772059523,505.710565160563,-36.5929880516034)) ;
#64099 = CARTESIAN_POINT('Ctrl Pts',(28.0458314162721,505.710565160563,-36.6038880984567)) ;
#64100 = CARTESIAN_POINT('Ctrl Pts',(28.0422863296697,505.710565160563,-36.6148292970828)) ;
#64101 = CARTESIAN_POINT('Ctrl Pts',(28.0388454345643,505.710565160563,-36.6257978938512)) ;
#64102 = CARTESIAN_POINT('Ctrl Pts',(28.0180863229789,505.710565160563,-36.6919720483306)) ;
#64103 = CARTESIAN_POINT('Ctrl Pts',(28.0010766258327,505.710565160563,-36.7592571926018)) ;
#64104 = CARTESIAN_POINT('Ctrl Pts',(27.9877106391096,505.710565160563,-36.8272984172306)) ;
#64105 = CARTESIAN_POINT('Ctrl Pts',(27.9739059651428,505.710565160563,-36.8975728340585)) ;
#64106 = CARTESIAN_POINT('Ctrl Pts',(27.963987764797,505.710565160563,-36.9686545452015)) ;
#64107 = CARTESIAN_POINT('Ctrl Pts',(27.9578857860212,505.710565160563,-37.0401845046639)) ;
#64108 = CARTESIAN_POINT('Ctrl Pts',(27.9532312624418,505.710565160563,-37.0947467860456)) ;
#64109 = CARTESIAN_POINT('Ctrl Pts',(27.9507981351901,505.710565160563,-37.1495706606258)) ;
#64110 = CARTESIAN_POINT('Ctrl Pts',(27.9505741662839,505.710565160563,-37.2045041243709)) ;
#64111 = CARTESIAN_POINT('Ctrl Pts',(27.9504367813379,505.710565160563,-37.2382009043224)) ;
#64112 = CARTESIAN_POINT('Ctrl Pts',(27.951130965593,505.710565160563,-37.271939021478)) ;
#64113 = CARTESIAN_POINT('Ctrl Pts',(27.952657027207,505.710565160563,-37.3056838599239)) ;
#64114 = CARTESIAN_POINT('Ctrl Pts',(27.953240415664,505.710565160563,-37.3185839611059)) ;
#64115 = CARTESIAN_POINT('Ctrl Pts',(27.9539455506795,505.710565160563,-37.3314873315597)) ;
#64116 = CARTESIAN_POINT('Ctrl Pts',(27.954772053826,505.710565160563,-37.3443845802242)) ;
#64117 = CARTESIAN_POINT('Ctrl Pts',(27.959678903322,505.710565160563,-37.4209539900082)) ;
#64118 = CARTESIAN_POINT('Ctrl Pts',(27.9688455129901,505.710565160563,-37.4971211765398)) ;
#64119 = CARTESIAN_POINT('Ctrl Pts',(27.9822039608736,505.710565160563,-37.5724724789569)) ;
#64120 = CARTESIAN_POINT('Ctrl Pts',(27.9922227967861,505.710565160563,-37.6289859557697)) ;
#64121 = CARTESIAN_POINT('Ctrl Pts',(28.0046006760498,505.710565160562,-37.6850411652294)) ;
#64122 = CARTESIAN_POINT('Ctrl Pts',(28.0193300502471,505.710565160562,-37.7404669874564)) ;
#64123 = CARTESIAN_POINT('Ctrl Pts',(28.0245595644987,505.710565160562,-37.7601453609814)) ;
#64124 = CARTESIAN_POINT('Ctrl Pts',(28.030085660545,505.710565160563,-37.7797443989801)) ;
#64125 = CARTESIAN_POINT('Ctrl Pts',(28.0359085594318,505.710565160563,-37.799256405901)) ;
#64126 = CARTESIAN_POINT('Ctrl Pts',(28.040317895285,505.710565160563,-37.8140316910907)) ;
#64127 = CARTESIAN_POINT('Ctrl Pts',(28.0448960245853,505.710565160563,-37.8287521502641)) ;
#64128 = CARTESIAN_POINT('Ctrl Pts',(28.049640158209,505.710565160563,-37.8434069169089)) ;
#64129 = CARTESIAN_POINT('Ctrl Pts',(28.0728350792194,505.710565160563,-37.9150567020365)) ;
#64130 = CARTESIAN_POINT('Ctrl Pts',(28.100010513494,505.710565160562,-37.9851915354304)) ;
#64131 = CARTESIAN_POINT('Ctrl Pts',(28.1311344486129,505.710565160562,-38.0534323638883)) ;
#64132 = CARTESIAN_POINT('Ctrl Pts',(28.1562723623073,505.710565160562,-38.1085485325109)) ;
#64133 = CARTESIAN_POINT('Ctrl Pts',(28.1839869552626,505.710565160562,-38.1624295731364)) ;
#64134 = CARTESIAN_POINT('Ctrl Pts',(28.2142859508539,505.710565160562,-38.2148719443432)) ;
#64135 = CARTESIAN_POINT('Ctrl Pts',(28.2202649143704,505.710565160562,-38.2252205060049)) ;
#64136 = CARTESIAN_POINT('Ctrl Pts',(28.2263445836864,505.710565160562,-38.2355130233344)) ;
#64137 = CARTESIAN_POINT('Ctrl Pts',(28.2325236144401,505.710565160562,-38.2457489606755)) ;
#64138 = CARTESIAN_POINT('',(4.83852762540252,505.710565160566,-24.0221601717538)) ;
#64139 = CARTESIAN_POINT('Origin',(6.48852762540252,505.710565160566,-24.0221601717538)) ;
#64140 = CARTESIAN_POINT('',(36.3885276254024,505.710565160561,-30.2221601717532)) ;
#64141 = CARTESIAN_POINT('',(38.3885276254024,505.710565160561,-30.2221601717533)) ;
#64142 = CARTESIAN_POINT('',(124.388527625402,505.710565160546,-30.2221601717572)) ;
#64143 = CARTESIAN_POINT('',(36.3885276254021,505.710565160561,-37.2221601717532)) ;
#64144 = CARTESIAN_POINT('',(36.388527625403,505.710565160561,-18.3721601717532)) ;
#64145 = CARTESIAN_POINT('',(38.3885276254021,505.710565160561,-37.2221601717533)) ;
#64146 = CARTESIAN_POINT('',(125.388527625402,505.710565160545,-37.2221601717573)) ;
#64147 = CARTESIAN_POINT('',(38.3885276254031,505.710565160561,-14.8721601717533)) ;
#64148 = CARTESIAN_POINT('',(186.388527625402,505.710565160535,-30.22216017176)) ;
#64149 = CARTESIAN_POINT('',(188.388527625402,505.710565160534,-30.2221601717601)) ;
#64150 = CARTESIAN_POINT('',(199.388527625402,505.710565160532,-30.2221601717606)) ;
#64151 = CARTESIAN_POINT('',(186.388527625402,505.710565160535,-37.22216017176)) ;
#64152 = CARTESIAN_POINT('',(186.388527625403,505.710565160535,-18.37216017176)) ;
#64153 = CARTESIAN_POINT('',(188.388527625402,505.710565160534,-37.2221601717601)) ;
#64154 = CARTESIAN_POINT('',(200.388527625402,505.710565160532,-37.2221601717607)) ;
#64155 = CARTESIAN_POINT('',(188.388527625403,505.710565160534,-14.8721601717601)) ;
#64156 = CARTESIAN_POINT('',(21.3885276254024,505.710565160564,-30.2221601717525)) ;
#64157 = CARTESIAN_POINT('',(23.3885276254024,505.710565160563,-30.2221601717526)) ;
#64158 = CARTESIAN_POINT('',(116.888527625402,505.710565160547,-30.2221601717569)) ;
#64159 = CARTESIAN_POINT('',(21.3885276254021,505.710565160564,-37.2221601717525)) ;
#64160 = CARTESIAN_POINT('',(21.388527625403,505.710565160564,-18.3721601717525)) ;
#64161 = CARTESIAN_POINT('',(23.3885276254021,505.710565160563,-37.2221601717526)) ;
#64162 = CARTESIAN_POINT('',(117.888527625402,505.710565160547,-37.2221601717569)) ;
#64163 = CARTESIAN_POINT('',(23.3885276254031,505.710565160563,-14.8721601717526)) ;
#64164 = CARTESIAN_POINT('',(185.73826464091,505.710565160535,-24.0199774237433)) ;
#64165 = CARTESIAN_POINT('Origin',(187.388264603403,505.710565160534,-24.0203292412001)) ;
#64166 = CARTESIAN_POINT('Origin',(212.388527625421,616.21056516053,-47.0221601717612)) ;
#64167 = CARTESIAN_POINT('',(0.388527630194573,616.210565160567,-47.5221601717516)) ;
#64168 = CARTESIAN_POINT('',(0.388527634368074,616.710565160567,-47.0221601717516)) ;
#64169 = CARTESIAN_POINT('Origin',(0.388527634368039,616.210565160567,-47.0221601717516)) ;
#64170 = CARTESIAN_POINT('',(140.388527625421,616.210565160543,-47.5221601717579)) ;
#64171 = CARTESIAN_POINT('',(212.388527625421,616.21056516053,-47.5221601717612)) ;
#64172 = CARTESIAN_POINT('',(140.388527625421,616.710565160543,-47.022160171758)) ;
#64173 = CARTESIAN_POINT('Origin',(140.388527625421,616.210565160543,-47.022160171758)) ;
#64174 = CARTESIAN_POINT('',(212.388527625421,616.71056516053,-47.0221601717612)) ;
#64175 = CARTESIAN_POINT('Origin',(212.388527625421,616.71056516053,-49.5221601717612)) ;
#64176 = CARTESIAN_POINT('',(104.888527625422,616.710565160549,-19.5221601717563)) ;
#64177 = CARTESIAN_POINT('',(-2.6114723745787,616.710565160568,-43.4900362557631)) ;
#64178 = CARTESIAN_POINT('',(-2.61147237457784,616.710565160568,-24.5221601717514)) ;
#64179 = CARTESIAN_POINT('',(0.388527634368074,616.710565160567,-43.4900362557631)) ;
#64180 = CARTESIAN_POINT('',(103.388527625431,616.710565160549,-43.4900362557631)) ;
#64181 = CARTESIAN_POINT('',(0.388527634368081,616.710565160567,-49.0060982137622)) ;
#64182 = CARTESIAN_POINT('',(140.388527625422,616.710565160543,-28.5221601717579)) ;
#64183 = CARTESIAN_POINT('',(140.388527625421,616.710565160543,-49.5221601717579)) ;
#64184 = CARTESIAN_POINT('',(144.388527625422,616.710565160542,-28.5221601717581)) ;
#64185 = CARTESIAN_POINT('Origin',(142.388527625422,616.710565160542,-28.522160171758)) ;
#64186 = CARTESIAN_POINT('',(144.388527625421,616.710565160542,-47.0221601717582)) ;
#64187 = CARTESIAN_POINT('',(144.388527625422,616.710565160542,-38.0221601717581)) ;
#64188 = CARTESIAN_POINT('',(148.388527625421,616.710565160541,-47.0221601717583)) ;
#64189 = CARTESIAN_POINT('',(212.388527625421,616.71056516053,-47.0221601717612)) ;
#64190 = CARTESIAN_POINT('',(148.388527625422,616.710565160541,-28.5221601717583)) ;
#64191 = CARTESIAN_POINT('',(148.388527625421,616.710565160541,-49.5221601717583)) ;
#64192 = CARTESIAN_POINT('',(152.388527625422,616.71056516054,-28.5221601717585)) ;
#64193 = CARTESIAN_POINT('Origin',(150.388527625422,616.710565160541,-28.5221601717584)) ;
#64194 = CARTESIAN_POINT('',(152.388527625421,616.71056516054,-47.0221601717585)) ;
#64195 = CARTESIAN_POINT('',(152.388527625422,616.71056516054,-38.0221601717585)) ;
#64196 = CARTESIAN_POINT('',(193.688527625421,616.710565160533,-47.0221601717604)) ;
#64197 = CARTESIAN_POINT('',(212.388527625421,616.71056516053,-47.0221601717612)) ;
#64198 = CARTESIAN_POINT('',(193.688527625422,616.710565160533,-28.5221601717604)) ;
#64199 = CARTESIAN_POINT('',(193.688527625421,616.710565160533,-49.5221601717604)) ;
#64200 = CARTESIAN_POINT('',(197.688527625422,616.710565160532,-28.5221601717605)) ;
#64201 = CARTESIAN_POINT('Origin',(195.688527625422,616.710565160533,-28.5221601717604)) ;
#64202 = CARTESIAN_POINT('',(197.688527625421,616.710565160533,-47.0221601717606)) ;
#64203 = CARTESIAN_POINT('',(197.688527625421,616.710565160533,-49.5221601717605)) ;
#64204 = CARTESIAN_POINT('',(201.668527625421,616.710565160532,-47.0221601717608)) ;
#64205 = CARTESIAN_POINT('',(212.388527625421,616.71056516053,-47.0221601717612)) ;
#64206 = CARTESIAN_POINT('',(201.668527625422,616.710565160532,-28.5221601717607)) ;
#64207 = CARTESIAN_POINT('',(201.668527625421,616.710565160532,-49.5221601717607)) ;
#64208 = CARTESIAN_POINT('',(205.668527625422,616.710565160531,-28.5221601717609)) ;
#64209 = CARTESIAN_POINT('Origin',(203.668527625422,616.710565160532,-28.5221601717608)) ;
#64210 = CARTESIAN_POINT('',(205.668527625421,616.710565160531,-49.5221601717609)) ;
#64211 = CARTESIAN_POINT('',(4.83852762542202,616.710565160566,-24.0221601717537)) ;
#64212 = CARTESIAN_POINT('Origin',(6.48852762542202,616.710565160566,-24.0221601717538)) ;
#64213 = CARTESIAN_POINT('',(21.3885276254216,616.710565160564,-37.2221601717525)) ;
#64214 = CARTESIAN_POINT('',(23.3885276254216,616.710565160563,-37.2221601717526)) ;
#64215 = CARTESIAN_POINT('',(117.888527625422,616.710565160547,-37.2221601717569)) ;
#64216 = CARTESIAN_POINT('',(21.3885276254219,616.710565160564,-30.2221601717525)) ;
#64217 = CARTESIAN_POINT('',(21.3885276254213,616.710565160564,-43.3721601717525)) ;
#64218 = CARTESIAN_POINT('',(23.3885276254219,616.710565160563,-30.2221601717526)) ;
#64219 = CARTESIAN_POINT('',(116.888527625422,616.710565160547,-30.2221601717569)) ;
#64220 = CARTESIAN_POINT('',(23.3885276254215,616.710565160563,-39.8721601717526)) ;
#64221 = CARTESIAN_POINT('',(186.388527625422,616.710565160535,-37.22216017176)) ;
#64222 = CARTESIAN_POINT('',(188.388527625422,616.710565160534,-37.2221601717601)) ;
#64223 = CARTESIAN_POINT('',(200.388527625422,616.710565160532,-37.2221601717607)) ;
#64224 = CARTESIAN_POINT('',(186.388527625422,616.710565160535,-30.22216017176)) ;
#64225 = CARTESIAN_POINT('',(186.388527625421,616.710565160535,-43.37216017176)) ;
#64226 = CARTESIAN_POINT('',(188.388527625422,616.710565160534,-30.2221601717601)) ;
#64227 = CARTESIAN_POINT('',(199.388527625422,616.710565160532,-30.2221601717606)) ;
#64228 = CARTESIAN_POINT('',(188.388527625421,616.710565160534,-39.8721601717601)) ;
#64229 = CARTESIAN_POINT('',(171.388527625422,616.710565160537,-37.2221601717593)) ;
#64230 = CARTESIAN_POINT('',(173.388527625422,616.710565160537,-37.2221601717594)) ;
#64231 = CARTESIAN_POINT('',(192.888527625422,616.710565160533,-37.2221601717603)) ;
#64232 = CARTESIAN_POINT('',(171.388527625422,616.710565160537,-30.2221601717593)) ;
#64233 = CARTESIAN_POINT('',(171.388527625421,616.710565160537,-43.3721601717593)) ;
#64234 = CARTESIAN_POINT('',(173.388527625422,616.710565160537,-30.2221601717594)) ;
#64235 = CARTESIAN_POINT('',(191.888527625422,616.710565160534,-30.2221601717603)) ;
#64236 = CARTESIAN_POINT('',(173.388527625421,616.710565160537,-39.8721601717594)) ;
#64237 = CARTESIAN_POINT('',(36.3885276254216,616.710565160561,-37.2221601717532)) ;
#64238 = CARTESIAN_POINT('',(38.3885276254216,616.710565160561,-37.2221601717533)) ;
#64239 = CARTESIAN_POINT('',(125.388527625422,616.710565160545,-37.2221601717573)) ;
#64240 = CARTESIAN_POINT('',(36.3885276254219,616.710565160561,-30.2221601717532)) ;
#64241 = CARTESIAN_POINT('',(36.3885276254213,616.710565160561,-43.3721601717532)) ;
#64242 = CARTESIAN_POINT('',(38.3885276254219,616.710565160561,-30.2221601717533)) ;
#64243 = CARTESIAN_POINT('',(124.388527625422,616.710565160545,-30.2221601717572)) ;
#64244 = CARTESIAN_POINT('',(38.3885276254215,616.710565160561,-39.8721601717533)) ;
#64245 = CARTESIAN_POINT('',(187.382265311382,616.710565160534,-25.6703183346474)) ;
#64246 = CARTESIAN_POINT('Origin',(187.388264603422,616.710565160534,-24.0203292412001)) ;
#64247 = CARTESIAN_POINT('',(31.5554754095649,616.709694579094,-37.0753480170549)) ;
#64248 = CARTESIAN_POINT('Ctrl Pts',(29.0652954453167,616.710565160562,-35.1395326620899)) ;
#64249 = CARTESIAN_POINT('Ctrl Pts',(29.1351294046756,616.710565160562,-35.1164998682415)) ;
#64250 = CARTESIAN_POINT('Ctrl Pts',(29.2060755187498,616.710565160562,-35.097620673558)) ;
#64251 = CARTESIAN_POINT('Ctrl Pts',(29.2777966627579,616.710565160562,-35.0827784591697)) ;
#64252 = CARTESIAN_POINT('Ctrl Pts',(29.3511765960227,616.710565160562,-35.0675929693622)) ;
#64253 = CARTESIAN_POINT('Ctrl Pts',(29.4253688687927,616.710565160562,-35.0566334627366)) ;
#64254 = CARTESIAN_POINT('Ctrl Pts',(29.5000158983603,616.710565160562,-35.0498295941094)) ;
#64255 = CARTESIAN_POINT('Ctrl Pts',(29.5628148257399,616.710565160562,-35.0441056469638)) ;
#64256 = CARTESIAN_POINT('Ctrl Pts',(29.6259359910898,616.710565160562,-35.0413238912052)) ;
#64257 = CARTESIAN_POINT('Ctrl Pts',(29.6891600328717,616.710565160562,-35.0414702603465)) ;
#64258 = CARTESIAN_POINT('Ctrl Pts',(29.7173612583189,616.710565160562,-35.0415355486299)) ;
#64259 = CARTESIAN_POINT('Ctrl Pts',(29.7455828283297,616.710565160562,-35.0421837488871)) ;
#64260 = CARTESIAN_POINT('Ctrl Pts',(29.7738045152508,616.710565160562,-35.04341513634)) ;
#64261 = CARTESIAN_POINT('Ctrl Pts',(29.7892687576035,616.710565160562,-35.044089882469)) ;
#64262 = CARTESIAN_POINT('Ctrl Pts',(29.8047330254023,616.710565160562,-35.0449397499688)) ;
#64263 = CARTESIAN_POINT('Ctrl Pts',(29.8201939125384,616.710565160562,-35.0459648986994)) ;
#64264 = CARTESIAN_POINT('Ctrl Pts',(29.8345628533837,616.710565160562,-35.0469176448995)) ;
#64265 = CARTESIAN_POINT('Ctrl Pts',(29.8489310522879,616.710565160562,-35.0480220901629)) ;
#64266 = CARTESIAN_POINT('Ctrl Pts',(29.8632734423503,616.710565160562,-35.0492761421653)) ;
#64267 = CARTESIAN_POINT('Ctrl Pts',(29.9362514172939,616.710565160562,-35.0556570992591)) ;
#64268 = CARTESIAN_POINT('Ctrl Pts',(30.008687827618,616.710565160562,-35.0659142384965)) ;
#64269 = CARTESIAN_POINT('Ctrl Pts',(30.0802481411886,616.710565160562,-35.0799778810538)) ;
#64270 = CARTESIAN_POINT('Ctrl Pts',(30.1507148608536,616.710565160562,-35.0938266012187)) ;
#64271 = CARTESIAN_POINT('Ctrl Pts',(30.220332959107,616.710565160562,-35.1113668001717)) ;
#64272 = CARTESIAN_POINT('Ctrl Pts',(30.2887636507385,616.710565160562,-35.1325775802419)) ;
#64273 = CARTESIAN_POINT('Ctrl Pts',(30.346718206272,616.710565160562,-35.1505411767244)) ;
#64274 = CARTESIAN_POINT('Ctrl Pts',(30.4038210539397,616.710565160562,-35.1711383711428)) ;
#64275 = CARTESIAN_POINT('Ctrl Pts',(30.4598482127828,616.710565160562,-35.1943794772149)) ;
#64276 = CARTESIAN_POINT('Ctrl Pts',(30.4829009790285,616.710565160562,-35.2039421928092)) ;
#64277 = CARTESIAN_POINT('Ctrl Pts',(30.5057714016489,616.710565160562,-35.2139527496974)) ;
#64278 = CARTESIAN_POINT('Ctrl Pts',(30.5284428038845,616.710565160562,-35.224412822659)) ;
#64279 = CARTESIAN_POINT('Ctrl Pts',(30.5390186169923,616.710565160562,-35.229292263974)) ;
#64280 = CARTESIAN_POINT('Ctrl Pts',(30.5495511123406,616.710565160562,-35.234269530304)) ;
#64281 = CARTESIAN_POINT('Ctrl Pts',(30.5600385439176,616.710565160562,-35.2393448310897)) ;
#64282 = CARTESIAN_POINT('Ctrl Pts',(30.5708533815617,616.710565160562,-35.244578577178)) ;
#64283 = CARTESIAN_POINT('Ctrl Pts',(30.5816126498371,616.710565160562,-35.2499129016229)) ;
#64284 = CARTESIAN_POINT('Ctrl Pts',(30.5923111405141,616.710565160562,-35.2553457748175)) ;
#64285 = CARTESIAN_POINT('Ctrl Pts',(30.6536613282617,616.710565160562,-35.2865004302325)) ;
#64286 = CARTESIAN_POINT('Ctrl Pts',(30.7130542560941,616.710565160562,-35.3209113718768)) ;
#64287 = CARTESIAN_POINT('Ctrl Pts',(30.770186000803,616.710565160562,-35.3585552909014)) ;
#64288 = CARTESIAN_POINT('Ctrl Pts',(30.8223319344572,616.710565160562,-35.3929140753906)) ;
#64289 = CARTESIAN_POINT('Ctrl Pts',(30.8725942861496,616.710565160562,-35.4299668351395)) ;
#64290 = CARTESIAN_POINT('Ctrl Pts',(30.9207155073971,616.710565160562,-35.4697230936572)) ;
#64291 = CARTESIAN_POINT('Ctrl Pts',(30.977274484471,616.710565160562,-35.5164503639917)) ;
#64292 = CARTESIAN_POINT('Ctrl Pts',(31.0308770037112,616.710565160562,-35.5669131889342)) ;
#64293 = CARTESIAN_POINT('Ctrl Pts',(31.0813189646559,616.710565160562,-35.6207353285878)) ;
#64294 = CARTESIAN_POINT('Ctrl Pts',(31.0925085957903,616.710565160562,-35.6326747908592)) ;
#64295 = CARTESIAN_POINT('Ctrl Pts',(31.1035424675763,616.710565160562,-35.6447796390117)) ;
#64296 = CARTESIAN_POINT('Ctrl Pts',(31.1144179492562,616.710565160562,-35.6570458691578)) ;
#64297 = CARTESIAN_POINT('Ctrl Pts',(31.125064388927,616.710565160562,-35.6690537675742)) ;
#64298 = CARTESIAN_POINT('Ctrl Pts',(31.1355623407383,616.710565160562,-35.6812204659215)) ;
#64299 = CARTESIAN_POINT('Ctrl Pts',(31.1458894648435,616.710565160562,-35.6935180916591)) ;
#64300 = CARTESIAN_POINT('Ctrl Pts',(31.1898516741418,616.710565160562,-35.7458686580936)) ;
#64301 = CARTESIAN_POINT('Ctrl Pts',(31.2307855322649,616.710565160562,-35.8006576376647)) ;
#64302 = CARTESIAN_POINT('Ctrl Pts',(31.268577106942,616.710565160562,-35.8575501098362)) ;
#64303 = CARTESIAN_POINT('Ctrl Pts',(31.3064239741415,616.710565160562,-35.9145258208863)) ;
#64304 = CARTESIAN_POINT('Ctrl Pts',(31.3411196762928,616.710565160562,-35.9736122848845)) ;
#64305 = CARTESIAN_POINT('Ctrl Pts',(31.3725019056337,616.710565160562,-36.0344921687448)) ;
#64306 = CARTESIAN_POINT('Ctrl Pts',(31.3956129454238,616.710565160562,-36.0793263773992)) ;
#64307 = CARTESIAN_POINT('Ctrl Pts',(31.4169259867845,616.710565160562,-36.1251336930938)) ;
#64308 = CARTESIAN_POINT('Ctrl Pts',(31.4363581232945,616.710565160562,-36.1717887688914)) ;
#64309 = CARTESIAN_POINT('Ctrl Pts',(31.4443461212685,616.710565160562,-36.1909673420122)) ;
#64310 = CARTESIAN_POINT('Ctrl Pts',(31.4520160980142,616.710565160562,-36.2102891591937)) ;
#64311 = CARTESIAN_POINT('Ctrl Pts',(31.4593614982079,616.710565160562,-36.2297454134763)) ;
#64312 = CARTESIAN_POINT('Ctrl Pts',(31.4648122432911,616.710565160562,-36.2441831676588)) ;
#64313 = CARTESIAN_POINT('Ctrl Pts',(31.4700842485553,616.710565160562,-36.2586949491632)) ;
#64314 = CARTESIAN_POINT('Ctrl Pts',(31.4751746647096,616.710565160562,-36.2732771191433)) ;
#64315 = CARTESIAN_POINT('Ctrl Pts',(31.4794594741956,616.710565160562,-36.2855515223281)) ;
#64316 = CARTESIAN_POINT('Ctrl Pts',(31.4836128170683,616.710565160562,-36.297867844351)) ;
#64317 = CARTESIAN_POINT('Ctrl Pts',(31.4876324001455,616.710565160562,-36.3102203290086)) ;
#64318 = CARTESIAN_POINT('Ctrl Pts',(31.5080082748776,616.710565160562,-36.3728369425173)) ;
#64319 = CARTESIAN_POINT('Ctrl Pts',(31.524961188787,616.710565160562,-36.4364120290553)) ;
#64320 = CARTESIAN_POINT('Ctrl Pts',(31.5383233055122,616.710565160562,-36.5006546081721)) ;
#64321 = CARTESIAN_POINT('Ctrl Pts',(31.5477840532232,616.710565160562,-36.5461401286044)) ;
#64322 = CARTESIAN_POINT('Ctrl Pts',(31.5554437254137,616.710565160562,-36.5919603907947)) ;
#64323 = CARTESIAN_POINT('Ctrl Pts',(31.561227196496,616.710565160562,-36.6380096873979)) ;
#64324 = CARTESIAN_POINT('Ctrl Pts',(31.5630746651284,616.710565160562,-36.6527196478715)) ;
#64325 = CARTESIAN_POINT('Ctrl Pts',(31.5647307999987,616.710565160562,-36.6674551981726)) ;
#64326 = CARTESIAN_POINT('Ctrl Pts',(31.5661921596199,616.710565160562,-36.6822055678034)) ;
#64327 = CARTESIAN_POINT('Ctrl Pts',(31.5724090354787,616.710565160562,-36.7449561841024)) ;
#64328 = CARTESIAN_POINT('Ctrl Pts',(31.5750942763573,616.710565160562,-36.8078591320246)) ;
#64329 = CARTESIAN_POINT('Ctrl Pts',(31.574079138145,616.710565160562,-36.8706478918813)) ;
#64330 = CARTESIAN_POINT('Ctrl Pts',(31.5731334449241,616.710565160562,-36.9291413106388)) ;
#64331 = CARTESIAN_POINT('Ctrl Pts',(31.5689759954375,616.710565160562,-36.9875361088946)) ;
#64332 = CARTESIAN_POINT('Ctrl Pts',(31.5614316605456,616.710565160562,-37.0456039639648)) ;
#64333 = CARTESIAN_POINT('Ctrl Pts',(31.5601435095963,616.710565160562,-37.0555187097575)) ;
#64334 = CARTESIAN_POINT('Ctrl Pts',(31.5587565273789,616.710565160562,-37.0654238825553)) ;
#64335 = CARTESIAN_POINT('Ctrl Pts',(31.5572713557558,616.710565160562,-37.0753183083685)) ;
#64336 = CARTESIAN_POINT('Ctrl Pts',(31.5536802139309,616.709694579094,-37.0752907371637)) ;
#64337 = CARTESIAN_POINT('Ctrl Pts',(31.5534371170828,616.709984772917,-37.0829095784596)) ;
#64338 = CARTESIAN_POINT('Ctrl Pts',(31.5531417298432,616.710274966739,-37.0905267513044)) ;
#64339 = CARTESIAN_POINT('Ctrl Pts',(31.5527940800387,616.710565160562,-37.0981415381289)) ;
#64340 = CARTESIAN_POINT('Ctrl Pts',(29.5692971707939,616.710565160562,-38.6572894990043)) ;
#64341 = CARTESIAN_POINT('Ctrl Pts',(29.5054553546424,616.710565160562,-38.6523321037633)) ;
#64342 = CARTESIAN_POINT('Ctrl Pts',(29.4421828366268,616.710565160562,-38.6433990979037)) ;
#64343 = CARTESIAN_POINT('Ctrl Pts',(29.3797148829646,616.710565160562,-38.6307914294923)) ;
#64344 = CARTESIAN_POINT('Ctrl Pts',(29.3172469293023,616.710565160562,-38.6181837610809)) ;
#64345 = CARTESIAN_POINT('Ctrl Pts',(29.2555827598154,616.710565160562,-38.601901087878)) ;
#64346 = CARTESIAN_POINT('Ctrl Pts',(29.1949472804358,616.710565160562,-38.5821888640866)) ;
#64347 = CARTESIAN_POINT('Ctrl Pts',(29.1329194349116,616.710565160562,-38.5620239905707)) ;
#64348 = CARTESIAN_POINT('Ctrl Pts',(29.071967191479,616.710565160562,-38.5382700716443)) ;
#64349 = CARTESIAN_POINT('Ctrl Pts',(29.0123330057214,616.710565160562,-38.5111354809055)) ;
#64350 = CARTESIAN_POINT('Ctrl Pts',(28.9927857260204,616.710565160562,-38.5022411289829)) ;
#64351 = CARTESIAN_POINT('Ctrl Pts',(28.9733801346285,616.710565160562,-38.4929831301336)) ;
#64352 = CARTESIAN_POINT('Ctrl Pts',(28.9541250633592,616.710565160562,-38.4833676492202)) ;
#64353 = CARTESIAN_POINT('Ctrl Pts',(28.9423245452005,616.710565160562,-38.4774747779067)) ;
#64354 = CARTESIAN_POINT('Ctrl Pts',(28.9305792368964,616.710565160562,-38.4714467930994)) ;
#64355 = CARTESIAN_POINT('Ctrl Pts',(28.9189098346057,616.710565160562,-38.4652952396331)) ;
#64356 = CARTESIAN_POINT('Ctrl Pts',(28.8596160434162,616.710565160562,-38.4340383750884)) ;
#64357 = CARTESIAN_POINT('Ctrl Pts',(28.8021715482124,616.710565160562,-38.3995418155636)) ;
#64358 = CARTESIAN_POINT('Ctrl Pts',(28.7468176421506,616.710565160562,-38.3620742445524)) ;
#64359 = CARTESIAN_POINT('Ctrl Pts',(28.6903533001159,616.710565160562,-38.3238550492814)) ;
#64360 = CARTESIAN_POINT('Ctrl Pts',(28.6360632941515,616.710565160562,-38.2825441451409)) ;
#64361 = CARTESIAN_POINT('Ctrl Pts',(28.5842118032974,616.710565160562,-38.2383730315202)) ;
#64362 = CARTESIAN_POINT('Ctrl Pts',(28.5410521825941,616.710565160562,-38.2016063257127)) ;
#64363 = CARTESIAN_POINT('Ctrl Pts',(28.4995819204966,616.710565160562,-38.162856848819)) ;
#64364 = CARTESIAN_POINT('Ctrl Pts',(28.4599650517436,616.710565160562,-38.1222331755884)) ;
#64365 = CARTESIAN_POINT('Ctrl Pts',(28.4415739837682,616.710565160562,-38.1033747256578)) ;
#64366 = CARTESIAN_POINT('Ctrl Pts',(28.4235825196302,616.710565160562,-38.084112082613)) ;
#64367 = CARTESIAN_POINT('Ctrl Pts',(28.4060082484722,616.710565160562,-38.0644546500545)) ;
#64368 = CARTESIAN_POINT('Ctrl Pts',(28.3984388547211,616.710565160562,-38.0559880202961)) ;
#64369 = CARTESIAN_POINT('Ctrl Pts',(28.3909473261853,616.710565160562,-38.0474485305842)) ;
#64370 = CARTESIAN_POINT('Ctrl Pts',(28.3835437024959,616.710565160562,-38.0388472958062)) ;
#64371 = CARTESIAN_POINT('Ctrl Pts',(28.3377233367417,616.710565160562,-37.9856150219903)) ;
#64372 = CARTESIAN_POINT('Ctrl Pts',(28.2951791805688,616.710565160562,-37.9299229619158)) ;
#64373 = CARTESIAN_POINT('Ctrl Pts',(28.2561786153644,616.710565160562,-37.872022688255)) ;
#64374 = CARTESIAN_POINT('Ctrl Pts',(28.2211117359888,616.710565160562,-37.8199623680613)) ;
#64375 = CARTESIAN_POINT('Ctrl Pts',(28.1889093151112,616.710565160562,-37.7661158567172)) ;
#64376 = CARTESIAN_POINT('Ctrl Pts',(28.1597844471134,616.710565160562,-37.710635294839)) ;
#64377 = CARTESIAN_POINT('Ctrl Pts',(28.1281437015729,616.710565160562,-37.6503621859286)) ;
#64378 = CARTESIAN_POINT('Ctrl Pts',(28.1001337962876,616.710565160562,-37.5881605235266)) ;
#64379 = CARTESIAN_POINT('Ctrl Pts',(28.0756957976418,616.710565160562,-37.5243505776644)) ;
#64380 = CARTESIAN_POINT('Ctrl Pts',(28.0664447763215,616.710565160562,-37.5001952784449)) ;
#64381 = CARTESIAN_POINT('Ctrl Pts',(28.0577060649063,616.710565160562,-37.4758092124162)) ;
#64382 = CARTESIAN_POINT('Ctrl Pts',(28.0494781473923,616.710565160562,-37.4512088109423)) ;
#64383 = CARTESIAN_POINT('Ctrl Pts',(28.0458324122321,616.710565160562,-37.4403085377617)) ;
#64384 = CARTESIAN_POINT('Ctrl Pts',(28.0422873762234,616.710565160562,-37.4293671270742)) ;
#64385 = CARTESIAN_POINT('Ctrl Pts',(28.0388465277051,616.710565160562,-37.418398332039)) ;
#64386 = CARTESIAN_POINT('Ctrl Pts',(28.018086867898,616.710565160562,-37.3522203377988)) ;
#64387 = CARTESIAN_POINT('Ctrl Pts',(28.001076777631,616.710565160562,-37.2849317662674)) ;
#64388 = CARTESIAN_POINT('Ctrl Pts',(27.987710553931,616.710565160562,-37.2168874703652)) ;
#64389 = CARTESIAN_POINT('Ctrl Pts',(27.9739057996822,616.710565160562,-37.1466107187521)) ;
#64390 = CARTESIAN_POINT('Ctrl Pts',(27.9639875930527,616.710565160562,-37.0755270717528)) ;
#64391 = CARTESIAN_POINT('Ctrl Pts',(27.9578856891573,616.710565160562,-37.0039955050982)) ;
#64392 = CARTESIAN_POINT('Ctrl Pts',(27.9532315299756,616.710565160562,-36.9494355999537)) ;
#64393 = CARTESIAN_POINT('Ctrl Pts',(27.9507985212582,616.710565160562,-36.894614327456)) ;
#64394 = CARTESIAN_POINT('Ctrl Pts',(27.950574430833,616.710565160562,-36.8396836324218)) ;
#64395 = CARTESIAN_POINT('Ctrl Pts',(27.9504369704838,616.710565160562,-36.8059883394654)) ;
#64396 = CARTESIAN_POINT('Ctrl Pts',(27.9511309993669,616.710565160562,-36.7722517715414)) ;
#64397 = CARTESIAN_POINT('Ctrl Pts',(27.9526568263021,616.710565160562,-36.7385085318701)) ;
#64398 = CARTESIAN_POINT('Ctrl Pts',(27.9532401980609,616.710565160562,-36.7256074271509)) ;
#64399 = CARTESIAN_POINT('Ctrl Pts',(27.9539453351246,616.710565160562,-36.7127030614827)) ;
#64400 = CARTESIAN_POINT('Ctrl Pts',(27.9547718594983,616.710565160562,-36.6998048208729)) ;
#64401 = CARTESIAN_POINT('Ctrl Pts',(27.9595493423161,616.710565160562,-36.6252503069937)) ;
#64402 = CARTESIAN_POINT('Ctrl Pts',(27.96836558868,616.710565160562,-36.5510772905987)) ;
#64403 = CARTESIAN_POINT('Ctrl Pts',(27.9811572181665,616.710565160562,-36.4776677315349)) ;
#64404 = CARTESIAN_POINT('Ctrl Pts',(27.9913560767737,616.710565160562,-36.4191377597205)) ;
#64405 = CARTESIAN_POINT('Ctrl Pts',(28.0040830323133,616.710565160563,-36.3610924409845)) ;
#64406 = CARTESIAN_POINT('Ctrl Pts',(28.0193293617847,616.710565160563,-36.3037215267236)) ;
#64407 = CARTESIAN_POINT('Ctrl Pts',(28.0245563318108,616.710565160563,-36.2840527894203)) ;
#64408 = CARTESIAN_POINT('Ctrl Pts',(28.0300795996869,616.710565160562,-36.2644633173544)) ;
#64409 = CARTESIAN_POINT('Ctrl Pts',(28.0358993862355,616.710565160562,-36.244960793289)) ;
#64410 = CARTESIAN_POINT('Ctrl Pts',(28.0403069622081,616.710565160562,-36.2301906886194)) ;
#64411 = CARTESIAN_POINT('Ctrl Pts',(28.0448832231379,616.710565160563,-36.2154753485809)) ;
#64412 = CARTESIAN_POINT('Ctrl Pts',(28.049625372632,616.710565160563,-36.2008256626758)) ;
#64413 = CARTESIAN_POINT('Ctrl Pts',(28.0728186318987,616.710565160563,-36.1291758836473)) ;
#64414 = CARTESIAN_POINT('Ctrl Pts',(28.0999924465964,616.710565160563,-36.0590410222514)) ;
#64415 = CARTESIAN_POINT('Ctrl Pts',(28.1311148021221,616.710565160563,-35.9908000485429)) ;
#64416 = CARTESIAN_POINT('Ctrl Pts',(28.1562581569131,616.710565160563,-35.9356690347023)) ;
#64417 = CARTESIAN_POINT('Ctrl Pts',(28.1839795933006,616.710565160563,-35.8817737322274)) ;
#64418 = CARTESIAN_POINT('Ctrl Pts',(28.2142868426508,616.710565160563,-35.8293178017528)) ;
#64419 = CARTESIAN_POINT('Ctrl Pts',(28.2202628586927,616.710565160563,-35.8189744849317)) ;
#64420 = CARTESIAN_POINT('Ctrl Pts',(28.2263394813903,616.710565160563,-35.8086871540485)) ;
#64421 = CARTESIAN_POINT('Ctrl Pts',(28.2325153683705,616.710565160563,-35.7984563440547)) ;
#64422 = CARTESIAN_POINT('',(181.555506994667,616.709677724475,-37.0754500573667)) ;
#64423 = CARTESIAN_POINT('Ctrl Pts',(179.065295445318,616.710565160536,-35.1395326620961)) ;
#64424 = CARTESIAN_POINT('Ctrl Pts',(179.135760309488,616.710565160536,-35.1162917818011)) ;
#64425 = CARTESIAN_POINT('Ctrl Pts',(179.207358091158,616.710565160536,-35.097280708745)) ;
#64426 = CARTESIAN_POINT('Ctrl Pts',(179.279742381724,616.710565160536,-35.082379713154)) ;
#64427 = CARTESIAN_POINT('Ctrl Pts',(179.35212667229,616.710565160536,-35.067478717563)) ;
#64428 = CARTESIAN_POINT('Ctrl Pts',(179.42529849312,616.710565160536,-35.05668810083)) ;
#64429 = CARTESIAN_POINT('Ctrl Pts',(179.49891473763,616.710565160536,-35.0499403314768)) ;
#64430 = CARTESIAN_POINT('Ctrl Pts',(179.573357338759,616.710565160536,-35.0431168171042)) ;
#64431 = CARTESIAN_POINT('Ctrl Pts',(179.648255450353,616.710565160536,-35.0404276243099)) ;
#64432 = CARTESIAN_POINT('Ctrl Pts',(179.723241986661,616.710565160536,-35.0418526440978)) ;
#64433 = CARTESIAN_POINT('Ctrl Pts',(179.740096938686,616.710565160536,-35.0421729501333)) ;
#64434 = CARTESIAN_POINT('Ctrl Pts',(179.756956273047,616.710565160536,-35.0427013079803)) ;
#64435 = CARTESIAN_POINT('Ctrl Pts',(179.773815652038,616.710565160536,-35.0434378135935)) ;
#64436 = CARTESIAN_POINT('Ctrl Pts',(179.789278957467,616.710565160536,-35.0441133314317)) ;
#64437 = CARTESIAN_POINT('Ctrl Pts',(179.804742299989,616.710565160536,-35.0449639535352)) ;
#64438 = CARTESIAN_POINT('Ctrl Pts',(179.820202273595,616.710565160536,-35.0459898383144)) ;
#64439 = CARTESIAN_POINT('Ctrl Pts',(179.83457385404,616.710565160536,-35.046943500074)) ;
#64440 = CARTESIAN_POINT('Ctrl Pts',(179.848944705152,616.710565160536,-35.0480489188537)) ;
#64441 = CARTESIAN_POINT('Ctrl Pts',(179.863289748568,616.710565160536,-35.0493039991915)) ;
#64442 = CARTESIAN_POINT('Ctrl Pts',(179.936267392455,616.710565160536,-35.0556889785383)) ;
#64443 = CARTESIAN_POINT('Ctrl Pts',(180.008703721566,616.710565160536,-35.0659500945493)) ;
#64444 = CARTESIAN_POINT('Ctrl Pts',(180.080264148198,616.710565160536,-35.0800175215934)) ;
#64445 = CARTESIAN_POINT('Ctrl Pts',(180.151287993452,616.710565160536,-35.0939794668824)) ;
#64446 = CARTESIAN_POINT('Ctrl Pts',(180.221449976707,616.710565160536,-35.1116912348591)) ;
#64447 = CARTESIAN_POINT('Ctrl Pts',(180.290403053554,616.710565160536,-35.1331314491422)) ;
#64448 = CARTESIAN_POINT('Ctrl Pts',(180.347810086237,616.710565160536,-35.1509815457351)) ;
#64449 = CARTESIAN_POINT('Ctrl Pts',(180.404379083585,616.710565160536,-35.1714168999107)) ;
#64450 = CARTESIAN_POINT('Ctrl Pts',(180.459892061383,616.710565160536,-35.1944475435978)) ;
#64451 = CARTESIAN_POINT('Ctrl Pts',(180.482945306168,616.710565160536,-35.2040116327092)) ;
#64452 = CARTESIAN_POINT('Ctrl Pts',(180.505816207519,616.710565160536,-35.2140235218046)) ;
#64453 = CARTESIAN_POINT('Ctrl Pts',(180.528488085772,616.710565160536,-35.2244848788825)) ;
#64454 = CARTESIAN_POINT('Ctrl Pts',(180.539061091979,616.710565160536,-35.229363521582)) ;
#64455 = CARTESIAN_POINT('Ctrl Pts',(180.549590804644,616.710565160536,-35.2343399228102)) ;
#64456 = CARTESIAN_POINT('Ctrl Pts',(180.560075478962,616.710565160536,-35.2394142911207)) ;
#64457 = CARTESIAN_POINT('Ctrl Pts',(180.570894238498,616.710565160536,-35.2446503498554)) ;
#64458 = CARTESIAN_POINT('Ctrl Pts',(180.581657404697,616.710565160536,-35.2499870499363)) ;
#64459 = CARTESIAN_POINT('Ctrl Pts',(180.59235974437,616.710565160536,-35.2554223495306)) ;
#64460 = CARTESIAN_POINT('Ctrl Pts',(180.653713401841,616.710565160536,-35.2865814717173)) ;
#64461 = CARTESIAN_POINT('Ctrl Pts',(180.713109614463,616.710565160536,-35.3209966878714)) ;
#64462 = CARTESIAN_POINT('Ctrl Pts',(180.770244363422,616.710565160536,-35.358644552309)) ;
#64463 = CARTESIAN_POINT('Ctrl Pts',(180.822393082669,616.710565160536,-35.3930069665766)) ;
#64464 = CARTESIAN_POINT('Ctrl Pts',(180.872657983207,616.710565160536,-35.4300630865994)) ;
#64465 = CARTESIAN_POINT('Ctrl Pts',(180.920781439408,616.710565160535,-35.4698223282051)) ;
#64466 = CARTESIAN_POINT('Ctrl Pts',(180.977342516551,616.710565160535,-35.5165526694802)) ;
#64467 = CARTESIAN_POINT('Ctrl Pts',(181.030946757108,616.710565160536,-35.5670179744961)) ;
#64468 = CARTESIAN_POINT('Ctrl Pts',(181.081390104837,616.710565160535,-35.6208420838424)) ;
#64469 = CARTESIAN_POINT('Ctrl Pts',(181.092579707588,616.710565160535,-35.6327816245176)) ;
#64470 = CARTESIAN_POINT('Ctrl Pts',(181.103613543871,616.710565160535,-35.6448865160113)) ;
#64471 = CARTESIAN_POINT('Ctrl Pts',(181.114488983632,616.710565160535,-35.6571527556512)) ;
#64472 = CARTESIAN_POINT('Ctrl Pts',(181.125135943949,616.710565160535,-35.6691612968745)) ;
#64473 = CARTESIAN_POINT('Ctrl Pts',(181.135634394718,616.710565160535,-35.6813286224832)) ;
#64474 = CARTESIAN_POINT('Ctrl Pts',(181.145961995009,616.710565160535,-35.6936268588133)) ;
#64475 = CARTESIAN_POINT('Ctrl Pts',(181.190055697178,616.710565160536,-35.7461341939821)) ;
#64476 = CARTESIAN_POINT('Ctrl Pts',(181.23110279425,616.710565160536,-35.8010940082152)) ;
#64477 = CARTESIAN_POINT('Ctrl Pts',(181.268988309028,616.710565160536,-35.8581685016228)) ;
#64478 = CARTESIAN_POINT('Ctrl Pts',(181.306869165289,616.710565160535,-35.9152359769777)) ;
#64479 = CARTESIAN_POINT('Ctrl Pts',(181.341589526853,616.710565160535,-35.9744187271591)) ;
#64480 = CARTESIAN_POINT('Ctrl Pts',(181.372986267054,616.710565160536,-36.0353982117686)) ;
#64481 = CARTESIAN_POINT('Ctrl Pts',(181.39593969148,616.710565160536,-36.0799788906067)) ;
#64482 = CARTESIAN_POINT('Ctrl Pts',(181.41711574832,616.710565160536,-36.12552033319)) ;
#64483 = CARTESIAN_POINT('Ctrl Pts',(181.436432961007,616.710565160536,-36.1718994265542)) ;
#64484 = CARTESIAN_POINT('Ctrl Pts',(181.444420861294,616.710565160536,-36.1910777406913)) ;
#64485 = CARTESIAN_POINT('Ctrl Pts',(181.452090730016,616.710565160535,-36.21039927642)) ;
#64486 = CARTESIAN_POINT('Ctrl Pts',(181.459436013036,616.710565160535,-36.2298552288666)) ;
#64487 = CARTESIAN_POINT('Ctrl Pts',(181.464888066979,616.710565160535,-36.2442964562457)) ;
#64488 = CARTESIAN_POINT('Ctrl Pts',(181.470161284513,616.710565160535,-36.2588117376376)) ;
#64489 = CARTESIAN_POINT('Ctrl Pts',(181.475252814629,616.710565160535,-36.2733974322528)) ;
#64490 = CARTESIAN_POINT('Ctrl Pts',(181.479536714035,616.710565160535,-36.2856695090322)) ;
#64491 = CARTESIAN_POINT('Ctrl Pts',(181.483689186601,616.710565160535,-36.2979834742669)) ;
#64492 = CARTESIAN_POINT('Ctrl Pts',(181.487707944483,616.710565160535,-36.3103335862059)) ;
#64493 = CARTESIAN_POINT('Ctrl Pts',(181.508083347335,616.710565160536,-36.3729495768764)) ;
#64494 = CARTESIAN_POINT('Ctrl Pts',(181.525035664371,616.710565160536,-36.4365238783295)) ;
#64495 = CARTESIAN_POINT('Ctrl Pts',(181.538397094034,616.710565160536,-36.5007655742198)) ;
#64496 = CARTESIAN_POINT('Ctrl Pts',(181.547857457299,616.710565160535,-36.5462509597779)) ;
#64497 = CARTESIAN_POINT('Ctrl Pts',(181.555516660982,616.710565160535,-36.5920710450797)) ;
#64498 = CARTESIAN_POINT('Ctrl Pts',(181.56129958931,616.710565160536,-36.6381201422034)) ;
#64499 = CARTESIAN_POINT('Ctrl Pts',(181.563146895243,616.710565160536,-36.6528301239732)) ;
#64500 = CARTESIAN_POINT('Ctrl Pts',(181.564802857695,616.710565160536,-36.6675656946417)) ;
#64501 = CARTESIAN_POINT('Ctrl Pts',(181.566264035161,616.710565160536,-36.6823160803653)) ;
#64502 = CARTESIAN_POINT('Ctrl Pts',(181.572480068538,616.710565160535,-36.7450660830706)) ;
#64503 = CARTESIAN_POINT('Ctrl Pts',(181.575164374536,616.710565160536,-36.807968384507)) ;
#64504 = CARTESIAN_POINT('Ctrl Pts',(181.574148237453,616.710565160536,-36.8707565192832)) ;
#64505 = CARTESIAN_POINT('Ctrl Pts',(181.573201640889,616.710565160536,-36.9292476752771)) ;
#64506 = CARTESIAN_POINT('Ctrl Pts',(181.569043416825,616.710565160536,-36.9876402348526)) ;
#64507 = CARTESIAN_POINT('Ctrl Pts',(181.56149847437,616.710565160536,-37.0457059401061)) ;
#64508 = CARTESIAN_POINT('Ctrl Pts',(181.56021018879,616.710565160535,-37.0556205565811)) ;
#64509 = CARTESIAN_POINT('Ctrl Pts',(181.558823072082,616.710565160535,-37.065525602202)) ;
#64510 = CARTESIAN_POINT('Ctrl Pts',(181.557337766069,616.710565160536,-37.0754199028953)) ;
#64511 = CARTESIAN_POINT('Ctrl Pts',(181.553676994016,616.709677724475,-37.0753915560276)) ;
#64512 = CARTESIAN_POINT('Ctrl Pts',(181.553428681374,616.709973536495,-37.0831591097797)) ;
#64513 = CARTESIAN_POINT('Ctrl Pts',(181.553126016963,616.710269348516,-37.0909249260131)) ;
#64514 = CARTESIAN_POINT('Ctrl Pts',(181.55276903042,616.710565160536,-37.0986882443158)) ;
#64515 = CARTESIAN_POINT('Ctrl Pts',(179.569297170793,616.710565160536,-38.6572894990112)) ;
#64516 = CARTESIAN_POINT('Ctrl Pts',(179.507575048679,616.710565160536,-38.652496700609)) ;
#64517 = CARTESIAN_POINT('Ctrl Pts',(179.446384992941,616.710565160536,-38.6439866958335)) ;
#64518 = CARTESIAN_POINT('Ctrl Pts',(179.385939827787,616.710565160536,-38.6320324698614)) ;
#64519 = CARTESIAN_POINT('Ctrl Pts',(179.321346845425,616.710565160536,-38.6192579310643)) ;
#64520 = CARTESIAN_POINT('Ctrl Pts',(179.257603783352,616.710565160536,-38.6025505502925)) ;
#64521 = CARTESIAN_POINT('Ctrl Pts',(179.194958758116,616.710565160536,-38.5821821676965)) ;
#64522 = CARTESIAN_POINT('Ctrl Pts',(179.132933456879,616.710565160536,-38.5620152819549)) ;
#64523 = CARTESIAN_POINT('Ctrl Pts',(179.071983667288,616.710565160536,-38.5382589733736)) ;
#64524 = CARTESIAN_POINT('Ctrl Pts',(179.012351808975,616.710565160536,-38.5111217596247)) ;
#64525 = CARTESIAN_POINT('Ctrl Pts',(178.99280394022,616.710565160536,-38.5022259326666)) ;
#64526 = CARTESIAN_POINT('Ctrl Pts',(178.97339776577,616.710565160536,-38.4929663833965)) ;
#64527 = CARTESIAN_POINT('Ctrl Pts',(178.954142117937,616.710565160536,-38.4833492830115)) ;
#64528 = CARTESIAN_POINT('Ctrl Pts',(178.942337688862,616.710565160536,-38.4774536423981)) ;
#64529 = CARTESIAN_POINT('Ctrl Pts',(178.930588497952,616.710565160536,-38.4714227769235)) ;
#64530 = CARTESIAN_POINT('Ctrl Pts',(178.918915261483,616.710565160536,-38.4652682451263)) ;
#64531 = CARTESIAN_POINT('Ctrl Pts',(178.859687972246,616.710565160536,-38.4340415809661)) ;
#64532 = CARTESIAN_POINT('Ctrl Pts',(178.802305834108,616.710565160536,-38.3995820670162)) ;
#64533 = CARTESIAN_POINT('Ctrl Pts',(178.747009323128,616.710565160536,-38.3621576925695)) ;
#64534 = CARTESIAN_POINT('Ctrl Pts',(178.690706061567,616.710565160536,-38.3240519548677)) ;
#64535 = CARTESIAN_POINT('Ctrl Pts',(178.6365641045,616.710565160536,-38.2828721018293)) ;
#64536 = CARTESIAN_POINT('Ctrl Pts',(178.58484526323,616.710565160536,-38.2388479055619)) ;
#64537 = CARTESIAN_POINT('Ctrl Pts',(178.541462842338,616.710565160536,-38.2019198506213)) ;
#64538 = CARTESIAN_POINT('Ctrl Pts',(178.499785181819,616.710565160536,-38.1629894148874)) ;
#64539 = CARTESIAN_POINT('Ctrl Pts',(178.459978643299,616.710565160536,-38.1221668939241)) ;
#64540 = CARTESIAN_POINT('Ctrl Pts',(178.441589914141,616.710565160536,-38.1033088291572)) ;
#64541 = CARTESIAN_POINT('Ctrl Pts',(178.4236006766,616.710565160536,-38.0840466916977)) ;
#64542 = CARTESIAN_POINT('Ctrl Pts',(178.406028512192,616.710565160536,-38.0643898917392)) ;
#64543 = CARTESIAN_POINT('Ctrl Pts',(178.398456975362,616.710565160536,-38.0559201220854)) ;
#64544 = CARTESIAN_POINT('Ctrl Pts',(178.390963333105,616.710565160536,-38.0473774447142)) ;
#64545 = CARTESIAN_POINT('Ctrl Pts',(178.383557642961,616.710565160536,-38.0387729957834)) ;
#64546 = CARTESIAN_POINT('Ctrl Pts',(178.337737205006,616.710565160536,-37.9855356052508)) ;
#64547 = CARTESIAN_POINT('Ctrl Pts',(178.295192883898,616.710565160536,-37.9298386851746)) ;
#64548 = CARTESIAN_POINT('Ctrl Pts',(178.256192046795,616.710565160536,-37.8719339906431)) ;
#64549 = CARTESIAN_POINT('Ctrl Pts',(178.221120823221,616.710565160536,-37.8198636086029)) ;
#64550 = CARTESIAN_POINT('Ctrl Pts',(178.188914641014,616.710565160536,-37.7660069730285)) ;
#64551 = CARTESIAN_POINT('Ctrl Pts',(178.159786658629,616.710565160536,-37.7105164081319)) ;
#64552 = CARTESIAN_POINT('Ctrl Pts',(178.128218081803,616.710565160536,-37.6503763634864)) ;
#64553 = CARTESIAN_POINT('Ctrl Pts',(178.100263805153,616.710565160536,-37.5883170941831)) ;
#64554 = CARTESIAN_POINT('Ctrl Pts',(178.075865254137,616.710565160536,-37.5246566438292)) ;
#64555 = CARTESIAN_POINT('Ctrl Pts',(178.066552311063,616.710565160536,-37.5003574077897)) ;
#64556 = CARTESIAN_POINT('Ctrl Pts',(178.057757876326,616.710565160536,-37.4758245865156)) ;
#64557 = CARTESIAN_POINT('Ctrl Pts',(178.049480403893,616.710565160536,-37.4510749075307)) ;
#64558 = CARTESIAN_POINT('Ctrl Pts',(178.045834737263,616.710565160536,-37.4401743482714)) ;
#64559 = CARTESIAN_POINT('Ctrl Pts',(178.042289765575,616.710565160536,-37.4292326659532)) ;
#64560 = CARTESIAN_POINT('Ctrl Pts',(178.038848977129,616.710565160536,-37.4182636134829)) ;
#64561 = CARTESIAN_POINT('Ctrl Pts',(178.017905664152,616.710565160536,-37.3514974339986)) ;
#64562 = CARTESIAN_POINT('Ctrl Pts',(178.00077847231,616.710565160536,-37.2836014755171)) ;
#64563 = CARTESIAN_POINT('Ctrl Pts',(177.987359061536,616.710565160536,-37.2149398559529)) ;
#64564 = CARTESIAN_POINT('Ctrl Pts',(177.973632227832,616.710565160536,-37.1447052793803)) ;
#64565 = CARTESIAN_POINT('Ctrl Pts',(177.96378473025,616.710565160536,-37.0736687309019)) ;
#64566 = CARTESIAN_POINT('Ctrl Pts',(177.95774689361,616.710565160536,-37.0021880127456)) ;
#64567 = CARTESIAN_POINT('Ctrl Pts',(177.95318461716,616.710565160536,-36.9481761511335)) ;
#64568 = CARTESIAN_POINT('Ctrl Pts',(177.950798421621,616.710565160536,-36.8939099228487)) ;
#64569 = CARTESIAN_POINT('Ctrl Pts',(177.95057652878,616.710565160536,-36.8395366347886)) ;
#64570 = CARTESIAN_POINT('Ctrl Pts',(177.950439026467,616.710565160536,-36.8058426551063)) ;
#64571 = CARTESIAN_POINT('Ctrl Pts',(177.951132932983,616.710565160536,-36.7721074653787)) ;
#64572 = CARTESIAN_POINT('Ctrl Pts',(177.952658557802,616.710565160536,-36.7383656561305)) ;
#64573 = CARTESIAN_POINT('Ctrl Pts',(177.953241924976,616.710565160536,-36.7254634906293)) ;
#64574 = CARTESIAN_POINT('Ctrl Pts',(177.953947076004,616.710565160536,-36.7125580728955)) ;
#64575 = CARTESIAN_POINT('Ctrl Pts',(177.95477363332,616.710565160536,-36.6996587838914)) ;
#64576 = CARTESIAN_POINT('Ctrl Pts',(177.959680119899,616.710565160536,-36.6230879433847)) ;
#64577 = CARTESIAN_POINT('Ctrl Pts',(177.96884650041,616.710565160536,-36.5469198339896)) ;
#64578 = CARTESIAN_POINT('Ctrl Pts',(177.982204867157,616.710565160536,-36.4715679483824)) ;
#64579 = CARTESIAN_POINT('Ctrl Pts',(177.992223642217,616.710565160536,-36.4150540341769)) ;
#64580 = CARTESIAN_POINT('Ctrl Pts',(178.004601543926,616.710565160536,-36.3589985786665)) ;
#64581 = CARTESIAN_POINT('Ctrl Pts',(178.01933103088,616.710565160536,-36.3035726335972)) ;
#64582 = CARTESIAN_POINT('Ctrl Pts',(178.024555445297,616.710565160536,-36.2839135573912)) ;
#64583 = CARTESIAN_POINT('Ctrl Pts',(178.030075870223,616.710565160536,-36.2643336763624)) ;
#64584 = CARTESIAN_POINT('Ctrl Pts',(178.035892526252,616.710565160536,-36.2448406603716)) ;
#64585 = CARTESIAN_POINT('Ctrl Pts',(178.040298354069,616.710565160536,-36.2300756696835)) ;
#64586 = CARTESIAN_POINT('Ctrl Pts',(178.044872758394,616.710565160536,-36.215365382693)) ;
#64587 = CARTESIAN_POINT('Ctrl Pts',(178.049612935484,616.710565160536,-36.2007207121868)) ;
#64588 = CARTESIAN_POINT('Ctrl Pts',(178.072804589896,616.710565160536,-36.1290706174879)) ;
#64589 = CARTESIAN_POINT('Ctrl Pts',(178.099976840661,616.710565160536,-36.0589354223635)) ;
#64590 = CARTESIAN_POINT('Ctrl Pts',(178.131097670835,616.710565160536,-35.9906940138396)) ;
#64591 = CARTESIAN_POINT('Ctrl Pts',(178.156246568811,616.710565160536,-35.9355477914836)) ;
#64592 = CARTESIAN_POINT('Ctrl Pts',(178.183974962278,616.710565160536,-35.8816378803032)) ;
#64593 = CARTESIAN_POINT('Ctrl Pts',(178.21429059059,616.710565160536,-35.8291680617348)) ;
#64594 = CARTESIAN_POINT('Ctrl Pts',(178.220263208248,616.710565160536,-35.8188307478686)) ;
#64595 = CARTESIAN_POINT('Ctrl Pts',(178.226336317829,616.710565160493,-35.8085493533407)) ;
#64596 = CARTESIAN_POINT('Ctrl Pts',(178.232508579458,616.710565160534,-35.798324412355)) ;
#64597 = CARTESIAN_POINT('',(87.3885276254219,616.710565160552,-31.1471601717549)) ;
#64598 = CARTESIAN_POINT('',(87.3885276254219,616.710565160552,-39.8971601717549)) ;
#64599 = CARTESIAN_POINT('',(87.3885276254219,616.710565160552,-44.7721601717581)) ;
#64600 = CARTESIAN_POINT('',(87.2635276254219,616.710565160552,-40.0221601717549)) ;
#64601 = CARTESIAN_POINT('Origin',(87.2635276254219,616.710565160552,-39.8971601717549)) ;
#64602 = CARTESIAN_POINT('',(73.5135276254219,616.710565160554,-40.0221601717549)) ;
#64603 = CARTESIAN_POINT('',(142.888527625421,616.710565160542,-40.0221601717549)) ;
#64604 = CARTESIAN_POINT('',(73.3885276254219,616.710565160554,-39.8971601717549)) ;
#64605 = CARTESIAN_POINT('Origin',(73.5135276254219,616.710565160555,-39.8971601717549)) ;
#64606 = CARTESIAN_POINT('',(73.3885276254219,616.710565160554,-31.1471601717549)) ;
#64607 = CARTESIAN_POINT('',(73.3885276254219,616.710565160554,-40.272160171758)) ;
#64608 = CARTESIAN_POINT('',(73.5135276254219,616.710565160554,-31.0221601717549)) ;
#64609 = CARTESIAN_POINT('Origin',(73.5135276254219,616.710565160555,-31.1471601717549)) ;
#64610 = CARTESIAN_POINT('',(87.2635276254219,616.710565160552,-31.0221601717549)) ;
#64611 = CARTESIAN_POINT('',(149.888527625421,616.710565160541,-31.0221601717549)) ;
#64612 = CARTESIAN_POINT('Origin',(87.2635276254219,616.710565160552,-31.1471601717549)) ;
#64613 = CARTESIAN_POINT('',(94.6885276254222,616.710565160551,-25.7721601717558)) ;
#64614 = CARTESIAN_POINT('',(97.4385276254221,616.71056516055,-25.772160171756)) ;
#64615 = CARTESIAN_POINT('',(156.063527625422,616.71056516054,-25.7721601717586)) ;
#64616 = CARTESIAN_POINT('',(97.4385276254222,616.71056516055,-24.122160171756)) ;
#64617 = CARTESIAN_POINT('',(97.4385276254242,616.71056516055,19.910655277814)) ;
#64618 = CARTESIAN_POINT('',(124.938527625422,616.710565160545,-24.1221601717572)) ;
#64619 = CARTESIAN_POINT('',(97.4385276254222,616.71056516055,-24.122160171756)) ;
#64620 = CARTESIAN_POINT('',(124.938527625422,616.710565160545,-25.7721601717572)) ;
#64621 = CARTESIAN_POINT('',(124.938527625422,616.710565160545,-38.6663657544472)) ;
#64622 = CARTESIAN_POINT('',(127.688527625422,616.710565160545,-25.7721601717573)) ;
#64623 = CARTESIAN_POINT('',(156.063527625422,616.71056516054,-25.7721601717586)) ;
#64624 = CARTESIAN_POINT('',(127.688527625422,616.710565160545,-38.1221601717573)) ;
#64625 = CARTESIAN_POINT('',(127.688527625422,616.710565160545,-36.8221601717574)) ;
#64626 = CARTESIAN_POINT('',(122.688527625421,616.710564962099,-43.1221604682021)) ;
#64627 = CARTESIAN_POINT('Origin',(122.688527625422,616.710565160546,-38.1221601717571)) ;
#64628 = CARTESIAN_POINT('',(99.6885276254214,616.710565358997,-43.122160473101)) ;
#64629 = CARTESIAN_POINT('',(158.688527625421,616.710565160539,-43.1221607670988)) ;
#64630 = CARTESIAN_POINT('',(94.6885276254216,616.710565160551,-38.1221601717558)) ;
#64631 = CARTESIAN_POINT('Origin',(99.6885276254216,616.71056516055,-38.1221601717561)) ;
#64632 = CARTESIAN_POINT('',(94.6885276254213,616.710565160551,-45.8221601717558)) ;
#64633 = CARTESIAN_POINT('Origin',(212.388527625403,503.71056516053,0.477839828238782)) ;
#64634 = CARTESIAN_POINT('',(-2.61147237459854,503.710565160568,-43.4900362557631)) ;
#64635 = CARTESIAN_POINT('',(-2.61147237459654,503.710565160568,0.477839828248549)) ;
#64636 = CARTESIAN_POINT('',(0.388527634349634,503.710565160567,-43.4900362557631)) ;
#64637 = CARTESIAN_POINT('',(103.388527625413,503.710565160549,-43.4900362557631)) ;
#64638 = CARTESIAN_POINT('',(0.38852763376135,503.710565160567,-47.5221601717516)) ;
#64639 = CARTESIAN_POINT('',(0.388527634349642,503.710565160567,-24.0060982137622)) ;
#64640 = CARTESIAN_POINT('',(193.688527625401,503.710565160533,-47.5221601717604)) ;
#64641 = CARTESIAN_POINT('',(-2.61147237459866,503.710565160568,-47.5221601717515)) ;
#64642 = CARTESIAN_POINT('',(193.688527625402,503.710565160533,-28.5221601717604)) ;
#64643 = CARTESIAN_POINT('',(193.688527625401,503.710565160533,-47.5221601717604)) ;
#64644 = CARTESIAN_POINT('',(197.688527625402,503.710565160533,-28.5221601717606)) ;
#64645 = CARTESIAN_POINT('Origin',(195.688527625402,503.710565160533,-28.5221601717605)) ;
#64646 = CARTESIAN_POINT('',(197.688527625401,503.710565160533,-47.5221601717606)) ;
#64647 = CARTESIAN_POINT('',(197.688527625401,503.710565160533,-47.5221601717606)) ;
#64648 = CARTESIAN_POINT('',(201.668527625401,503.710565160532,-47.5221601717608)) ;
#64649 = CARTESIAN_POINT('',(201.668527625401,503.710565160532,-47.5221601717608)) ;
#64650 = CARTESIAN_POINT('',(201.668527625402,503.710565160532,-28.5221601717607)) ;
#64651 = CARTESIAN_POINT('',(201.668527625401,503.710565160532,-47.5221601717608)) ;
#64652 = CARTESIAN_POINT('',(205.668527625402,503.710565160531,-28.5221601717609)) ;
#64653 = CARTESIAN_POINT('Origin',(203.668527625402,503.710565160532,-28.5221601717608)) ;
#64654 = CARTESIAN_POINT('',(205.668527625401,503.710565160531,-47.5221601717609)) ;
#64655 = CARTESIAN_POINT('',(205.668527625402,503.710565160531,-28.5221601717609)) ;
#64656 = CARTESIAN_POINT('',(-2.61147237459866,503.710565160568,-47.5221601717515)) ;
#64657 = CARTESIAN_POINT('',(104.888527625403,503.710565160549,-19.5221601717563)) ;
#64658 = CARTESIAN_POINT('',(3.73852762540217,503.710565160567,-24.0221601717537)) ;
#64659 = CARTESIAN_POINT('Origin',(6.48852762540217,503.710565160566,-24.0221601717538)) ;
#64660 = CARTESIAN_POINT('',(21.3885276254017,503.710565160564,-37.2221601717525)) ;
#64661 = CARTESIAN_POINT('',(23.3885276254017,503.710565160563,-37.2221601717526)) ;
#64662 = CARTESIAN_POINT('',(21.3885276254017,503.710565160564,-37.2221601717525)) ;
#64663 = CARTESIAN_POINT('',(21.3885276254021,503.710565160564,-30.2221601717525)) ;
#64664 = CARTESIAN_POINT('',(21.3885276254021,503.710565160564,-30.2221601717525)) ;
#64665 = CARTESIAN_POINT('',(23.3885276254021,503.710565160563,-30.2221601717526)) ;
#64666 = CARTESIAN_POINT('',(23.3885276254021,503.710565160563,-30.2221601717526)) ;
#64667 = CARTESIAN_POINT('',(23.3885276254017,503.710565160563,-37.2221601717526)) ;
#64668 = CARTESIAN_POINT('',(36.3885276254017,503.710565160561,-37.2221601717532)) ;
#64669 = CARTESIAN_POINT('',(38.3885276254017,503.710565160561,-37.2221601717533)) ;
#64670 = CARTESIAN_POINT('',(36.3885276254017,503.710565160561,-37.2221601717532)) ;
#64671 = CARTESIAN_POINT('',(36.3885276254021,503.710565160561,-30.2221601717532)) ;
#64672 = CARTESIAN_POINT('',(36.3885276254021,503.710565160561,-30.2221601717532)) ;
#64673 = CARTESIAN_POINT('',(38.3885276254021,503.710565160561,-30.2221601717533)) ;
#64674 = CARTESIAN_POINT('',(38.3885276254021,503.710565160561,-30.2221601717533)) ;
#64675 = CARTESIAN_POINT('',(38.3885276254017,503.710565160561,-37.2221601717533)) ;
#64676 = CARTESIAN_POINT('',(186.388527625402,503.710565160535,-37.22216017176)) ;
#64677 = CARTESIAN_POINT('',(188.388527625402,503.710565160534,-37.2221601717601)) ;
#64678 = CARTESIAN_POINT('',(186.388527625402,503.710565160535,-37.22216017176)) ;
#64679 = CARTESIAN_POINT('',(186.388527625402,503.710565160535,-30.22216017176)) ;
#64680 = CARTESIAN_POINT('',(186.388527625402,503.710565160535,-30.22216017176)) ;
#64681 = CARTESIAN_POINT('',(188.388527625402,503.710565160534,-30.2221601717601)) ;
#64682 = CARTESIAN_POINT('',(188.388527625402,503.710565160534,-30.2221601717601)) ;
#64683 = CARTESIAN_POINT('',(188.388527625402,503.710565160534,-37.2221601717601)) ;
#64684 = CARTESIAN_POINT('',(174.638527625402,503.710565160537,-38.1221601717595)) ;
#64685 = CARTESIAN_POINT('',(169.388527626231,503.710565160538,-43.3721601717593)) ;
#64686 = CARTESIAN_POINT('Origin',(169.388527625402,503.710565160538,-38.1221601717593)) ;
#64687 = CARTESIAN_POINT('',(89.9885276254015,503.710565160552,-43.3721601717557)) ;
#64688 = CARTESIAN_POINT('',(89.9885276254015,503.710565160552,-43.3721601717557)) ;
#64689 = CARTESIAN_POINT('',(84.7385276254017,503.710565160553,-38.122160172492)) ;
#64690 = CARTESIAN_POINT('Origin',(89.9885276254017,503.710565160551,-38.1221601717557)) ;
#64691 = CARTESIAN_POINT('',(84.7385276254024,503.710565160553,-24.1221601717554)) ;
#64692 = CARTESIAN_POINT('',(84.7385276254024,503.710565160553,-24.1221601717554)) ;
#64693 = CARTESIAN_POINT('',(174.638527625402,503.710565160537,-24.1221601717595)) ;
#64694 = CARTESIAN_POINT('',(174.638527625402,503.710565160537,-24.1221601717595)) ;
#64695 = CARTESIAN_POINT('',(174.638527625402,503.710565160537,-38.1221601717595)) ;
#64696 = CARTESIAN_POINT('',(184.638264665915,503.710565160535,-24.0197428787721)) ;
#64697 = CARTESIAN_POINT('Origin',(187.388264603402,503.710565160534,-24.0203292412001)) ;
#64698 = CARTESIAN_POINT('Ctrl Pts',(180.967886278451,503.710565160535,-38.2912310516114)) ;
#64699 = CARTESIAN_POINT('Ctrl Pts',(180.92565375431,503.710565160535,-38.3365015005273)) ;
#64700 = CARTESIAN_POINT('Ctrl Pts',(180.88084697963,503.710565160535,-38.3790384629369)) ;
#64701 = CARTESIAN_POINT('Ctrl Pts',(180.833812038503,503.710565160535,-38.4188456718954)) ;
#64702 = CARTESIAN_POINT('Ctrl Pts',(180.783552496009,503.710565160535,-38.4613819664522)) ;
#64703 = CARTESIAN_POINT('Ctrl Pts',(180.730748583964,503.710565160535,-38.5008021215736)) ;
#64704 = CARTESIAN_POINT('Ctrl Pts',(180.6757674221,503.710565160535,-38.5370815538523)) ;
#64705 = CARTESIAN_POINT('Ctrl Pts',(180.621328160552,503.710565160535,-38.5730034120977)) ;
#64706 = CARTESIAN_POINT('Ctrl Pts',(180.564753402286,503.710565160535,-38.6058465535098)) ;
#64707 = CARTESIAN_POINT('Ctrl Pts',(180.506357253569,503.710565160535,-38.635551369466)) ;
#64708 = CARTESIAN_POINT('Ctrl Pts',(180.487215433648,503.710565160535,-38.6452883855246)) ;
#64709 = CARTESIAN_POINT('Ctrl Pts',(180.467877629559,503.710565160535,-38.6546878813455)) ;
#64710 = CARTESIAN_POINT('Ctrl Pts',(180.448354169154,503.710565160535,-38.6637467966359)) ;
#64711 = CARTESIAN_POINT('Ctrl Pts',(180.436388189703,503.710565160535,-38.669299029281)) ;
#64712 = CARTESIAN_POINT('Ctrl Pts',(180.424350978305,503.710565160535,-38.6747238305229)) ;
#64713 = CARTESIAN_POINT('Ctrl Pts',(180.412264471211,503.710565160535,-38.680012215594)) ;
#64714 = CARTESIAN_POINT('Ctrl Pts',(180.350923190186,503.710565160535,-38.7068517575963)) ;
#64715 = CARTESIAN_POINT('Ctrl Pts',(180.288204921529,503.710565160536,-38.7302329640473)) ;
#64716 = CARTESIAN_POINT('Ctrl Pts',(180.224469064525,503.710565160536,-38.7501348242744)) ;
#64717 = CARTESIAN_POINT('Ctrl Pts',(180.159384674807,503.710565160536,-38.770457771012)) ;
#64718 = CARTESIAN_POINT('Ctrl Pts',(180.093238347601,503.710565160536,-38.7871531590327)) ;
#64719 = CARTESIAN_POINT('Ctrl Pts',(180.02637585154,503.710565160536,-38.8001588616604)) ;
#64720 = CARTESIAN_POINT('Ctrl Pts',(179.970650823328,503.710565160536,-38.8109981690234)) ;
#64721 = CARTESIAN_POINT('Ctrl Pts',(179.914427390569,503.710565160536,-38.8192740427725)) ;
#64722 = CARTESIAN_POINT('Ctrl Pts',(179.857893451262,503.710565160536,-38.8249257343172)) ;
#64723 = CARTESIAN_POINT('Ctrl Pts',(179.831683152833,503.710565160536,-38.8275459748988)) ;
#64724 = CARTESIAN_POINT('Ctrl Pts',(179.805405999129,503.710565160536,-38.8296018263968)) ;
#64725 = CARTESIAN_POINT('Ctrl Pts',(179.779080308959,503.710565160536,-38.8310854028428)) ;
#64726 = CARTESIAN_POINT('Ctrl Pts',(179.767740376304,503.710565160536,-38.8317244613776)) ;
#64727 = CARTESIAN_POINT('Ctrl Pts',(179.756392022526,503.710565160536,-38.8322572009363)) ;
#64728 = CARTESIAN_POINT('Ctrl Pts',(179.745050204682,503.710565160536,-38.8326827020381)) ;
#64729 = CARTESIAN_POINT('Ctrl Pts',(179.674861914567,503.710565160536,-38.8353158949874)) ;
#64730 = CARTESIAN_POINT('Ctrl Pts',(179.604793209435,503.710565160536,-38.8338540559347)) ;
#64731 = CARTESIAN_POINT('Ctrl Pts',(179.535207522758,503.710565160536,-38.828245024526)) ;
#64732 = CARTESIAN_POINT('Ctrl Pts',(179.472638445,503.710565160536,-38.8232015746569)) ;
#64733 = CARTESIAN_POINT('Ctrl Pts',(179.41045891369,503.710565160536,-38.8148047974643)) ;
#64734 = CARTESIAN_POINT('Ctrl Pts',(179.34892078897,503.710565160536,-38.8029829646867)) ;
#64735 = CARTESIAN_POINT('Ctrl Pts',(179.282222053105,503.710565160536,-38.7901697484007)) ;
#64736 = CARTESIAN_POINT('Ctrl Pts',(179.216275960956,503.710565160536,-38.7733339808827)) ;
#64737 = CARTESIAN_POINT('Ctrl Pts',(179.151294678068,503.710565160536,-38.7527197824229)) ;
#64738 = CARTESIAN_POINT('Ctrl Pts',(179.126490124642,503.710565160536,-38.744850962906)) ;
#64739 = CARTESIAN_POINT('Ctrl Pts',(179.10182620156,503.710565160536,-38.7364310486033)) ;
#64740 = CARTESIAN_POINT('Ctrl Pts',(179.077315026189,503.710565160536,-38.7274716808344)) ;
#64741 = CARTESIAN_POINT('Ctrl Pts',(179.066519724691,503.710565160536,-38.7235257633161)) ;
#64742 = CARTESIAN_POINT('Ctrl Pts',(179.055755047888,503.710565160536,-38.7194754705714)) ;
#64743 = CARTESIAN_POINT('Ctrl Pts',(179.045033923296,503.710565160536,-38.7153266502158)) ;
#64744 = CARTESIAN_POINT('Ctrl Pts',(178.979778672122,503.710565160536,-38.6900744192535)) ;
#64745 = CARTESIAN_POINT('Ctrl Pts',(178.916019125604,503.710565160536,-38.6611341011757)) ;
#64746 = CARTESIAN_POINT('Ctrl Pts',(178.853972447146,503.710565160536,-38.6288174516854)) ;
#64747 = CARTESIAN_POINT('Ctrl Pts',(178.790503950737,503.710565160536,-38.5957602566335)) ;
#64748 = CARTESIAN_POINT('Ctrl Pts',(178.728826906058,503.710565160536,-38.5591699147713)) ;
#64749 = CARTESIAN_POINT('Ctrl Pts',(178.669177648379,503.710565160536,-38.519324021345)) ;
#64750 = CARTESIAN_POINT('Ctrl Pts',(178.624103739663,503.710565160536,-38.4892145072808)) ;
#64751 = CARTESIAN_POINT('Ctrl Pts',(178.580187697085,503.710565160536,-38.4572448398469)) ;
#64752 = CARTESIAN_POINT('Ctrl Pts',(178.537537375342,503.710565160536,-38.4235161002359)) ;
#64753 = CARTESIAN_POINT('Ctrl Pts',(178.511107918117,503.710565160536,-38.4026151493317)) ;
#64754 = CARTESIAN_POINT('Ctrl Pts',(178.485164615864,503.710565160536,-38.3810384077748)) ;
#64755 = CARTESIAN_POINT('Ctrl Pts',(178.459734712388,503.710565160536,-38.3588072065482)) ;
#64756 = CARTESIAN_POINT('Ctrl Pts',(178.450011722904,503.710565160536,-38.3503072240003)) ;
#64757 = CARTESIAN_POINT('Ctrl Pts',(178.440362108393,503.710565160536,-38.3417100057849)) ;
#64758 = CARTESIAN_POINT('Ctrl Pts',(178.430792970441,503.710565160536,-38.3330216985486)) ;
#64759 = CARTESIAN_POINT('Ctrl Pts',(178.373987234065,503.710565160536,-38.2814448801484)) ;
#64760 = CARTESIAN_POINT('Ctrl Pts',(178.320152186293,503.710565160536,-38.226788560022)) ;
#64761 = CARTESIAN_POINT('Ctrl Pts',(178.269568813303,503.710565160536,-38.1693636809231)) ;
#64762 = CARTESIAN_POINT('Ctrl Pts',(178.23163128356,503.710565160536,-38.1262950215989)) ;
#64763 = CARTESIAN_POINT('Ctrl Pts',(178.195523006449,503.710565160536,-38.0816677449143)) ;
#64764 = CARTESIAN_POINT('Ctrl Pts',(178.161373031284,503.710565160536,-38.0355944133095)) ;
#64765 = CARTESIAN_POINT('Ctrl Pts',(178.149255999991,503.710565160536,-38.019246758644)) ;
#64766 = CARTESIAN_POINT('Ctrl Pts',(178.137385615073,503.710565160536,-38.0027169197252)) ;
#64767 = CARTESIAN_POINT('Ctrl Pts',(178.125768018023,503.710565160536,-37.9860095118681)) ;
#64768 = CARTESIAN_POINT('Ctrl Pts',(178.116969171299,503.710565160536,-37.9733557831959)) ;
#64769 = CARTESIAN_POINT('Ctrl Pts',(178.108318282793,503.710565160536,-37.9606043293897)) ;
#64770 = CARTESIAN_POINT('Ctrl Pts',(178.099822126482,503.710565160536,-37.9477641318199)) ;
#64771 = CARTESIAN_POINT('Ctrl Pts',(178.058264513485,503.710565160536,-37.8849583238938)) ;
#64772 = CARTESIAN_POINT('Ctrl Pts',(178.020373148467,503.710565160536,-37.8199849150515)) ;
#64773 = CARTESIAN_POINT('Ctrl Pts',(177.986424343053,503.710565160536,-37.7531052054847)) ;
#64774 = CARTESIAN_POINT('Ctrl Pts',(177.958995501856,503.710565160536,-37.6990699335321)) ;
#64775 = CARTESIAN_POINT('Ctrl Pts',(177.934140557017,503.710565160536,-37.6437892876456)) ;
#64776 = CARTESIAN_POINT('Ctrl Pts',(177.91202358458,503.710565160536,-37.5873842224957)) ;
#64777 = CARTESIAN_POINT('Ctrl Pts',(177.907910233637,503.710565160536,-37.5768939156241)) ;
#64778 = CARTESIAN_POINT('Ctrl Pts',(177.903891641335,503.710565160536,-37.5663646802333)) ;
#64779 = CARTESIAN_POINT('Ctrl Pts',(177.899967455474,503.710565160536,-37.5557976775097)) ;
#64780 = CARTESIAN_POINT('',(180.969462539582,503.709690117684,-35.7520600489767)) ;
#64781 = CARTESIAN_POINT('Ctrl Pts',(177.903353299729,503.710565160537,-36.4919899545743)) ;
#64782 = CARTESIAN_POINT('Ctrl Pts',(177.92875366093,503.710565160537,-36.4233890781418)) ;
#64783 = CARTESIAN_POINT('Ctrl Pts',(177.958054337873,503.710565160536,-36.3564906321787)) ;
#64784 = CARTESIAN_POINT('Ctrl Pts',(177.990958463266,503.710565160536,-36.2914824522412)) ;
#64785 = CARTESIAN_POINT('Ctrl Pts',(178.024805498497,503.710565160536,-36.2246113796841)) ;
#64786 = CARTESIAN_POINT('Ctrl Pts',(178.062466153447,503.710565160536,-36.1597396883479)) ;
#64787 = CARTESIAN_POINT('Ctrl Pts',(178.103662086193,503.710565160536,-36.0971030288243)) ;
#64788 = CARTESIAN_POINT('Ctrl Pts',(178.138514153112,503.710565160536,-36.0441119468471)) ;
#64789 = CARTESIAN_POINT('Ctrl Pts',(178.175897575913,503.710565160536,-35.9927208717011)) ;
#64790 = CARTESIAN_POINT('Ctrl Pts',(178.21566192862,503.710565160536,-35.943095316901)) ;
#64791 = CARTESIAN_POINT('Ctrl Pts',(178.233297088326,503.710565160536,-35.921086796082)) ;
#64792 = CARTESIAN_POINT('Ctrl Pts',(178.251400720061,503.710565160536,-35.8994258300726)) ;
#64793 = CARTESIAN_POINT('Ctrl Pts',(178.269960423474,503.710565160536,-35.8781284061811)) ;
#64794 = CARTESIAN_POINT('Ctrl Pts',(178.280129763591,503.710565160536,-35.8664589984135)) ;
#64795 = CARTESIAN_POINT('Ctrl Pts',(178.290436033294,503.710565160536,-35.8548987517908)) ;
#64796 = CARTESIAN_POINT('Ctrl Pts',(178.300877233601,503.710565160536,-35.8434504287225)) ;
#64797 = CARTESIAN_POINT('Ctrl Pts',(178.31058164402,503.710565160536,-35.8328099637962)) ;
#64798 = CARTESIAN_POINT('Ctrl Pts',(178.320404209226,503.710565160536,-35.822264668811)) ;
#64799 = CARTESIAN_POINT('Ctrl Pts',(178.330327661833,503.710565160536,-35.8118328392013)) ;
#64800 = CARTESIAN_POINT('Ctrl Pts',(178.380816949237,503.710565160536,-35.758756993108)) ;
#64801 = CARTESIAN_POINT('Ctrl Pts',(178.433998984568,503.710565160536,-35.7085211059001)) ;
#64802 = CARTESIAN_POINT('Ctrl Pts',(178.489610693573,503.710565160536,-35.6613432501725)) ;
#64803 = CARTESIAN_POINT('Ctrl Pts',(178.54480483254,503.710565160536,-35.6145196374518)) ;
#64804 = CARTESIAN_POINT('Ctrl Pts',(178.602393186154,503.710565160536,-35.5707077956924)) ;
#64805 = CARTESIAN_POINT('Ctrl Pts',(178.662142797171,503.710565160536,-35.5301657365235)) ;
#64806 = CARTESIAN_POINT('Ctrl Pts',(178.711887595478,503.710565160536,-35.4964122689777)) ;
#64807 = CARTESIAN_POINT('Ctrl Pts',(178.763131118042,503.710565160536,-35.4649258789429)) ;
#64808 = CARTESIAN_POINT('Ctrl Pts',(178.815745375594,503.710565160536,-35.4358832546787)) ;
#64809 = CARTESIAN_POINT('Ctrl Pts',(178.837595338189,503.710565160536,-35.4238222605043)) ;
#64810 = CARTESIAN_POINT('Ctrl Pts',(178.8596817389,503.710565160536,-35.412183045738)) ;
#64811 = CARTESIAN_POINT('Ctrl Pts',(178.881995487401,503.710565160536,-35.4009796924745)) ;
#64812 = CARTESIAN_POINT('Ctrl Pts',(178.892403669081,503.710565160536,-35.3957539216374)) ;
#64813 = CARTESIAN_POINT('Ctrl Pts',(178.902861315364,503.710565160536,-35.3906229947982)) ;
#64814 = CARTESIAN_POINT('Ctrl Pts',(178.913367501389,503.710565160536,-35.3855884072292)) ;
#64815 = CARTESIAN_POINT('Ctrl Pts',(178.924203481469,503.710565160536,-35.38039578162)) ;
#64816 = CARTESIAN_POINT('Ctrl Pts',(178.935083458973,503.710565160536,-35.3753093268688)) ;
#64817 = CARTESIAN_POINT('Ctrl Pts',(178.946002593126,503.710565160536,-35.3703318526568)) ;
#64818 = CARTESIAN_POINT('Ctrl Pts',(179.008613014799,503.710565160536,-35.3417909670061)) ;
#64819 = CARTESIAN_POINT('Ctrl Pts',(179.072548898588,503.710565160536,-35.3168105966183)) ;
#64820 = CARTESIAN_POINT('Ctrl Pts',(179.137602482649,503.710565160536,-35.2956138225865)) ;
#64821 = CARTESIAN_POINT('Ctrl Pts',(179.196978933428,503.710565160536,-35.2762668607217)) ;
#64822 = CARTESIAN_POINT('Ctrl Pts',(179.257287126168,503.710565160536,-35.2600722124355)) ;
#64823 = CARTESIAN_POINT('Ctrl Pts',(179.318373891923,503.710565160536,-35.2472371731657)) ;
#64824 = CARTESIAN_POINT('Ctrl Pts',(179.390171666925,503.710565160536,-35.2321516263986)) ;
#64825 = CARTESIAN_POINT('Ctrl Pts',(179.463046503792,503.710565160536,-35.2217065918144)) ;
#64826 = CARTESIAN_POINT('Ctrl Pts',(179.536577016775,503.710565160536,-35.2158270641581)) ;
#64827 = CARTESIAN_POINT('Ctrl Pts',(179.552888295767,503.710565160536,-35.2145228081146)) ;
#64828 = CARTESIAN_POINT('Ctrl Pts',(179.569231755604,503.710565160536,-35.2134434417709)) ;
#64829 = CARTESIAN_POINT('Ctrl Pts',(179.585602626049,503.710565160536,-35.2125885256099)) ;
#64830 = CARTESIAN_POINT('Ctrl Pts',(179.601628939277,503.710565160536,-35.2117516028435)) ;
#64831 = CARTESIAN_POINT('Ctrl Pts',(179.617686819584,503.710565160536,-35.2111297845562)) ;
#64832 = CARTESIAN_POINT('Ctrl Pts',(179.633740546289,503.710565160536,-35.2107231585423)) ;
#64833 = CARTESIAN_POINT('Ctrl Pts',(179.702365296106,503.710565160536,-35.2089849572519)) ;
#64834 = CARTESIAN_POINT('Ctrl Pts',(179.771008351008,503.710565160536,-35.2111671895507)) ;
#64835 = CARTESIAN_POINT('Ctrl Pts',(179.839332646661,503.710565160536,-35.2171487203655)) ;
#64836 = CARTESIAN_POINT('Ctrl Pts',(179.907485468652,503.710565160536,-35.2231152393167)) ;
#64837 = CARTESIAN_POINT('Ctrl Pts',(179.975322186611,503.710565160536,-35.2328624822925)) ;
#64838 = CARTESIAN_POINT('Ctrl Pts',(180.04249323035,503.710565160536,-35.2463196524421)) ;
#64839 = CARTESIAN_POINT('Ctrl Pts',(180.091658875707,503.710565160536,-35.2561695880431)) ;
#64840 = CARTESIAN_POINT('Ctrl Pts',(180.140467636658,503.710565160536,-35.2680081514718)) ;
#64841 = CARTESIAN_POINT('Ctrl Pts',(180.188772438976,503.710565160536,-35.2818222804086)) ;
#64842 = CARTESIAN_POINT('Ctrl Pts',(180.208747209415,503.710565160536,-35.2875346328267)) ;
#64843 = CARTESIAN_POINT('Ctrl Pts',(180.228635683059,503.710565160536,-35.2935849339919)) ;
#64844 = CARTESIAN_POINT('Ctrl Pts',(180.248426887822,503.710565160536,-35.299972818117)) ;
#64845 = CARTESIAN_POINT('Ctrl Pts',(180.263114163255,503.710565160536,-35.3047133387022)) ;
#64846 = CARTESIAN_POINT('Ctrl Pts',(180.277747862838,503.710565160535,-35.3096397827144)) ;
#64847 = CARTESIAN_POINT('Ctrl Pts',(180.292323364453,503.710565160535,-35.3147521090727)) ;
#64848 = CARTESIAN_POINT('Ctrl Pts',(180.30459079341,503.710565160535,-35.3190548838288)) ;
#64849 = CARTESIAN_POINT('Ctrl Pts',(180.316809027902,503.710565160536,-35.3234865664285)) ;
#64850 = CARTESIAN_POINT('Ctrl Pts',(180.32897214156,503.710565160536,-35.3280453620711)) ;
#64851 = CARTESIAN_POINT('Ctrl Pts',(180.390631696042,503.710565160535,-35.3511556705168)) ;
#64852 = CARTESIAN_POINT('Ctrl Pts',(180.450906378727,503.710565160535,-35.3775397554398)) ;
#64853 = CARTESIAN_POINT('Ctrl Pts',(180.509464067445,503.710565160535,-35.4071474167633)) ;
#64854 = CARTESIAN_POINT('Ctrl Pts',(180.550924650743,503.710565160536,-35.4281105205919)) ;
#64855 = CARTESIAN_POINT('Ctrl Pts',(180.591523970704,503.710565160535,-35.4506904812246)) ;
#64856 = CARTESIAN_POINT('Ctrl Pts',(180.631132547835,503.710565160535,-35.4748801279865)) ;
#64857 = CARTESIAN_POINT('Ctrl Pts',(180.643785109954,503.710565160535,-35.4826072676732)) ;
#64858 = CARTESIAN_POINT('Ctrl Pts',(180.656338382547,503.710565160535,-35.4904999551133)) ;
#64859 = CARTESIAN_POINT('Ctrl Pts',(180.668781798428,503.710565160535,-35.4985541650934)) ;
#64860 = CARTESIAN_POINT('Ctrl Pts',(180.721718073743,503.710565160535,-35.5328180586265)) ;
#64861 = CARTESIAN_POINT('Ctrl Pts',(180.772571486636,503.710565160536,-35.5699380877714)) ;
#64862 = CARTESIAN_POINT('Ctrl Pts',(180.821028469939,503.710565160536,-35.6098800128957)) ;
#64863 = CARTESIAN_POINT('Ctrl Pts',(180.866170170906,503.710565160536,-35.64708923058)) ;
#64864 = CARTESIAN_POINT('Ctrl Pts',(180.909232299481,503.710565160536,-35.6867479872827)) ;
#64865 = CARTESIAN_POINT('Ctrl Pts',(180.949927175311,503.710565160536,-35.7288508505215)) ;
#64866 = CARTESIAN_POINT('Ctrl Pts',(180.956875633919,503.710565160536,-35.7360397163559)) ;
#64867 = CARTESIAN_POINT('Ctrl Pts',(180.963754988301,503.710565160536,-35.7432998832669)) ;
#64868 = CARTESIAN_POINT('Ctrl Pts',(180.970564720765,503.710565160536,-35.7506301174499)) ;
#64869 = CARTESIAN_POINT('Ctrl Pts',(180.968292474022,503.709690117684,-35.7534348777401)) ;
#64870 = CARTESIAN_POINT('Ctrl Pts',(180.974127456679,503.709981798635,-35.7584008141771)) ;
#64871 = CARTESIAN_POINT('Ctrl Pts',(180.979928180602,503.710273479585,-35.7634070046711)) ;
#64872 = CARTESIAN_POINT('Ctrl Pts',(180.985694093679,503.710565160536,-35.7684529727346)) ;
#64873 = CARTESIAN_POINT('Ctrl Pts',(30.9678862784492,503.710565160562,-38.2912310516066)) ;
#64874 = CARTESIAN_POINT('Ctrl Pts',(30.9254422200844,503.710565160562,-38.3367282510996)) ;
#64875 = CARTESIAN_POINT('Ctrl Pts',(30.880398964238,503.710565160562,-38.37946524855)) ;
#64876 = CARTESIAN_POINT('Ctrl Pts',(30.8331075426913,503.710565160562,-38.4194456475178)) ;
#64877 = CARTESIAN_POINT('Ctrl Pts',(30.7840703595289,503.710565160562,-38.4609019218898)) ;
#64878 = CARTESIAN_POINT('Ctrl Pts',(30.7326155242731,503.710565160562,-38.4993948706189)) ;
#64879 = CARTESIAN_POINT('Ctrl Pts',(30.6790837502068,503.710565160562,-38.5349018025089)) ;
#64880 = CARTESIAN_POINT('Ctrl Pts',(30.6299497827742,503.710565160562,-38.5674917262607)) ;
#64881 = CARTESIAN_POINT('Ctrl Pts',(30.5790650716403,503.710565160562,-38.5975660462198)) ;
#64882 = CARTESIAN_POINT('Ctrl Pts',(30.5266633462617,503.710565160562,-38.6250826007819)) ;
#64883 = CARTESIAN_POINT('Ctrl Pts',(30.5009196669565,503.710565160562,-38.6386008075034)) ;
#64884 = CARTESIAN_POINT('Ctrl Pts',(30.4748094721683,503.710565160562,-38.651501306899)) ;
#64885 = CARTESIAN_POINT('Ctrl Pts',(30.4483585771217,503.710565160562,-38.6637766953976)) ;
#64886 = CARTESIAN_POINT('Ctrl Pts',(30.4363981919332,503.710565160562,-38.6693272967865)) ;
#64887 = CARTESIAN_POINT('Ctrl Pts',(30.4243666589546,503.710565160562,-38.6747505776815)) ;
#64888 = CARTESIAN_POINT('Ctrl Pts',(30.4122858861223,503.710565160562,-38.680037562082)) ;
#64889 = CARTESIAN_POINT('Ctrl Pts',(30.3508796463339,503.710565160562,-38.7069111600186)) ;
#64890 = CARTESIAN_POINT('Ctrl Pts',(30.2880936832432,503.710565160562,-38.7303188817798)) ;
#64891 = CARTESIAN_POINT('Ctrl Pts',(30.2242884283509,503.710565160562,-38.7502394834274)) ;
#64892 = CARTESIAN_POINT('Ctrl Pts',(30.1592053579717,503.710565160562,-38.7705590311074)) ;
#64893 = CARTESIAN_POINT('Ctrl Pts',(30.0930609196203,503.710565160562,-38.78725096046)) ;
#64894 = CARTESIAN_POINT('Ctrl Pts',(30.0262007044099,503.710565160562,-38.8002529480405)) ;
#64895 = CARTESIAN_POINT('Ctrl Pts',(29.9705502048792,503.710565160562,-38.8110750356074)) ;
#64896 = CARTESIAN_POINT('Ctrl Pts',(29.9144028696759,503.710565160562,-38.8193401845523)) ;
#64897 = CARTESIAN_POINT('Ctrl Pts',(29.8579457755199,503.710565160562,-38.8249877807562)) ;
#64898 = CARTESIAN_POINT('Ctrl Pts',(29.8317333455311,503.710565160562,-38.8276098997708)) ;
#64899 = CARTESIAN_POINT('Ctrl Pts',(29.8054540290931,503.710565160562,-38.8296674312635)) ;
#64900 = CARTESIAN_POINT('Ctrl Pts',(29.7791261443209,503.710565160562,-38.8311524769637)) ;
#64901 = CARTESIAN_POINT('Ctrl Pts',(29.7677907216731,503.710565160562,-38.8317918606745)) ;
#64902 = CARTESIAN_POINT('Ctrl Pts',(29.7564469004184,503.710565160562,-38.8323249875451)) ;
#64903 = CARTESIAN_POINT('Ctrl Pts',(29.7451096041583,503.710565160562,-38.8327509389944)) ;
#64904 = CARTESIAN_POINT('Ctrl Pts',(29.6749262076145,503.710565160562,-38.8353877863331)) ;
#64905 = CARTESIAN_POINT('Ctrl Pts',(29.6048622076397,503.710565160562,-38.8339293126068)) ;
#64906 = CARTESIAN_POINT('Ctrl Pts',(29.5352808719665,503.710565160562,-38.8283232046894)) ;
#64907 = CARTESIAN_POINT('Ctrl Pts',(29.472724443851,503.710565160562,-38.8232830874862)) ;
#64908 = CARTESIAN_POINT('Ctrl Pts',(29.4105571672994,503.710565160562,-38.8148902218149)) ;
#64909 = CARTESIAN_POINT('Ctrl Pts',(29.3490306789795,503.710565160562,-38.803072799948)) ;
#64910 = CARTESIAN_POINT('Ctrl Pts',(29.2823373784577,503.710565160562,-38.7902629860047)) ;
#64911 = CARTESIAN_POINT('Ctrl Pts',(29.2163961579544,503.710565160562,-38.7734303424986)) ;
#64912 = CARTESIAN_POINT('Ctrl Pts',(29.1514192353771,503.710565160562,-38.7528190391024)) ;
#64913 = CARTESIAN_POINT('Ctrl Pts',(29.1266144198082,503.710565160562,-38.7449507135631)) ;
#64914 = CARTESIAN_POINT('Ctrl Pts',(29.1019501818377,503.710565160562,-38.7365311742612)) ;
#64915 = CARTESIAN_POINT('Ctrl Pts',(29.0774386443169,503.710565160562,-38.7275720679129)) ;
#64916 = CARTESIAN_POINT('Ctrl Pts',(29.0666435317903,503.710565160562,-38.7236263928982)) ;
#64917 = CARTESIAN_POINT('Ctrl Pts',(29.0558790328607,503.710565160562,-38.7195763273467)) ;
#64918 = CARTESIAN_POINT('Ctrl Pts',(29.045158075543,503.710565160562,-38.7154277191505)) ;
#64919 = CARTESIAN_POINT('Ctrl Pts',(28.9791589808581,503.710565160562,-38.6898885460116)) ;
#64920 = CARTESIAN_POINT('Ctrl Pts',(28.9146895319876,503.710565160562,-38.660576147959)) ;
#64921 = CARTESIAN_POINT('Ctrl Pts',(28.8519745023136,503.710565160562,-38.6278128528298)) ;
#64922 = CARTESIAN_POINT('Ctrl Pts',(28.7892594726396,503.710565160562,-38.5950495577006)) ;
#64923 = CARTESIAN_POINT('Ctrl Pts',(28.7282980769725,503.710565160562,-38.5588348642162)) ;
#64924 = CARTESIAN_POINT('Ctrl Pts',(28.6693189033772,503.710565160562,-38.5194369089193)) ;
#64925 = CARTESIAN_POINT('Ctrl Pts',(28.6242424962455,503.710565160562,-38.4893259703478)) ;
#64926 = CARTESIAN_POINT('Ctrl Pts',(28.5803239211359,503.710565160562,-38.4573544700511)) ;
#64927 = CARTESIAN_POINT('Ctrl Pts',(28.5376710848583,503.710565160562,-38.4236235398199)) ;
#64928 = CARTESIAN_POINT('Ctrl Pts',(28.5112402242038,503.710565160562,-38.4027213538343)) ;
#64929 = CARTESIAN_POINT('Ctrl Pts',(28.4852955197386,503.710565160562,-38.3811432476202)) ;
#64930 = CARTESIAN_POINT('Ctrl Pts',(28.4598642273998,503.710565160562,-38.3589105629124)) ;
#64931 = CARTESIAN_POINT('Ctrl Pts',(28.4501422583436,503.710565160562,-38.3504113694824)) ;
#64932 = CARTESIAN_POINT('Ctrl Pts',(28.4404936410195,503.710565160562,-38.3418149523954)) ;
#64933 = CARTESIAN_POINT('Ctrl Pts',(28.4309254817057,503.710565160562,-38.3331274627464)) ;
#64934 = CARTESIAN_POINT('Ctrl Pts',(28.3756155014068,503.710565160562,-38.2829083071518)) ;
#64935 = CARTESIAN_POINT('Ctrl Pts',(28.3231217092647,503.710565160562,-38.22976926723)) ;
#64936 = CARTESIAN_POINT('Ctrl Pts',(28.2737032752297,503.710565160562,-38.1739980997431)) ;
#64937 = CARTESIAN_POINT('Ctrl Pts',(28.2343018407941,503.710565160562,-38.1295316158888)) ;
#64938 = CARTESIAN_POINT('Ctrl Pts',(28.196855448234,503.710565160562,-38.0833907473793)) ;
#64939 = CARTESIAN_POINT('Ctrl Pts',(28.1615070381898,503.710565160562,-38.0357006475321)) ;
#64940 = CARTESIAN_POINT('Ctrl Pts',(28.1493824195391,503.710565160562,-38.0193427894744)) ;
#64941 = CARTESIAN_POINT('Ctrl Pts',(28.1375047434509,503.710565160562,-38.0028025194573)) ;
#64942 = CARTESIAN_POINT('Ctrl Pts',(28.1258801643615,503.710565160562,-37.986084462753)) ;
#64943 = CARTESIAN_POINT('Ctrl Pts',(28.1170775594472,503.710565160562,-37.9734248690617)) ;
#64944 = CARTESIAN_POINT('Ctrl Pts',(28.1084230601432,503.710565160562,-37.9606674908369)) ;
#64945 = CARTESIAN_POINT('Ctrl Pts',(28.0999234232508,503.710565160562,-37.947821283878)) ;
#64946 = CARTESIAN_POINT('Ctrl Pts',(28.0583671615653,503.710565160562,-37.885013855183)) ;
#64947 = CARTESIAN_POINT('Ctrl Pts',(28.0204771462595,503.710565160562,-37.820038892815)) ;
#64948 = CARTESIAN_POINT('Ctrl Pts',(27.9865297735914,503.710565160562,-37.7531577608557)) ;
#64949 = CARTESIAN_POINT('Ctrl Pts',(27.9591114444449,503.710565160562,-37.6991397693109)) ;
#64950 = CARTESIAN_POINT('Ctrl Pts',(27.9342653114978,503.710565160562,-37.6438773379502)) ;
#64951 = CARTESIAN_POINT('Ctrl Pts',(27.9121553253602,503.710565160562,-37.5874913344463)) ;
#64952 = CARTESIAN_POINT('Ctrl Pts',(27.9080344254389,503.710565160562,-37.5769820073054)) ;
#64953 = CARTESIAN_POINT('Ctrl Pts',(27.9040086289005,503.710565160562,-37.5664336134156)) ;
#64954 = CARTESIAN_POINT('Ctrl Pts',(27.9000775815771,503.710565160562,-37.5558473201923)) ;
#64955 = CARTESIAN_POINT('',(30.9693502314749,503.709709629953,-35.752017413352)) ;
#64956 = CARTESIAN_POINT('Ctrl Pts',(27.9033532997302,503.710565160562,-36.4919899545636)) ;
#64957 = CARTESIAN_POINT('Ctrl Pts',(27.9291186323697,503.710565160562,-36.4224033692924)) ;
#64958 = CARTESIAN_POINT('Ctrl Pts',(27.9588957600935,503.710565160562,-36.3545683136294)) ;
#64959 = CARTESIAN_POINT('Ctrl Pts',(27.9923754132967,503.710565160562,-36.2886810453698)) ;
#64960 = CARTESIAN_POINT('Ctrl Pts',(28.0258550664998,503.710565160562,-36.2227937771102)) ;
#64961 = CARTESIAN_POINT('Ctrl Pts',(28.063038117047,503.710565160562,-36.1588536853544)) ;
#64962 = CARTESIAN_POINT('Ctrl Pts',(28.1036581552326,503.710565160562,-36.0970869979891)) ;
#64963 = CARTESIAN_POINT('Ctrl Pts',(28.138506638453,503.710565160562,-36.0440965168282)) ;
#64964 = CARTESIAN_POINT('Ctrl Pts',(28.175885788979,503.710565160562,-35.9927059676394)) ;
#64965 = CARTESIAN_POINT('Ctrl Pts',(28.2156453273487,503.710565160562,-35.9430808735254)) ;
#64966 = CARTESIAN_POINT('Ctrl Pts',(28.233276288535,503.710565160562,-35.9210751324112)) ;
#64967 = CARTESIAN_POINT('Ctrl Pts',(28.2513755055103,503.710565160562,-35.8994168519458)) ;
#64968 = CARTESIAN_POINT('Ctrl Pts',(28.2699305950182,503.710565160562,-35.8781220145597)) ;
#64969 = CARTESIAN_POINT('Ctrl Pts',(28.2800999139146,503.710565160562,-35.866451146999)) ;
#64970 = CARTESIAN_POINT('Ctrl Pts',(28.2904061701111,503.710565160562,-35.8548894646611)) ;
#64971 = CARTESIAN_POINT('Ctrl Pts',(28.3008473659548,503.710565160562,-35.8434397311424)) ;
#64972 = CARTESIAN_POINT('Ctrl Pts',(28.3105489342056,503.710565160562,-35.8328010674446)) ;
#64973 = CARTESIAN_POINT('Ctrl Pts',(28.320368593542,503.710565160562,-35.82225754226)) ;
#64974 = CARTESIAN_POINT('Ctrl Pts',(28.3302890881604,503.710565160562,-35.8118274425855)) ;
#64975 = CARTESIAN_POINT('Ctrl Pts',(28.3807743786878,503.710565160562,-35.7587487774032)) ;
#64976 = CARTESIAN_POINT('Ctrl Pts',(28.4339522312143,503.710565160562,-35.7085102932475)) ;
#64977 = CARTESIAN_POINT('Ctrl Pts',(28.4895597627111,503.710565160562,-35.6613301145146)) ;
#64978 = CARTESIAN_POINT('Ctrl Pts',(28.5443167148798,503.710565160562,-35.6148716093329)) ;
#64979 = CARTESIAN_POINT('Ctrl Pts',(28.6014304833919,503.710565160562,-35.5713781267935)) ;
#64980 = CARTESIAN_POINT('Ctrl Pts',(28.6606736741946,503.710565160562,-35.5311015201684)) ;
#64981 = CARTESIAN_POINT('Ctrl Pts',(28.7108477173343,503.710565160562,-35.496990592466)) ;
#64982 = CARTESIAN_POINT('Ctrl Pts',(28.7625497744598,503.710565160562,-35.4651875878731)) ;
#64983 = CARTESIAN_POINT('Ctrl Pts',(28.8156483638411,503.710565160562,-35.4358740627275)) ;
#64984 = CARTESIAN_POINT('Ctrl Pts',(28.8374967095457,503.710565160562,-35.4238124987826)) ;
#64985 = CARTESIAN_POINT('Ctrl Pts',(28.8595815347472,503.710565160562,-35.4121727463269)) ;
#64986 = CARTESIAN_POINT('Ctrl Pts',(28.8818937578735,503.710565160562,-35.4009688898361)) ;
#64987 = CARTESIAN_POINT('Ctrl Pts',(28.8923047118028,503.710565160562,-35.3957411349371)) ;
#64988 = CARTESIAN_POINT('Ctrl Pts',(28.9027651743749,503.710565160562,-35.3906082950447)) ;
#64989 = CARTESIAN_POINT('Ctrl Pts',(28.9132742207043,503.710565160562,-35.3855718671928)) ;
#64990 = CARTESIAN_POINT('Ctrl Pts',(28.9241052156119,503.710565160562,-35.3803811464836)) ;
#64991 = CARTESIAN_POINT('Ctrl Pts',(28.9349801687178,503.710565160562,-35.3752965290426)) ;
#64992 = CARTESIAN_POINT('Ctrl Pts',(28.9458942687065,503.710565160562,-35.3703208106301)) ;
#64993 = CARTESIAN_POINT('Ctrl Pts',(29.008497953578,503.710565160562,-35.3417799041121)) ;
#64994 = CARTESIAN_POINT('Ctrl Pts',(29.0724274399235,503.710565160562,-35.3167994837945)) ;
#64995 = CARTESIAN_POINT('Ctrl Pts',(29.137475170634,503.710565160562,-35.2956026432451)) ;
#64996 = CARTESIAN_POINT('Ctrl Pts',(29.1968462968923,503.710565160562,-35.2762556147971)) ;
#64997 = CARTESIAN_POINT('Ctrl Pts',(29.257149618713,503.710565160562,-35.2600608879941)) ;
#64998 = CARTESIAN_POINT('Ctrl Pts',(29.3182321292239,503.710565160562,-35.2472257671074)) ;
#64999 = CARTESIAN_POINT('Ctrl Pts',(29.3900256430099,503.710565160562,-35.2321399688877)) ;
#65000 = CARTESIAN_POINT('Ctrl Pts',(29.4628970918069,503.710565160562,-35.2216947742465)) ;
#65001 = CARTESIAN_POINT('Ctrl Pts',(29.5364249740576,503.710565160562,-35.2158151578688)) ;
#65002 = CARTESIAN_POINT('Ctrl Pts',(29.5527362121146,503.710565160562,-35.2145108387523)) ;
#65003 = CARTESIAN_POINT('Ctrl Pts',(29.5690796704536,503.710565160562,-35.2134314278103)) ;
#65004 = CARTESIAN_POINT('Ctrl Pts',(29.5854505771297,503.710565160562,-35.2125764852655)) ;
#65005 = CARTESIAN_POINT('Ctrl Pts',(29.6014759873991,503.710565160562,-35.2117395856784)) ;
#65006 = CARTESIAN_POINT('Ctrl Pts',(29.6175329970076,503.710565160562,-35.2111177828552)) ;
#65007 = CARTESIAN_POINT('Ctrl Pts',(29.6335858867968,503.710565160562,-35.2107111643659)) ;
#65008 = CARTESIAN_POINT('Ctrl Pts',(29.7019240276124,503.710565160562,-35.2089801644062)) ;
#65009 = CARTESIAN_POINT('Ctrl Pts',(29.7702809286704,503.710565160562,-35.2111372171644)) ;
#65010 = CARTESIAN_POINT('Ctrl Pts',(29.8383236179072,503.710565160562,-35.2170625644197)) ;
#65011 = CARTESIAN_POINT('Ctrl Pts',(29.9064660399472,503.710565160562,-35.2229965966859)) ;
#65012 = CARTESIAN_POINT('Ctrl Pts',(29.9742943886661,503.710565160562,-35.2327104142748)) ;
#65013 = CARTESIAN_POINT('Ctrl Pts',(30.041459281945,503.710565160562,-35.2461330463219)) ;
#65014 = CARTESIAN_POINT('Ctrl Pts',(30.0909216190662,503.710565160562,-35.2560178941786)) ;
#65015 = CARTESIAN_POINT('Ctrl Pts',(30.1400239014881,503.710565160562,-35.2679151962761)) ;
#65016 = CARTESIAN_POINT('Ctrl Pts',(30.1886164081109,503.710565160562,-35.2818116137659)) ;
#65017 = CARTESIAN_POINT('Ctrl Pts',(30.208591560155,503.710565160562,-35.2875240799777)) ;
#65018 = CARTESIAN_POINT('Ctrl Pts',(30.2284804448505,503.710565160562,-35.2935745008466)) ;
#65019 = CARTESIAN_POINT('Ctrl Pts',(30.2482720871462,503.710565160562,-35.2999625101028)) ;
#65020 = CARTESIAN_POINT('Ctrl Pts',(30.2629556614958,503.710565160562,-35.3047018241757)) ;
#65021 = CARTESIAN_POINT('Ctrl Pts',(30.2775857039317,503.710565160562,-35.3096269627605)) ;
#65022 = CARTESIAN_POINT('Ctrl Pts',(30.292157594932,503.710565160562,-35.314737884601)) ;
#65023 = CARTESIAN_POINT('Ctrl Pts',(30.304427653017,503.710565160562,-35.3190414652309)) ;
#65024 = CARTESIAN_POINT('Ctrl Pts',(30.3166485167175,503.710565160562,-35.3234740071886)) ;
#65025 = CARTESIAN_POINT('Ctrl Pts',(30.3288142437168,503.710565160562,-35.328033710417)) ;
#65026 = CARTESIAN_POINT('Ctrl Pts',(30.3904749935855,503.710565160562,-35.3511441024435)) ;
#65027 = CARTESIAN_POINT('Ctrl Pts',(30.4507511168733,503.710565160562,-35.3775282676525)) ;
#65028 = CARTESIAN_POINT('Ctrl Pts',(30.5093104003278,503.710565160562,-35.4071359897249)) ;
#65029 = CARTESIAN_POINT('Ctrl Pts',(30.5507715572228,503.710565160562,-35.4280988556914)) ;
#65030 = CARTESIAN_POINT('Ctrl Pts',(30.5913715511612,503.710565160562,-35.4506785253586)) ;
#65031 = CARTESIAN_POINT('Ctrl Pts',(30.6309808754795,503.710565160562,-35.4748678223483)) ;
#65032 = CARTESIAN_POINT('Ctrl Pts',(30.6436335721306,503.710565160562,-35.4825947867002)) ;
#65033 = CARTESIAN_POINT('Ctrl Pts',(30.6561869871989,503.710565160562,-35.4904872892693)) ;
#65034 = CARTESIAN_POINT('Ctrl Pts',(30.6686305569726,503.710565160562,-35.4985413075622)) ;
#65035 = CARTESIAN_POINT('Ctrl Pts',(30.7215682446495,503.710565160562,-35.5328048760309)) ;
#65036 = CARTESIAN_POINT('Ctrl Pts',(30.7724231620797,503.710565160562,-35.5699245066469)) ;
#65037 = CARTESIAN_POINT('Ctrl Pts',(30.8208816659006,503.710565160562,-35.6098659448696)) ;
#65038 = CARTESIAN_POINT('Ctrl Pts',(30.8660265554225,503.710565160562,-35.6470761695718)) ;
#65039 = CARTESIAN_POINT('Ctrl Pts',(30.9090917235183,503.710565160561,-35.6867360487803)) ;
#65040 = CARTESIAN_POINT('Ctrl Pts',(30.949789392883,503.710565160561,-35.7288401364669)) ;
#65041 = CARTESIAN_POINT('Ctrl Pts',(30.956738104198,503.710565160561,-35.7360289793437)) ;
#65042 = CARTESIAN_POINT('Ctrl Pts',(30.9636177085578,503.710565160561,-35.7432891216704)) ;
#65043 = CARTESIAN_POINT('Ctrl Pts',(30.9704276883881,503.710565160561,-35.750619329669)) ;
#65044 = CARTESIAN_POINT('Ctrl Pts',(30.968206386886,503.709709629953,-35.753361617214)) ;
#65045 = CARTESIAN_POINT('Ctrl Pts',(30.9739106697334,503.709994806822,-35.7582156525672)) ;
#65046 = CARTESIAN_POINT('Ctrl Pts',(30.9795822178181,503.710279983692,-35.7631081565965)) ;
#65047 = CARTESIAN_POINT('Ctrl Pts',(30.9852205152954,503.710565160562,-35.7680386843137)) ;
#65048 = CARTESIAN_POINT('Origin',(212.388527625421,618.71056516053,-49.5221601717612)) ;
#65049 = CARTESIAN_POINT('',(205.668527625422,618.710565160531,-47.5221601717609)) ;
#65050 = CARTESIAN_POINT('',(-2.61147237457848,618.710565160568,-47.5221601717514)) ;
#65051 = CARTESIAN_POINT('',(205.668527625422,618.710565160531,-28.5221601717609)) ;
#65052 = CARTESIAN_POINT('',(205.668527625422,618.710565160531,-47.5221601717609)) ;
#65053 = CARTESIAN_POINT('',(201.668527625422,618.710565160532,-28.5221601717607)) ;
#65054 = CARTESIAN_POINT('Origin',(203.668527625422,618.710565160532,-28.5221601717608)) ;
#65055 = CARTESIAN_POINT('',(201.668527625421,618.710565160532,-47.5221601717607)) ;
#65056 = CARTESIAN_POINT('',(201.668527625422,618.710565160532,-28.5221601717607)) ;
#65057 = CARTESIAN_POINT('',(197.688527625422,618.710565160533,-47.5221601717605)) ;
#65058 = CARTESIAN_POINT('',(201.668527625421,618.710565160532,-47.5221601717607)) ;
#65059 = CARTESIAN_POINT('',(197.688527625422,618.710565160533,-28.5221601717605)) ;
#65060 = CARTESIAN_POINT('',(197.688527625422,618.710565160533,-47.5221601717605)) ;
#65061 = CARTESIAN_POINT('',(193.688527625422,618.710565160533,-28.5221601717604)) ;
#65062 = CARTESIAN_POINT('Origin',(195.688527625422,618.710565160533,-28.5221601717604)) ;
#65063 = CARTESIAN_POINT('',(193.688527625422,618.710565160533,-47.5221601717603)) ;
#65064 = CARTESIAN_POINT('',(193.688527625422,618.710565160533,-47.5221601717603)) ;
#65065 = CARTESIAN_POINT('',(152.388527625422,618.710565160541,-47.5221601717584)) ;
#65066 = CARTESIAN_POINT('',(152.388527625422,618.710565160541,-47.5221601717584)) ;
#65067 = CARTESIAN_POINT('',(152.388527625422,618.710565160541,-28.5221601717585)) ;
#65068 = CARTESIAN_POINT('',(152.388527625422,618.710565160541,-47.5221601717584)) ;
#65069 = CARTESIAN_POINT('',(148.388527625422,618.710565160541,-28.5221601717583)) ;
#65070 = CARTESIAN_POINT('Origin',(150.388527625422,618.710565160541,-28.5221601717584)) ;
#65071 = CARTESIAN_POINT('',(148.388527625422,618.710565160541,-47.5221601717583)) ;
#65072 = CARTESIAN_POINT('',(148.388527625422,618.710565160541,-28.5221601717583)) ;
#65073 = CARTESIAN_POINT('',(144.388527625422,618.710565160542,-47.5221601717581)) ;
#65074 = CARTESIAN_POINT('',(144.388527625422,618.710565160542,-47.5221601717581)) ;
#65075 = CARTESIAN_POINT('',(144.388527625422,618.710565160542,-28.5221601717581)) ;
#65076 = CARTESIAN_POINT('',(144.388527625422,618.710565160542,-47.5221601717581)) ;
#65077 = CARTESIAN_POINT('',(140.388527625422,618.710565160543,-28.5221601717579)) ;
#65078 = CARTESIAN_POINT('Origin',(142.388527625422,618.710565160542,-28.522160171758)) ;
#65079 = CARTESIAN_POINT('',(140.388527625421,618.710565160543,-47.5221601717579)) ;
#65080 = CARTESIAN_POINT('',(140.388527625422,618.710565160543,-28.5221601717579)) ;
#65081 = CARTESIAN_POINT('',(0.388527633780582,618.710565160567,-47.5221601717516)) ;
#65082 = CARTESIAN_POINT('',(-2.61147237457848,618.710565160568,-47.5221601717514)) ;
#65083 = CARTESIAN_POINT('',(0.3885276343684,618.710565160567,-43.4900362557631)) ;
#65084 = CARTESIAN_POINT('',(0.388527634368422,618.710565160567,-49.0060982137622)) ;
#65085 = CARTESIAN_POINT('',(-2.61147237457834,618.710565160568,-43.4900362557631)) ;
#65086 = CARTESIAN_POINT('',(103.388527625432,618.710565160549,-43.4900362557631)) ;
#65087 = CARTESIAN_POINT('',(-2.61147237457749,618.710565160568,-24.5221601717514)) ;
#65088 = CARTESIAN_POINT('',(104.888527625423,618.710565160549,-19.5221601717563)) ;
#65089 = CARTESIAN_POINT('',(87.2635276254222,618.710565160552,-30.8971601717549)) ;
#65090 = CARTESIAN_POINT('',(87.5135276254222,618.710565160552,-31.1471601717549)) ;
#65091 = CARTESIAN_POINT('Origin',(87.2635276254222,618.710565160552,-31.1471601717549)) ;
#65092 = CARTESIAN_POINT('',(73.5135276254222,618.710565160554,-30.8971601717549)) ;
#65093 = CARTESIAN_POINT('',(149.888527625422,618.710565160541,-30.8971601717549)) ;
#65094 = CARTESIAN_POINT('',(73.2635276254222,618.710565160554,-31.1471601717549)) ;
#65095 = CARTESIAN_POINT('Origin',(73.5135276254222,618.710565160554,-31.1471601717549)) ;
#65096 = CARTESIAN_POINT('',(73.2635276254222,618.710565160554,-39.8971601717549)) ;
#65097 = CARTESIAN_POINT('',(73.2635276254222,618.710565160554,-40.272160171758)) ;
#65098 = CARTESIAN_POINT('',(73.5135276254222,618.710565160554,-40.1471601717549)) ;
#65099 = CARTESIAN_POINT('Origin',(73.5135276254222,618.710565160554,-39.8971601717549)) ;
#65100 = CARTESIAN_POINT('',(87.2635276254222,618.710565160552,-40.1471601717549)) ;
#65101 = CARTESIAN_POINT('',(142.888527625422,618.710565160542,-40.1471601717549)) ;
#65102 = CARTESIAN_POINT('',(87.5135276254222,618.710565160552,-39.8971601717549)) ;
#65103 = CARTESIAN_POINT('Origin',(87.2635276254222,618.710565160552,-39.8971601717549)) ;
#65104 = CARTESIAN_POINT('',(87.5135276254222,618.710565160552,-44.772160171758)) ;
#65105 = CARTESIAN_POINT('Ctrl Pts',(30.9678862784723,618.710565160562,-35.7530892919022)) ;
#65106 = CARTESIAN_POINT('Ctrl Pts',(30.9246614854188,618.710565160562,-35.7067551968985)) ;
#65107 = CARTESIAN_POINT('Ctrl Pts',(30.8787404524756,618.710565160562,-35.6632842920493)) ;
#65108 = CARTESIAN_POINT('Ctrl Pts',(30.830493598688,618.710565160562,-35.6226728706452)) ;
#65109 = CARTESIAN_POINT('Ctrl Pts',(30.7822467449005,618.710565160562,-35.5820614492412)) ;
#65110 = CARTESIAN_POINT('Ctrl Pts',(30.7316733549856,618.710565160562,-35.5443091349957)) ;
#65111 = CARTESIAN_POINT('Ctrl Pts',(30.679095936171,618.710565160562,-35.5094375726184)) ;
#65112 = CARTESIAN_POINT('Ctrl Pts',(30.6299565110526,618.710565160562,-35.476846232708)) ;
#65113 = CARTESIAN_POINT('Ctrl Pts',(30.5790656467369,618.710565160562,-35.4467712038711)) ;
#65114 = CARTESIAN_POINT('Ctrl Pts',(30.5266572192249,618.710565160562,-35.4192545791151)) ;
#65115 = CARTESIAN_POINT('Ctrl Pts',(30.5009144572275,618.710565160562,-35.405738548284)) ;
#65116 = CARTESIAN_POINT('Ctrl Pts',(30.4748051669133,618.710565160562,-35.3928401771113)) ;
#65117 = CARTESIAN_POINT('Ctrl Pts',(30.4483551673175,618.710565160562,-35.3805668582694)) ;
#65118 = CARTESIAN_POINT('Ctrl Pts',(30.4363904345703,618.710565160562,-35.3750149874902)) ;
#65119 = CARTESIAN_POINT('Ctrl Pts',(30.4243544886558,618.710565160562,-35.3695905233535)) ;
#65120 = CARTESIAN_POINT('Ctrl Pts',(30.412269259522,618.710565160562,-35.3643024486773)) ;
#65121 = CARTESIAN_POINT('Ctrl Pts',(30.3509280970973,618.710565160562,-35.3374616958843)) ;
#65122 = CARTESIAN_POINT('Ctrl Pts',(30.2882099920363,618.710565160562,-35.3140793129021)) ;
#65123 = CARTESIAN_POINT('Ctrl Pts',(30.2244743219518,618.710565160562,-35.294176343009)) ;
#65124 = CARTESIAN_POINT('Ctrl Pts',(30.1593907420887,618.710565160562,-35.2738524564187)) ;
#65125 = CARTESIAN_POINT('Ctrl Pts',(30.0932452692249,618.710565160562,-35.2571561292323)) ;
#65126 = CARTESIAN_POINT('Ctrl Pts',(30.026383639428,618.710565160562,-35.2441495216079)) ;
#65127 = CARTESIAN_POINT('Ctrl Pts',(29.9706599072117,618.710565160562,-35.233309571662)) ;
#65128 = CARTESIAN_POINT('Ctrl Pts',(29.9144377890335,618.710565160562,-35.2250330262529)) ;
#65129 = CARTESIAN_POINT('Ctrl Pts',(29.8579051586923,618.710565160562,-35.2193806515948)) ;
#65130 = CARTESIAN_POINT('Ctrl Pts',(29.8316943845793,618.710565160562,-35.2167599860699)) ;
#65131 = CARTESIAN_POINT('Ctrl Pts',(29.8054167484692,618.710565160562,-35.2147037537742)) ;
#65132 = CARTESIAN_POINT('Ctrl Pts',(29.7790905690437,618.710565160562,-35.2132198434095)) ;
#65133 = CARTESIAN_POINT('Ctrl Pts',(29.7677516535389,618.710565160562,-35.2125807102497)) ;
#65134 = CARTESIAN_POINT('Ctrl Pts',(29.7564043220059,618.710565160562,-35.2120478819763)) ;
#65135 = CARTESIAN_POINT('Ctrl Pts',(29.745063524007,618.710565160562,-35.2116222778698)) ;
#65136 = CARTESIAN_POINT('Ctrl Pts',(29.6748763277332,618.710565160562,-35.2089882516788)) ;
#65137 = CARTESIAN_POINT('Ctrl Pts',(29.6048086763084,618.710565160562,-35.2104493210499)) ;
#65138 = CARTESIAN_POINT('Ctrl Pts',(29.5352239666675,618.710565160562,-35.2160576802378)) ;
#65139 = CARTESIAN_POINT('Ctrl Pts',(29.4726577330004,618.710565160562,-35.2211003672482)) ;
#65140 = CARTESIAN_POINT('Ctrl Pts',(29.4104809593564,618.710565160563,-35.2294962498139)) ;
#65141 = CARTESIAN_POINT('Ctrl Pts',(29.3489454561395,618.710565160563,-35.2413170737421)) ;
#65142 = CARTESIAN_POINT('Ctrl Pts',(29.2822479435602,618.710565160563,-35.2541295074014)) ;
#65143 = CARTESIAN_POINT('Ctrl Pts',(29.2163029514434,618.710565160563,-35.2709645531108)) ;
#65144 = CARTESIAN_POINT('Ctrl Pts',(29.1513226566763,618.710565160563,-35.2915780798982)) ;
#65145 = CARTESIAN_POINT('Ctrl Pts',(29.1265180515532,618.710565160563,-35.2994467790783)) ;
#65146 = CARTESIAN_POINT('Ctrl Pts',(29.1018540653138,618.710565160563,-35.3078665994065)) ;
#65147 = CARTESIAN_POINT('Ctrl Pts',(29.0773428165287,618.710565160563,-35.3168258983797)) ;
#65148 = CARTESIAN_POINT('Ctrl Pts',(29.0665475612047,618.710565160563,-35.3207717569031)) ;
#65149 = CARTESIAN_POINT('Ctrl Pts',(29.055782928172,618.710565160563,-35.3248219940153)) ;
#65150 = CARTESIAN_POINT('Ctrl Pts',(29.0450618450274,618.710565160563,-35.3289707620551)) ;
#65151 = CARTESIAN_POINT('Ctrl Pts',(28.9798075371171,618.710565160563,-35.3542224071978)) ;
#65152 = CARTESIAN_POINT('Ctrl Pts',(28.9160488162804,618.710565160563,-35.3831621836307)) ;
#65153 = CARTESIAN_POINT('Ctrl Pts',(28.8540028587099,618.710565160563,-35.4154783248475)) ;
#65154 = CARTESIAN_POINT('Ctrl Pts',(28.7905349461042,618.710565160563,-35.448535079982)) ;
#65155 = CARTESIAN_POINT('Ctrl Pts',(28.7288583842423,618.710565160563,-35.4851250339393)) ;
#65156 = CARTESIAN_POINT('Ctrl Pts',(28.6692095221533,618.710565160563,-35.5249705780916)) ;
#65157 = CARTESIAN_POINT('Ctrl Pts',(28.6089722266453,618.710565160563,-35.5652091967965)) ;
#65158 = CARTESIAN_POINT('Ctrl Pts',(28.5508019236201,618.710565160563,-35.6087684304393)) ;
#65159 = CARTESIAN_POINT('Ctrl Pts',(28.4949591104778,618.710565160563,-35.6554128189863)) ;
#65160 = CARTESIAN_POINT('Ctrl Pts',(28.4831219231459,618.710565160563,-35.6653001855809)) ;
#65161 = CARTESIAN_POINT('Ctrl Pts',(28.4713894054236,618.710565160563,-35.6753263402784)) ;
#65162 = CARTESIAN_POINT('Ctrl Pts',(28.4597641973492,618.710565160563,-35.68548929546)) ;
#65163 = CARTESIAN_POINT('Ctrl Pts',(28.4500414342721,618.710565160563,-35.6939891007762)) ;
#65164 = CARTESIAN_POINT('Ctrl Pts',(28.440392041099,618.710565160563,-35.702586139205)) ;
#65165 = CARTESIAN_POINT('Ctrl Pts',(28.430823120432,618.710565160563,-35.7112742631367)) ;
#65166 = CARTESIAN_POINT('Ctrl Pts',(28.3755127664173,618.710565160563,-35.7614934286106)) ;
#65167 = CARTESIAN_POINT('Ctrl Pts',(28.3230188069169,618.710565160563,-35.8146323668433)) ;
#65168 = CARTESIAN_POINT('Ctrl Pts',(28.2736003531469,618.710565160563,-35.870403376926)) ;
#65169 = CARTESIAN_POINT('Ctrl Pts',(28.2341986630398,618.710565160563,-35.9148700060615)) ;
#65170 = CARTESIAN_POINT('Ctrl Pts',(28.1967521325585,618.710565160563,-35.9610110047264)) ;
#65171 = CARTESIAN_POINT('Ctrl Pts',(28.1614036766299,618.710565160563,-36.00870124493)) ;
#65172 = CARTESIAN_POINT('Ctrl Pts',(28.1492849977504,618.710565160563,-36.0250511162762)) ;
#65173 = CARTESIAN_POINT('Ctrl Pts',(28.1374130297479,618.710565160563,-36.0415832216434)) ;
#65174 = CARTESIAN_POINT('Ctrl Pts',(28.1257939169347,618.710565160563,-36.0582929435484)) ;
#65175 = CARTESIAN_POINT('Ctrl Pts',(28.1169942611476,618.710565160563,-36.070947937387)) ;
#65176 = CARTESIAN_POINT('Ctrl Pts',(28.1083425954881,618.710565160563,-36.0837006692725)) ;
#65177 = CARTESIAN_POINT('Ctrl Pts',(28.0998456901819,618.710565160563,-36.0965421634147)) ;
#65178 = CARTESIAN_POINT('Ctrl Pts',(28.0582883984916,618.710565160563,-36.1593482908903)) ;
#65179 = CARTESIAN_POINT('Ctrl Pts',(28.0203973528173,618.710565160563,-36.2243220061981)) ;
#65180 = CARTESIAN_POINT('Ctrl Pts',(27.9864488831358,618.710565160563,-36.2912019953229)) ;
#65181 = CARTESIAN_POINT('Ctrl Pts',(27.9590223508319,618.710565160563,-36.3452334789043)) ;
#65182 = CARTESIAN_POINT('Ctrl Pts',(27.9341693434085,618.710565160563,-36.4005101339978)) ;
#65183 = CARTESIAN_POINT('Ctrl Pts',(27.9120539095342,618.710565160563,-36.4569110249402)) ;
#65184 = CARTESIAN_POINT('Ctrl Pts',(27.9079385582216,618.710565160563,-36.4674063867718)) ;
#65185 = CARTESIAN_POINT('Ctrl Pts',(27.9039180571055,618.710565160563,-36.4779407140531)) ;
#65186 = CARTESIAN_POINT('Ctrl Pts',(27.8999920534665,618.710565160563,-36.4885128439382)) ;
#65187 = CARTESIAN_POINT('',(30.969436549502,618.711435750373,-38.2922703312628)) ;
#65188 = CARTESIAN_POINT('Ctrl Pts',(27.9033532997491,618.710565160563,-37.5523303889371)) ;
#65189 = CARTESIAN_POINT('Ctrl Pts',(27.9288862972234,618.710565160563,-37.6212894872279)) ;
#65190 = CARTESIAN_POINT('Ctrl Pts',(27.9583601267478,618.710565160563,-37.6885283764075)) ;
#65191 = CARTESIAN_POINT('Ctrl Pts',(27.9914734180815,618.710565160563,-37.7538561924087)) ;
#65192 = CARTESIAN_POINT('Ctrl Pts',(28.0253525646813,618.710565160563,-37.8206949319665)) ;
#65193 = CARTESIAN_POINT('Ctrl Pts',(28.0630422037844,618.710565160563,-37.8855339267015)) ;
#65194 = CARTESIAN_POINT('Ctrl Pts',(28.1042643880468,618.710565160563,-37.9481374667155)) ;
#65195 = CARTESIAN_POINT('Ctrl Pts',(28.1389437182194,618.710565160563,-38.0008044680635)) ;
#65196 = CARTESIAN_POINT('Ctrl Pts',(28.1761242586142,618.710565160563,-38.0518889788485)) ;
#65197 = CARTESIAN_POINT('Ctrl Pts',(28.2156582418674,618.710565160563,-38.1012282656295)) ;
#65198 = CARTESIAN_POINT('Ctrl Pts',(28.233292464534,618.710565160563,-38.123236166117)) ;
#65199 = CARTESIAN_POINT('Ctrl Pts',(28.2513951108522,618.710565160563,-38.1448965329139)) ;
#65200 = CARTESIAN_POINT('Ctrl Pts',(28.2699537842564,618.710565160563,-38.1661933798041)) ;
#65201 = CARTESIAN_POINT('Ctrl Pts',(28.2801231194327,618.710565160563,-38.177863113384)) ;
#65202 = CARTESIAN_POINT('Ctrl Pts',(28.2904293858722,618.710565160563,-38.1894236804798)) ;
#65203 = CARTESIAN_POINT('Ctrl Pts',(28.3008705848837,618.710565160563,-38.2008723184176)) ;
#65204 = CARTESIAN_POINT('Ctrl Pts',(28.3105743611267,618.710565160563,-38.21151238195)) ;
#65205 = CARTESIAN_POINT('Ctrl Pts',(28.3203962779074,618.710565160563,-38.2220572825773)) ;
#65206 = CARTESIAN_POINT('Ctrl Pts',(28.3303190704187,618.710565160563,-38.232488726747)) ;
#65207 = CARTESIAN_POINT('Ctrl Pts',(28.3808070646547,618.710565160563,-38.2855647829586)) ;
#65208 = CARTESIAN_POINT('Ctrl Pts',(28.4339877215713,618.710565160563,-38.3358008763694)) ;
#65209 = CARTESIAN_POINT('Ctrl Pts',(28.4895980151892,618.710565160563,-38.3829789282195)) ;
#65210 = CARTESIAN_POINT('Ctrl Pts',(28.5443605121329,618.710565160563,-38.4294377356122)) ;
#65211 = CARTESIAN_POINT('Ctrl Pts',(28.6014800276728,618.710565160563,-38.4729314705988)) ;
#65212 = CARTESIAN_POINT('Ctrl Pts',(28.6607289931891,618.710565160563,-38.5132082911547)) ;
#65213 = CARTESIAN_POINT('Ctrl Pts',(28.710909637196,618.710565160563,-38.5473205625916)) ;
#65214 = CARTESIAN_POINT('Ctrl Pts',(28.7626184193456,618.710565160563,-38.5791247261134)) ;
#65215 = CARTESIAN_POINT('Ctrl Pts',(28.8157237359714,618.710565160563,-38.6084392126371)) ;
#65216 = CARTESIAN_POINT('Ctrl Pts',(28.8375733334271,618.710565160563,-38.6205003351548)) ;
#65217 = CARTESIAN_POINT('Ctrl Pts',(28.8596593778976,618.710565160563,-38.6321396712192)) ;
#65218 = CARTESIAN_POINT('Ctrl Pts',(28.8819727809855,618.710565160563,-38.6433431382079)) ;
#65219 = CARTESIAN_POINT('Ctrl Pts',(28.8923815922453,618.710565160563,-38.6485693590977)) ;
#65220 = CARTESIAN_POINT('Ctrl Pts',(28.9028398779815,618.710565160563,-38.6537007199305)) ;
#65221 = CARTESIAN_POINT('Ctrl Pts',(28.913346713321,618.710565160563,-38.6587357250361)) ;
#65222 = CARTESIAN_POINT('Ctrl Pts',(28.9241815639023,618.710565160563,-38.6639279190919)) ;
#65223 = CARTESIAN_POINT('Ctrl Pts',(28.9350604028915,618.710565160563,-38.6690139576571)) ;
#65224 = CARTESIAN_POINT('Ctrl Pts',(28.9459783961876,618.710565160563,-38.6739910342067)) ;
#65225 = CARTESIAN_POINT('Ctrl Pts',(29.0085873058914,618.710565160563,-38.7025319325049)) ;
#65226 = CARTESIAN_POINT('Ctrl Pts',(29.0725217509502,618.710565160562,-38.7275123221109)) ;
#65227 = CARTESIAN_POINT('Ctrl Pts',(29.1375740146656,618.710565160562,-38.7487091191263)) ;
#65228 = CARTESIAN_POINT('Ctrl Pts',(29.1969492541683,618.710565160562,-38.7680560999629)) ;
#65229 = CARTESIAN_POINT('Ctrl Pts',(29.2572563340101,618.710565160563,-38.7842507710163)) ;
#65230 = CARTESIAN_POINT('Ctrl Pts',(29.31834212105,618.710565160563,-38.7970858349689)) ;
#65231 = CARTESIAN_POINT('Ctrl Pts',(29.3901389193237,618.710565160562,-38.8121714472215)) ;
#65232 = CARTESIAN_POINT('Ctrl Pts',(29.4630129701239,618.710565160562,-38.8226165274978)) ;
#65233 = CARTESIAN_POINT('Ctrl Pts',(29.5365428627453,618.710565160562,-38.8284960853624)) ;
#65234 = CARTESIAN_POINT('Ctrl Pts',(29.5528541311509,618.710565160562,-38.8298003582644)) ;
#65235 = CARTESIAN_POINT('Ctrl Pts',(29.5691975890634,618.710565160562,-38.8308797372017)) ;
#65236 = CARTESIAN_POINT('Ctrl Pts',(29.5855684658677,618.710565160562,-38.8317346617483)) ;
#65237 = CARTESIAN_POINT('Ctrl Pts',(29.6015945658302,618.710565160562,-38.8325715812613)) ;
#65238 = CARTESIAN_POINT('Ctrl Pts',(29.6176522398986,618.710565160562,-38.8331933981503)) ;
#65239 = CARTESIAN_POINT('Ctrl Pts',(29.6337057677761,618.710565160562,-38.833600024665)) ;
#65240 = CARTESIAN_POINT('Ctrl Pts',(29.7023301789556,618.710565160562,-38.8353382410466)) ;
#65241 = CARTESIAN_POINT('Ctrl Pts',(29.7709730308323,618.710565160562,-38.8331560000629)) ;
#65242 = CARTESIAN_POINT('Ctrl Pts',(29.8392972346922,618.710565160562,-38.827174441035)) ;
#65243 = CARTESIAN_POINT('Ctrl Pts',(29.9074499692971,618.710565160562,-38.8212078935756)) ;
#65244 = CARTESIAN_POINT('Ctrl Pts',(29.9752867105702,618.710565160562,-38.8114606021859)) ;
#65245 = CARTESIAN_POINT('Ctrl Pts',(30.0424578652503,618.710565160562,-38.7980033675824)) ;
#65246 = CARTESIAN_POINT('Ctrl Pts',(30.0916234690244,618.710565160562,-38.7881534094038)) ;
#65247 = CARTESIAN_POINT('Ctrl Pts',(30.140432237142,618.710565160562,-38.7763148247249)) ;
#65248 = CARTESIAN_POINT('Ctrl Pts',(30.1887370875502,618.710565160562,-38.762500677227)) ;
#65249 = CARTESIAN_POINT('Ctrl Pts',(30.2087119349343,618.710565160562,-38.7567883008159)) ;
#65250 = CARTESIAN_POINT('Ctrl Pts',(30.2286004920296,618.710565160562,-38.750737974188)) ;
#65251 = CARTESIAN_POINT('Ctrl Pts',(30.248391786102,618.710565160562,-38.744350063234)) ;
#65252 = CARTESIAN_POINT('Ctrl Pts',(30.263078162565,618.710565160562,-38.7396098342859)) ;
#65253 = CARTESIAN_POINT('Ctrl Pts',(30.2777109734449,618.710565160562,-38.7346837055941)) ;
#65254 = CARTESIAN_POINT('Ctrl Pts',(30.292285597272,618.710565160562,-38.7295717182766)) ;
#65255 = CARTESIAN_POINT('Ctrl Pts',(30.3045536459369,618.710565160562,-38.7252687523868)) ;
#65256 = CARTESIAN_POINT('Ctrl Pts',(30.3167724999768,618.710565160562,-38.7208368658164)) ;
#65257 = CARTESIAN_POINT('Ctrl Pts',(30.3289362292424,618.710565160562,-38.716277854615)) ;
#65258 = CARTESIAN_POINT('Ctrl Pts',(30.3905960186477,618.710565160562,-38.6931675350383)) ;
#65259 = CARTESIAN_POINT('Ctrl Pts',(30.4508709911739,618.710565160562,-38.666783438768)) ;
#65260 = CARTESIAN_POINT('Ctrl Pts',(30.5094290049217,618.710565160562,-38.6371757693896)) ;
#65261 = CARTESIAN_POINT('Ctrl Pts',(30.5508896963081,618.710565160562,-38.6162127215639)) ;
#65262 = CARTESIAN_POINT('Ctrl Pts',(30.5914891470767,618.710565160562,-38.5936328280989)) ;
#65263 = CARTESIAN_POINT('Ctrl Pts',(30.6310978718703,618.710565160562,-38.5694432608945)) ;
#65264 = CARTESIAN_POINT('Ctrl Pts',(30.6437504598953,618.710565160562,-38.5617161596072)) ;
#65265 = CARTESIAN_POINT('Ctrl Pts',(30.6563037601999,618.710565160562,-38.5538235125602)) ;
#65266 = CARTESIAN_POINT('Ctrl Pts',(30.6687472063364,618.710565160562,-38.5457693443873)) ;
#65267 = CARTESIAN_POINT('Ctrl Pts',(30.7216837718687,618.710565160562,-38.5115055241707)) ;
#65268 = CARTESIAN_POINT('Ctrl Pts',(30.7725374966231,618.710565160562,-38.4743855832958)) ;
#65269 = CARTESIAN_POINT('Ctrl Pts',(30.8209947969149,618.710565160562,-38.4344437646062)) ;
#65270 = CARTESIAN_POINT('Ctrl Pts',(30.8661371617876,618.710565160562,-38.3972343422465)) ;
#65271 = CARTESIAN_POINT('Ctrl Pts',(30.9091999248329,618.710565160562,-38.3575753566552)) ;
#65272 = CARTESIAN_POINT('Ctrl Pts',(30.9498953849965,618.710565160562,-38.3154722432163)) ;
#65273 = CARTESIAN_POINT('Ctrl Pts',(30.9568438963168,618.710565160562,-38.3082833833491)) ;
#65274 = CARTESIAN_POINT('Ctrl Pts',(30.9637233028815,618.710565160562,-38.301023222749)) ;
#65275 = CARTESIAN_POINT('Ctrl Pts',(30.9705330870232,618.710565160562,-38.2936929952148)) ;
#65276 = CARTESIAN_POINT('Ctrl Pts',(30.9682724688976,618.711435750373,-38.2909024911338)) ;
#65277 = CARTESIAN_POINT('Ctrl Pts',(30.9740776063841,618.711145553769,-38.2859621126416)) ;
#65278 = CARTESIAN_POINT('Ctrl Pts',(30.9798488362412,618.710855357166,-38.2809818913689)) ;
#65279 = CARTESIAN_POINT('Ctrl Pts',(30.9855856147846,618.710565160562,-38.2759622964822)) ;
#65280 = CARTESIAN_POINT('Ctrl Pts',(180.967886278469,618.710565160535,-35.7530892919063)) ;
#65281 = CARTESIAN_POINT('Ctrl Pts',(180.925656002869,618.710565160535,-35.7078212532777)) ;
#65282 = CARTESIAN_POINT('Ctrl Pts',(180.880851236392,618.710565160535,-35.6652868410807)) ;
#65283 = CARTESIAN_POINT('Ctrl Pts',(180.833818101144,618.710565160535,-35.6254822445482)) ;
#65284 = CARTESIAN_POINT('Ctrl Pts',(180.783557499346,618.710565160535,-35.5829462119081)) ;
#65285 = CARTESIAN_POINT('Ctrl Pts',(180.730751994801,618.710565160535,-35.5435267603272)) ;
#65286 = CARTESIAN_POINT('Ctrl Pts',(180.675768818775,618.710565160535,-35.507248385621)) ;
#65287 = CARTESIAN_POINT('Ctrl Pts',(180.627658539752,618.710565160535,-35.4755048077531)) ;
#65288 = CARTESIAN_POINT('Ctrl Pts',(180.577879742994,618.710565160535,-35.4461663668647)) ;
#65289 = CARTESIAN_POINT('Ctrl Pts',(180.5266506585,618.710565160535,-35.4192725627713)) ;
#65290 = CARTESIAN_POINT('Ctrl Pts',(180.500908854801,618.710565160535,-35.4057588521023)) ;
#65291 = CARTESIAN_POINT('Ctrl Pts',(180.474800508004,618.710565160535,-35.3928627527034)) ;
#65292 = CARTESIAN_POINT('Ctrl Pts',(180.448351441031,618.710565160535,-35.3805916458249)) ;
#65293 = CARTESIAN_POINT('Ctrl Pts',(180.436382104309,618.710565160535,-35.3750384438792)) ;
#65294 = CARTESIAN_POINT('Ctrl Pts',(180.424341484995,618.710565160535,-35.3696127401546)) ;
#65295 = CARTESIAN_POINT('Ctrl Pts',(180.412251536294,618.710565160535,-35.3643235246544)) ;
#65296 = CARTESIAN_POINT('Ctrl Pts',(180.350909936507,618.710565160535,-35.3374872701404)) ;
#65297 = CARTESIAN_POINT('Ctrl Pts',(180.288191225939,618.710565160536,-35.3141092617675)) ;
#65298 = CARTESIAN_POINT('Ctrl Pts',(180.224454861394,618.710565160536,-35.2942104227471)) ;
#65299 = CARTESIAN_POINT('Ctrl Pts',(180.159558087471,618.710565160536,-35.2739492976196)) ;
#65300 = CARTESIAN_POINT('Ctrl Pts',(180.093605424765,618.710565160535,-35.257294627986)) ;
#65301 = CARTESIAN_POINT('Ctrl Pts',(180.026939752979,618.710565160535,-35.2443078456473)) ;
#65302 = CARTESIAN_POINT('Ctrl Pts',(179.971019742292,618.710565160535,-35.2334143679739)) ;
#65303 = CARTESIAN_POINT('Ctrl Pts',(179.914597108006,618.710565160536,-35.2251021895574)) ;
#65304 = CARTESIAN_POINT('Ctrl Pts',(179.857861807401,618.710565160536,-35.2194326090212)) ;
#65305 = CARTESIAN_POINT('Ctrl Pts',(179.831652792875,618.710565160536,-35.2168135320613)) ;
#65306 = CARTESIAN_POINT('Ctrl Pts',(179.805376940538,618.710565160536,-35.214758725493)) ;
#65307 = CARTESIAN_POINT('Ctrl Pts',(179.779052569468,618.710565160536,-35.2132760679416)) ;
#65308 = CARTESIAN_POINT('Ctrl Pts',(179.767709862447,618.710565160536,-35.2126372169631)) ;
#65309 = CARTESIAN_POINT('Ctrl Pts',(179.756358720358,618.710565160536,-35.2121047236115)) ;
#65310 = CARTESIAN_POINT('Ctrl Pts',(179.745014120561,618.710565160536,-35.2116795079059)) ;
#65311 = CARTESIAN_POINT('Ctrl Pts',(179.674822878097,618.710565160536,-35.2090486157432)) ;
#65312 = CARTESIAN_POINT('Ctrl Pts',(179.604751323395,618.710565160536,-35.2105125865917)) ;
#65313 = CARTESIAN_POINT('Ctrl Pts',(179.535162987157,618.710565160536,-35.2161234898321)) ;
#65314 = CARTESIAN_POINT('Ctrl Pts',(179.472586177512,618.710565160536,-35.2211690541175)) ;
#65315 = CARTESIAN_POINT('Ctrl Pts',(179.410399142565,618.710565160536,-35.22956830857)) ;
#65316 = CARTESIAN_POINT('Ctrl Pts',(179.34885387623,618.710565160536,-35.2413929346126)) ;
#65317 = CARTESIAN_POINT('Ctrl Pts',(179.282151812096,618.710565160536,-35.254208330688)) ;
#65318 = CARTESIAN_POINT('Ctrl Pts',(179.216202716827,618.710565160536,-35.2710461175169)) ;
#65319 = CARTESIAN_POINT('Ctrl Pts',(179.151218726316,618.710565160536,-35.2916622027171)) ;
#65320 = CARTESIAN_POINT('Ctrl Pts',(179.12641429349,618.710565160536,-35.2995313762851)) ;
#65321 = CARTESIAN_POINT('Ctrl Pts',(179.101750521018,618.710565160536,-35.307951574045)) ;
#65322 = CARTESIAN_POINT('Ctrl Pts',(179.07723952307,618.710565160536,-35.3169111578168)) ;
#65323 = CARTESIAN_POINT('Ctrl Pts',(179.06644408674,618.710565160536,-35.3208572483169)) ;
#65324 = CARTESIAN_POINT('Ctrl Pts',(179.055679281374,618.710565160536,-35.3249077051062)) ;
#65325 = CARTESIAN_POINT('Ctrl Pts',(179.044958034348,618.710565160536,-35.3290566806503)) ;
#65326 = CARTESIAN_POINT('Ctrl Pts',(178.979700192647,618.710565160536,-35.3543105702976)) ;
#65327 = CARTESIAN_POINT('Ctrl Pts',(178.915938366599,618.710565160536,-35.3832524293362)) ;
#65328 = CARTESIAN_POINT('Ctrl Pts',(178.853889686145,618.710565160536,-35.415570530269)) ;
#65329 = CARTESIAN_POINT('Ctrl Pts',(178.790419543132,618.710565160536,-35.4486290010233)) ;
#65330 = CARTESIAN_POINT('Ctrl Pts',(178.728741119599,618.710565160536,-35.485220480269)) ;
#65331 = CARTESIAN_POINT('Ctrl Pts',(178.669090714849,618.710565160536,-35.525067407697)) ;
#65332 = CARTESIAN_POINT('Ctrl Pts',(178.624018007635,618.710565160536,-35.5551763214728)) ;
#65333 = CARTESIAN_POINT('Ctrl Pts',(178.580103192787,618.710565160536,-35.5871451589576)) ;
#65334 = CARTESIAN_POINT('Ctrl Pts',(178.537454095892,618.710565160536,-35.6208728672108)) ;
#65335 = CARTESIAN_POINT('Ctrl Pts',(178.511025350192,618.710565160536,-35.641773216559)) ;
#65336 = CARTESIAN_POINT('Ctrl Pts',(178.485082760104,618.710565160536,-35.6633492815855)) ;
#65337 = CARTESIAN_POINT('Ctrl Pts',(178.459653562549,618.710565160536,-35.6855797374052)) ;
#65338 = CARTESIAN_POINT('Ctrl Pts',(178.449929967101,618.710565160536,-35.694080200644)) ;
#65339 = CARTESIAN_POINT('Ctrl Pts',(178.440279759941,618.710565160536,-35.7026779060663)) ;
#65340 = CARTESIAN_POINT('Ctrl Pts',(178.430710039992,618.710565160536,-35.7113667095423)) ;
#65341 = CARTESIAN_POINT('Ctrl Pts',(178.373903690972,618.710565160536,-35.7629438931444)) ;
#65342 = CARTESIAN_POINT('Ctrl Pts',(178.320068210137,618.710565160536,-35.8176004972375)) ;
#65343 = CARTESIAN_POINT('Ctrl Pts',(178.26948453935,618.710565160536,-35.8750256209584)) ;
#65344 = CARTESIAN_POINT('Ctrl Pts',(178.23154678626,618.710565160536,-35.918094463749)) ;
#65345 = CARTESIAN_POINT('Ctrl Pts',(178.195438361975,618.710565160536,-35.9627219017164)) ;
#65346 = CARTESIAN_POINT('Ctrl Pts',(178.161288298157,618.710565160536,-36.0087953897241)) ;
#65347 = CARTESIAN_POINT('Ctrl Pts',(178.149175580158,618.710565160536,-36.025137238174)) ;
#65348 = CARTESIAN_POINT('Ctrl Pts',(178.137309339071,618.710565160536,-36.0416611396476)) ;
#65349 = CARTESIAN_POINT('Ctrl Pts',(178.125695708976,618.710565160536,-36.0583624845284)) ;
#65350 = CARTESIAN_POINT('Ctrl Pts',(178.116898961978,618.710565160536,-36.0710129223538)) ;
#65351 = CARTESIAN_POINT('Ctrl Pts',(178.108250089833,618.710565160536,-36.0837610514211)) ;
#65352 = CARTESIAN_POINT('Ctrl Pts',(178.099755876389,618.710565160536,-36.0965978756731)) ;
#65353 = CARTESIAN_POINT('Ctrl Pts',(178.058197337227,618.710565160536,-36.1594029449052)) ;
#65354 = CARTESIAN_POINT('Ctrl Pts',(178.020305055465,618.710565160536,-36.2243756452309)) ;
#65355 = CARTESIAN_POINT('Ctrl Pts',(177.986355294698,618.710565160536,-36.2912547125809)) ;
#65356 = CARTESIAN_POINT('Ctrl Pts',(177.958920326772,618.710565160536,-36.3453000144096)) ;
#65357 = CARTESIAN_POINT('Ctrl Pts',(177.934060234432,618.710565160536,-36.4005912193201)) ;
#65358 = CARTESIAN_POINT('Ctrl Pts',(177.911939165789,618.710565160536,-36.457007322563)) ;
#65359 = CARTESIAN_POINT('Ctrl Pts',(177.907831226466,618.710565160536,-36.4674839379868)) ;
#65360 = CARTESIAN_POINT('Ctrl Pts',(177.903817797862,618.710565160574,-36.4779993817103)) ;
#65361 = CARTESIAN_POINT('Ctrl Pts',(177.899898529339,618.710565160544,-36.4885524971287)) ;
#65362 = CARTESIAN_POINT('',(180.969536013849,618.711452603529,-38.2922314065076)) ;
#65363 = CARTESIAN_POINT('Ctrl Pts',(177.90335329975,618.710565160536,-37.552330388949)) ;
#65364 = CARTESIAN_POINT('Ctrl Pts',(177.92875265027,618.710565160536,-37.6209285357504)) ;
#65365 = CARTESIAN_POINT('Ctrl Pts',(177.958052767198,618.710565160537,-37.6878243168137)) ;
#65366 = CARTESIAN_POINT('Ctrl Pts',(177.99095668214,618.710565160536,-37.7528299326183)) ;
#65367 = CARTESIAN_POINT('Ctrl Pts',(178.024804526857,618.710565160536,-37.8197003944861)) ;
#65368 = CARTESIAN_POINT('Ctrl Pts',(178.062466592364,618.710565160536,-37.8845714605626)) ;
#65369 = CARTESIAN_POINT('Ctrl Pts',(178.10366440299,618.710565160536,-37.9472075021294)) ;
#65370 = CARTESIAN_POINT('Ctrl Pts',(178.138518637012,618.710565160537,-38.0001989406988)) ;
#65371 = CARTESIAN_POINT('Ctrl Pts',(178.17590464559,618.710565160537,-38.051590324619)) ;
#65372 = CARTESIAN_POINT('Ctrl Pts',(178.215671915688,618.710565160536,-38.1012161461691)) ;
#65373 = CARTESIAN_POINT('Ctrl Pts',(178.233309628192,618.710565160536,-38.1232263563529)) ;
#65374 = CARTESIAN_POINT('Ctrl Pts',(178.251415944853,618.710565160536,-38.1448889538452)) ;
#65375 = CARTESIAN_POINT('Ctrl Pts',(178.269978455095,618.710565160536,-38.1661879483558)) ;
#65376 = CARTESIAN_POINT('Ctrl Pts',(178.280147809454,618.710565160536,-38.1778564683908)) ;
#65377 = CARTESIAN_POINT('Ctrl Pts',(178.290454088964,618.710565160536,-38.1894158417102)) ;
#65378 = CARTESIAN_POINT('Ctrl Pts',(178.300895293865,618.710565160536,-38.2008633066224)) ;
#65379 = CARTESIAN_POINT('Ctrl Pts',(178.310601431425,618.710565160536,-38.211504862862)) ;
#65380 = CARTESIAN_POINT('Ctrl Pts',(178.320425762691,618.710565160536,-38.222051229921)) ;
#65381 = CARTESIAN_POINT('Ctrl Pts',(178.330351013256,618.710565160536,-38.2324841072426)) ;
#65382 = CARTESIAN_POINT('Ctrl Pts',(178.380800128125,618.710565160536,-38.2855134411581)) ;
#65383 = CARTESIAN_POINT('Ctrl Pts',(178.433937571481,618.710565160536,-38.3357077319362)) ;
#65384 = CARTESIAN_POINT('Ctrl Pts',(178.489500808843,618.710565160536,-38.382849507741)) ;
#65385 = CARTESIAN_POINT('Ctrl Pts',(178.544743275573,618.710565160536,-38.4297191306276)) ;
#65386 = CARTESIAN_POINT('Ctrl Pts',(178.602384494608,618.710565160536,-38.4735719050078)) ;
#65387 = CARTESIAN_POINT('Ctrl Pts',(178.662190756132,618.710565160536,-38.5141491743324)) ;
#65388 = CARTESIAN_POINT('Ctrl Pts',(178.711939225079,618.710565160536,-38.5479024465072)) ;
#65389 = CARTESIAN_POINT('Ctrl Pts',(178.763186423315,618.710565160536,-38.5793886345307)) ;
#65390 = CARTESIAN_POINT('Ctrl Pts',(178.815804283139,618.710565160536,-38.6084310566786)) ;
#65391 = CARTESIAN_POINT('Ctrl Pts',(178.837655252695,618.710565160536,-38.6204916970072)) ;
#65392 = CARTESIAN_POINT('Ctrl Pts',(178.859742637093,618.710565160536,-38.632130576785)) ;
#65393 = CARTESIAN_POINT('Ctrl Pts',(178.882057340823,618.710565160536,-38.6433336153461)) ;
#65394 = CARTESIAN_POINT('Ctrl Pts',(178.892463777766,618.710565160536,-38.6485581397573)) ;
#65395 = CARTESIAN_POINT('Ctrl Pts',(178.902919652307,618.710565160536,-38.6536878644943)) ;
#65396 = CARTESIAN_POINT('Ctrl Pts',(178.913424039632,618.710565160536,-38.6587212953844)) ;
#65397 = CARTESIAN_POINT('Ctrl Pts',(178.924263143256,618.710565160536,-38.6639151136734)) ;
#65398 = CARTESIAN_POINT('Ctrl Pts',(178.93514626959,618.710565160536,-38.6690027184636)) ;
#65399 = CARTESIAN_POINT('Ctrl Pts',(178.946068559414,618.710565160536,-38.6739812913392)) ;
#65400 = CARTESIAN_POINT('Ctrl Pts',(179.008683124175,618.710565160536,-38.702522117372)) ;
#65401 = CARTESIAN_POINT('Ctrl Pts',(179.072622958707,618.710565160536,-38.7275024100009)) ;
#65402 = CARTESIAN_POINT('Ctrl Pts',(179.13768017974,618.710565160536,-38.7486990958925)) ;
#65403 = CARTESIAN_POINT('Ctrl Pts',(179.197059993512,618.710565160536,-38.7680459914542)) ;
#65404 = CARTESIAN_POINT('Ctrl Pts',(179.257371289354,618.710565160536,-38.7842405601685)) ;
#65405 = CARTESIAN_POINT('Ctrl Pts',(179.318460801853,618.710565160536,-38.7970755115389)) ;
#65406 = CARTESIAN_POINT('Ctrl Pts',(179.390261310164,618.710565160536,-38.8121608509833)) ;
#65407 = CARTESIAN_POINT('Ctrl Pts',(179.46313837298,618.710565160536,-38.8226057307213)) ;
#65408 = CARTESIAN_POINT('Ctrl Pts',(179.536670670084,618.710565160536,-38.82848514471)) ;
#65409 = CARTESIAN_POINT('Ctrl Pts',(179.552981982092,618.710565160536,-38.8297893465338)) ;
#65410 = CARTESIAN_POINT('Ctrl Pts',(179.569325451759,618.710565160536,-38.8308686706868)) ;
#65411 = CARTESIAN_POINT('Ctrl Pts',(179.585696309858,618.710565160536,-38.8317235565352)) ;
#65412 = CARTESIAN_POINT('Ctrl Pts',(179.601723236992,618.710565160536,-38.8325604823162)) ;
#65413 = CARTESIAN_POINT('Ctrl Pts',(179.617781712558,618.710565160536,-38.8331822982082)) ;
#65414 = CARTESIAN_POINT('Ctrl Pts',(179.633836014706,618.710565160536,-38.8335889163139)) ;
#65415 = CARTESIAN_POINT('Ctrl Pts',(179.70246178681,618.710565160536,-38.835327047389)) ;
#65416 = CARTESIAN_POINT('Ctrl Pts',(179.771105501388,618.710565160536,-38.8331448085213)) ;
#65417 = CARTESIAN_POINT('Ctrl Pts',(179.839430158321,618.710565160536,-38.8271633236124)) ;
#65418 = CARTESIAN_POINT('Ctrl Pts',(179.907568389827,618.710565160536,-38.8211981593254)) ;
#65419 = CARTESIAN_POINT('Ctrl Pts',(179.975390358138,618.710565160536,-38.8114539801615)) ;
#65420 = CARTESIAN_POINT('Ctrl Pts',(180.042546786254,618.710565160536,-38.7980015312525)) ;
#65421 = CARTESIAN_POINT('Ctrl Pts',(180.091727522222,618.710565160536,-38.7881498855279)) ;
#65422 = CARTESIAN_POINT('Ctrl Pts',(180.140551072165,618.710565160536,-38.7763084156596)) ;
#65423 = CARTESIAN_POINT('Ctrl Pts',(180.18887025211,618.710565160536,-38.7624901938655)) ;
#65424 = CARTESIAN_POINT('Ctrl Pts',(180.208844836146,618.710565160536,-38.7567779025399)) ;
#65425 = CARTESIAN_POINT('Ctrl Pts',(180.228733105885,618.710565160536,-38.7507276669264)) ;
#65426 = CARTESIAN_POINT('Ctrl Pts',(180.248524090962,618.710565160536,-38.7443398525418)) ;
#65427 = CARTESIAN_POINT('Ctrl Pts',(180.263213998755,618.710565160536,-38.7395984814609)) ;
#65428 = CARTESIAN_POINT('Ctrl Pts',(180.277850301612,618.710565160536,-38.7346711184834)) ;
#65429 = CARTESIAN_POINT('Ctrl Pts',(180.292428375474,618.710565160536,-38.7295578045955)) ;
#65430 = CARTESIAN_POINT('Ctrl Pts',(180.304694037984,618.710565160536,-38.7252555776313)) ;
#65431 = CARTESIAN_POINT('Ctrl Pts',(180.316910506913,618.710565160536,-38.720824480024)) ;
#65432 = CARTESIAN_POINT('Ctrl Pts',(180.329071866739,618.710565160536,-38.7162663029856)) ;
#65433 = CARTESIAN_POINT('Ctrl Pts',(180.390730875172,618.710565160536,-38.6931560027825)) ;
#65434 = CARTESIAN_POINT('Ctrl Pts',(180.451004861965,618.710565160536,-38.6667719293244)) ;
#65435 = CARTESIAN_POINT('Ctrl Pts',(180.509561757029,618.710565160536,-38.6371642734416)) ;
#65436 = CARTESIAN_POINT('Ctrl Pts',(180.551022103343,618.710565160536,-38.6162010091653)) ;
#65437 = CARTESIAN_POINT('Ctrl Pts',(180.591621123789,618.710565160536,-38.5936208597328)) ;
#65438 = CARTESIAN_POINT('Ctrl Pts',(180.631229354313,618.710565160536,-38.5694309926077)) ;
#65439 = CARTESIAN_POINT('Ctrl Pts',(180.643881857526,618.710565160536,-38.5617037508834)) ;
#65440 = CARTESIAN_POINT('Ctrl Pts',(180.656435066235,618.710565160536,-38.5538109563834)) ;
#65441 = CARTESIAN_POINT('Ctrl Pts',(180.668878411365,618.710565160536,-38.545756635812)) ;
#65442 = CARTESIAN_POINT('Ctrl Pts',(180.721813972028,618.710565160536,-38.511492539563)) ;
#65443 = CARTESIAN_POINT('Ctrl Pts',(180.772666608596,618.710565160536,-38.474372270941)) ;
#65444 = CARTESIAN_POINT('Ctrl Pts',(180.821122797544,618.710565160536,-38.434430061149)) ;
#65445 = CARTESIAN_POINT('Ctrl Pts',(180.866262830651,618.710565160536,-38.3972213430987)) ;
#65446 = CARTESIAN_POINT('Ctrl Pts',(180.909323361008,618.710565160536,-38.3575631474454)) ;
#65447 = CARTESIAN_POINT('Ctrl Pts',(180.950016762044,618.710565160536,-38.3154608990898)) ;
#65448 = CARTESIAN_POINT('Ctrl Pts',(180.956965088351,618.710565160536,-38.308272014593)) ;
#65449 = CARTESIAN_POINT('Ctrl Pts',(180.963844311663,618.710565160536,-38.3010118281384)) ;
#65450 = CARTESIAN_POINT('Ctrl Pts',(180.970653914223,618.710565160536,-38.2936815735458)) ;
#65451 = CARTESIAN_POINT('Ctrl Pts',(180.968349279596,618.711452603529,-38.2908371184949)) ;
#65452 = CARTESIAN_POINT('Ctrl Pts',(180.97426742378,618.711156789198,-38.2857999494516)) ;
#65453 = CARTESIAN_POINT('Ctrl Pts',(180.980150321186,618.710860974867,-38.2807213691574)) ;
#65454 = CARTESIAN_POINT('Ctrl Pts',(180.985997395766,618.710565160536,-38.2756018749041)) ;
#65455 = CARTESIAN_POINT('',(94.4385276254219,618.710565160551,-38.1221601717558)) ;
#65456 = CARTESIAN_POINT('',(99.688527624592,618.71056516055,-43.3721601717561)) ;
#65457 = CARTESIAN_POINT('Origin',(99.6885276254219,618.71056516055,-38.1221601717561)) ;
#65458 = CARTESIAN_POINT('',(122.688527625422,618.710565160546,-43.3721601717571)) ;
#65459 = CARTESIAN_POINT('',(122.688527625422,618.710565160546,-43.3721601717571)) ;
#65460 = CARTESIAN_POINT('',(127.938527625422,618.710565160545,-38.1221601724939)) ;
#65461 = CARTESIAN_POINT('Origin',(122.688527625422,618.710565160546,-38.1221601717571)) ;
#65462 = CARTESIAN_POINT('',(127.938527625423,618.710565160545,-24.1221601717574)) ;
#65463 = CARTESIAN_POINT('',(127.938527625423,618.710565160545,-24.1221601717574)) ;
#65464 = CARTESIAN_POINT('',(94.4385276254226,618.710565160551,-24.1221601717558)) ;
#65465 = CARTESIAN_POINT('',(94.4385276254226,618.710565160551,-24.1221601717558)) ;
#65466 = CARTESIAN_POINT('',(94.4385276254219,618.710565160551,-38.1221601717558)) ;
#65467 = CARTESIAN_POINT('',(21.3885276254223,618.710565160564,-30.2221601717525)) ;
#65468 = CARTESIAN_POINT('',(23.3885276254223,618.710565160563,-30.2221601717526)) ;
#65469 = CARTESIAN_POINT('',(21.3885276254223,618.710565160564,-30.2221601717525)) ;
#65470 = CARTESIAN_POINT('',(21.388527625422,618.710565160564,-37.2221601717525)) ;
#65471 = CARTESIAN_POINT('',(21.388527625422,618.710565160564,-37.2221601717525)) ;
#65472 = CARTESIAN_POINT('',(23.388527625422,618.710565160563,-37.2221601717526)) ;
#65473 = CARTESIAN_POINT('',(23.388527625422,618.710565160563,-37.2221601717526)) ;
#65474 = CARTESIAN_POINT('',(23.3885276254223,618.710565160563,-30.2221601717526)) ;
#65475 = CARTESIAN_POINT('',(36.3885276254223,618.710565160561,-30.2221601717532)) ;
#65476 = CARTESIAN_POINT('',(38.3885276254223,618.710565160561,-30.2221601717533)) ;
#65477 = CARTESIAN_POINT('',(36.3885276254223,618.710565160561,-30.2221601717532)) ;
#65478 = CARTESIAN_POINT('',(36.388527625422,618.710565160561,-37.2221601717532)) ;
#65479 = CARTESIAN_POINT('',(36.388527625422,618.710565160561,-37.2221601717532)) ;
#65480 = CARTESIAN_POINT('',(38.388527625422,618.710565160561,-37.2221601717533)) ;
#65481 = CARTESIAN_POINT('',(38.388527625422,618.710565160561,-37.2221601717533)) ;
#65482 = CARTESIAN_POINT('',(38.3885276254223,618.710565160561,-30.2221601717533)) ;
#65483 = CARTESIAN_POINT('',(171.388527625422,618.710565160537,-30.2221601717593)) ;
#65484 = CARTESIAN_POINT('',(173.388527625422,618.710565160537,-30.2221601717594)) ;
#65485 = CARTESIAN_POINT('',(171.388527625422,618.710565160537,-30.2221601717593)) ;
#65486 = CARTESIAN_POINT('',(171.388527625422,618.710565160537,-37.2221601717593)) ;
#65487 = CARTESIAN_POINT('',(171.388527625422,618.710565160537,-37.2221601717593)) ;
#65488 = CARTESIAN_POINT('',(173.388527625422,618.710565160537,-37.2221601717594)) ;
#65489 = CARTESIAN_POINT('',(173.388527625422,618.710565160537,-37.2221601717594)) ;
#65490 = CARTESIAN_POINT('',(173.388527625422,618.710565160537,-30.2221601717594)) ;
#65491 = CARTESIAN_POINT('',(186.388527625422,618.710565160535,-30.22216017176)) ;
#65492 = CARTESIAN_POINT('',(188.388527625422,618.710565160534,-30.2221601717601)) ;
#65493 = CARTESIAN_POINT('',(186.388527625422,618.710565160535,-30.22216017176)) ;
#65494 = CARTESIAN_POINT('',(186.388527625422,618.710565160535,-37.22216017176)) ;
#65495 = CARTESIAN_POINT('',(186.388527625422,618.710565160535,-37.22216017176)) ;
#65496 = CARTESIAN_POINT('',(188.388527625422,618.710565160534,-37.2221601717601)) ;
#65497 = CARTESIAN_POINT('',(188.388527625422,618.710565160534,-37.2221601717601)) ;
#65498 = CARTESIAN_POINT('',(188.388527625422,618.710565160534,-30.2221601717601)) ;
#65499 = CARTESIAN_POINT('',(187.378265783355,618.710565160534,-26.7703110636122)) ;
#65500 = CARTESIAN_POINT('Origin',(187.388264603423,618.710565160534,-24.0203292412001)) ;
#65501 = CARTESIAN_POINT('',(6.47826578335511,618.710565160566,-26.770311063604)) ;
#65502 = CARTESIAN_POINT('Origin',(6.48826460342255,618.710565160563,-24.0203292411918)) ;
#65503 = CARTESIAN_POINT('Origin',(0.388527634368701,620.552123681176,-48.4900362557631)) ;
#65504 = CARTESIAN_POINT('',(0.388527634368074,616.710565160567,-49.5221601717515)) ;
#65505 = CARTESIAN_POINT('Origin',(0.388527634368074,616.710565160567,-47.5221601717516)) ;
#65506 = CARTESIAN_POINT('',(0.388527634367972,616.077123681176,-49.5221601717516)) ;
#65507 = CARTESIAN_POINT('',(0.38852763435921,562.381344420871,-49.5221601717516)) ;
#65508 = CARTESIAN_POINT('',(0.38852763436797,616.077123681176,-48.4900362557631)) ;
#65509 = CARTESIAN_POINT('',(0.388527625421941,503.131344420871,-47.5221601717516)) ;
#65510 = CARTESIAN_POINT('',(0.388527634359032,561.302123681176,-43.4900362557631)) ;
#65511 = CARTESIAN_POINT('Origin',(-0.611472374578195,502.052123681177,-48.4900362557631)) ;
#65512 = CARTESIAN_POINT('',(-0.611472374577496,506.335123681177,-43.4900362557631)) ;
#65513 = CARTESIAN_POINT('',(-0.611472374577496,506.335123681177,-48.4900362557631)) ;
#65514 = CARTESIAN_POINT('',(-0.611472374559588,616.077123681177,-43.4900362557631)) ;
#65515 = CARTESIAN_POINT('',(-0.611472374559588,616.077123681177,-48.4900362557631)) ;
#65516 = CARTESIAN_POINT('',(-0.611472374559506,616.57735283115,-43.4900362557631)) ;
#65517 = CARTESIAN_POINT('',(-0.611472374578195,502.052123681177,-43.4900362557631)) ;
#65518 = CARTESIAN_POINT('',(-0.611472374559505,616.585559486892,-19.5221601717515)) ;
#65519 = CARTESIAN_POINT('Ctrl Pts',(-0.611472374559507,616.577352831186,
-43.4900362559989)) ;
#65520 = CARTESIAN_POINT('Ctrl Pts',(-0.611472374559485,616.580300554184,
-42.8711455790505)) ;
#65521 = CARTESIAN_POINT('Ctrl Pts',(-0.611472374559468,616.578645899186,
-42.2555490188023)) ;
#65522 = CARTESIAN_POINT('Ctrl Pts',(-0.611472374559405,616.576796842089,
-40.3433653577621)) ;
#65523 = CARTESIAN_POINT('Ctrl Pts',(-0.611472374559349,616.580239054546,
-39.0434564517781)) ;
#65524 = CARTESIAN_POINT('Ctrl Pts',(-0.61147237455923,616.584223500474,-36.4426213256376)) ;
#65525 = CARTESIAN_POINT('Ctrl Pts',(-0.611472374559168,616.584762379478,
-35.1426809282471)) ;
#65526 = CARTESIAN_POINT('Ctrl Pts',(-0.611472374558881,616.586580540637,
-29.0698861297919)) ;
#65527 = CARTESIAN_POINT('Ctrl Pts',(-0.611472374558661,616.585990493313,
-24.2959347172062)) ;
#65528 = CARTESIAN_POINT('Ctrl Pts',(-0.611472374558452,616.585559486892,
-19.5221601717825)) ;
#65529 = CARTESIAN_POINT('',(-0.611472374577577,505.835569713225,-19.5221601717515)) ;
#65530 = CARTESIAN_POINT('',(-0.611472374577774,504.632344420872,-19.5221601717515)) ;
#65531 = CARTESIAN_POINT('',(-0.611472374577577,505.835569713225,-43.4900362557631)) ;
#65532 = CARTESIAN_POINT('',(-0.611472374577577,505.835569713225,-47.7060982137573)) ;
#65533 = CARTESIAN_POINT('',(-0.611472374578195,502.052123681177,-43.4900362557631)) ;
#65534 = CARTESIAN_POINT('Origin',(-283.146192374579,616.710565160617,-47.5221601717387)) ;
#65535 = CARTESIAN_POINT('',(140.388527625421,616.710565160543,-49.5221601717579)) ;
#65536 = CARTESIAN_POINT('Origin',(140.388527625421,616.710565160543,-47.5221601717579)) ;
#65537 = CARTESIAN_POINT('',(-0.611472374578952,616.710565160567,-49.5221601717515)) ;
#65538 = CARTESIAN_POINT('Origin',(-283.146192374579,616.710565160617,-47.5221601717387)) ;
#65539 = CARTESIAN_POINT('',(205.668527625421,616.710565160531,-49.5221601717609)) ;
#65540 = CARTESIAN_POINT('',(-0.611472374578952,616.710565160567,-49.5221601717515)) ;
#65541 = CARTESIAN_POINT('Origin',(205.668527625421,616.710565160531,-47.5221601717609)) ;
#65542 = CARTESIAN_POINT('Origin',(-283.146192374598,505.710565160617,-47.5221601717387)) ;
#65543 = CARTESIAN_POINT('',(205.668527625402,505.710565160531,-49.5221601717609)) ;
#65544 = CARTESIAN_POINT('Origin',(205.668527625402,505.710565160531,-47.5221601717609)) ;
#65545 = CARTESIAN_POINT('',(-0.611472374598421,505.710565160567,-49.5221601717515)) ;
#65546 = CARTESIAN_POINT('Origin',(212.388527625402,506.21056516053,-47.0221601717613)) ;
#65547 = CARTESIAN_POINT('',(193.688527625402,506.210565160533,-47.5221601717604)) ;
#65548 = CARTESIAN_POINT('Origin',(193.688527625402,506.210565160533,-47.0221601717604)) ;
#65549 = CARTESIAN_POINT('',(0.388527630175977,506.210565160568,-47.5221601717516)) ;
#65550 = CARTESIAN_POINT('',(212.388527625402,506.210565160531,-47.5221601717613)) ;
#65551 = CARTESIAN_POINT('Origin',(0.388527634348712,506.210565160567,-47.0221601717516)) ;
#65552 = CARTESIAN_POINT('Origin',(-2.61147237459646,504.210565160568,0.477839828248552)) ;
#65553 = CARTESIAN_POINT('',(-2.61147237459865,503.131344420872,-43.4900362557631)) ;
#65554 = CARTESIAN_POINT('Origin',(-2.61147237459681,507.212565160568,-19.5221601717514)) ;
#65555 = CARTESIAN_POINT('',(-2.61147237457763,616.585559486893,-19.5221601717514)) ;
#65556 = CARTESIAN_POINT('',(-0.611472374559505,616.585559486893,-19.5221601717515)) ;
#65557 = CARTESIAN_POINT('',(-2.61147237459708,505.835569713225,-19.5221601717514)) ;
#65558 = CARTESIAN_POINT('',(-2.6114723745971,505.711565160568,-19.5221601717514)) ;
#65559 = CARTESIAN_POINT('',(-1.31147237459708,505.835569713225,-19.5221601717515)) ;
#65560 = CARTESIAN_POINT('Origin',(-0.0114723745983569,505.835569713225,-46.9221601717515)) ;
#65561 = CARTESIAN_POINT('',(-2.61147237459817,505.835569713225,-43.4900362557631)) ;
#65562 = CARTESIAN_POINT('',(-2.81147237458794,505.835569713225,-43.4900362557631)) ;
#65563 = CARTESIAN_POINT('',(-2.61147237459725,505.835569713225,-23.2221601717514)) ;
#65564 = CARTESIAN_POINT('Ctrl Pts',(-2.6427223745788,616.576179137963,-43.6993995739517)) ;
#65565 = CARTESIAN_POINT('Ctrl Pts',(0.327277625449208,616.576179137963,-43.6993995739518)) ;
#65566 = CARTESIAN_POINT('Ctrl Pts',(-2.6427223745788,616.576400591684,-43.6645773254828)) ;
#65567 = CARTESIAN_POINT('Ctrl Pts',(0.327277625449208,616.576400591684,-43.6645773254829)) ;
#65568 = CARTESIAN_POINT('Ctrl Pts',(-2.6427223745788,616.576612329461,-43.6297316873501)) ;
#65569 = CARTESIAN_POINT('Ctrl Pts',(0.327277625449208,616.576612329461,-43.6297316873502)) ;
#65570 = CARTESIAN_POINT('Ctrl Pts',(-2.6427223745788,616.576808621265,-43.5948637771549)) ;
#65571 = CARTESIAN_POINT('Ctrl Pts',(0.327277625449208,616.576808621265,-43.594863777155)) ;
#65572 = CARTESIAN_POINT('Ctrl Pts',(-2.6427223745788,616.577000756849,-43.5607341490021)) ;
#65573 = CARTESIAN_POINT('Ctrl Pts',(0.327277625449208,616.577000756849,-43.5607341490022)) ;
#65574 = CARTESIAN_POINT('Ctrl Pts',(-2.64272237457879,616.577177913241,-43.5266148439379)) ;
#65575 = CARTESIAN_POINT('Ctrl Pts',(0.327277625449218,616.577177913241,-43.526614843938)) ;
#65576 = CARTESIAN_POINT('Ctrl Pts',(-2.64272237457879,616.577341045865,-43.4925055365579)) ;
#65577 = CARTESIAN_POINT('Ctrl Pts',(0.327277625449218,616.577341045865,-43.492505536558)) ;
#65578 = CARTESIAN_POINT('Ctrl Pts',(-2.64272237457877,616.580304957246,-42.8727829948047)) ;
#65579 = CARTESIAN_POINT('Ctrl Pts',(0.327277625449238,616.580304957246,-42.8727829948048)) ;
#65580 = CARTESIAN_POINT('Ctrl Pts',(-2.64272237457875,616.578646689173,-42.2563659747035)) ;
#65581 = CARTESIAN_POINT('Ctrl Pts',(0.327277625449258,616.578646689173,-42.2563659747036)) ;
#65582 = CARTESIAN_POINT('Ctrl Pts',(-2.64272237457873,616.5780518982,-41.6412689173054)) ;
#65583 = CARTESIAN_POINT('Ctrl Pts',(0.327277625449278,616.5780518982,-41.6412689173055)) ;
#65584 = CARTESIAN_POINT('Ctrl Pts',(-2.64272237457869,616.576796842089,-40.343365357762)) ;
#65585 = CARTESIAN_POINT('Ctrl Pts',(0.327277625449318,616.576796842089,-40.3433653577621)) ;
#65586 = CARTESIAN_POINT('Ctrl Pts',(-2.64272237457863,616.580239054546,-39.043456451778)) ;
#65587 = CARTESIAN_POINT('Ctrl Pts',(0.327277625449378,616.580239054546,-39.0434564517781)) ;
#65588 = CARTESIAN_POINT('Ctrl Pts',(-2.64272237457858,616.58223127751,-37.7430388887073)) ;
#65589 = CARTESIAN_POINT('Ctrl Pts',(0.327277625449428,616.58223127751,-37.7430388887074)) ;
#65590 = CARTESIAN_POINT('Ctrl Pts',(-2.64272237457852,616.584223500474,-36.4426213256375)) ;
#65591 = CARTESIAN_POINT('Ctrl Pts',(0.327277625449487,616.584223500474,-36.4426213256376)) ;
#65592 = CARTESIAN_POINT('Ctrl Pts',(-2.64272237457845,616.584762379478,-35.1426809282471)) ;
#65593 = CARTESIAN_POINT('Ctrl Pts',(0.327277625449558,616.584762379478,-35.1426809282472)) ;
#65594 = CARTESIAN_POINT('Ctrl Pts',(-2.64272237457839,616.585151546832,-33.8428327434185)) ;
#65595 = CARTESIAN_POINT('Ctrl Pts',(0.327277625449618,616.585151546832,-33.8428327434186)) ;
#65596 = CARTESIAN_POINT('Ctrl Pts',(-2.64272237457817,616.586580545288,-29.0698705940761)) ;
#65597 = CARTESIAN_POINT('Ctrl Pts',(0.327277625449838,616.586580545288,-29.0698705940762)) ;
#65598 = CARTESIAN_POINT('Ctrl Pts',(-2.64272237457795,616.585990489473,-24.2959036392336)) ;
#65599 = CARTESIAN_POINT('Ctrl Pts',(0.327277625450058,616.585990489473,-24.2959036392337)) ;
#65600 = CARTESIAN_POINT('Ctrl Pts',(-2.64272237457774,616.585559482684,-19.5221135565507)) ;
#65601 = CARTESIAN_POINT('Ctrl Pts',(0.327277625450268,616.585559482684,-19.5221135565508)) ;
#65602 = CARTESIAN_POINT('Ctrl Pts',(-2.64272237457773,616.585553230033,-19.4528597904909)) ;
#65603 = CARTESIAN_POINT('Ctrl Pts',(0.327277625450278,616.585553230033,-19.452859790491)) ;
#65604 = CARTESIAN_POINT('Ctrl Pts',(-2.64272237457773,616.585547010851,-19.3836060616588)) ;
#65605 = CARTESIAN_POINT('Ctrl Pts',(0.327277625450278,616.585547010851,-19.3836060616589)) ;
#65606 = CARTESIAN_POINT('Ctrl Pts',(-2.64272237457773,616.585540831787,-19.3143523736628)) ;
#65607 = CARTESIAN_POINT('Ctrl Pts',(0.327277625450278,616.585540831787,-19.3143523736629)) ;
#65608 = CARTESIAN_POINT('',(-2.61147237457872,616.57735283115,-43.4900362557631)) ;
#65609 = CARTESIAN_POINT('',(-0.611472374559506,616.57735283115,-43.4900362557633)) ;
#65610 = CARTESIAN_POINT('Ctrl Pts',(-2.61147237457763,616.585559486893,-19.5221601717514)) ;
#65611 = CARTESIAN_POINT('Ctrl Pts',(-2.61147237457784,616.585990493314,-24.2959347171855)) ;
#65612 = CARTESIAN_POINT('Ctrl Pts',(-2.61147237457806,616.586580540637,-29.0698861297815)) ;
#65613 = CARTESIAN_POINT('Ctrl Pts',(-2.61147237457834,616.584762379478,-35.1426809282471)) ;
#65614 = CARTESIAN_POINT('Ctrl Pts',(-2.61147237457841,616.584223500474,-36.4426213256375)) ;
#65615 = CARTESIAN_POINT('Ctrl Pts',(-2.61147237457852,616.580239054546,-39.043456451778)) ;
#65616 = CARTESIAN_POINT('Ctrl Pts',(-2.61147237457858,616.576796842089,-40.343365357762)) ;
#65617 = CARTESIAN_POINT('Ctrl Pts',(-2.61147237457864,616.578645899187,-42.2555490187243)) ;
#65618 = CARTESIAN_POINT('Ctrl Pts',(-2.61147237457866,616.580300554185,-42.8711455788942)) ;
#65619 = CARTESIAN_POINT('Ctrl Pts',(-2.61147237457868,616.577352831188,-43.4900362557634)) ;
#65620 = CARTESIAN_POINT('Origin',(-5.6114723745782,502.052123681177,-43.4900362557631)) ;
#65621 = CARTESIAN_POINT('',(-2.61147237459808,506.335123681177,-43.4900362557631)) ;
#65622 = CARTESIAN_POINT('',(-5.61147237457748,506.335123681177,-43.4900362557631)) ;
#65623 = CARTESIAN_POINT('',(-2.61147237459865,503.131344420872,-43.4900362557631)) ;
#65624 = CARTESIAN_POINT('Origin',(-5.61147237457746,506.335123681177,-48.4900362557631)) ;
#65625 = CARTESIAN_POINT('',(0.388527634350065,506.335123681176,-49.5221601717516)) ;
#65626 = CARTESIAN_POINT('',(103.388527625412,506.33512368116,-49.5221601717563)) ;
#65627 = CARTESIAN_POINT('',(0.388527634350062,506.335123681176,-48.4900362557631)) ;
#65628 = CARTESIAN_POINT('',(-2.6114723745972,506.335123681177,-24.0060982137574)) ;
#65629 = CARTESIAN_POINT('Origin',(0.388527634368701,620.552123681176,-48.4900362557631)) ;
#65630 = CARTESIAN_POINT('',(0.388527625421941,503.131344420871,-47.5221601717516)) ;
#65631 = CARTESIAN_POINT('',(0.388527634349961,505.710565160567,-49.5221601717516)) ;
#65632 = CARTESIAN_POINT('',(0.38852763435921,562.381344420871,-49.5221601717516)) ;
#65633 = CARTESIAN_POINT('Origin',(0.38852763434857,505.710565160567,-47.5221601717516)) ;
#65634 = CARTESIAN_POINT('',(0.388527634359032,561.302123681176,-43.4900362557631)) ;
#65635 = CARTESIAN_POINT('Origin',(-5.6114723745782,502.052123681177,-43.4900362557631)) ;
#65636 = CARTESIAN_POINT('Origin',(-5.6114723745782,502.052123681177,-43.4900362557631)) ;
#65637 = CARTESIAN_POINT('',(-2.61147237459865,503.131344420872,-43.4900362557631)) ;
#65638 = CARTESIAN_POINT('Origin',(-5.61147237457896,616.077123681177,-48.4900362557631)) ;
#65639 = CARTESIAN_POINT('',(103.38852762542,616.07712368116,-49.5221601717563)) ;
#65640 = CARTESIAN_POINT('',(-2.61147237457881,616.077123681177,-43.4900362557631)) ;
#65641 = CARTESIAN_POINT('',(-2.61147237457792,616.077123681177,-24.0060982137574)) ;
#65642 = CARTESIAN_POINT('',(-5.61147237456928,616.077123681177,-43.4900362557631)) ;
#65643 = CARTESIAN_POINT('Origin',(-5.6114723745782,502.052123681177,-43.4900362557631)) ;
#65644 = CARTESIAN_POINT('',(-2.61147237459865,503.131344420872,-43.4900362557631)) ;
#65645 = CARTESIAN_POINT('Origin',(174.388527625403,506.710565160537,-20.8221601717595)) ;
#65646 = CARTESIAN_POINT('',(173.388527625403,506.710565160537,-30.2221601717594)) ;
#65647 = CARTESIAN_POINT('Origin',(174.388527625403,506.710565160537,-30.2221601717595)) ;
#65648 = CARTESIAN_POINT('',(173.388527625403,506.710565160537,-25.7721601717594)) ;
#65649 = CARTESIAN_POINT('',(173.388527625403,506.710565160537,-20.8221601717595)) ;
#65650 = CARTESIAN_POINT('Origin',(174.388527625403,506.710565160537,-25.7721601717595)) ;
#65651 = CARTESIAN_POINT('Origin',(173.388527625402,504.210565160537,-42.1221601717595)) ;
#65652 = CARTESIAN_POINT('',(173.388527625403,506.960565160537,-30.2221601717594)) ;
#65653 = CARTESIAN_POINT('',(173.388527625403,506.210565160537,-30.2221601717594)) ;
#65654 = CARTESIAN_POINT('',(173.388527625403,506.960565160537,-25.7721601717594)) ;
#65655 = CARTESIAN_POINT('',(173.388527625402,506.960565160537,-45.8221601717595)) ;
#65656 = CARTESIAN_POINT('',(173.388527625403,506.210565160537,-25.7721601717594)) ;
#65657 = CARTESIAN_POINT('Origin',(84.9885276254035,506.710565160552,-11.8221601717554)) ;
#65658 = CARTESIAN_POINT('',(85.9885276254023,506.710565160552,-38.1221601717554)) ;
#65659 = CARTESIAN_POINT('Origin',(84.9885276254023,506.710565160552,-38.1221601717554)) ;
#65660 = CARTESIAN_POINT('',(85.9885276254028,506.710565160552,-25.7721601717555)) ;
#65661 = CARTESIAN_POINT('Origin',(84.9885276254028,506.710565160552,-25.7721601717554)) ;
#65662 = CARTESIAN_POINT('',(85.9885276254035,506.710565160552,-11.8221601717555)) ;
#65663 = CARTESIAN_POINT('Origin',(89.9885276254023,506.710565160552,-38.1221601717556)) ;
#65664 = CARTESIAN_POINT('',(89.9885276254021,506.710565160552,-42.122160469427)) ;
#65665 = CARTESIAN_POINT('Origin',(89.988527625402,506.710565160552,-43.1221601717556)) ;
#65666 = CARTESIAN_POINT('Origin',(89.9885276254023,506.710565160552,-38.1221601717556)) ;
#65667 = CARTESIAN_POINT('Origin',(158.688527625402,506.710565160539,-43.1221607671016)) ;
#65668 = CARTESIAN_POINT('',(169.388527625402,506.710565160538,-42.1221604694307)) ;
#65669 = CARTESIAN_POINT('Origin',(169.388527625402,506.710565160538,-43.122160767102)) ;
#65670 = CARTESIAN_POINT('',(158.688527625402,506.710565160539,-42.1221607671016)) ;
#65671 = CARTESIAN_POINT('Origin',(169.388527625402,506.710565160538,-38.1221601717593)) ;
#65672 = CARTESIAN_POINT('',(173.388527625402,506.710565160537,-38.1221601717594)) ;
#65673 = CARTESIAN_POINT('Origin',(174.388527625402,506.710565160537,-38.1221601717595)) ;
#65674 = CARTESIAN_POINT('Origin',(169.388527625402,506.710565160538,-38.1221601717593)) ;
#65675 = CARTESIAN_POINT('Origin',(174.388527625403,506.710565160537,-20.8221601717595)) ;
#65676 = CARTESIAN_POINT('',(173.388527625402,506.710565160537,-37.2221601717594)) ;
#65677 = CARTESIAN_POINT('Origin',(174.388527625402,506.710565160537,-37.2221601717595)) ;
#65678 = CARTESIAN_POINT('',(173.388527625403,506.710565160537,-20.8221601717595)) ;
#65679 = CARTESIAN_POINT('Origin',(173.388527625402,504.210565160537,-42.1221601717595)) ;
#65680 = CARTESIAN_POINT('',(173.388527625402,506.960565160537,-38.1221601717594)) ;
#65681 = CARTESIAN_POINT('',(173.388527625402,507.460565160537,-38.1221601717594)) ;
#65682 = CARTESIAN_POINT('',(173.388527625402,506.960565160537,-37.2221601717594)) ;
#65683 = CARTESIAN_POINT('',(173.388527625402,506.960565160537,-45.8221601717595)) ;
#65684 = CARTESIAN_POINT('',(173.388527625402,507.460565160537,-37.2221601717594)) ;
#65685 = CARTESIAN_POINT('Origin',(169.388527625376,354.701436995038,-38.1221601717593)) ;
#65686 = CARTESIAN_POINT('',(169.388527625402,506.960565160538,-42.1221604694306)) ;
#65687 = CARTESIAN_POINT('',(169.388527625402,506.210565160538,-42.1221601717592)) ;
#65688 = CARTESIAN_POINT('Origin',(169.388527625402,506.960565160538,-38.1221601717593)) ;
#65689 = CARTESIAN_POINT('Origin',(104.988527625411,561.210565160549,-42.1221607670991)) ;
#65690 = CARTESIAN_POINT('',(89.9885276254021,506.960565160552,-42.1221604694269)) ;
#65691 = CARTESIAN_POINT('',(89.9885276254479,767.719724046651,-42.1221607670984)) ;
#65692 = CARTESIAN_POINT('',(158.688527625402,506.960565160539,-42.1221607671016)) ;
#65693 = CARTESIAN_POINT('Origin',(89.9885276254481,767.719724046652,-38.1221601717556)) ;
#65694 = CARTESIAN_POINT('',(85.9885276254023,506.960565160552,-38.1221601717554)) ;
#65695 = CARTESIAN_POINT('',(85.9885276254022,506.210565160552,-38.1221601717555)) ;
#65696 = CARTESIAN_POINT('Origin',(89.9885276254023,506.960565160551,-38.1221601717556)) ;
#65697 = CARTESIAN_POINT('Origin',(85.9885276254025,504.210565160552,-24.1221601717555)) ;
#65698 = CARTESIAN_POINT('',(85.9885276254028,506.960565160552,-25.7721601717555)) ;
#65699 = CARTESIAN_POINT('',(85.9885276254027,506.210565160552,-25.7721601717555)) ;
#65700 = CARTESIAN_POINT('',(85.9885276254024,506.960565160552,-36.8221601717555)) ;
#65701 = CARTESIAN_POINT('Origin',(127.688527625422,615.710565160545,-36.8221601717574)) ;
#65702 = CARTESIAN_POINT('',(126.688527625421,615.710565160545,-38.1221601717573)) ;
#65703 = CARTESIAN_POINT('Origin',(127.688527625421,615.710565160545,-38.1221601717573)) ;
#65704 = CARTESIAN_POINT('',(126.688527625422,615.710565160545,-25.7721601717573)) ;
#65705 = CARTESIAN_POINT('Origin',(127.688527625422,615.710565160545,-25.7721601717573)) ;
#65706 = CARTESIAN_POINT('',(126.688527625422,615.710565160545,-36.8221601717573)) ;
#65707 = CARTESIAN_POINT('Origin',(122.688527625421,615.710565160546,-38.1221601717571)) ;
#65708 = CARTESIAN_POINT('',(122.688527625421,615.710565160546,-42.1221604694271)) ;
#65709 = CARTESIAN_POINT('Origin',(122.688527625421,615.710565160546,-43.1221601717571)) ;
#65710 = CARTESIAN_POINT('Origin',(122.688527625421,615.710565160546,-38.1221601717571)) ;
#65711 = CARTESIAN_POINT('Origin',(158.688527625421,615.710565160539,-43.1221607670988)) ;
#65712 = CARTESIAN_POINT('',(99.6885276254213,615.71056516055,-42.1221604694261)) ;
#65713 = CARTESIAN_POINT('Origin',(99.6885276254212,615.71056516055,-43.1221607670961)) ;
#65714 = CARTESIAN_POINT('',(158.688527625421,615.710565160539,-42.1221607670988)) ;
#65715 = CARTESIAN_POINT('Origin',(99.6885276254214,615.71056516055,-38.1221601717561)) ;
#65716 = CARTESIAN_POINT('',(95.6885276254214,615.71056516055,-38.1221601717559)) ;
#65717 = CARTESIAN_POINT('Origin',(94.6885276254214,615.710565160551,-38.1221601717558)) ;
#65718 = CARTESIAN_POINT('Origin',(99.6885276254214,615.71056516055,-38.1221601717561)) ;
#65719 = CARTESIAN_POINT('Origin',(94.6885276254211,615.710565160551,-45.8221601717558)) ;
#65720 = CARTESIAN_POINT('',(95.688527625422,615.71056516055,-25.7721601717559)) ;
#65721 = CARTESIAN_POINT('Origin',(94.688527625422,615.710565160551,-25.7721601717558)) ;
#65722 = CARTESIAN_POINT('',(95.6885276254211,615.71056516055,-45.8221601717559)) ;
#65723 = CARTESIAN_POINT('Origin',(95.6885276254217,618.21056516055,-42.1221601717559)) ;
#65724 = CARTESIAN_POINT('',(95.6885276254213,615.460565160551,-38.1221601717559)) ;
#65725 = CARTESIAN_POINT('',(95.6885276254212,614.960565160551,-38.1221601717559)) ;
#65726 = CARTESIAN_POINT('',(95.6885276254219,615.460565160551,-25.7721601717559)) ;
#65727 = CARTESIAN_POINT('',(95.688527625421,615.460565160551,-45.8221601717559)) ;
#65728 = CARTESIAN_POINT('',(95.6885276254174,589.898065160551,-25.7721601717559)) ;
#65729 = CARTESIAN_POINT('Origin',(99.6885276254481,767.71972404665,-38.122160171756)) ;
#65730 = CARTESIAN_POINT('',(99.6885276254212,615.46056516055,-42.1221604694261)) ;
#65731 = CARTESIAN_POINT('',(99.6885276254213,616.21056516055,-42.1221601717561)) ;
#65732 = CARTESIAN_POINT('Origin',(99.6885276254213,615.46056516055,-38.1221601717561)) ;
#65733 = CARTESIAN_POINT('Origin',(104.988527625411,561.210565160549,-42.1221607670963)) ;
#65734 = CARTESIAN_POINT('',(122.688527625421,615.460565160546,-42.1221604694271)) ;
#65735 = CARTESIAN_POINT('',(122.688527625375,354.701436995046,-42.1221607670972)) ;
#65736 = CARTESIAN_POINT('',(158.688527625421,615.460565160539,-42.1221607670988)) ;
#65737 = CARTESIAN_POINT('Origin',(122.688527625376,354.701436995046,-38.1221601717572)) ;
#65738 = CARTESIAN_POINT('',(126.688527625421,615.460565160545,-38.1221601717573)) ;
#65739 = CARTESIAN_POINT('',(126.688527625422,616.210565160545,-38.1221601717573)) ;
#65740 = CARTESIAN_POINT('Origin',(122.688527625421,615.460565160546,-38.1221601717571)) ;
#65741 = CARTESIAN_POINT('Origin',(126.688527625423,618.210565160545,-24.1221601717573)) ;
#65742 = CARTESIAN_POINT('',(126.688527625422,615.460565160545,-25.7721601717573)) ;
#65743 = CARTESIAN_POINT('',(126.688527625417,589.898065160545,-25.7721601717573)) ;
#65744 = CARTESIAN_POINT('',(126.688527625421,615.460565160545,-36.8221601717573)) ;
#65745 = CARTESIAN_POINT('Origin',(94.8885276254124,564.535138680008,-46.5221601717561)) ;
#65746 = CARTESIAN_POINT('',(97.6385276254124,566.122851920279,-47.522160171756)) ;
#65747 = CARTESIAN_POINT('',(94.8885276254124,564.535138680008,-47.5221601717559)) ;
#65748 = CARTESIAN_POINT('',(125.890374340326,582.434063226238,-47.5221601717573)) ;
#65749 = CARTESIAN_POINT('',(97.6385276254124,566.122851920279,-49.522160171756)) ;
#65750 = CARTESIAN_POINT('',(97.6385276254124,566.122851920279,-46.772160171756)) ;
#65751 = CARTESIAN_POINT('',(94.8885276254124,564.535138680008,-49.5221601717559)) ;
#65752 = CARTESIAN_POINT('',(125.890374340326,582.434063226239,-49.5221601717573)) ;
#65753 = CARTESIAN_POINT('',(94.8885276254124,564.535138680008,-46.5221601717561)) ;
#65754 = CARTESIAN_POINT('Origin',(92.1385276254124,566.122851920279,-46.522160171756)) ;
#65755 = CARTESIAN_POINT('',(92.1385276254124,566.122851920279,-47.5221601717558)) ;
#65756 = CARTESIAN_POINT('',(150.636680910491,532.348927374043,-47.5221601717585)) ;
#65757 = CARTESIAN_POINT('',(92.1385276254124,566.122851920279,-49.5221601717558)) ;
#65758 = CARTESIAN_POINT('',(150.636680910491,532.348927374043,-49.5221601717584)) ;
#65759 = CARTESIAN_POINT('',(92.1385276254124,566.122851920279,-46.772160171756)) ;
#65760 = CARTESIAN_POINT('Origin',(92.1385276254124,569.298278400822,-46.5221601717557)) ;
#65761 = CARTESIAN_POINT('',(92.1385276254124,569.298278400822,-47.5221601717558)) ;
#65762 = CARTESIAN_POINT('',(92.1385276254124,536.754421780676,-47.5221601717558)) ;
#65763 = CARTESIAN_POINT('',(92.1385276254124,569.298278400822,-49.5221601717558)) ;
#65764 = CARTESIAN_POINT('',(92.1385276254124,536.754421780676,-49.5221601717558)) ;
#65765 = CARTESIAN_POINT('',(92.1385276254124,569.298278400822,-46.7721601717557)) ;
#65766 = CARTESIAN_POINT('Origin',(94.8885276254124,570.885991641093,-46.5221601717556)) ;
#65767 = CARTESIAN_POINT('',(94.8885276254124,570.885991641094,-47.5221601717559)) ;
#65768 = CARTESIAN_POINT('',(124.515374340326,587.991059567189,-47.5221601717573)) ;
#65769 = CARTESIAN_POINT('',(94.8885276254124,570.885991641094,-49.5221601717559)) ;
#65770 = CARTESIAN_POINT('',(124.515374340326,587.991059567189,-49.5221601717572)) ;
#65771 = CARTESIAN_POINT('',(94.8885276254124,570.885991641093,-46.5221601717556)) ;
#65772 = CARTESIAN_POINT('Origin',(97.6385276254124,566.122851920279,-46.522160171756)) ;
#65773 = CARTESIAN_POINT('',(97.6385276254124,569.298278400822,-47.522160171756)) ;
#65774 = CARTESIAN_POINT('',(97.6385276254125,535.166708540405,-47.522160171756)) ;
#65775 = CARTESIAN_POINT('',(97.6385276254124,569.298278400822,-49.522160171756)) ;
#65776 = CARTESIAN_POINT('',(97.6385276254124,569.298278400822,-46.7721601717557)) ;
#65777 = CARTESIAN_POINT('',(97.6385276254125,535.166708540405,-49.522160171756)) ;
#65778 = CARTESIAN_POINT('Origin',(97.6385276254124,569.298278400822,-46.5221601717557)) ;
#65779 = CARTESIAN_POINT('',(154.761680910491,536.318210474722,-47.5221601717586)) ;
#65780 = CARTESIAN_POINT('',(154.761680910491,536.318210474722,-49.5221601717586)) ;
#65781 = CARTESIAN_POINT('Origin',(184.888527625403,510.035138679992,-46.5221601717602)) ;
#65782 = CARTESIAN_POINT('',(187.638527625403,511.622851920263,-47.5221601717601)) ;
#65783 = CARTESIAN_POINT('',(184.888527625403,510.035138679992,-47.52216017176)) ;
#65784 = CARTESIAN_POINT('',(193.939970466886,515.260991641077,-47.5221601717604)) ;
#65785 = CARTESIAN_POINT('',(187.638527625403,511.622851920264,-49.5221601717601)) ;
#65786 = CARTESIAN_POINT('',(187.638527625403,511.622851920263,-46.7721601717601)) ;
#65787 = CARTESIAN_POINT('',(184.888527625403,510.035138679992,-49.52216017176)) ;
#65788 = CARTESIAN_POINT('',(193.939970466886,515.260991641077,-49.5221601717604)) ;
#65789 = CARTESIAN_POINT('',(184.888527625403,510.035138679992,-46.5221601717602)) ;
#65790 = CARTESIAN_POINT('Origin',(182.138527625403,511.622851920263,-46.5221601717601)) ;
#65791 = CARTESIAN_POINT('',(182.138527625403,511.622851920263,-47.5221601717599)) ;
#65792 = CARTESIAN_POINT('',(195.087084783918,504.146998959177,-47.5221601717605)) ;
#65793 = CARTESIAN_POINT('',(182.138527625403,511.622851920264,-49.5221601717599)) ;
#65794 = CARTESIAN_POINT('',(195.087084783918,504.146998959177,-49.5221601717605)) ;
#65795 = CARTESIAN_POINT('',(182.138527625403,511.622851920263,-46.7721601717601)) ;
#65796 = CARTESIAN_POINT('Origin',(182.138527625403,514.798278400806,-46.5221601717598)) ;
#65797 = CARTESIAN_POINT('',(182.138527625403,514.798278400806,-47.5221601717599)) ;
#65798 = CARTESIAN_POINT('',(182.138527625403,509.504421780668,-47.5221601717599)) ;
#65799 = CARTESIAN_POINT('',(182.138527625403,514.798278400806,-49.5221601717599)) ;
#65800 = CARTESIAN_POINT('',(182.138527625403,509.504421780668,-49.5221601717599)) ;
#65801 = CARTESIAN_POINT('',(182.138527625403,514.798278400806,-46.7721601717598)) ;
#65802 = CARTESIAN_POINT('Origin',(184.888527625403,516.385991641078,-46.5221601717597)) ;
#65803 = CARTESIAN_POINT('',(184.888527625403,516.385991641078,-47.52216017176)) ;
#65804 = CARTESIAN_POINT('',(192.564970466886,520.817987982027,-47.5221601717604)) ;
#65805 = CARTESIAN_POINT('',(184.888527625403,516.385991641078,-49.52216017176)) ;
#65806 = CARTESIAN_POINT('',(192.564970466886,520.817987982027,-49.5221601717603)) ;
#65807 = CARTESIAN_POINT('',(184.888527625403,516.385991641078,-46.5221601717597)) ;
#65808 = CARTESIAN_POINT('Origin',(187.638527625403,511.622851920263,-46.5221601717601)) ;
#65809 = CARTESIAN_POINT('',(187.638527625403,514.798278400806,-47.5221601717601)) ;
#65810 = CARTESIAN_POINT('',(187.638527625403,507.916708540397,-47.5221601717601)) ;
#65811 = CARTESIAN_POINT('',(187.638527625403,514.798278400806,-49.5221601717601)) ;
#65812 = CARTESIAN_POINT('',(187.638527625403,514.798278400806,-46.7721601717598)) ;
#65813 = CARTESIAN_POINT('',(187.638527625403,507.916708540397,-49.5221601717601)) ;
#65814 = CARTESIAN_POINT('Origin',(187.638527625403,514.798278400806,-46.5221601717598)) ;
#65815 = CARTESIAN_POINT('',(199.212084783918,508.116282059856,-47.5221601717607)) ;
#65816 = CARTESIAN_POINT('',(199.212084783918,508.116282059856,-49.5221601717607)) ;
#65817 = CARTESIAN_POINT('Origin',(-2.61147237459646,504.210565160568,0.477839828248552)) ;
#65818 = CARTESIAN_POINT('Origin',(-2.61147237459646,504.210565160568,0.477839828248552)) ;
#65819 = CARTESIAN_POINT('Origin',(212.388527625421,616.21056516053,-47.0221601717612)) ;
#65820 = CARTESIAN_POINT('',(148.388527625421,616.210565160541,-47.5221601717583)) ;
#65821 = CARTESIAN_POINT('Origin',(148.388527625421,616.210565160541,-47.0221601717583)) ;
#65822 = CARTESIAN_POINT('',(144.388527625421,616.210565160542,-47.5221601717581)) ;
#65823 = CARTESIAN_POINT('Origin',(144.388527625421,616.210565160542,-47.0221601717582)) ;
#65824 = CARTESIAN_POINT('',(212.388527625421,616.21056516053,-47.5221601717612)) ;
#65825 = CARTESIAN_POINT('Origin',(212.388527625402,506.21056516053,-47.0221601717613)) ;
#65826 = CARTESIAN_POINT('',(197.688527625402,506.210565160533,-47.5221601717606)) ;
#65827 = CARTESIAN_POINT('Origin',(197.688527625402,506.210565160533,-47.0221601717606)) ;
#65828 = CARTESIAN_POINT('',(201.668527625402,506.210565160532,-47.5221601717607)) ;
#65829 = CARTESIAN_POINT('Origin',(201.668527625402,506.210565160532,-47.0221601717608)) ;
#65830 = CARTESIAN_POINT('',(212.388527625402,506.21056516053,-47.5221601717613)) ;
#65831 = CARTESIAN_POINT('Origin',(212.388527625402,506.21056516053,-47.0221601717613)) ;
#65832 = CARTESIAN_POINT('',(205.668527625402,506.210565160531,-47.5221601717609)) ;
#65833 = CARTESIAN_POINT('',(212.388527625402,506.21056516053,-47.5221601717613)) ;
#65834 = CARTESIAN_POINT('Origin',(205.668527625402,506.210565160531,-47.022160171761)) ;
#65835 = CARTESIAN_POINT('Origin',(212.388527625421,616.21056516053,-47.0221601717612)) ;
#65836 = CARTESIAN_POINT('',(201.668527625421,616.210565160532,-47.5221601717607)) ;
#65837 = CARTESIAN_POINT('Origin',(201.668527625421,616.210565160532,-47.0221601717608)) ;
#65838 = CARTESIAN_POINT('',(197.688527625421,616.210565160533,-47.5221601717605)) ;
#65839 = CARTESIAN_POINT('Origin',(197.688527625421,616.210565160533,-47.0221601717606)) ;
#65840 = CARTESIAN_POINT('',(212.388527625421,616.21056516053,-47.5221601717612)) ;
#65841 = CARTESIAN_POINT('Origin',(212.388527625421,616.21056516053,-47.0221601717612)) ;
#65842 = CARTESIAN_POINT('',(152.388527625421,616.210565160541,-47.5221601717585)) ;
#65843 = CARTESIAN_POINT('Origin',(152.388527625421,616.210565160541,-47.0221601717585)) ;
#65844 = CARTESIAN_POINT('',(193.688527625421,616.210565160533,-47.5221601717603)) ;
#65845 = CARTESIAN_POINT('',(212.388527625421,616.21056516053,-47.5221601717612)) ;
#65846 = CARTESIAN_POINT('Origin',(193.688527625421,616.210565160533,-47.0221601717604)) ;
#65847 = CARTESIAN_POINT('Origin',(140.388527625421,618.210565160543,-49.5221601717579)) ;
#65848 = CARTESIAN_POINT('',(140.38852762542,612.710565160543,-47.5221601717579)) ;
#65849 = CARTESIAN_POINT('',(140.38852762542,612.710565160543,-47.5221601717579)) ;
#65850 = CARTESIAN_POINT('',(140.38852762542,612.710565160543,-49.5221601717579)) ;
#65851 = CARTESIAN_POINT('',(140.38852762542,612.710565160543,-49.5221601717579)) ;
#65852 = CARTESIAN_POINT('',(140.388527625421,616.710565160543,-49.5221601717579)) ;
#65853 = CARTESIAN_POINT('',(140.388527625422,616.210565160543,-28.5221601717579)) ;
#65854 = CARTESIAN_POINT('Origin',(187.388264603402,504.260565160534,-24.0203292412001)) ;
#65855 = CARTESIAN_POINT('',(185.73826464091,504.810565160535,-24.0199774237433)) ;
#65856 = CARTESIAN_POINT('Origin',(187.388264603403,504.810565160534,-24.0203292412001)) ;
#65857 = CARTESIAN_POINT('',(185.188264653412,504.260565160534,-24.0198601512577)) ;
#65858 = CARTESIAN_POINT('Origin',(187.388264603402,504.210565160534,-24.0203292412001)) ;
#65859 = CARTESIAN_POINT('',(185.73826464091,504.210565160534,-24.0199774237433)) ;
#65860 = CARTESIAN_POINT('Origin',(187.388264603422,618.160565160534,-24.0203292412001)) ;
#65861 = CARTESIAN_POINT('',(187.382265311382,617.610565160534,-25.6703183346474)) ;
#65862 = CARTESIAN_POINT('Origin',(187.388264603422,617.610565160534,-24.0203292412001)) ;
#65863 = CARTESIAN_POINT('',(187.380265547368,618.160565160534,-26.2203146991298)) ;
#65864 = CARTESIAN_POINT('Origin',(187.388264603422,618.210565160534,-24.0203292412001)) ;
#65865 = CARTESIAN_POINT('',(187.382265311382,618.210565160534,-25.6703183346474)) ;
#65866 = CARTESIAN_POINT('Origin',(6.48852762540227,504.260565160566,-24.0221601717538)) ;
#65867 = CARTESIAN_POINT('',(4.83852762540237,504.810565160566,-24.0221601717538)) ;
#65868 = CARTESIAN_POINT('Origin',(6.48852762540237,504.810565160566,-24.0221601717538)) ;
#65869 = CARTESIAN_POINT('',(4.28852762540227,504.260565160566,-24.0221601717537)) ;
#65870 = CARTESIAN_POINT('Origin',(6.48852762540226,504.210565160566,-24.0221601717538)) ;
#65871 = CARTESIAN_POINT('',(4.83852762540226,504.210565160566,-24.0221601717537)) ;
#65872 = CARTESIAN_POINT('Origin',(99.7385276254127,561.58556516055,-25.7721601717561)) ;
#65873 = CARTESIAN_POINT('',(97.6885276254219,615.46056516055,-25.772160171756)) ;
#65874 = CARTESIAN_POINT('',(149.488527625422,615.460565160541,-25.7721601717583)) ;
#65875 = CARTESIAN_POINT('Origin',(94.4385276254219,615.460565160551,-25.7721601717558)) ;
#65876 = CARTESIAN_POINT('Origin',(99.7385276254127,561.58556516055,-25.7721601717561)) ;
#65877 = CARTESIAN_POINT('',(124.688527625422,615.460565160545,-25.7721601717572)) ;
#65878 = CARTESIAN_POINT('',(149.488527625422,615.460565160541,-25.7721601717583)) ;
#65879 = CARTESIAN_POINT('Origin',(127.938527625422,615.460565160545,-25.7721601717574)) ;
#65880 = CARTESIAN_POINT('Origin',(111.188527625422,614.960565160548,-29.5221601717566)) ;
#65881 = CARTESIAN_POINT('',(112.938527625421,613.460565160548,-29.5221601717567)) ;
#65882 = CARTESIAN_POINT('Origin',(111.188527625421,613.460565160548,-29.5221601717566)) ;
#65883 = CARTESIAN_POINT('',(112.938527625422,614.460565160548,-29.5221601717567)) ;
#65884 = CARTESIAN_POINT('',(112.938527625422,614.960565160548,-29.5221601717567)) ;
#65885 = CARTESIAN_POINT('',(111.188527625422,614.460565160548,-27.7721601717566)) ;
#65886 = CARTESIAN_POINT('Origin',(111.188527625422,614.460565160548,-29.5221601717566)) ;
#65887 = CARTESIAN_POINT('Origin',(111.188527625422,614.460565160548,-29.5221601717566)) ;
#65888 = CARTESIAN_POINT('Origin',(111.188527625422,614.960565160548,-29.5221601717566)) ;
#65889 = CARTESIAN_POINT('',(111.188527625422,615.460565160548,-26.7721601717566)) ;
#65890 = CARTESIAN_POINT('',(111.188527625422,614.960565160548,-27.2721601717566)) ;
#65891 = CARTESIAN_POINT('Origin',(111.188527625422,615.460565160548,-29.5221601717566)) ;
#65892 = CARTESIAN_POINT('Origin',(195.688527625419,612.880565160533,-89.2041436556704)) ;
#65893 = CARTESIAN_POINT('',(197.68852762542,612.880565160533,-47.5221601717605)) ;
#65894 = CARTESIAN_POINT('',(193.68852762542,612.880565160533,-47.5221601717603)) ;
#65895 = CARTESIAN_POINT('Origin',(195.68852762542,612.880565160533,-47.5221601717604)) ;
#65896 = CARTESIAN_POINT('',(197.68852762542,612.880565160533,-49.5221601717605)) ;
#65897 = CARTESIAN_POINT('',(197.68852762542,612.880565160533,-47.5221601717605)) ;
#65898 = CARTESIAN_POINT('',(193.68852762542,612.880565160533,-49.5221601717603)) ;
#65899 = CARTESIAN_POINT('Origin',(195.68852762542,612.880565160533,-49.5221601717604)) ;
#65900 = CARTESIAN_POINT('',(193.68852762542,612.880565160533,-49.5221601717603)) ;
#65901 = CARTESIAN_POINT('Origin',(203.668527625419,612.880565160532,-89.2041436556707)) ;
#65902 = CARTESIAN_POINT('',(205.66852762542,612.880565160531,-47.5221601717609)) ;
#65903 = CARTESIAN_POINT('',(201.66852762542,612.880565160532,-47.5221601717607)) ;
#65904 = CARTESIAN_POINT('Origin',(203.66852762542,612.880565160532,-47.5221601717608)) ;
#65905 = CARTESIAN_POINT('',(205.66852762542,612.880565160531,-49.5221601717609)) ;
#65906 = CARTESIAN_POINT('',(205.66852762542,612.880565160531,-47.5221601717609)) ;
#65907 = CARTESIAN_POINT('',(201.66852762542,612.880565160532,-49.5221601717607)) ;
#65908 = CARTESIAN_POINT('Origin',(203.66852762542,612.880565160532,-49.5221601717608)) ;
#65909 = CARTESIAN_POINT('',(201.66852762542,612.880565160532,-49.5221601717607)) ;
#65910 = CARTESIAN_POINT('Origin',(203.668527625405,509.540565160532,19.9106552778092)) ;
#65911 = CARTESIAN_POINT('',(205.668527625402,509.540565160531,-49.522160171761)) ;
#65912 = CARTESIAN_POINT('',(201.668527625402,509.540565160532,-49.5221601717608)) ;
#65913 = CARTESIAN_POINT('Origin',(203.668527625402,509.540565160532,-49.5221601717608)) ;
#65914 = CARTESIAN_POINT('',(205.668527625402,509.540565160531,-47.5221601717609)) ;
#65915 = CARTESIAN_POINT('',(205.668527625402,509.540565160531,-49.5221601717609)) ;
#65916 = CARTESIAN_POINT('',(201.668527625402,509.540565160532,-47.5221601717607)) ;
#65917 = CARTESIAN_POINT('Origin',(203.668527625402,509.540565160532,-47.5221601717608)) ;
#65918 = CARTESIAN_POINT('',(201.668527625402,509.540565160532,-47.5221601717607)) ;
#65919 = CARTESIAN_POINT('Origin',(195.688527625405,509.540565160533,19.9106552778095)) ;
#65920 = CARTESIAN_POINT('',(197.688527625402,509.540565160533,-49.5221601717606)) ;
#65921 = CARTESIAN_POINT('',(193.688527625402,509.540565160533,-49.5221601717604)) ;
#65922 = CARTESIAN_POINT('Origin',(195.688527625402,509.540565160533,-49.5221601717605)) ;
#65923 = CARTESIAN_POINT('',(197.688527625402,509.540565160533,-47.5221601717606)) ;
#65924 = CARTESIAN_POINT('',(197.688527625402,509.540565160533,-49.5221601717606)) ;
#65925 = CARTESIAN_POINT('',(193.688527625402,509.540565160533,-47.5221601717604)) ;
#65926 = CARTESIAN_POINT('Origin',(195.688527625402,509.540565160533,-47.5221601717605)) ;
#65927 = CARTESIAN_POINT('',(193.688527625402,509.540565160533,-47.5221601717604)) ;
#65928 = CARTESIAN_POINT('Origin',(142.388527625419,612.710565160542,-88.630160171758)) ;
#65929 = CARTESIAN_POINT('',(144.38852762542,612.710565160542,-49.5221601717581)) ;
#65930 = CARTESIAN_POINT('Origin',(142.38852762542,612.710565160542,-49.522160171758)) ;
#65931 = CARTESIAN_POINT('',(144.38852762542,612.710565160542,-47.5221601717581)) ;
#65932 = CARTESIAN_POINT('Origin',(142.38852762542,612.710565160542,-47.522160171758)) ;
#65933 = CARTESIAN_POINT('',(144.38852762542,612.710565160542,-47.5221601717581)) ;
#65934 = CARTESIAN_POINT('Origin',(150.388527625419,612.710565160541,-88.6301601717583)) ;
#65935 = CARTESIAN_POINT('',(152.38852762542,612.710565160541,-49.5221601717584)) ;
#65936 = CARTESIAN_POINT('',(148.38852762542,612.710565160541,-49.5221601717583)) ;
#65937 = CARTESIAN_POINT('Origin',(150.38852762542,612.710565160541,-49.5221601717583)) ;
#65938 = CARTESIAN_POINT('',(148.38852762542,612.710565160541,-47.5221601717583)) ;
#65939 = CARTESIAN_POINT('',(148.38852762542,612.710565160541,-49.5221601717583)) ;
#65940 = CARTESIAN_POINT('',(152.38852762542,612.710565160541,-47.5221601717585)) ;
#65941 = CARTESIAN_POINT('Origin',(150.38852762542,612.710565160541,-47.5221601717583)) ;
#65942 = CARTESIAN_POINT('',(152.38852762542,612.710565160541,-47.5221601717585)) ;
#65943 = CARTESIAN_POINT('Origin',(122.688527625421,615.460565160546,-38.1221601717571)) ;
#65944 = CARTESIAN_POINT('',(124.688527625421,615.460565160545,-38.1221601717572)) ;
#65945 = CARTESIAN_POINT('Origin',(127.938527625421,615.460565160545,-38.1221601717574)) ;
#65946 = CARTESIAN_POINT('',(122.688527625421,615.460565160546,-40.1221601717571)) ;
#65947 = CARTESIAN_POINT('Origin',(122.688527625421,615.460565160546,-43.3721601717571)) ;
#65948 = CARTESIAN_POINT('Origin',(122.688527625421,615.460565160546,-38.1221601717571)) ;
#65949 = CARTESIAN_POINT('Origin',(127.938527625421,615.460565160545,-38.6663657544474)) ;
#65950 = CARTESIAN_POINT('Origin',(127.938527625422,615.460565160545,-24.1221601717574)) ;
#65951 = CARTESIAN_POINT('',(124.688527625421,615.460565160545,-38.1221601726072)) ;
#65952 = CARTESIAN_POINT('Origin',(150.388527625448,766.820965161141,-28.5221601717584)) ;
#65953 = CARTESIAN_POINT('',(148.388527625422,616.210565160541,-28.5221601717583)) ;
#65954 = CARTESIAN_POINT('',(152.388527625422,618.710565160541,-28.5221601717585)) ;
#65955 = CARTESIAN_POINT('Origin',(195.688527625376,354.701436995033,-28.5221601717605)) ;
#65956 = CARTESIAN_POINT('',(197.688527625422,618.710565160533,-28.5221601717605)) ;
#65957 = CARTESIAN_POINT('',(193.688527625422,616.210565160533,-28.5221601717604)) ;
#65958 = CARTESIAN_POINT('Origin',(203.668527625376,354.701436995032,-28.5221601717608)) ;
#65959 = CARTESIAN_POINT('',(205.668527625422,618.710565160531,-28.5221601717609)) ;
#65960 = CARTESIAN_POINT('',(201.668527625422,616.210565160532,-28.5221601717607)) ;
#65961 = CARTESIAN_POINT('Origin',(-2.61147237459681,507.212565160568,-19.5221601717514)) ;
#65962 = CARTESIAN_POINT('Origin',(142.388527625448,766.820965161142,-28.522160171758)) ;
#65963 = CARTESIAN_POINT('',(144.388527625422,618.710565160542,-28.5221601717581)) ;
#65964 = CARTESIAN_POINT('Origin',(188.388527625422,618.210565160534,-30.2221601717601)) ;
#65965 = CARTESIAN_POINT('',(188.388527625422,618.710565160534,-30.2221601717601)) ;
#65966 = CARTESIAN_POINT('',(188.388527625422,616.210565160534,-37.2221601717601)) ;
#65967 = CARTESIAN_POINT('Origin',(188.388527625422,618.210565160534,-37.2221601717601)) ;
#65968 = CARTESIAN_POINT('',(186.388527625422,616.210565160535,-37.22216017176)) ;
#65969 = CARTESIAN_POINT('Origin',(186.388527625422,618.210565160535,-37.22216017176)) ;
#65970 = CARTESIAN_POINT('',(186.388527625422,616.210565160535,-30.22216017176)) ;
#65971 = CARTESIAN_POINT('Origin',(186.388527625422,618.210565160535,-30.22216017176)) ;
#65972 = CARTESIAN_POINT('Origin',(173.388527625422,618.210565160537,-30.2221601717594)) ;
#65973 = CARTESIAN_POINT('',(173.388527625422,618.710565160537,-30.2221601717594)) ;
#65974 = CARTESIAN_POINT('',(173.388527625422,616.210565160537,-37.2221601717594)) ;
#65975 = CARTESIAN_POINT('Origin',(173.388527625422,618.210565160537,-37.2221601717594)) ;
#65976 = CARTESIAN_POINT('',(171.388527625422,616.210565160537,-37.2221601717593)) ;
#65977 = CARTESIAN_POINT('Origin',(171.388527625422,618.210565160537,-37.2221601717593)) ;
#65978 = CARTESIAN_POINT('',(171.388527625422,616.210565160537,-30.2221601717593)) ;
#65979 = CARTESIAN_POINT('Origin',(171.388527625422,618.210565160537,-30.2221601717593)) ;
#65980 = CARTESIAN_POINT('Origin',(38.3885276254222,618.210565160561,-30.2221601717533)) ;
#65981 = CARTESIAN_POINT('',(38.3885276254223,618.710565160561,-30.2221601717533)) ;
#65982 = CARTESIAN_POINT('',(38.3885276254215,616.210565160561,-37.2221601717533)) ;
#65983 = CARTESIAN_POINT('Origin',(38.3885276254219,618.210565160561,-37.2221601717533)) ;
#65984 = CARTESIAN_POINT('',(36.3885276254215,616.210565160561,-37.2221601717532)) ;
#65985 = CARTESIAN_POINT('Origin',(36.3885276254219,618.210565160561,-37.2221601717532)) ;
#65986 = CARTESIAN_POINT('',(36.3885276254219,616.210565160561,-30.2221601717532)) ;
#65987 = CARTESIAN_POINT('Origin',(36.3885276254222,618.210565160561,-30.2221601717532)) ;
#65988 = CARTESIAN_POINT('Origin',(97.6885276254225,618.21056516055,-24.122160171756)) ;
#65989 = CARTESIAN_POINT('Origin',(94.438527625422,615.460565160551,-24.1221601717558)) ;
#65990 = CARTESIAN_POINT('Origin',(21.3885276254219,618.210565160564,-37.2221601717525)) ;
#65991 = CARTESIAN_POINT('',(21.3885276254215,616.210565160564,-37.2221601717525)) ;
#65992 = CARTESIAN_POINT('',(21.3885276254219,616.210565160564,-30.2221601717525)) ;
#65993 = CARTESIAN_POINT('Origin',(21.3885276254222,618.210565160564,-30.2221601717525)) ;
#65994 = CARTESIAN_POINT('',(23.3885276254223,618.710565160563,-30.2221601717526)) ;
#65995 = CARTESIAN_POINT('Origin',(23.3885276254222,618.210565160563,-30.2221601717526)) ;
#65996 = CARTESIAN_POINT('',(23.3885276254215,616.210565160563,-37.2221601717526)) ;
#65997 = CARTESIAN_POINT('Origin',(23.3885276254219,618.210565160563,-37.2221601717526)) ;
#65998 = CARTESIAN_POINT('Origin',(148.388527625421,618.210565160541,-49.5221601717583)) ;
#65999 = CARTESIAN_POINT('',(148.38852762542,612.710565160541,-47.5221601717583)) ;
#66000 = CARTESIAN_POINT('',(148.388527625421,616.710565160541,-49.5221601717583)) ;
#66001 = CARTESIAN_POINT('',(148.388527625421,616.710565160541,-49.5221601717583)) ;
#66002 = CARTESIAN_POINT('Origin',(148.388527625421,616.710565160541,-47.5221601717583)) ;
#66003 = CARTESIAN_POINT('Origin',(201.668527625411,561.210565160532,-49.5221601717607)) ;
#66004 = CARTESIAN_POINT('',(201.668527625421,615.210565160532,-47.5221601717607)) ;
#66005 = CARTESIAN_POINT('',(201.668527625421,616.710565160532,-49.5221601717607)) ;
#66006 = CARTESIAN_POINT('',(201.668527625421,616.710565160532,-49.5221601717607)) ;
#66007 = CARTESIAN_POINT('Origin',(201.668527625421,616.710565160532,-47.5221601717607)) ;
#66008 = CARTESIAN_POINT('Origin',(493.123247625421,616.710565160481,-47.522160171774)) ;
#66009 = CARTESIAN_POINT('',(197.688527625421,616.710565160533,-49.5221601717605)) ;
#66010 = CARTESIAN_POINT('Origin',(197.688527625421,616.710565160533,-47.5221601717605)) ;
#66011 = CARTESIAN_POINT('',(201.668527625421,616.710565160532,-49.5221601717607)) ;
#66012 = CARTESIAN_POINT('Origin',(-283.146192374579,616.710565160617,-47.5221601717387)) ;
#66013 = CARTESIAN_POINT('',(144.388527625421,616.710565160542,-49.5221601717581)) ;
#66014 = CARTESIAN_POINT('',(144.388527625421,616.710565160542,-49.5221601717581)) ;
#66015 = CARTESIAN_POINT('Origin',(144.388527625421,616.710565160542,-47.5221601717581)) ;
#66016 = CARTESIAN_POINT('Origin',(193.688527625411,561.210565160533,-49.5221601717604)) ;
#66017 = CARTESIAN_POINT('',(193.68852762542,612.880565160533,-47.5221601717603)) ;
#66018 = CARTESIAN_POINT('',(193.688527625421,616.710565160533,-49.5221601717603)) ;
#66019 = CARTESIAN_POINT('',(193.688527625421,616.710565160533,-49.5221601717603)) ;
#66020 = CARTESIAN_POINT('Origin',(193.688527625421,616.710565160533,-47.5221601717604)) ;
#66021 = CARTESIAN_POINT('Origin',(-283.146192374579,616.710565160617,-47.5221601717387)) ;
#66022 = CARTESIAN_POINT('',(152.388527625421,616.710565160541,-49.5221601717585)) ;
#66023 = CARTESIAN_POINT('',(152.388527625421,616.710565160541,-49.5221601717585)) ;
#66024 = CARTESIAN_POINT('Origin',(152.388527625421,616.710565160541,-47.5221601717585)) ;
#66025 = CARTESIAN_POINT('Origin',(99.1443220427211,615.46056516055,-43.3721601717561)) ;
#66026 = CARTESIAN_POINT('',(99.6885276246509,615.46056516055,-40.1221601717561)) ;
#66027 = CARTESIAN_POINT('Origin',(99.6885276254211,615.46056516055,-43.3721601717561)) ;
#66028 = CARTESIAN_POINT('',(99.6885276245213,615.46056516055,-40.1221601717561)) ;
#66029 = CARTESIAN_POINT('Origin',(99.6885276254213,615.46056516055,-38.1221601717561)) ;
#66030 = CARTESIAN_POINT('',(97.6885276254214,615.46056516055,-38.122160171756)) ;
#66031 = CARTESIAN_POINT('Origin',(94.4385276254214,615.460565160551,-38.1221601717558)) ;
#66032 = CARTESIAN_POINT('Origin',(99.6885276254213,615.46056516055,-38.1221601717561)) ;
#66033 = CARTESIAN_POINT('Origin',(94.438527625424,615.460565160551,19.9106552778142)) ;
#66034 = CARTESIAN_POINT('',(97.6885276254219,615.46056516055,-25.772160171756)) ;
#66035 = CARTESIAN_POINT('Origin',(197.688527625411,561.210565160533,-49.5221601717606)) ;
#66036 = CARTESIAN_POINT('',(197.68852762542,612.880565160533,-47.5221601717605)) ;
#66037 = CARTESIAN_POINT('',(197.68852762542,612.880565160533,-49.5221601717605)) ;
#66038 = CARTESIAN_POINT('Origin',(205.668527625411,561.210565160531,-49.5221601717609)) ;
#66039 = CARTESIAN_POINT('',(205.66852762542,612.880565160531,-47.5221601717609)) ;
#66040 = CARTESIAN_POINT('',(205.66852762542,612.880565160531,-49.5221601717609)) ;
#66041 = CARTESIAN_POINT('Origin',(152.388527625422,618.210565160541,-26.5221601717585)) ;
#66042 = CARTESIAN_POINT('',(152.38852762542,612.710565160541,-49.5221601717584)) ;
#66043 = CARTESIAN_POINT('',(152.388527625421,615.210565160541,-47.5221601717585)) ;
#66044 = CARTESIAN_POINT('Origin',(144.388527625422,618.210565160542,-26.5221601717581)) ;
#66045 = CARTESIAN_POINT('',(144.38852762542,612.710565160542,-49.5221601717581)) ;
#66046 = CARTESIAN_POINT('',(144.388527625421,615.210565160542,-47.5221601717581)) ;
#66047 = CARTESIAN_POINT('Origin',(212.388527625402,506.96056516053,-49.5221601717612)) ;
#66048 = CARTESIAN_POINT('',(171.388527625403,506.960565160537,-25.7721601717594)) ;
#66049 = CARTESIAN_POINT('',(171.388527625403,506.960565160537,-30.2221601717593)) ;
#66050 = CARTESIAN_POINT('',(171.388527625403,506.960565160537,-25.7721601717594)) ;
#66051 = CARTESIAN_POINT('',(156.063527625403,506.96056516054,-25.7721601717587)) ;
#66052 = CARTESIAN_POINT('',(173.388527625403,506.960565160537,-24.1221601717594)) ;
#66053 = CARTESIAN_POINT('',(173.388527625401,506.960565160537,-55.8221601717594)) ;
#66054 = CARTESIAN_POINT('',(85.9885276254029,506.960565160552,-24.1221601717555)) ;
#66055 = CARTESIAN_POINT('',(173.388527625403,506.960565160537,-24.1221601717594)) ;
#66056 = CARTESIAN_POINT('',(85.9885276254019,506.960565160552,-46.8221601717555)) ;
#66057 = CARTESIAN_POINT('',(87.9885276254028,506.960565160552,-25.7721601717556)) ;
#66058 = CARTESIAN_POINT('',(156.063527625403,506.96056516054,-25.7721601717587)) ;
#66059 = CARTESIAN_POINT('',(87.9885276254023,506.960565160552,-38.1221601717556)) ;
#66060 = CARTESIAN_POINT('',(87.9885276254023,506.960565160552,-38.1221601726056)) ;
#66061 = CARTESIAN_POINT('',(89.9885276254022,506.960565160551,-40.1221601717556)) ;
#66062 = CARTESIAN_POINT('Origin',(89.9885276254023,506.960565160551,-38.1221601717556)) ;
#66063 = CARTESIAN_POINT('',(169.388527626173,506.960565160538,-40.1221601717593)) ;
#66064 = CARTESIAN_POINT('',(169.388527626302,506.960565160538,-40.1221601717592)) ;
#66065 = CARTESIAN_POINT('',(171.388527625402,506.960565160537,-38.1221601717593)) ;
#66066 = CARTESIAN_POINT('Origin',(169.388527625402,506.960565160538,-38.1221601717593)) ;
#66067 = CARTESIAN_POINT('',(171.388527625402,506.960565160537,-37.2221601717593)) ;
#66068 = CARTESIAN_POINT('',(171.388527625402,506.960565160537,-37.2221601717593)) ;
#66069 = CARTESIAN_POINT('',(171.388527625402,506.960565160537,-37.2221601717593)) ;
#66070 = CARTESIAN_POINT('',(102.988527625403,506.960565160549,-26.7721601717562)) ;
#66071 = CARTESIAN_POINT('Origin',(102.988527625403,506.960565160549,-29.5221601717562)) ;
#66072 = CARTESIAN_POINT('',(119.388527625403,506.960565160546,-26.772160171757)) ;
#66073 = CARTESIAN_POINT('Origin',(119.388527625403,506.960565160546,-29.522160171757)) ;
#66074 = CARTESIAN_POINT('',(137.988527625403,506.960565160543,-26.7721601717578)) ;
#66075 = CARTESIAN_POINT('Origin',(137.988527625403,506.960565160543,-29.5221601717578)) ;
#66076 = CARTESIAN_POINT('',(156.988527625403,506.96056516054,-26.7721601717587)) ;
#66077 = CARTESIAN_POINT('Origin',(156.988527625403,506.96056516054,-29.5221601717587)) ;
#66078 = CARTESIAN_POINT('Origin',(173.388527625402,504.210565160537,-24.1221601717594)) ;
#66079 = CARTESIAN_POINT('',(171.388527625403,508.960565160537,-24.1221601717594)) ;
#66080 = CARTESIAN_POINT('Origin',(171.388527625403,506.960565160537,-24.1221601717593)) ;
#66081 = CARTESIAN_POINT('',(87.9885276254033,508.960565160552,-24.1221601717556)) ;
#66082 = CARTESIAN_POINT('',(192.888527625403,508.960565160534,-24.1221601717603)) ;
#66083 = CARTESIAN_POINT('Origin',(87.9885276254029,506.960565160552,-24.1221601717556)) ;
#66084 = CARTESIAN_POINT('Origin',(156.988527625403,507.46056516054,-29.5221601717587)) ;
#66085 = CARTESIAN_POINT('',(155.238527625403,508.96056516054,-29.5221601717586)) ;
#66086 = CARTESIAN_POINT('Origin',(156.988527625403,508.96056516054,-29.5221601717587)) ;
#66087 = CARTESIAN_POINT('',(155.238527625403,507.96056516054,-29.5221601717586)) ;
#66088 = CARTESIAN_POINT('',(155.238527625403,507.46056516054,-29.5221601717586)) ;
#66089 = CARTESIAN_POINT('',(156.988527625403,507.96056516054,-27.7721601717587)) ;
#66090 = CARTESIAN_POINT('Origin',(156.988527625403,507.96056516054,-29.5221601717587)) ;
#66091 = CARTESIAN_POINT('Origin',(156.988527625403,507.96056516054,-29.5221601717587)) ;
#66092 = CARTESIAN_POINT('Origin',(156.988527625403,507.46056516054,-29.5221601717587)) ;
#66093 = CARTESIAN_POINT('',(156.988527625403,507.46056516054,-27.2721601717587)) ;
#66094 = CARTESIAN_POINT('Origin',(137.988527625403,507.460565160543,-29.5221601717578)) ;
#66095 = CARTESIAN_POINT('',(136.238527625403,508.960565160543,-29.5221601717578)) ;
#66096 = CARTESIAN_POINT('Origin',(137.988527625403,508.960565160543,-29.5221601717578)) ;
#66097 = CARTESIAN_POINT('',(136.238527625403,507.960565160543,-29.5221601717577)) ;
#66098 = CARTESIAN_POINT('',(136.238527625403,507.460565160543,-29.5221601717577)) ;
#66099 = CARTESIAN_POINT('',(137.988527625403,507.960565160543,-27.7721601717579)) ;
#66100 = CARTESIAN_POINT('Origin',(137.988527625403,507.960565160543,-29.5221601717578)) ;
#66101 = CARTESIAN_POINT('Origin',(137.988527625403,507.960565160543,-29.5221601717578)) ;
#66102 = CARTESIAN_POINT('Origin',(137.988527625403,507.460565160543,-29.5221601717578)) ;
#66103 = CARTESIAN_POINT('',(137.988527625403,507.460565160543,-27.2721601717578)) ;
#66104 = CARTESIAN_POINT('Origin',(119.388527625403,507.460565160546,-29.522160171757)) ;
#66105 = CARTESIAN_POINT('',(117.638527625403,508.960565160547,-29.5221601717569)) ;
#66106 = CARTESIAN_POINT('Origin',(119.388527625403,508.960565160546,-29.522160171757)) ;
#66107 = CARTESIAN_POINT('',(117.638527625403,507.960565160546,-29.5221601717569)) ;
#66108 = CARTESIAN_POINT('',(117.638527625403,507.460565160546,-29.5221601717569)) ;
#66109 = CARTESIAN_POINT('',(119.388527625403,507.960565160546,-27.772160171757)) ;
#66110 = CARTESIAN_POINT('Origin',(119.388527625403,507.960565160546,-29.522160171757)) ;
#66111 = CARTESIAN_POINT('Origin',(119.388527625403,507.960565160546,-29.522160171757)) ;
#66112 = CARTESIAN_POINT('Origin',(119.388527625403,507.460565160546,-29.522160171757)) ;
#66113 = CARTESIAN_POINT('',(119.388527625403,507.460565160546,-27.272160171757)) ;
#66114 = CARTESIAN_POINT('Origin',(102.988527625403,507.460565160549,-29.5221601717562)) ;
#66115 = CARTESIAN_POINT('',(101.238527625403,508.96056516055,-29.5221601717562)) ;
#66116 = CARTESIAN_POINT('Origin',(102.988527625403,508.960565160549,-29.5221601717562)) ;
#66117 = CARTESIAN_POINT('',(101.238527625403,507.960565160549,-29.5221601717561)) ;
#66118 = CARTESIAN_POINT('',(101.238527625403,507.460565160549,-29.5221601717561)) ;
#66119 = CARTESIAN_POINT('',(102.988527625403,507.960565160549,-27.7721601717563)) ;
#66120 = CARTESIAN_POINT('Origin',(102.988527625403,507.960565160549,-29.5221601717563)) ;
#66121 = CARTESIAN_POINT('Origin',(102.988527625403,507.960565160549,-29.5221601717563)) ;
#66122 = CARTESIAN_POINT('Origin',(102.988527625403,507.460565160549,-29.5221601717562)) ;
#66123 = CARTESIAN_POINT('',(102.988527625403,507.460565160549,-27.2721601717562)) ;
#66124 = CARTESIAN_POINT('Origin',(171.388527625422,618.210565160537,-37.2221601717593)) ;
#66125 = CARTESIAN_POINT('',(171.388527625403,508.960565160537,-37.2221601717594)) ;
#66126 = CARTESIAN_POINT('',(171.388527625403,508.960565160537,-30.2221601717593)) ;
#66127 = CARTESIAN_POINT('',(171.388527625402,508.960565160537,-43.3721601717594)) ;
#66128 = CARTESIAN_POINT('',(171.388527625403,506.960565160537,-30.2221601717593)) ;
#66129 = CARTESIAN_POINT('',(171.388527625403,509.460565160537,-37.2221601717594)) ;
#66130 = CARTESIAN_POINT('Origin',(99.7385276254032,506.585565284346,-25.7721601717561)) ;
#66131 = CARTESIAN_POINT('Origin',(174.638527625403,506.960565160537,-25.7721601717595)) ;
#66132 = CARTESIAN_POINT('Origin',(99.7385276254032,506.585565284346,-25.7721601717561)) ;
#66133 = CARTESIAN_POINT('Origin',(84.7385276254028,506.960565160553,-25.7721601717554)) ;
#66134 = CARTESIAN_POINT('Origin',(201.668527625411,561.210565160532,-49.5221601717607)) ;
#66135 = CARTESIAN_POINT('',(201.668527625402,503.710565160532,-28.5221601717607)) ;
#66136 = CARTESIAN_POINT('',(201.668527625402,505.710565160532,-49.5221601717607)) ;
#66137 = CARTESIAN_POINT('Origin',(201.668527625402,505.710565160532,-47.5221601717607)) ;
#66138 = CARTESIAN_POINT('',(201.668527625402,509.540565160532,-49.5221601717607)) ;
#66139 = CARTESIAN_POINT('',(201.668527625402,507.210565160532,-47.5221601717607)) ;
#66140 = CARTESIAN_POINT('Origin',(205.668527625411,561.210565160531,-49.5221601717609)) ;
#66141 = CARTESIAN_POINT('',(205.668527625402,509.540565160531,-47.5221601717609)) ;
#66142 = CARTESIAN_POINT('',(205.668527625402,505.710565160531,-49.5221601717609)) ;
#66143 = CARTESIAN_POINT('',(205.668527625403,506.210565160531,-28.5221601717609)) ;
#66144 = CARTESIAN_POINT('Origin',(21.3885276254222,618.210565160564,-30.2221601717525)) ;
#66145 = CARTESIAN_POINT('',(23.3885276254025,506.210565160563,-30.2221601717526)) ;
#66146 = CARTESIAN_POINT('',(21.3885276254025,506.210565160564,-30.2221601717525)) ;
#66147 = CARTESIAN_POINT('Origin',(23.3885276254222,618.210565160563,-30.2221601717526)) ;
#66148 = CARTESIAN_POINT('',(23.3885276254017,503.710565160563,-37.2221601717526)) ;
#66149 = CARTESIAN_POINT('Origin',(23.3885276254219,618.210565160563,-37.2221601717526)) ;
#66150 = CARTESIAN_POINT('',(21.3885276254022,506.210565160564,-37.2221601717525)) ;
#66151 = CARTESIAN_POINT('Origin',(21.3885276254219,618.210565160564,-37.2221601717525)) ;
#66152 = CARTESIAN_POINT('Origin',(173.388527625422,618.210565160537,-30.2221601717594)) ;
#66153 = CARTESIAN_POINT('',(173.388527625402,503.960565160537,-37.2221601717594)) ;
#66154 = CARTESIAN_POINT('',(173.388527625402,506.210565160537,-37.2221601717594)) ;
#66155 = CARTESIAN_POINT('',(173.388527625402,503.960565160537,-30.2221601717594)) ;
#66156 = CARTESIAN_POINT('',(173.388527625402,503.960565160537,-30.2221601717594)) ;
#66157 = CARTESIAN_POINT('',(173.388527625403,506.210565160537,-30.2221601717594)) ;
#66158 = CARTESIAN_POINT('Origin',(195.688527625376,354.701436995033,-28.5221601717605)) ;
#66159 = CARTESIAN_POINT('',(197.688527625403,506.210565160533,-28.5221601717605)) ;
#66160 = CARTESIAN_POINT('',(193.688527625402,503.710565160533,-28.5221601717604)) ;
#66161 = CARTESIAN_POINT('Origin',(203.668527625376,354.701436995032,-28.5221601717608)) ;
#66162 = CARTESIAN_POINT('Origin',(-2.61147237459681,507.212565160568,-19.5221601717514)) ;
#66163 = CARTESIAN_POINT('Origin',(171.388527625402,504.210565160537,-24.1221601717594)) ;
#66164 = CARTESIAN_POINT('Origin',(174.638527625403,506.960565160537,-24.1221601717595)) ;
#66165 = CARTESIAN_POINT('Origin',(84.7385276254029,506.960565160552,-24.1221601717554)) ;
#66166 = CARTESIAN_POINT('Origin',(38.3885276254219,618.210565160561,-37.2221601717533)) ;
#66167 = CARTESIAN_POINT('',(36.3885276254022,506.210565160561,-37.2221601717532)) ;
#66168 = CARTESIAN_POINT('',(38.3885276254017,503.710565160561,-37.2221601717533)) ;
#66169 = CARTESIAN_POINT('Origin',(36.3885276254219,618.210565160561,-37.2221601717532)) ;
#66170 = CARTESIAN_POINT('',(36.3885276254025,506.210565160561,-30.2221601717532)) ;
#66171 = CARTESIAN_POINT('Origin',(36.3885276254222,618.210565160561,-30.2221601717532)) ;
#66172 = CARTESIAN_POINT('',(38.3885276254025,506.210565160561,-30.2221601717533)) ;
#66173 = CARTESIAN_POINT('Origin',(38.3885276254222,618.210565160561,-30.2221601717533)) ;
#66174 = CARTESIAN_POINT('Origin',(188.388527625422,618.210565160534,-37.2221601717601)) ;
#66175 = CARTESIAN_POINT('',(186.388527625402,506.210565160535,-37.22216017176)) ;
#66176 = CARTESIAN_POINT('',(188.388527625402,503.710565160534,-37.2221601717601)) ;
#66177 = CARTESIAN_POINT('Origin',(186.388527625422,618.210565160535,-37.22216017176)) ;
#66178 = CARTESIAN_POINT('',(186.388527625403,506.210565160535,-30.22216017176)) ;
#66179 = CARTESIAN_POINT('Origin',(186.388527625422,618.210565160535,-30.22216017176)) ;
#66180 = CARTESIAN_POINT('',(188.388527625403,506.210565160534,-30.2221601717601)) ;
#66181 = CARTESIAN_POINT('Origin',(188.388527625422,618.210565160534,-30.2221601717601)) ;
#66182 = CARTESIAN_POINT('Origin',(169.388527625402,506.960565160538,-38.1221601717593)) ;
#66183 = CARTESIAN_POINT('Origin',(169.388527625402,506.960565160538,-43.3721601717593)) ;
#66184 = CARTESIAN_POINT('Origin',(174.638527625402,506.960565160537,-38.1221601717595)) ;
#66185 = CARTESIAN_POINT('Origin',(169.932733208102,506.960565160537,-43.3721601717593)) ;
#66186 = CARTESIAN_POINT('Origin',(89.988527625402,506.960565160551,-43.3721601717557)) ;
#66187 = CARTESIAN_POINT('Origin',(89.9885276254023,506.960565160551,-38.1221601717556)) ;
#66188 = CARTESIAN_POINT('Origin',(84.7385276254023,506.960565160553,-38.1221601717554)) ;
#66189 = CARTESIAN_POINT('Origin',(-283.146192374598,505.710565160617,-47.5221601717387)) ;
#66190 = CARTESIAN_POINT('',(193.688527625402,505.710565160533,-49.5221601717604)) ;
#66191 = CARTESIAN_POINT('',(-0.611472374598421,505.710565160567,-49.5221601717515)) ;
#66192 = CARTESIAN_POINT('Origin',(193.688527625402,505.710565160533,-47.5221601717604)) ;
#66193 = CARTESIAN_POINT('Origin',(193.688527625411,561.210565160533,-49.5221601717604)) ;
#66194 = CARTESIAN_POINT('',(193.688527625402,509.540565160533,-49.5221601717604)) ;
#66195 = CARTESIAN_POINT('',(193.688527625402,507.210565160533,-47.5221601717604)) ;
#66196 = CARTESIAN_POINT('Origin',(493.123247625402,505.710565160481,-47.522160171774)) ;
#66197 = CARTESIAN_POINT('',(197.688527625402,505.710565160533,-49.5221601717605)) ;
#66198 = CARTESIAN_POINT('Origin',(197.688527625402,505.710565160533,-47.5221601717605)) ;
#66199 = CARTESIAN_POINT('',(201.668527625402,505.710565160532,-49.5221601717607)) ;
#66200 = CARTESIAN_POINT('Origin',(197.688527625411,561.210565160533,-49.5221601717606)) ;
#66201 = CARTESIAN_POINT('',(197.688527625402,509.540565160533,-47.5221601717606)) ;
#66202 = CARTESIAN_POINT('',(197.688527625402,505.710565160533,-49.5221601717605)) ;
#66203 = CARTESIAN_POINT('Origin',(174.638527625405,506.960565160537,19.9106552778105)) ;
#66204 = CARTESIAN_POINT('Origin',(174.638527625403,506.960565160537,-30.2221601717595)) ;
#66205 = CARTESIAN_POINT('Origin',(174.638527625402,506.960565160537,-37.2221601717595)) ;
#66206 = CARTESIAN_POINT('Origin',(84.7385276254022,506.960565160553,-38.6663657544454)) ;
#66207 = CARTESIAN_POINT('Origin',(99.738527625422,615.46056516055,-22.6221601717603)) ;
#66208 = CARTESIAN_POINT('',(95.688527625422,615.460565160551,-24.1221601717559)) ;
#66209 = CARTESIAN_POINT('',(126.688527625422,615.460565160545,-24.1221601717573)) ;
#66210 = CARTESIAN_POINT('',(95.688527625422,615.460565160551,-24.1221601717559)) ;
#66211 = CARTESIAN_POINT('',(126.688527625422,615.460565160545,-24.1221601717573)) ;
#66212 = CARTESIAN_POINT('',(95.688527625422,615.460565160551,-24.1221601717559)) ;
#66213 = CARTESIAN_POINT('Origin',(6.48852762540226,504.210565160566,-24.0221601717538)) ;
#66214 = CARTESIAN_POINT('',(4.83852769761494,617.610303266554,-24.0221601717537)) ;
#66215 = CARTESIAN_POINT('',(6.48225865783948,617.612395100656,-25.6721482626337)) ;
#66216 = CARTESIAN_POINT('Origin',(6.48852838553329,617.610565789223,-24.022160479896)) ;
#66217 = CARTESIAN_POINT('',(4.83852762540226,504.210565160566,-24.0221601717537)) ;
#66218 = CARTESIAN_POINT('Origin',(6.48852838553329,617.610565789223,-24.022160479896)) ;
#66219 = CARTESIAN_POINT('Origin',(6.48826460342246,618.160565160566,-24.0203292411918)) ;
#66220 = CARTESIAN_POINT('',(6.48026554736851,618.160565160566,-26.2203146991215)) ;
#66221 = CARTESIAN_POINT('Ctrl Pts',(27.8977259437596,618.707397415445,-37.5528630721564)) ;
#66222 = CARTESIAN_POINT('Ctrl Pts',(28.0743877192963,618.67030643865,-38.2156681467201)) ;
#66223 = CARTESIAN_POINT('Ctrl Pts',(29.1421966155256,618.596141379903,-39.3386387111389)) ;
#66224 = CARTESIAN_POINT('Ctrl Pts',(31.4346649598415,618.484902239203,-38.9068600918672)) ;
#66225 = CARTESIAN_POINT('Ctrl Pts',(32.3091095046996,618.373679993346,-36.7435823810485)) ;
#66226 = CARTESIAN_POINT('Ctrl Pts',(30.966253505222,618.262457747489,-34.8371854931543)) ;
#66227 = CARTESIAN_POINT('Ctrl Pts',(28.6354820240381,618.151235501631,-34.9326680111136)) ;
#66228 = CARTESIAN_POINT('Ctrl Pts',(27.4535163667976,618.040013255774,-36.9436582668131)) ;
#66229 = CARTESIAN_POINT('Ctrl Pts',(28.5034276654628,617.928791009917,-39.0264313282299)) ;
#66230 = CARTESIAN_POINT('Ctrl Pts',(30.8229580687087,617.817568764059,-39.2721846815949)) ;
#66231 = CARTESIAN_POINT('Ctrl Pts',(32.2860034094053,617.706346518201,-37.4555666679615)) ;
#66232 = CARTESIAN_POINT('Ctrl Pts',(31.5515705394677,617.595124272344,-35.2417057246827)) ;
#66233 = CARTESIAN_POINT('Ctrl Pts',(29.2928260283501,617.483902026487,-34.659773469075)) ;
#66234 = CARTESIAN_POINT('Ctrl Pts',(27.5800809010859,617.37267978063,-36.2431580734666)) ;
#66235 = CARTESIAN_POINT('Ctrl Pts',(27.9832559996343,617.261457534773,-38.5405622264581)) ;
#66236 = CARTESIAN_POINT('Ctrl Pts',(30.132705572695,617.150235288915,-39.446169146318)) ;
#66237 = CARTESIAN_POINT('Ctrl Pts',(32.0585169830119,617.039013043057,-38.1299719592266)) ;
#66238 = CARTESIAN_POINT('Ctrl Pts',(31.9950195758766,616.9277907972,-35.7981098946905)) ;
#66239 = CARTESIAN_POINT('Ctrl Pts',(30.0015829148602,616.816568551343,-34.5882249381669)) ;
#66240 = CARTESIAN_POINT('Ctrl Pts',(27.9028912368749,616.705346305486,-35.6079881248491)) ;
#66241 = CARTESIAN_POINT('Ctrl Pts',(27.6282710239295,616.594109768654,-37.9244882573162)) ;
#66242 = CARTESIAN_POINT('Ctrl Pts',(28.8212760718149,616.519947313775,-38.9133119870574)) ;
#66243 = CARTESIAN_POINT('Ctrl Pts',(29.4945169267138,616.482858940849,-39.0444589860994)) ;
#66244 = CARTESIAN_POINT('Ctrl Pts',(28.0258055392794,618.783926575113,-37.5187199360264)) ;
#66245 = CARTESIAN_POINT('Ctrl Pts',(28.191101657974,618.746835598319,-38.1388829902218)) ;
#66246 = CARTESIAN_POINT('Ctrl Pts',(29.1902123343951,618.672670539572,-39.1896064709675)) ;
#66247 = CARTESIAN_POINT('Ctrl Pts',(31.3351931509543,618.561431398871,-38.7856066261564)) ;
#66248 = CARTESIAN_POINT('Ctrl Pts',(32.1533797045511,618.450209153014,-36.7615048748273)) ;
#66249 = CARTESIAN_POINT('Ctrl Pts',(30.8969172694545,618.338986907157,-34.9777573419897)) ;
#66250 = CARTESIAN_POINT('Ctrl Pts',(28.7160975746836,618.2277646613,-35.0670969264808)) ;
#66251 = CARTESIAN_POINT('Ctrl Pts',(27.6101744909914,618.116542415443,-36.9487087408633)) ;
#66252 = CARTESIAN_POINT('Ctrl Pts',(28.5925390240981,618.005320169585,-38.897485164783)) ;
#66253 = CARTESIAN_POINT('Ctrl Pts',(30.7628408434119,617.894097923727,-39.1274278071231)) ;
#66254 = CARTESIAN_POINT('Ctrl Pts',(32.1317601557906,617.782875677869,-37.4276831629185)) ;
#66255 = CARTESIAN_POINT('Ctrl Pts',(31.4445775297042,617.671653432013,-35.3562524861823)) ;
#66256 = CARTESIAN_POINT('Ctrl Pts',(29.3311509003384,617.560431186156,-34.8117592425087)) ;
#66257 = CARTESIAN_POINT('Ctrl Pts',(27.7285964089117,617.449208940298,-36.2932757092798)) ;
#66258 = CARTESIAN_POINT('Ctrl Pts',(28.1058329601794,617.33798669444,-38.4428747858684)) ;
#66259 = CARTESIAN_POINT('Ctrl Pts',(30.1169962165045,617.226764448583,-39.2902188616367)) ;
#66260 = CARTESIAN_POINT('Ctrl Pts',(31.9189092251107,617.115542202726,-38.0587001258951)) ;
#66261 = CARTESIAN_POINT('Ctrl Pts',(31.8594969673389,617.004319956867,-35.876860011202)) ;
#66262 = CARTESIAN_POINT('Ctrl Pts',(29.9943094250516,616.893097711011,-34.7448138355498)) ;
#66263 = CARTESIAN_POINT('Ctrl Pts',(28.0306385197095,616.781875465154,-35.6989698561946)) ;
#66264 = CARTESIAN_POINT('Ctrl Pts',(27.7736861870555,616.670638928323,-37.8664363592844)) ;
#66265 = CARTESIAN_POINT('Ctrl Pts',(28.8899384346023,616.596476473445,-38.7916434342315)) ;
#66266 = CARTESIAN_POINT('Ctrl Pts',(29.5198658760269,616.559388100518,-38.9143530008837)) ;
#66267 = CARTESIAN_POINT('Ctrl Pts',(28.1538851347994,618.860455734782,-37.4845767998963)) ;
#66268 = CARTESIAN_POINT('Ctrl Pts',(28.3078155966519,618.823364757988,-38.0620978337234)) ;
#66269 = CARTESIAN_POINT('Ctrl Pts',(29.2382280532645,618.749199699239,-39.0405742307961)) ;
#66270 = CARTESIAN_POINT('Ctrl Pts',(31.2357213420671,618.637960558539,-38.6643531604454)) ;
#66271 = CARTESIAN_POINT('Ctrl Pts',(31.9976499044024,618.526738312682,-36.779427368606)) ;
#66272 = CARTESIAN_POINT('Ctrl Pts',(30.8275810336869,618.415516066825,-35.1183291908253)) ;
#66273 = CARTESIAN_POINT('Ctrl Pts',(28.7967131253291,618.304293820967,-35.2015258418478)) ;
#66274 = CARTESIAN_POINT('Ctrl Pts',(27.7668326151852,618.19307157511,-36.9537592149134)) ;
#66275 = CARTESIAN_POINT('Ctrl Pts',(28.6816503827333,618.081849329253,-38.7685390013363)) ;
#66276 = CARTESIAN_POINT('Ctrl Pts',(30.7027236181152,617.970627083395,-38.9826709326515)) ;
#66277 = CARTESIAN_POINT('Ctrl Pts',(31.9775169021757,617.859404837538,-37.3997996578756)) ;
#66278 = CARTESIAN_POINT('Ctrl Pts',(31.3375845199407,617.74818259168,-35.4707992476819)) ;
#66279 = CARTESIAN_POINT('Ctrl Pts',(29.3694757723265,617.636960345823,-34.9637450159425)) ;
#66280 = CARTESIAN_POINT('Ctrl Pts',(27.8771119167374,617.525738099966,-36.3433933450928)) ;
#66281 = CARTESIAN_POINT('Ctrl Pts',(28.2284099207247,617.414515854109,-38.3451873452787)) ;
#66282 = CARTESIAN_POINT('Ctrl Pts',(30.1012868603142,617.303293608251,-39.1342685769555)) ;
#66283 = CARTESIAN_POINT('Ctrl Pts',(31.7793014672095,617.192071362394,-37.9874282925633)) ;
#66284 = CARTESIAN_POINT('Ctrl Pts',(31.7239743588012,617.080849116536,-35.9556101277135)) ;
#66285 = CARTESIAN_POINT('Ctrl Pts',(29.987035935243,616.969626870679,-34.9014027329326)) ;
#66286 = CARTESIAN_POINT('Ctrl Pts',(28.158385802544,616.858404624822,-35.78995158754)) ;
#66287 = CARTESIAN_POINT('Ctrl Pts',(27.9191013501814,616.747168087991,-37.8083844612528)) ;
#66288 = CARTESIAN_POINT('Ctrl Pts',(28.9586007973896,616.673005633112,-38.6699748814058)) ;
#66289 = CARTESIAN_POINT('Ctrl Pts',(29.5452148253402,616.635917260186,-38.7842470156678)) ;
#66290 = CARTESIAN_POINT('Ctrl Pts',(28.2819647303194,618.93698489445,-37.4504336637662)) ;
#66291 = CARTESIAN_POINT('Ctrl Pts',(28.4245295353296,618.899893917656,-37.9853126772251)) ;
#66292 = CARTESIAN_POINT('Ctrl Pts',(29.286243772134,618.825728858908,-38.8915419906246)) ;
#66293 = CARTESIAN_POINT('Ctrl Pts',(31.1362495331798,618.714489718209,-38.5430996947345)) ;
#66294 = CARTESIAN_POINT('Ctrl Pts',(31.8419201042538,618.603267472351,-36.7973498623847)) ;
#66295 = CARTESIAN_POINT('Ctrl Pts',(30.7582447979194,618.492045226494,-35.2589010396609)) ;
#66296 = CARTESIAN_POINT('Ctrl Pts',(28.8773286759747,618.380822980637,-35.3359547572148)) ;
#66297 = CARTESIAN_POINT('Ctrl Pts',(27.9234907393791,618.26960073478,-36.9588096889635)) ;
#66298 = CARTESIAN_POINT('Ctrl Pts',(28.7707617413686,618.158378488922,-38.6395928378894)) ;
#66299 = CARTESIAN_POINT('Ctrl Pts',(30.6426063928184,618.047156243065,-38.8379140581797)) ;
#66300 = CARTESIAN_POINT('Ctrl Pts',(31.8232736485609,617.935933997207,-37.3719161528327)) ;
#66301 = CARTESIAN_POINT('Ctrl Pts',(31.2305915101772,617.82471175135,-35.5853460091816)) ;
#66302 = CARTESIAN_POINT('Ctrl Pts',(29.4078006443147,617.713489505493,-35.1157307893762)) ;
#66303 = CARTESIAN_POINT('Ctrl Pts',(28.0256274245631,617.602267259635,-36.393510980906)) ;
#66304 = CARTESIAN_POINT('Ctrl Pts',(28.35098688127,617.491045013778,-38.247499904689)) ;
#66305 = CARTESIAN_POINT('Ctrl Pts',(30.0855775041238,617.37982276792,-38.9783182922743)) ;
#66306 = CARTESIAN_POINT('Ctrl Pts',(31.6396937093084,617.268600522063,-37.9161564592317)) ;
#66307 = CARTESIAN_POINT('Ctrl Pts',(31.5884517502634,617.157378276205,-36.034360244225)) ;
#66308 = CARTESIAN_POINT('Ctrl Pts',(29.9797624454342,617.046156030348,-35.0579916303155)) ;
#66309 = CARTESIAN_POINT('Ctrl Pts',(28.2861330853785,616.934933784491,-35.8809333188854)) ;
#66310 = CARTESIAN_POINT('Ctrl Pts',(28.0645165133074,616.82369724766,-37.7503325632211)) ;
#66311 = CARTESIAN_POINT('Ctrl Pts',(29.027263160177,616.749534792781,-38.54830632858)) ;
#66312 = CARTESIAN_POINT('Ctrl Pts',(29.5705637746533,616.712446419854,-38.6541410304521)) ;
#66313 = CARTESIAN_POINT('Ctrl Pts',(30.966214425925,618.708683906554,-35.756042592416)) ;
#66314 = CARTESIAN_POINT('Ctrl Pts',(30.5447271292425,618.671595533668,-35.3972599237611)) ;
#66315 = CARTESIAN_POINT('Ctrl Pts',(29.3205834535133,618.597433078829,-35.1420827411956)) ;
#66316 = CARTESIAN_POINT('Ctrl Pts',(27.9972039226441,618.486196542039,-36.4809009401573)) ;
#66317 = CARTESIAN_POINT('Ctrl Pts',(28.4097628334874,618.374974296181,-38.3181294473258)) ;
#66318 = CARTESIAN_POINT('Ctrl Pts',(30.176119912037,618.263752050324,-38.9670975304033)) ;
#66319 = CARTESIAN_POINT('Ctrl Pts',(31.6793162682317,618.152529804466,-37.8338793668858)) ;
#66320 = CARTESIAN_POINT('Ctrl Pts',(31.5407722192233,618.041307558609,-35.9565753284643)) ;
#66321 = CARTESIAN_POINT('Ctrl Pts',(29.8878958341303,617.930085312751,-35.0560755863368)) ;
#66322 = CARTESIAN_POINT('Ctrl Pts',(28.2355306242915,617.818863066894,-35.9576425061243)) ;
#66323 = CARTESIAN_POINT('Ctrl Pts',(28.0982927495265,617.707640821037,-37.8349519584651)) ;
#66324 = CARTESIAN_POINT('Ctrl Pts',(29.6019442250164,617.596418575179,-38.9672669406877)) ;
#66325 = CARTESIAN_POINT('Ctrl Pts',(31.3682722736937,617.485196329322,-38.3167362318318)) ;
#66326 = CARTESIAN_POINT('Ctrl Pts',(31.7783015947118,617.373974083464,-36.4796186607374)) ;
#66327 = CARTESIAN_POINT('Ctrl Pts',(30.4561717720678,617.262751837607,-35.1398028414488)) ;
#66328 = CARTESIAN_POINT('Ctrl Pts',(28.6138177650868,617.15152959175,-35.5253308468272)) ;
#66329 = CARTESIAN_POINT('Ctrl Pts',(27.9397269121408,617.040307345893,-37.2829048646609)) ;
#66330 = CARTESIAN_POINT('Ctrl Pts',(29.0522159057932,616.929085100035,-38.801506501169)) ;
#66331 = CARTESIAN_POINT('Ctrl Pts',(30.930684117803,616.817862854177,-38.6895508033932)) ;
#66332 = CARTESIAN_POINT('Ctrl Pts',(31.8555878909266,616.70664060832,-37.049378113421)) ;
#66333 = CARTESIAN_POINT('Ctrl Pts',(30.9745593872839,616.595402487695,-35.3857503772719)) ;
#66334 = CARTESIAN_POINT('Ctrl Pts',(29.7287969659281,616.521238449023,-35.2770475901246)) ;
#66335 = CARTESIAN_POINT('Ctrl Pts',(29.2217315764459,616.484148492302,-35.4990562403977)) ;
#66336 = CARTESIAN_POINT('Ctrl Pts',(31.0526478907908,618.785673866071,-35.6544964574366)) ;
#66337 = CARTESIAN_POINT('Ctrl Pts',(30.59735614607,618.748585493184,-35.2669384255025)) ;
#66338 = CARTESIAN_POINT('Ctrl Pts',(29.2750327586311,618.674423038346,-34.9912953264635)) ;
#66339 = CARTESIAN_POINT('Ctrl Pts',(27.8455145257457,618.563186501555,-36.4374904513627)) ;
#66340 = CARTESIAN_POINT('Ctrl Pts',(28.2911618033656,618.451964255698,-38.4220697709847)) ;
#66341 = CARTESIAN_POINT('Ctrl Pts',(30.1991856095934,618.34074200984,-39.1230868909266)) ;
#66342 = CARTESIAN_POINT('Ctrl Pts',(31.8229424749996,618.229519763982,-37.8989814934968)) ;
#66343 = CARTESIAN_POINT('Ctrl Pts',(31.6732868097158,618.118297518125,-35.8711124740704)) ;
#66344 = CARTESIAN_POINT('Ctrl Pts',(29.8878451627196,618.007075272268,-34.898390159683)) ;
#66345 = CARTESIAN_POINT('Ctrl Pts',(28.1029556886482,617.895853026411,-35.872265242333)) ;
#66346 = CARTESIAN_POINT('Ctrl Pts',(27.9547109563982,617.784630780554,-37.9001401098902)) ;
#66347 = CARTESIAN_POINT('Ctrl Pts',(29.5789594429271,617.673408534696,-39.1232698883848)) ;
#66348 = CARTESIAN_POINT('Ctrl Pts',(31.4869518910064,617.562186288838,-38.4205648157511)) ;
#66349 = CARTESIAN_POINT('Ctrl Pts',(31.9298666986942,617.450964042981,-36.4361053295835)) ;
#66350 = CARTESIAN_POINT('Ctrl Pts',(30.5016984040935,617.339741797123,-34.9888325724452)) ;
#66351 = CARTESIAN_POINT('Ctrl Pts',(28.5115825053845,617.228519551267,-35.4052809911498)) ;
#66352 = CARTESIAN_POINT('Ctrl Pts',(27.7834276998808,617.117297305409,-37.303817310877)) ;
#66353 = CARTESIAN_POINT('Ctrl Pts',(28.9851413906358,617.006075059552,-38.9442150027259)) ;
#66354 = CARTESIAN_POINT('Ctrl Pts',(31.0142679535953,616.894852813694,-38.8232801480506)) ;
#66355 = CARTESIAN_POINT('Ctrl Pts',(32.0133515698245,616.783630567837,-37.0515610676928)) ;
#66356 = CARTESIAN_POINT('Ctrl Pts',(31.0616621411529,616.672392447211,-35.2545057815218)) ;
#66357 = CARTESIAN_POINT('Ctrl Pts',(29.7159861248389,616.59822840854,-35.1370847299129)) ;
#66358 = CARTESIAN_POINT('Ctrl Pts',(29.1682526873617,616.561138451819,-35.376899088546)) ;
#66359 = CARTESIAN_POINT('Ctrl Pts',(31.1390813556564,618.862663825587,-35.5529503224572)) ;
#66360 = CARTESIAN_POINT('Ctrl Pts',(30.6499851628975,618.825575452702,-35.1366169272439)) ;
#66361 = CARTESIAN_POINT('Ctrl Pts',(29.2294820637489,618.751412997863,-34.8405079117313)) ;
#66362 = CARTESIAN_POINT('Ctrl Pts',(27.6938251288474,618.640176461073,-36.3940799625681)) ;
#66363 = CARTESIAN_POINT('Ctrl Pts',(28.1725607732438,618.528954215214,-38.5260100946437)) ;
#66364 = CARTESIAN_POINT('Ctrl Pts',(30.2222513071496,618.417731969357,-39.2790762514498)) ;
#66365 = CARTESIAN_POINT('Ctrl Pts',(31.9665686817676,618.306509723498,-37.9640836201077)) ;
#66366 = CARTESIAN_POINT('Ctrl Pts',(31.8058014002084,618.195287477643,-35.7856496196763)) ;
#66367 = CARTESIAN_POINT('Ctrl Pts',(29.887794491309,618.084065231784,-34.7407047330292)) ;
#66368 = CARTESIAN_POINT('Ctrl Pts',(27.970380753005,617.972842985929,-35.7868879785417)) ;
#66369 = CARTESIAN_POINT('Ctrl Pts',(27.8111291632698,617.861620740071,-37.9653282613151)) ;
#66370 = CARTESIAN_POINT('Ctrl Pts',(29.555974660838,617.750398494213,-39.2792728360818)) ;
#66371 = CARTESIAN_POINT('Ctrl Pts',(31.6056315083191,617.639176248354,-38.5243933996705)) ;
#66372 = CARTESIAN_POINT('Ctrl Pts',(32.0814318026768,617.527954002496,-36.3925919984296)) ;
#66373 = CARTESIAN_POINT('Ctrl Pts',(30.5472250361189,617.416731756641,-34.8378623034417)) ;
#66374 = CARTESIAN_POINT('Ctrl Pts',(28.4093472456823,617.305509510783,-35.2852311354723)) ;
#66375 = CARTESIAN_POINT('Ctrl Pts',(27.627128487621,617.194287264926,-37.3247297570932)) ;
#66376 = CARTESIAN_POINT('Ctrl Pts',(28.9180668754785,617.083065019068,-39.0869235042828)) ;
#66377 = CARTESIAN_POINT('Ctrl Pts',(31.0978517893876,616.971842773211,-38.9570094927081)) ;
#66378 = CARTESIAN_POINT('Ctrl Pts',(32.1711152487225,616.860620527352,-37.0537440219648)) ;
#66379 = CARTESIAN_POINT('Ctrl Pts',(31.1487648950217,616.749382406728,-35.123261185772)) ;
#66380 = CARTESIAN_POINT('Ctrl Pts',(29.7031752837495,616.675218368056,-34.9971218697011)) ;
#66381 = CARTESIAN_POINT('Ctrl Pts',(29.1147737982774,616.638128411336,-35.2547419366944)) ;
#66382 = CARTESIAN_POINT('Ctrl Pts',(31.225514820522,618.939653785104,-35.4514041874778)) ;
#66383 = CARTESIAN_POINT('Ctrl Pts',(30.7026141797248,618.902565412218,-35.0062954289854)) ;
#66384 = CARTESIAN_POINT('Ctrl Pts',(29.1839313688666,618.828402957379,-34.6897204969993)) ;
#66385 = CARTESIAN_POINT('Ctrl Pts',(27.542135731949,618.717166420589,-36.3506694737735)) ;
#66386 = CARTESIAN_POINT('Ctrl Pts',(28.0539597431221,618.605944174731,-38.6299504183026)) ;
#66387 = CARTESIAN_POINT('Ctrl Pts',(30.245317004706,618.494721928873,-39.4350656119731)) ;
#66388 = CARTESIAN_POINT('Ctrl Pts',(32.1101948885357,618.383499683015,-38.0291857467188)) ;
#66389 = CARTESIAN_POINT('Ctrl Pts',(31.9383159907009,618.272277437158,-35.7001867652823)) ;
#66390 = CARTESIAN_POINT('Ctrl Pts',(29.8877438198984,618.161055191301,-34.5830193063753)) ;
#66391 = CARTESIAN_POINT('Ctrl Pts',(27.8378058173618,618.049832945444,-35.7015107147504)) ;
#66392 = CARTESIAN_POINT('Ctrl Pts',(27.6675473701414,617.938610699587,-38.0305164127401)) ;
#66393 = CARTESIAN_POINT('Ctrl Pts',(29.5329898787488,617.827388453729,-39.435275783779)) ;
#66394 = CARTESIAN_POINT('Ctrl Pts',(31.7243111256318,617.716166207871,-38.6282219835898)) ;
#66395 = CARTESIAN_POINT('Ctrl Pts',(32.2329969066591,617.604943962014,-36.3490786672756)) ;
#66396 = CARTESIAN_POINT('Ctrl Pts',(30.5927516681446,617.493721716156,-34.6868920344383)) ;
#66397 = CARTESIAN_POINT('Ctrl Pts',(28.30711198598,617.3824994703,-35.1651812797949)) ;
#66398 = CARTESIAN_POINT('Ctrl Pts',(27.4708292753611,617.271277224442,-37.3456422033094)) ;
#66399 = CARTESIAN_POINT('Ctrl Pts',(28.850992360321,617.160054978585,-39.2296320058398)) ;
#66400 = CARTESIAN_POINT('Ctrl Pts',(31.1814356251799,617.048832732727,-39.0907388373655)) ;
#66401 = CARTESIAN_POINT('Ctrl Pts',(32.3288789276206,616.937610486869,-37.0559269762365)) ;
#66402 = CARTESIAN_POINT('Ctrl Pts',(31.2358676488905,616.826372366244,-34.9920165900219)) ;
#66403 = CARTESIAN_POINT('Ctrl Pts',(29.6903644426602,616.752208327571,-34.8571590094894)) ;
#66404 = CARTESIAN_POINT('Ctrl Pts',(29.0612949091931,616.715118370851,-35.1325847848427)) ;
#66405 = CARTESIAN_POINT('Ctrl Pts',(177.897694697021,618.70737979957,-37.5528661540161)) ;
#66406 = CARTESIAN_POINT('Ctrl Pts',(178.074357719121,618.67028873138,-38.21568333661)) ;
#66407 = CARTESIAN_POINT('Ctrl Pts',(179.142367773108,618.596123581238,-39.3386569433631)) ;
#66408 = CARTESIAN_POINT('Ctrl Pts',(181.434831201881,618.484884349142,-38.9068792628014)) ;
#66409 = CARTESIAN_POINT('Ctrl Pts',(182.309288473454,618.373662103284,-36.7435478468336)) ;
#66410 = CARTESIAN_POINT('Ctrl Pts',(180.96634315944,618.262439857427,-34.8371019767222)) ;
#66411 = CARTESIAN_POINT('Ctrl Pts',(178.635482469432,618.15121761157,-34.9325952570238)) ;
#66412 = CARTESIAN_POINT('Ctrl Pts',(177.453462591305,618.039995365713,-36.9436498335109)) ;
#66413 = CARTESIAN_POINT('Ctrl Pts',(178.503397865929,617.928773119855,-39.0264888319928)) ;
#66414 = CARTESIAN_POINT('Ctrl Pts',(180.822992703844,617.817550873998,-39.2722505476327)) ;
#66415 = CARTESIAN_POINT('Ctrl Pts',(182.286079804168,617.70632862814,-37.4555779132756)) ;
#66416 = CARTESIAN_POINT('Ctrl Pts',(181.551623139311,617.595106382283,-35.2416494112721)) ;
#66417 = CARTESIAN_POINT('Ctrl Pts',(179.292809605602,617.483884136426,-34.6596980177064)) ;
#66418 = CARTESIAN_POINT('Ctrl Pts',(177.580012828887,617.372661890568,-36.24312800518)) ;
#66419 = CARTESIAN_POINT('Ctrl Pts',(177.983200659197,617.261439644711,-38.5405958736053)) ;
#66420 = CARTESIAN_POINT('Ctrl Pts',(180.132717649286,617.150217398854,-39.4462222224988)) ;
#66421 = CARTESIAN_POINT('Ctrl Pts',(182.058589537804,617.038995152996,-38.1299665592977)) ;
#66422 = CARTESIAN_POINT('Ctrl Pts',(181.995096791643,616.927772907139,-35.7980147600553)) ;
#66423 = CARTESIAN_POINT('Ctrl Pts',(180.001605178594,616.816550661281,-34.5880440328019)) ;
#66424 = CARTESIAN_POINT('Ctrl Pts',(177.902860787058,616.705328415424,-35.607823574719)) ;
#66425 = CARTESIAN_POINT('Ctrl Pts',(177.628241205805,616.594091799347,-37.9243184862603)) ;
#66426 = CARTESIAN_POINT('Ctrl Pts',(178.821262568672,616.519929265223,-38.913342614159)) ;
#66427 = CARTESIAN_POINT('Ctrl Pts',(179.494515316492,616.482840813051,-39.0444902412825)) ;
#66428 = CARTESIAN_POINT('Ctrl Pts',(178.025790309075,618.783918479111,-37.518719085898)) ;
#66429 = CARTESIAN_POINT('Ctrl Pts',(178.191086351244,618.746827410922,-38.1388888059787)) ;
#66430 = CARTESIAN_POINT('Ctrl Pts',(179.19037772995,618.672662260779,-39.1896072327892)) ;
#66431 = CARTESIAN_POINT('Ctrl Pts',(181.335337818873,618.561423028684,-38.7856113040128)) ;
#66432 = CARTESIAN_POINT('Ctrl Pts',(182.15353012827,618.450200782827,-36.761474522537)) ;
#66433 = CARTESIAN_POINT('Ctrl Pts',(180.89699357287,618.338978536969,-34.9776945713462)) ;
#66434 = CARTESIAN_POINT('Ctrl Pts',(178.716106807064,618.227756291112,-35.0670435539458)) ;
#66435 = CARTESIAN_POINT('Ctrl Pts',(177.610141306776,618.116534045255,-36.9487014024733)) ;
#66436 = CARTESIAN_POINT('Ctrl Pts',(178.592520886643,618.005311799398,-38.8975248678011)) ;
#66437 = CARTESIAN_POINT('Ctrl Pts',(180.762866675961,617.89408955354,-39.127473605398)) ;
#66438 = CARTESIAN_POINT('Ctrl Pts',(182.131814767968,617.782867307682,-37.4276906355025)) ;
#66439 = CARTESIAN_POINT('Ctrl Pts',(181.444615045002,617.671645061825,-35.3562123222927)) ;
#66440 = CARTESIAN_POINT('Ctrl Pts',(179.331139725258,617.560422815968,-34.8117052661604)) ;
#66441 = CARTESIAN_POINT('Ctrl Pts',(177.728548957449,617.449200570111,-36.2932530562397)) ;
#66442 = CARTESIAN_POINT('Ctrl Pts',(178.105794584794,617.337978324254,-38.4428955855411)) ;
#66443 = CARTESIAN_POINT('Ctrl Pts',(180.117005798173,617.226756078396,-39.2902514689432)) ;
#66444 = CARTESIAN_POINT('Ctrl Pts',(181.918961844844,617.115533832538,-38.0586872795428)) ;
#66445 = CARTESIAN_POINT('Ctrl Pts',(181.859554394874,617.004311586681,-35.8767796094398)) ;
#66446 = CARTESIAN_POINT('Ctrl Pts',(179.99432946089,616.893089340824,-34.7446616937728)) ;
#66447 = CARTESIAN_POINT('Ctrl Pts',(178.030623998811,616.781867094967,-35.6988258428971)) ;
#66448 = CARTESIAN_POINT('Ctrl Pts',(177.773674189261,616.67063047889,-37.8662711635459)) ;
#66449 = CARTESIAN_POINT('Ctrl Pts',(178.889933308802,616.596467944766,-38.7916587857429)) ;
#66450 = CARTESIAN_POINT('Ctrl Pts',(179.519867141423,616.559379492594,-38.9143680173957)) ;
#66451 = CARTESIAN_POINT('Ctrl Pts',(178.153885921129,618.860457158654,-37.48457201778)) ;
#66452 = CARTESIAN_POINT('Ctrl Pts',(178.307814983366,618.823366090463,-38.0620942753473)) ;
#66453 = CARTESIAN_POINT('Ctrl Pts',(179.238387686792,618.749200940321,-39.0405575222152)) ;
#66454 = CARTESIAN_POINT('Ctrl Pts',(181.235844435868,618.637961708226,-38.6643433452239)) ;
#66455 = CARTESIAN_POINT('Ctrl Pts',(181.997771783088,618.526739462368,-36.7794011982405)) ;
#66456 = CARTESIAN_POINT('Ctrl Pts',(180.827643986302,618.415517216512,-35.1182871659701)) ;
#66457 = CARTESIAN_POINT('Ctrl Pts',(178.796731144695,618.304294970654,-35.2014918508676)) ;
#66458 = CARTESIAN_POINT('Ctrl Pts',(177.766820022244,618.193072724797,-36.9537529714359)) ;
#66459 = CARTESIAN_POINT('Ctrl Pts',(178.681643907358,618.081850478939,-38.7685609036097)) ;
#66460 = CARTESIAN_POINT('Ctrl Pts',(180.702740648078,617.970628233082,-38.9826966631632)) ;
#66461 = CARTESIAN_POINT('Ctrl Pts',(181.977549731769,617.859405987224,-37.3998033577292)) ;
#66462 = CARTESIAN_POINT('Ctrl Pts',(181.337606950692,617.748183741368,-35.4707752333133)) ;
#66463 = CARTESIAN_POINT('Ctrl Pts',(179.369469844914,617.636961495509,-34.9637125146143)) ;
#66464 = CARTESIAN_POINT('Ctrl Pts',(177.877085086011,617.525739249652,-36.3433781072996)) ;
#66465 = CARTESIAN_POINT('Ctrl Pts',(178.228388510391,617.414517003795,-38.3451952974769)) ;
#66466 = CARTESIAN_POINT('Ctrl Pts',(180.101293947058,617.303294757937,-39.1342807153876)) ;
#66467 = CARTESIAN_POINT('Ctrl Pts',(181.779334151885,617.19207251208,-37.9874079997878)) ;
#66468 = CARTESIAN_POINT('Ctrl Pts',(181.724011998105,617.080850266222,-35.9555444588244)) ;
#66469 = CARTESIAN_POINT('Ctrl Pts',(179.987053743187,616.969628020365,-34.9012793547438)) ;
#66470 = CARTESIAN_POINT('Ctrl Pts',(178.158387210564,616.858405774508,-35.7898281110753)) ;
#66471 = CARTESIAN_POINT('Ctrl Pts',(177.919107172716,616.747169158432,-37.8082238408314)) ;
#66472 = CARTESIAN_POINT('Ctrl Pts',(178.958604048933,616.673006624308,-38.6699749573269)) ;
#66473 = CARTESIAN_POINT('Ctrl Pts',(179.545218966355,616.635918172135,-38.784245793509)) ;
#66474 = CARTESIAN_POINT('Ctrl Pts',(178.281981533183,618.936995838197,-37.4504249496618)) ;
#66475 = CARTESIAN_POINT('Ctrl Pts',(178.42454361549,618.899904770007,-37.9852997447159)) ;
#66476 = CARTESIAN_POINT('Ctrl Pts',(179.286397643634,618.825739619865,-38.891507811641)) ;
#66477 = CARTESIAN_POINT('Ctrl Pts',(181.136351052861,618.714500387769,-38.5430753864352)) ;
#66478 = CARTESIAN_POINT('Ctrl Pts',(181.842013437904,618.603278141912,-36.797327873944)) ;
#66479 = CARTESIAN_POINT('Ctrl Pts',(180.758294399734,618.492055896054,-35.2588797605942)) ;
#66480 = CARTESIAN_POINT('Ctrl Pts',(178.877355482327,618.380833650197,-35.3359401477894)) ;
#66481 = CARTESIAN_POINT('Ctrl Pts',(177.923498737714,618.26961140434,-36.9588045403982)) ;
#66482 = CARTESIAN_POINT('Ctrl Pts',(178.770766928071,618.158389158483,-38.6395969394181)) ;
#66483 = CARTESIAN_POINT('Ctrl Pts',(180.642614620195,618.047166912625,-38.8379197209285)) ;
#66484 = CARTESIAN_POINT('Ctrl Pts',(181.823284695569,617.935944666768,-37.3719160799559)) ;
#66485 = CARTESIAN_POINT('Ctrl Pts',(181.230598856383,617.82472242091,-35.5853381443338)) ;
#66486 = CARTESIAN_POINT('Ctrl Pts',(179.40779996457,617.713500175053,-35.1157197630681)) ;
#66487 = CARTESIAN_POINT('Ctrl Pts',(178.025621214571,617.602277929196,-36.3935031583595)) ;
#66488 = CARTESIAN_POINT('Ctrl Pts',(178.350982435989,617.491055683339,-38.2474950094128)) ;
#66489 = CARTESIAN_POINT('Ctrl Pts',(180.085582095943,617.379833437481,-38.978309961832)) ;
#66490 = CARTESIAN_POINT('Ctrl Pts',(181.639706458925,617.268611191623,-37.9161287200328)) ;
#66491 = CARTESIAN_POINT('Ctrl Pts',(181.588469601338,617.157388945766,-36.0343093082089)) ;
#66492 = CARTESIAN_POINT('Ctrl Pts',(179.979778025483,617.046166699909,-35.0578970157147)) ;
#66493 = CARTESIAN_POINT('Ctrl Pts',(178.286150422316,616.934944454052,-35.8808303792533)) ;
#66494 = CARTESIAN_POINT('Ctrl Pts',(178.064540156171,616.823707837974,-37.7501765181169)) ;
#66495 = CARTESIAN_POINT('Ctrl Pts',(179.027274789061,616.74954530385,-38.5482911289107)) ;
#66496 = CARTESIAN_POINT('Ctrl Pts',(179.570570791287,616.712456851679,-38.6541235696222)) ;
#66497 = CARTESIAN_POINT('Ctrl Pts',(180.966205148325,618.708673473592,-35.7560589666014)) ;
#66498 = CARTESIAN_POINT('Ctrl Pts',(180.544722495663,618.671585021452,-35.3972784943684)) ;
#66499 = CARTESIAN_POINT('Ctrl Pts',(179.32047618186,618.59742248736,-35.1421985305261)) ;
#66500 = CARTESIAN_POINT('Ctrl Pts',(177.997134246167,618.486185871316,-36.4809786807734)) ;
#66501 = CARTESIAN_POINT('Ctrl Pts',(178.409698571325,618.374963625458,-38.3182006227404)) ;
#66502 = CARTESIAN_POINT('Ctrl Pts',(180.176091219243,618.263741379601,-38.9671432459311)) ;
#66503 = CARTESIAN_POINT('Ctrl Pts',(181.679302531611,618.152519133743,-37.8339066297847)) ;
#66504 = CARTESIAN_POINT('Ctrl Pts',(181.540768571018,618.041296887886,-35.9565841108305)) ;
#66505 = CARTESIAN_POINT('Ctrl Pts',(179.887889235789,617.930074642029,-35.0560751610428)) ;
#66506 = CARTESIAN_POINT('Ctrl Pts',(178.235520635928,617.818852396172,-35.9576425269521)) ;
#66507 = CARTESIAN_POINT('Ctrl Pts',(178.098283704118,617.707630150314,-37.8349583017894)) ;
#66508 = CARTESIAN_POINT('Ctrl Pts',(179.601942656214,617.596407904457,-38.9672775885259)) ;
#66509 = CARTESIAN_POINT('Ctrl Pts',(181.368279105258,617.485185658599,-38.3167449143955)) ;
#66510 = CARTESIAN_POINT('Ctrl Pts',(181.778311152633,617.373963412741,-36.4796215614246)) ;
#66511 = CARTESIAN_POINT('Ctrl Pts',(180.456178212682,617.262741166885,-35.1398043372561)) ;
#66512 = CARTESIAN_POINT('Ctrl Pts',(178.613818725341,617.151518921027,-35.5253403081863)) ;
#66513 = CARTESIAN_POINT('Ctrl Pts',(177.939732202149,617.04029667517,-37.2829349308624)) ;
#66514 = CARTESIAN_POINT('Ctrl Pts',(179.052230194514,616.929074429313,-38.8015585494034)) ;
#66515 = CARTESIAN_POINT('Ctrl Pts',(180.930725121544,616.817852183455,-38.6896374882165)) ;
#66516 = CARTESIAN_POINT('Ctrl Pts',(181.855632185436,616.706629937598,-37.0494726460127)) ;
#66517 = CARTESIAN_POINT('Ctrl Pts',(180.974626616194,616.595391473834,-35.38588823888)) ;
#66518 = CARTESIAN_POINT('Ctrl Pts',(179.728787178078,616.521227092025,-35.2770659283329)) ;
#66519 = CARTESIAN_POINT('Ctrl Pts',(179.221724915396,616.484136792166,-35.499079332989)) ;
#66520 = CARTESIAN_POINT('Ctrl Pts',(181.052660894574,618.785683087004,-35.6544870935763)) ;
#66521 = CARTESIAN_POINT('Ctrl Pts',(180.597365161011,618.748594634865,-35.2669237685818)) ;
#66522 = CARTESIAN_POINT('Ctrl Pts',(179.274904746605,618.674432100772,-34.9913802354821)) ;
#66523 = CARTESIAN_POINT('Ctrl Pts',(177.845398849837,618.563195484728,-36.4375628642004)) ;
#66524 = CARTESIAN_POINT('Ctrl Pts',(178.291060790793,618.45197323887,-38.4221743458409)) ;
#66525 = CARTESIAN_POINT('Ctrl Pts',(180.199160759592,618.340750993013,-39.1231778291386)) ;
#66526 = CARTESIAN_POINT('Ctrl Pts',(181.822965898053,618.229528747155,-37.89902828659)) ;
#66527 = CARTESIAN_POINT('Ctrl Pts',(181.673318170411,618.118306501298,-35.8710991938916)) ;
#66528 = CARTESIAN_POINT('Ctrl Pts',(179.887838021533,618.00708425544,-34.8983476932453)) ;
#66529 = CARTESIAN_POINT('Ctrl Pts',(178.102909581328,617.895862009583,-35.8722425205302)) ;
#66530 = CARTESIAN_POINT('Ctrl Pts',(177.95466293548,617.784639763726,-37.9001643280707)) ;
#66531 = CARTESIAN_POINT('Ctrl Pts',(179.578951625178,617.673417517868,-39.1233229492518)) ;
#66532 = CARTESIAN_POINT('Ctrl Pts',(181.486990886596,617.562195272011,-38.4206018545543)) ;
#66533 = CARTESIAN_POINT('Ctrl Pts',(181.929917399976,617.450973026154,-36.4360968711268)) ;
#66534 = CARTESIAN_POINT('Ctrl Pts',(180.501717489587,617.339750780296,-34.9887939701297)) ;
#66535 = CARTESIAN_POINT('Ctrl Pts',(178.511556307444,617.228528534439,-35.4052592305405)) ;
#66536 = CARTESIAN_POINT('Ctrl Pts',(177.783391776534,617.117306288582,-37.3038553601391)) ;
#66537 = CARTESIAN_POINT('Ctrl Pts',(178.985138957165,617.006084042724,-38.9443092436912)) ;
#66538 = CARTESIAN_POINT('Ctrl Pts',(181.014334513363,616.894861796867,-38.823409412269)) ;
#66539 = CARTESIAN_POINT('Ctrl Pts',(182.013441445692,616.78363955101,-37.0516637656131)) ;
#66540 = CARTESIAN_POINT('Ctrl Pts',(181.061757967411,616.672401087247,-35.2546197397083)) ;
#66541 = CARTESIAN_POINT('Ctrl Pts',(179.71597213899,616.598236705436,-35.137067253513)) ;
#66542 = CARTESIAN_POINT('Ctrl Pts',(179.168231245286,616.561146405578,-35.3768914913441)) ;
#66543 = CARTESIAN_POINT('Ctrl Pts',(181.139116640822,618.862692700416,-35.5529152205513)) ;
#66544 = CARTESIAN_POINT('Ctrl Pts',(180.650007826359,618.825604248277,-35.1365690427952)) ;
#66545 = CARTESIAN_POINT('Ctrl Pts',(179.22933331135,618.751441714185,-34.840561940438)) ;
#66546 = CARTESIAN_POINT('Ctrl Pts',(177.693663453507,618.64020509814,-36.3941470476275)) ;
#66547 = CARTESIAN_POINT('Ctrl Pts',(178.172423010261,618.528982852283,-38.5261480689413)) ;
#66548 = CARTESIAN_POINT('Ctrl Pts',(180.222230299942,618.417760606425,-39.2792124123461)) ;
#66549 = CARTESIAN_POINT('Ctrl Pts',(181.966629264493,618.306538360567,-37.9641499433951)) ;
#66550 = CARTESIAN_POINT('Ctrl Pts',(181.805867769802,618.19531611471,-35.7856142769528)) ;
#66551 = CARTESIAN_POINT('Ctrl Pts',(179.887786807278,618.084093868853,-34.740620225448)) ;
#66552 = CARTESIAN_POINT('Ctrl Pts',(177.970298526728,617.972871622996,-35.7868425141084)) ;
#66553 = CARTESIAN_POINT('Ctrl Pts',(177.811042166842,617.861649377138,-37.9653703543519)) ;
#66554 = CARTESIAN_POINT('Ctrl Pts',(179.555960594141,617.750427131281,-39.2793683099778)) ;
#66555 = CARTESIAN_POINT('Ctrl Pts',(181.605702667935,617.639204885423,-38.5244587947131)) ;
#66556 = CARTESIAN_POINT('Ctrl Pts',(182.081523647319,617.527982639565,-36.3925721808291)) ;
#66557 = CARTESIAN_POINT('Ctrl Pts',(180.547256766493,617.416760393708,-34.8377836030034)) ;
#66558 = CARTESIAN_POINT('Ctrl Pts',(178.409293889545,617.305538147851,-35.2851781528945)) ;
#66559 = CARTESIAN_POINT('Ctrl Pts',(177.627051350921,617.194315901994,-37.3247757894159)) ;
#66560 = CARTESIAN_POINT('Ctrl Pts',(178.918047719815,617.083093656137,-39.0870599379789)) ;
#66561 = CARTESIAN_POINT('Ctrl Pts',(181.097943905179,616.971871410279,-38.9571813363214)) ;
#66562 = CARTESIAN_POINT('Ctrl Pts',(182.17125070595,616.860649164421,-37.0538548852137)) ;
#66563 = CARTESIAN_POINT('Ctrl Pts',(181.148889318629,616.749410700658,-35.1233512405364)) ;
#66564 = CARTESIAN_POINT('Ctrl Pts',(179.703157099901,616.675246318848,-34.9970685786932)) ;
#66565 = CARTESIAN_POINT('Ctrl Pts',(179.114737575175,616.63815601899,-35.2547036496991)) ;
#66566 = CARTESIAN_POINT('Ctrl Pts',(181.225572387071,618.939702313829,-35.4513433475264)) ;
#66567 = CARTESIAN_POINT('Ctrl Pts',(180.702650491707,618.902613861688,-35.0062143170084)) ;
#66568 = CARTESIAN_POINT('Ctrl Pts',(179.183761876095,618.828451327597,-34.6897436453939)) ;
#66569 = CARTESIAN_POINT('Ctrl Pts',(177.541928057179,618.717214711552,-36.3507312310546)) ;
#66570 = CARTESIAN_POINT('Ctrl Pts',(178.05378522973,618.605992465694,-38.6301217920418)) ;
#66571 = CARTESIAN_POINT('Ctrl Pts',(180.24529984029,618.494770219836,-39.4352469955538)) ;
#66572 = CARTESIAN_POINT('Ctrl Pts',(182.110292630934,618.383547973979,-38.0292716002004)) ;
#66573 = CARTESIAN_POINT('Ctrl Pts',(181.938417369194,618.272325728121,-35.7001293600139)) ;
#66574 = CARTESIAN_POINT('Ctrl Pts',(179.887735593022,618.161103482264,-34.5828927576505)) ;
#66575 = CARTESIAN_POINT('Ctrl Pts',(177.837687472128,618.049881236407,-35.7014425076866)) ;
#66576 = CARTESIAN_POINT('Ctrl Pts',(177.667421398203,617.93865899055,-38.0305763806333)) ;
#66577 = CARTESIAN_POINT('Ctrl Pts',(179.532969563104,617.827436744692,-39.4354136707037)) ;
#66578 = CARTESIAN_POINT('Ctrl Pts',(181.724414449273,617.716214498834,-38.6283157348719)) ;
#66579 = CARTESIAN_POINT('Ctrl Pts',(182.233129894662,617.604992252977,-36.3490474905313)) ;
#66580 = CARTESIAN_POINT('Ctrl Pts',(180.592796043397,617.49377000712,-34.6867732358772)) ;
#66581 = CARTESIAN_POINT('Ctrl Pts',(178.307031471648,617.382547761263,-35.1650970752487)) ;
#66582 = CARTESIAN_POINT('Ctrl Pts',(177.470710925308,617.271325515405,-37.3456962186925)) ;
#66583 = CARTESIAN_POINT('Ctrl Pts',(178.850956482466,617.160103269548,-39.2298106322666)) ;
#66584 = CARTESIAN_POINT('Ctrl Pts',(181.181553296997,617.04888102369,-39.090953260374)) ;
#66585 = CARTESIAN_POINT('Ctrl Pts',(182.329059966206,616.937658777833,-37.0560460048141)) ;
#66586 = CARTESIAN_POINT('Ctrl Pts',(181.236020669846,616.82642031407,-34.9920827413645)) ;
#66587 = CARTESIAN_POINT('Ctrl Pts',(179.690342060812,616.752255932259,-34.8570699038733)) ;
#66588 = CARTESIAN_POINT('Ctrl Pts',(179.061243905064,616.715165632402,-35.1325158080541)) ;
#66589 = CARTESIAN_POINT('Ctrl Pts',(27.8977541328133,503.71371705854,-36.4914598282363)) ;
#66590 = CARTESIAN_POINT('Ctrl Pts',(28.0744148476991,503.75080794899,-35.8286657489856)) ;
#66591 = CARTESIAN_POINT('Ctrl Pts',(29.1420348524557,503.824972921393,-34.7056981288284)) ;
#66592 = CARTESIAN_POINT('Ctrl Pts',(31.4345215740258,503.936211975746,-35.1374809470855)) ;
#66593 = CARTESIAN_POINT('Ctrl Pts',(32.308955341866,504.047434221604,-37.300709716721)) ;
#66594 = CARTESIAN_POINT('Ctrl Pts',(30.9661821194376,504.158656467462,-39.207060501706)) ;
#66595 = CARTESIAN_POINT('Ctrl Pts',(28.6354901248007,504.269878713319,-39.1115873870729)) ;
#66596 = CARTESIAN_POINT('Ctrl Pts',(27.4535723582629,504.381100959177,-37.1006559333751)) ;
#66597 = CARTESIAN_POINT('Ctrl Pts',(28.5034591693879,504.492323205034,-35.017943588011)) ;
#66598 = CARTESIAN_POINT('Ctrl Pts',(30.8229284125707,504.603545450891,-34.7721976604505)) ;
#66599 = CARTESIAN_POINT('Ctrl Pts',(32.2859340628205,504.714767696748,-36.5887649780755)) ;
#66600 = CARTESIAN_POINT('Ctrl Pts',(31.5515227471191,504.825989942606,-38.8025634523413)) ;
#66601 = CARTESIAN_POINT('Ctrl Pts',(29.2928420280764,504.937212188463,-39.3844784587789)) ;
#66602 = CARTESIAN_POINT('Ctrl Pts',(27.5801447756113,505.048434434321,-37.8011369057575)) ;
#66603 = CARTESIAN_POINT('Ctrl Pts',(27.9833082997518,505.159656680178,-35.5037932649875)) ;
#66604 = CARTESIAN_POINT('Ctrl Pts',(30.1326956298288,505.270878926035,-34.5982066401904)) ;
#66605 = CARTESIAN_POINT('Ctrl Pts',(32.0584516367322,505.382101171892,-35.9143520425694)) ;
#66606 = CARTESIAN_POINT('Ctrl Pts',(31.994950262249,505.49332341775,-38.2461341646642)) ;
#66607 = CARTESIAN_POINT('Ctrl Pts',(30.0015652353422,505.604545663607,-39.455939676632)) ;
#66608 = CARTESIAN_POINT('Ctrl Pts',(27.9029216508139,505.715767909465,-38.4361905755117)) ;
#66609 = CARTESIAN_POINT('Ctrl Pts',(27.6282984704502,505.82700437211,-36.1196715697614)) ;
#66610 = CARTESIAN_POINT('Ctrl Pts',(28.8212881368412,505.9011667528,-35.1310360076914)) ;
#66611 = CARTESIAN_POINT('Ctrl Pts',(29.4945182216124,505.938255051539,-34.9998895262024)) ;
#66612 = CARTESIAN_POINT('Ctrl Pts',(28.025819091536,503.637196597121,-36.5255993814499)) ;
#66613 = CARTESIAN_POINT('Ctrl Pts',(28.1911153557476,503.67428748757,-35.9054423458996)) ;
#66614 = CARTESIAN_POINT('Ctrl Pts',(29.1900561700542,503.748452459973,-34.8547143865864)) ;
#66615 = CARTESIAN_POINT('Ctrl Pts',(31.3350689482234,503.859691514327,-35.2587209414953)) ;
#66616 = CARTESIAN_POINT('Ctrl Pts',(32.1532510506677,503.970913760184,-37.2827908343813)) ;
#66617 = CARTESIAN_POINT('Ctrl Pts',(30.8968574178533,504.082136006042,-39.066507509811)) ;
#66618 = CARTESIAN_POINT('Ctrl Pts',(28.7160970830456,504.1933582519,-38.9771761087029)) ;
#66619 = CARTESIAN_POINT('Ctrl Pts',(27.6102111958496,504.304580497757,-37.0956063601769)) ;
#66620 = CARTESIAN_POINT('Ctrl Pts',(28.5925595795087,504.415802743614,-35.1468733306579)) ;
#66621 = CARTESIAN_POINT('Ctrl Pts',(30.7628191140068,504.527024989472,-34.916936053447)) ;
#66622 = CARTESIAN_POINT('Ctrl Pts',(32.1317107131565,504.638247235329,-36.6166449643197)) ;
#66623 = CARTESIAN_POINT('Ctrl Pts',(31.4445435240122,504.749469481186,-38.6880314508418)) ;
#66624 = CARTESIAN_POINT('Ctrl Pts',(29.331162033701,504.860691727044,-39.2325123033906)) ;
#66625 = CARTESIAN_POINT('Ctrl Pts',(27.7286413049629,504.971913972901,-37.751025919421)) ;
#66626 = CARTESIAN_POINT('Ctrl Pts',(28.1058696233806,505.083136218759,-35.6014686640044)) ;
#66627 = CARTESIAN_POINT('Ctrl Pts',(30.1169884860854,505.194358464616,-34.7541377444173)) ;
#66628 = CARTESIAN_POINT('Ctrl Pts',(31.9188620601296,505.305580710473,-35.985616504782)) ;
#66629 = CARTESIAN_POINT('Ctrl Pts',(31.8594456812183,505.41680295633,-38.1673968399694)) ;
#66630 = CARTESIAN_POINT('Ctrl Pts',(29.9942936110689,505.528025202188,-39.2993764749454)) ;
#66631 = CARTESIAN_POINT('Ctrl Pts',(28.0306541869974,505.639247448046,-38.3452270651154)) ;
#66632 = CARTESIAN_POINT('Ctrl Pts',(27.7736973088966,505.75048391069,-36.1777279814988)) ;
#66633 = CARTESIAN_POINT('Ctrl Pts',(28.8899428489712,505.824646291381,-35.2526906001961)) ;
#66634 = CARTESIAN_POINT('Ctrl Pts',(29.5198645496706,505.86173459012,-35.1299806730418)) ;
#66635 = CARTESIAN_POINT('Ctrl Pts',(28.1538840502585,503.560676135701,-36.5597389346635)) ;
#66636 = CARTESIAN_POINT('Ctrl Pts',(28.3078158637961,503.597767026151,-35.9822189428135)) ;
#66637 = CARTESIAN_POINT('Ctrl Pts',(29.2380774876526,503.671931998554,-35.0037306443446)) ;
#66638 = CARTESIAN_POINT('Ctrl Pts',(31.2356163224208,503.783171052908,-35.379960935905)) ;
#66639 = CARTESIAN_POINT('Ctrl Pts',(31.9975467594692,503.894393298765,-37.2648719520417)) ;
#66640 = CARTESIAN_POINT('Ctrl Pts',(30.8275327162687,504.005615544622,-38.9259545179161)) ;
#66641 = CARTESIAN_POINT('Ctrl Pts',(28.7967040412908,504.11683779048,-38.842764830333)) ;
#66642 = CARTESIAN_POINT('Ctrl Pts',(27.7668500334364,504.228060036338,-37.0905567869785)) ;
#66643 = CARTESIAN_POINT('Ctrl Pts',(28.6816599896297,504.339282282195,-35.2758030733051)) ;
#66644 = CARTESIAN_POINT('Ctrl Pts',(30.7027098154429,504.450504528052,-35.0616744464435)) ;
#66645 = CARTESIAN_POINT('Ctrl Pts',(31.9774873634924,504.561726773909,-36.6445249505641)) ;
#66646 = CARTESIAN_POINT('Ctrl Pts',(31.3375643009055,504.672949019767,-38.5734994493424)) ;
#66647 = CARTESIAN_POINT('Ctrl Pts',(29.3694820393255,504.784171265625,-39.0805461480023)) ;
#66648 = CARTESIAN_POINT('Ctrl Pts',(27.8771378343143,504.895393511482,-37.7009149330845)) ;
#66649 = CARTESIAN_POINT('Ctrl Pts',(28.2284309470095,505.006615757339,-35.6991440630211)) ;
#66650 = CARTESIAN_POINT('Ctrl Pts',(30.1012813423422,505.117838003197,-34.9100688486442)) ;
#66651 = CARTESIAN_POINT('Ctrl Pts',(31.7792724835269,505.229060249053,-36.0568809669946)) ;
#66652 = CARTESIAN_POINT('Ctrl Pts',(31.7239411001876,505.340282494911,-38.0886595152747)) ;
#66653 = CARTESIAN_POINT('Ctrl Pts',(29.9870219867958,505.451504740768,-39.1428132732589)) ;
#66654 = CARTESIAN_POINT('Ctrl Pts',(28.1583867231806,505.562726986626,-38.254263554719)) ;
#66655 = CARTESIAN_POINT('Ctrl Pts',(27.9190961473432,505.673963449271,-36.2357843932362)) ;
#66656 = CARTESIAN_POINT('Ctrl Pts',(28.9585975611013,505.748125829961,-35.3743451927006)) ;
#66657 = CARTESIAN_POINT('Ctrl Pts',(29.5452108777287,505.7852141287,-35.2600718198812)) ;
#66658 = CARTESIAN_POINT('Ctrl Pts',(28.2819490089811,503.484155674282,-36.5938784878771)) ;
#66659 = CARTESIAN_POINT('Ctrl Pts',(28.4245163718447,503.521246564731,-36.0589955397274)) ;
#66660 = CARTESIAN_POINT('Ctrl Pts',(29.2860988052509,503.595411537134,-35.1527469021027)) ;
#66661 = CARTESIAN_POINT('Ctrl Pts',(31.1361636966183,503.706650591488,-35.5012009303147)) ;
#66662 = CARTESIAN_POINT('Ctrl Pts',(31.8418424682708,503.817872837345,-37.2469530697021)) ;
#66663 = CARTESIAN_POINT('Ctrl Pts',(30.7582080146843,503.929095083203,-38.7854015260211)) ;
#66664 = CARTESIAN_POINT('Ctrl Pts',(28.8773109995357,504.040317329061,-38.708353551963)) ;
#66665 = CARTESIAN_POINT('Ctrl Pts',(27.923488871023,504.151539574918,-37.0855072137802)) ;
#66666 = CARTESIAN_POINT('Ctrl Pts',(28.7707603997505,504.262761820775,-35.4047328159522)) ;
#66667 = CARTESIAN_POINT('Ctrl Pts',(30.6426005168789,504.373984066633,-35.20641283944)) ;
#66668 = CARTESIAN_POINT('Ctrl Pts',(31.8232640138284,504.48520631249,-36.6724049368083)) ;
#66669 = CARTESIAN_POINT('Ctrl Pts',(31.2305850777988,504.596428558347,-38.458967447843)) ;
#66670 = CARTESIAN_POINT('Ctrl Pts',(29.4078020449499,504.707650804205,-38.9285799926139)) ;
#66671 = CARTESIAN_POINT('Ctrl Pts',(28.0256343636658,504.818873050062,-37.650803946748)) ;
#66672 = CARTESIAN_POINT('Ctrl Pts',(28.3509922706383,504.930095295921,-35.796819462038)) ;
#66673 = CARTESIAN_POINT('Ctrl Pts',(30.085574198599,505.041317541777,-35.0659999528711)) ;
#66674 = CARTESIAN_POINT('Ctrl Pts',(31.6396829069243,505.152539787634,-36.1281454292072)) ;
#66675 = CARTESIAN_POINT('Ctrl Pts',(31.588436519157,505.263762033491,-38.0099221905798)) ;
#66676 = CARTESIAN_POINT('Ctrl Pts',(29.9797503625226,505.374984279349,-38.9862500715725)) ;
#66677 = CARTESIAN_POINT('Ctrl Pts',(28.2861192593641,505.486206525207,-38.1633000443226)) ;
#66678 = CARTESIAN_POINT('Ctrl Pts',(28.0644949857897,505.597442987851,-36.2938408049737)) ;
#66679 = CARTESIAN_POINT('Ctrl Pts',(29.0272522732312,505.671605368542,-35.4959997852053)) ;
#66680 = CARTESIAN_POINT('Ctrl Pts',(29.5705572057869,505.70869366728,-35.3901629667207)) ;
#66681 = CARTESIAN_POINT('Ctrl Pts',(30.9662230989071,503.71243666145,-38.2882930583653)) ;
#66682 = CARTESIAN_POINT('Ctrl Pts',(30.5447314608486,503.749524960246,-38.6470777806288)) ;
#66683 = CARTESIAN_POINT('Ctrl Pts',(29.3206848071998,503.823687340995,-38.9023459275938)) ;
#66684 = CARTESIAN_POINT('Ctrl Pts',(27.9972632285561,503.934923803697,-37.5634843593214)) ;
#66685 = CARTESIAN_POINT('Ctrl Pts',(28.4098167138482,504.046146049554,-35.7262492988704)) ;
#66686 = CARTESIAN_POINT('Ctrl Pts',(30.1761400278415,504.157368295412,-35.0772583107157)) ;
#66687 = CARTESIAN_POINT('Ctrl Pts',(31.6793239520214,504.268590541268,-36.2104609029163)) ;
#66688 = CARTESIAN_POINT('Ctrl Pts',(31.5407717996218,504.379812787126,-38.0877489028456)) ;
#66689 = CARTESIAN_POINT('Ctrl Pts',(29.8878999526904,504.491035032984,-38.9882411575102)) ;
#66690 = CARTESIAN_POINT('Ctrl Pts',(28.2355391737867,504.602257278842,-38.0866757916757)) ;
#66691 = CARTESIAN_POINT('Ctrl Pts',(28.0983010872981,504.713479524699,-36.2093732450915)) ;
#66692 = CARTESIAN_POINT('Ctrl Pts',(29.6019455967526,504.824701770556,-35.0770627132181)) ;
#66693 = CARTESIAN_POINT('Ctrl Pts',(31.3682656918741,504.935924016413,-35.7275911699162)) ;
#66694 = CARTESIAN_POINT('Ctrl Pts',(31.7782928184681,505.04714626227,-37.5647021897656)) ;
#66695 = CARTESIAN_POINT('Ctrl Pts',(30.4561667902946,505.158368508128,-38.9045152432018)) ;
#66696 = CARTESIAN_POINT('Ctrl Pts',(28.6138192880979,505.269590753986,-38.5189930982623)) ;
#66697 = CARTESIAN_POINT('Ctrl Pts',(27.9397253017718,505.380812999843,-36.7614367744957)) ;
#66698 = CARTESIAN_POINT('Ctrl Pts',(29.0522068826185,505.4920352457,-35.2428536331562)) ;
#66699 = CARTESIAN_POINT('Ctrl Pts',(30.9306493708943,505.603257491557,-35.3548410007556)) ;
#66700 = CARTESIAN_POINT('Ctrl Pts',(31.855549839045,505.714479737415,-36.9950215303291)) ;
#66701 = CARTESIAN_POINT('Ctrl Pts',(30.9744952911176,505.82571756818,-38.6586996936158)) ;
#66702 = CARTESIAN_POINT('Ctrl Pts',(29.7288050765599,505.899881316993,-38.7672899890708)) ;
#66703 = CARTESIAN_POINT('Ctrl Pts',(29.2217365356442,505.936970983854,-38.5452851357495)) ;
#66704 = CARTESIAN_POINT('Ctrl Pts',(31.052637147478,503.635463816439,-38.3898167925285)) ;
#66705 = CARTESIAN_POINT('Ctrl Pts',(30.5973485790445,503.672552115236,-38.7773703471557)) ;
#66706 = CARTESIAN_POINT('Ctrl Pts',(29.2751528382168,503.746714495985,-39.0531069423909)) ;
#66707 = CARTESIAN_POINT('Ctrl Pts',(27.8456138828295,503.857950958687,-37.6068899556027)) ;
#66708 = CARTESIAN_POINT('Ctrl Pts',(28.2912476007037,503.969173204544,-35.6223378434861)) ;
#66709 = CARTESIAN_POINT('Ctrl Pts',(30.1992019713357,504.080395450401,-34.9213080928504)) ;
#66710 = CARTESIAN_POINT('Ctrl Pts',(31.82291735531,504.191617696258,-36.1453755223364)) ;
#66711 = CARTESIAN_POINT('Ctrl Pts',(31.6732555223731,504.302839942116,-38.1731921830943)) ;
#66712 = CARTESIAN_POINT('Ctrl Pts',(29.8878496233149,504.414062187973,-39.1458896045665)) ;
#66713 = CARTESIAN_POINT('Ctrl Pts',(28.1029957718174,504.525284433831,-38.172033025464)) ;
#66714 = CARTESIAN_POINT('Ctrl Pts',(27.9547533719926,504.636506679688,-36.1442006516409)) ;
#66715 = CARTESIAN_POINT('Ctrl Pts',(29.57896627286,504.747728925545,-34.9210968115423)) ;
#66716 = CARTESIAN_POINT('Ctrl Pts',(31.486917166518,504.858951171402,-35.6237873112628)) ;
#66717 = CARTESIAN_POINT('Ctrl Pts',(31.9298219518792,504.97017341726,-37.6082054366929)) ;
#66718 = CARTESIAN_POINT('Ctrl Pts',(30.5016824295189,505.081395663117,-39.0554502026324)) ;
#66719 = CARTESIAN_POINT('Ctrl Pts',(28.5116079390836,505.192617908975,-38.6390153089833)) ;
#66720 = CARTESIAN_POINT('Ctrl Pts',(27.7834623287988,505.303840154832,-36.7405309018553)) ;
#66721 = CARTESIAN_POINT('Ctrl Pts',(28.9851472511506,505.41506240069,-35.1001815282536)) ;
#66722 = CARTESIAN_POINT('Ctrl Pts',(31.0142109718713,505.526284646547,-35.221148502858)) ;
#66723 = CARTESIAN_POINT('Ctrl Pts',(32.0132737576184,505.637506892404,-36.9928454426161)) ;
#66724 = CARTESIAN_POINT('Ctrl Pts',(31.0615726380295,505.74874472317,-38.7899241528505)) ;
#66725 = CARTESIAN_POINT('Ctrl Pts',(29.7159978667007,505.822908471983,-38.9072216641162)) ;
#66726 = CARTESIAN_POINT('Ctrl Pts',(29.1682704879214,505.859998138843,-38.6674155500032)) ;
#66727 = CARTESIAN_POINT('Ctrl Pts',(31.1390511960491,503.558490971429,-38.4913405266917)) ;
#66728 = CARTESIAN_POINT('Ctrl Pts',(30.6499656972406,503.595579270226,-38.9076629136824)) ;
#66729 = CARTESIAN_POINT('Ctrl Pts',(29.2296208692337,503.669741650975,-39.2038679571878)) ;
#66730 = CARTESIAN_POINT('Ctrl Pts',(27.6939645371028,503.780978113676,-37.6502955518842)) ;
#66731 = CARTESIAN_POINT('Ctrl Pts',(28.1726784875591,503.892200359534,-35.5184263881019)) ;
#66732 = CARTESIAN_POINT('Ctrl Pts',(30.22226391483,504.003422605391,-34.7653578749853)) ;
#66733 = CARTESIAN_POINT('Ctrl Pts',(31.9665107585986,504.114644851248,-36.0802901417566)) ;
#66734 = CARTESIAN_POINT('Ctrl Pts',(31.8057392451245,504.225867097105,-38.2586354633428)) ;
#66735 = CARTESIAN_POINT('Ctrl Pts',(29.8877992939395,504.337089342963,-39.3035380516228)) ;
#66736 = CARTESIAN_POINT('Ctrl Pts',(27.9704523698482,504.448311588821,-38.2573902592525)) ;
#66737 = CARTESIAN_POINT('Ctrl Pts',(27.811205656687,504.559533834678,-36.0790280581902)) ;
#66738 = CARTESIAN_POINT('Ctrl Pts',(29.5559869489674,504.670756080535,-34.7651309098665)) ;
#66739 = CARTESIAN_POINT('Ctrl Pts',(31.605568641162,504.781978326392,-35.5199834526092)) ;
#66740 = CARTESIAN_POINT('Ctrl Pts',(32.0813510852903,504.893200572249,-37.6517086836202)) ;
#66741 = CARTESIAN_POINT('Ctrl Pts',(30.5471980687433,505.004422818107,-39.206385162063)) ;
#66742 = CARTESIAN_POINT('Ctrl Pts',(28.4093965900692,505.115645063965,-38.7590375197042)) ;
#66743 = CARTESIAN_POINT('Ctrl Pts',(27.6271993558257,505.226867309822,-36.719625029215)) ;
#66744 = CARTESIAN_POINT('Ctrl Pts',(28.9180876196827,505.338089555679,-34.957509423351)) ;
#66745 = CARTESIAN_POINT('Ctrl Pts',(31.0977725728485,505.449311801536,-35.0874560049603)) ;
#66746 = CARTESIAN_POINT('Ctrl Pts',(32.1709976761917,505.560534047393,-36.9906693549032)) ;
#66747 = CARTESIAN_POINT('Ctrl Pts',(31.1486499849412,505.671771878159,-38.9211486120855)) ;
#66748 = CARTESIAN_POINT('Ctrl Pts',(29.7031906568414,505.745935626972,-39.0471533391616)) ;
#66749 = CARTESIAN_POINT('Ctrl Pts',(29.1148044401986,505.783025293834,-38.7895459642568)) ;
#66750 = CARTESIAN_POINT('Ctrl Pts',(31.2254652446201,503.481518126418,-38.592864260855)) ;
#66751 = CARTESIAN_POINT('Ctrl Pts',(30.7025828154366,503.518606425215,-39.0379554802091)) ;
#66752 = CARTESIAN_POINT('Ctrl Pts',(29.1840889002507,503.592768805964,-39.3546289719847)) ;
#66753 = CARTESIAN_POINT('Ctrl Pts',(27.5423151913762,503.704005268666,-37.6937011481655)) ;
#66754 = CARTESIAN_POINT('Ctrl Pts',(28.0541093744144,503.815227514523,-35.4145149327176)) ;
#66755 = CARTESIAN_POINT('Ctrl Pts',(30.2453258583243,503.92644976038,-34.60940765712)) ;
#66756 = CARTESIAN_POINT('Ctrl Pts',(32.1101041618871,504.037672006237,-36.0152047611767)) ;
#66757 = CARTESIAN_POINT('Ctrl Pts',(31.9382229678757,504.148894252095,-38.3440787435914)) ;
#66758 = CARTESIAN_POINT('Ctrl Pts',(29.8877489645639,504.260116497952,-39.4611864986793)) ;
#66759 = CARTESIAN_POINT('Ctrl Pts',(27.837908967879,504.37133874381,-38.3427474930407)) ;
#66760 = CARTESIAN_POINT('Ctrl Pts',(27.6676579413815,504.482560989668,-36.0138554647395)) ;
#66761 = CARTESIAN_POINT('Ctrl Pts',(29.5330076250747,504.593783235524,-34.6091650081907)) ;
#66762 = CARTESIAN_POINT('Ctrl Pts',(31.7242201158058,504.705005481382,-35.4161795939558)) ;
#66763 = CARTESIAN_POINT('Ctrl Pts',(32.2328802187016,504.81622772724,-37.6952119305476)) ;
#66764 = CARTESIAN_POINT('Ctrl Pts',(30.5927137079678,504.927449973096,-39.3573201214937)) ;
#66765 = CARTESIAN_POINT('Ctrl Pts',(28.3071852410547,505.038672218954,-38.8790597304251)) ;
#66766 = CARTESIAN_POINT('Ctrl Pts',(27.4709363828527,505.149894464812,-36.6987191565747)) ;
#66767 = CARTESIAN_POINT('Ctrl Pts',(28.8510279882148,505.261116710669,-34.8148373184484)) ;
#66768 = CARTESIAN_POINT('Ctrl Pts',(31.1813341738256,505.372338956526,-34.9537635070626)) ;
#66769 = CARTESIAN_POINT('Ctrl Pts',(32.328721594765,505.483561202383,-36.9884932671904)) ;
#66770 = CARTESIAN_POINT('Ctrl Pts',(31.235727331853,505.59479903315,-39.0523730713204)) ;
#66771 = CARTESIAN_POINT('Ctrl Pts',(29.6903834469821,505.668962781963,-39.1870850142069)) ;
#66772 = CARTESIAN_POINT('Ctrl Pts',(29.0613383924757,505.706052448823,-38.9116763785105)) ;
#66773 = CARTESIAN_POINT('Ctrl Pts',(177.897717671888,503.713737563885,-36.4914564811708)) ;
#66774 = CARTESIAN_POINT('Ctrl Pts',(178.074379770071,503.750828565321,-35.8286481930038)) ;
#66775 = CARTESIAN_POINT('Ctrl Pts',(179.142242773597,503.82499364871,-34.7056767914726)) ;
#66776 = CARTESIAN_POINT('Ctrl Pts',(181.434708312697,503.936232814051,-35.1374547995427)) ;
#66777 = CARTESIAN_POINT('Ctrl Pts',(182.309156092825,504.047455059908,-37.3007467834596)) ;
#66778 = CARTESIAN_POINT('Ctrl Pts',(180.9662761525,504.158677305767,-39.2071568534577)) ;
#66779 = CARTESIAN_POINT('Ctrl Pts',(178.635481119123,504.269899551625,-39.111671513941)) ;
#66780 = CARTESIAN_POINT('Ctrl Pts',(177.453501211943,504.381121797482,-37.1006641248506)) ;
#66781 = CARTESIAN_POINT('Ctrl Pts',(178.503419192989,504.492344043339,-35.0178734541952)) ;
#66782 = CARTESIAN_POINT('Ctrl Pts',(180.822967024381,504.603566289197,-34.7721178983205)) ;
#66783 = CARTESIAN_POINT('Ctrl Pts',(182.286023668365,504.714788535052,-36.5887505440602)) ;
#66784 = CARTESIAN_POINT('Ctrl Pts',(181.551584491592,504.82601078091,-38.8026295560003)) ;
#66785 = CARTESIAN_POINT('Ctrl Pts',(179.292821524194,504.937233026769,-39.3845668730687)) ;
#66786 = CARTESIAN_POINT('Ctrl Pts',(177.580062568716,505.048455272626,-37.8011699949904)) ;
#66787 = CARTESIAN_POINT('Ctrl Pts',(177.983241051759,505.159677518484,-35.503748604351)) ;
#66788 = CARTESIAN_POINT('Ctrl Pts',(180.132708648325,505.270899764341,-34.5981362170648)) ;
#66789 = CARTESIAN_POINT('Ctrl Pts',(182.058536181622,505.382122010198,-35.9143487880221)) ;
#66790 = CARTESIAN_POINT('Ctrl Pts',(181.995039985258,505.493344256054,-38.24623454224)) ;
#66791 = CARTESIAN_POINT('Ctrl Pts',(180.001588542046,505.604566501912,-39.4561424861251)) ;
#66792 = CARTESIAN_POINT('Ctrl Pts',(177.902882844478,505.71578874777,-38.43637509949)) ;
#66793 = CARTESIAN_POINT('Ctrl Pts',(177.628263058505,505.82702530589,-36.1198778771031)) ;
#66794 = CARTESIAN_POINT('Ctrl Pts',(178.821272510594,505.901187782059,-35.1310002461774)) ;
#66795 = CARTESIAN_POINT('Ctrl Pts',(179.494516518593,505.938276176274,-34.9998530865222)) ;
#66796 = CARTESIAN_POINT('Ctrl Pts',(178.025801529032,503.637205871377,-36.5256006623227)) ;
#66797 = CARTESIAN_POINT('Ctrl Pts',(178.191097618669,503.674296872814,-35.9054358429339)) ;
#66798 = CARTESIAN_POINT('Ctrl Pts',(179.190256920894,503.748461956203,-34.854713682631)) ;
#66799 = CARTESIAN_POINT('Ctrl Pts',(181.335230818161,503.859701121544,-35.2587121466989)) ;
#66800 = CARTESIAN_POINT('Ctrl Pts',(182.153418760753,503.970923367401,-37.2828232002907)) ;
#66801 = CARTESIAN_POINT('Ctrl Pts',(180.896936440721,504.082145613258,-39.0665794958116)) ;
#66802 = CARTESIAN_POINT('Ctrl Pts',(178.716099075358,504.193367859116,-38.9772374501662)) ;
#66803 = CARTESIAN_POINT('Ctrl Pts',(177.610164872749,504.304590104974,-37.0956133719672)) ;
#66804 = CARTESIAN_POINT('Ctrl Pts',(178.592533691474,504.415812350831,-35.1468243734714)) ;
#66805 = CARTESIAN_POINT('Ctrl Pts',(180.762847472397,504.527034596688,-34.9168801307035)) ;
#66806 = CARTESIAN_POINT('Ctrl Pts',(182.131774620067,504.638256842545,-36.6166350624903)) ;
#66807 = CARTESIAN_POINT('Ctrl Pts',(181.444587468748,504.749479088403,-38.6880784980957)) ;
#66808 = CARTESIAN_POINT('Ctrl Pts',(179.331147801914,504.86070133426,-39.2325753874353)) ;
#66809 = CARTESIAN_POINT('Ctrl Pts',(177.72858358049,504.971923580118,-37.751050402843)) ;
#66810 = CARTESIAN_POINT('Ctrl Pts',(178.105822543221,505.083145825975,-35.6014395014372)) ;
#66811 = CARTESIAN_POINT('Ctrl Pts',(180.116998636827,505.194368071832,-34.7540920065066)) ;
#66812 = CARTESIAN_POINT('Ctrl Pts',(181.918923123416,505.305590317689,-35.9856226706786)) ;
#66813 = CARTESIAN_POINT('Ctrl Pts',(181.859512117469,505.416812563547,-38.1674805825633)) ;
#66814 = CARTESIAN_POINT('Ctrl Pts',(179.994314478408,505.528034809404,-39.2995460001091)) ;
#66815 = CARTESIAN_POINT('Ctrl Pts',(178.030634387015,505.639257055262,-38.3453879600819)) ;
#66816 = CARTESIAN_POINT('Ctrl Pts',(177.773682968319,505.750493613383,-36.1779285194202)) ;
#66817 = CARTESIAN_POINT('Ctrl Pts',(178.889937101816,505.82465608955,-35.2526728635555)) ;
#66818 = CARTESIAN_POINT('Ctrl Pts',(179.519866232276,505.861744483766,-35.1299633923057)) ;
#66819 = CARTESIAN_POINT('Ctrl Pts',(178.153885386176,503.56067417887,-36.5597448434743)) ;
#66820 = CARTESIAN_POINT('Ctrl Pts',(178.307815467267,503.597765180306,-35.9822234928638)) ;
#66821 = CARTESIAN_POINT('Ctrl Pts',(179.238271068191,503.671930263695,-35.0037505737895)) ;
#66822 = CARTESIAN_POINT('Ctrl Pts',(181.235753323625,503.783169429037,-35.379969493855)) ;
#66823 = CARTESIAN_POINT('Ctrl Pts',(181.997681428681,503.894391674893,-37.2648996171217)) ;
#66824 = CARTESIAN_POINT('Ctrl Pts',(180.827596728942,504.005613920752,-38.9260021381655)) ;
#66825 = CARTESIAN_POINT('Ctrl Pts',(178.796717031594,504.116836166609,-38.8428033863913)) ;
#66826 = CARTESIAN_POINT('Ctrl Pts',(177.766828533554,504.228058412467,-37.0905626190838)) ;
#66827 = CARTESIAN_POINT('Ctrl Pts',(178.68164818996,504.339280658324,-35.2757752927476)) ;
#66828 = CARTESIAN_POINT('Ctrl Pts',(180.702727920414,504.450502904182,-35.0616423630866)) ;
#66829 = CARTESIAN_POINT('Ctrl Pts',(181.977525571768,504.561725150037,-36.6445195809203)) ;
#66830 = CARTESIAN_POINT('Ctrl Pts',(181.337590445906,504.672947395896,-38.5735274401913)) ;
#66831 = CARTESIAN_POINT('Ctrl Pts',(179.369474079635,504.784169641753,-39.0805839018018)) ;
#66832 = CARTESIAN_POINT('Ctrl Pts',(177.877104592264,504.895391887611,-37.7009308106956)) ;
#66833 = CARTESIAN_POINT('Ctrl Pts',(178.228404034682,505.006614133468,-35.6991303985234)) ;
#66834 = CARTESIAN_POINT('Ctrl Pts',(180.101288625331,505.117836379325,-34.9100477959482)) ;
#66835 = CARTESIAN_POINT('Ctrl Pts',(181.779310065209,505.229058625183,-36.0568965533351)) ;
#66836 = CARTESIAN_POINT('Ctrl Pts',(181.72398424968,505.340280871041,-38.0887266228865)) ;
#66837 = CARTESIAN_POINT('Ctrl Pts',(179.987040414768,505.451503116897,-39.1429495140928)) ;
#66838 = CARTESIAN_POINT('Ctrl Pts',(178.158385929553,505.562725362755,-38.2544008206738)) ;
#66839 = CARTESIAN_POINT('Ctrl Pts',(177.919102878132,505.673961920876,-36.2359791617375)) ;
#66840 = CARTESIAN_POINT('Ctrl Pts',(178.958601693041,505.748124397043,-35.3743454809335)) ;
#66841 = CARTESIAN_POINT('Ctrl Pts',(179.545215945959,505.785212791258,-35.2600736980892)) ;
#66842 = CARTESIAN_POINT('Ctrl Pts',(178.281969243322,503.484142486362,-36.5938890246262)) ;
#66843 = CARTESIAN_POINT('Ctrl Pts',(178.424533315865,503.521233487799,-36.0590111427939)) ;
#66844 = CARTESIAN_POINT('Ctrl Pts',(179.286285215488,503.595398571188,-35.152787464948)) ;
#66845 = CARTESIAN_POINT('Ctrl Pts',(181.136275829091,503.706637736529,-35.5012268410111)) ;
#66846 = CARTESIAN_POINT('Ctrl Pts',(181.84194409661,503.817859982386,-37.2469760339526)) ;
#66847 = CARTESIAN_POINT('Ctrl Pts',(180.758257017163,503.929082228244,-38.7854247805194)) ;
#66848 = CARTESIAN_POINT('Ctrl Pts',(178.87733498783,504.040304474101,-38.7083693226163)) ;
#66849 = CARTESIAN_POINT('Ctrl Pts',(177.923492194359,504.151526719959,-37.0855118662004)) ;
#66850 = CARTESIAN_POINT('Ctrl Pts',(178.770762688445,504.262748965816,-35.4047262120238)) ;
#66851 = CARTESIAN_POINT('Ctrl Pts',(180.64260836843,504.373971211673,-35.2064045954696)) ;
#66852 = CARTESIAN_POINT('Ctrl Pts',(181.823276523471,504.48519345753,-36.6724040993504)) ;
#66853 = CARTESIAN_POINT('Ctrl Pts',(181.230593423062,504.596415703388,-38.4589763822867)) ;
#66854 = CARTESIAN_POINT('Ctrl Pts',(179.407800357355,504.707637949245,-38.9285924161684)) ;
#66855 = CARTESIAN_POINT('Ctrl Pts',(178.025625604036,504.818860195103,-37.6508112185482)) ;
#66856 = CARTESIAN_POINT('Ctrl Pts',(178.350985526144,504.93008244096,-35.7968212956097)) ;
#66857 = CARTESIAN_POINT('Ctrl Pts',(180.085578613834,505.041304686817,-35.0660035853901)) ;
#66858 = CARTESIAN_POINT('Ctrl Pts',(181.639697007003,505.152526932675,-36.1281704359915)) ;
#66859 = CARTESIAN_POINT('Ctrl Pts',(181.588456381889,505.263749178532,-38.0099726632097)) ;
#66860 = CARTESIAN_POINT('Ctrl Pts',(179.979766351128,505.37497142439,-38.9863530280767)) ;
#66861 = CARTESIAN_POINT('Ctrl Pts',(178.286137472091,505.486193670247,-38.1634136812656)) ;
#66862 = CARTESIAN_POINT('Ctrl Pts',(178.064522787946,505.597430228368,-36.2940298040548)) ;
#66863 = CARTESIAN_POINT('Ctrl Pts',(179.027266284264,505.671592704535,-35.4960180983116)) ;
#66864 = CARTESIAN_POINT('Ctrl Pts',(179.570565659642,505.708681098751,-35.3901840038727)) ;
#66865 = CARTESIAN_POINT('Ctrl Pts',(180.966211923875,503.712449228157,-38.2882733352088)) ;
#66866 = CARTESIAN_POINT('Ctrl Pts',(180.544725879619,503.749537622418,-38.6470554114846)) ;
#66867 = CARTESIAN_POINT('Ctrl Pts',(179.320554395332,503.82370009863,-38.9022063717596)) ;
#66868 = CARTESIAN_POINT('Ctrl Pts',(177.997185744815,503.934936656795,-37.5633992739045)) ;
#66869 = CARTESIAN_POINT('Ctrl Pts',(178.409746192673,504.046158902652,-35.7261726101518)) ;
#66870 = CARTESIAN_POINT('Ctrl Pts',(180.176112949347,504.157381148509,-35.0772113129443)) ;
#66871 = CARTESIAN_POINT('Ctrl Pts',(181.679313189748,504.268603394366,-36.2104342869482)) ;
#66872 = CARTESIAN_POINT('Ctrl Pts',(181.540771709607,504.379825640224,-38.087743183612)) ;
#66873 = CARTESIAN_POINT('Ctrl Pts',(179.88789431332,504.491047886081,-38.9882452844909)) ;
#66874 = CARTESIAN_POINT('Ctrl Pts',(178.235528027901,504.602270131939,-38.0866781045897)) ;
#66875 = CARTESIAN_POINT('Ctrl Pts',(178.098290323385,504.713492377796,-36.2093668187347)) ;
#66876 = CARTESIAN_POINT('Ctrl Pts',(179.601943814894,504.824714623653,-35.0770506193662)) ;
#66877 = CARTESIAN_POINT('Ctrl Pts',(181.36827414496,504.93593686951,-35.7275819122057)) ;
#66878 = CARTESIAN_POINT('Ctrl Pts',(181.778304157799,505.047159115368,-37.5647011898004)) ;
#66879 = CARTESIAN_POINT('Ctrl Pts',(180.456173380299,505.158381361225,-38.9045175683596)) ;
#66880 = CARTESIAN_POINT('Ctrl Pts',(178.613817724806,505.269603607083,-38.5189875961006)) ;
#66881 = CARTESIAN_POINT('Ctrl Pts',(177.939727930398,505.380825852941,-36.761408185579)) ;
#66882 = CARTESIAN_POINT('Ctrl Pts',(179.052219255809,505.492048098798,-35.2428008227509)) ;
#66883 = CARTESIAN_POINT('Ctrl Pts',(180.930694777575,505.603270344655,-35.3547472317361)) ;
#66884 = CARTESIAN_POINT('Ctrl Pts',(181.855599490743,505.714492590512,-36.9949177133331)) ;
#66885 = CARTESIAN_POINT('Ctrl Pts',(180.974577666776,505.825730800284,-38.6585326954567)) ;
#66886 = CARTESIAN_POINT('Ctrl Pts',(179.728794440342,505.899894928103,-38.7672677976822)) ;
#66887 = CARTESIAN_POINT('Ctrl Pts',(179.221729919173,505.936984973969,-38.5452579363092)) ;
#66888 = CARTESIAN_POINT('Ctrl Pts',(181.052651241069,503.635454107785,-38.3898262273626)) ;
#66889 = CARTESIAN_POINT('Ctrl Pts',(180.597358481875,503.672542502045,-38.7773856345679)) ;
#66890 = CARTESIAN_POINT('Ctrl Pts',(179.274998179785,503.746704978258,-39.0530018413153)) ;
#66891 = CARTESIAN_POINT('Ctrl Pts',(177.845484266961,503.857941536421,-37.6068111882233)) ;
#66892 = CARTESIAN_POINT('Ctrl Pts',(178.291135522085,503.96916378228,-35.6222235407668)) ;
#66893 = CARTESIAN_POINT('Ctrl Pts',(180.19917970375,504.080386028136,-34.9212101059385)) ;
#66894 = CARTESIAN_POINT('Ctrl Pts',(181.822949207867,504.191608273994,-36.1453270646094)) ;
#66895 = CARTESIAN_POINT('Ctrl Pts',(181.673295539339,504.302830519851,-38.1732118761487)) ;
#66896 = CARTESIAN_POINT('Ctrl Pts',(179.887843516382,504.414052765709,-39.1459417962898)) ;
#66897 = CARTESIAN_POINT('Ctrl Pts',(178.102943599667,504.525275011566,-38.172061368858)) ;
#66898 = CARTESIAN_POINT('Ctrl Pts',(177.954698280501,504.636497257424,-36.1441739764944)) ;
#66899 = CARTESIAN_POINT('Ctrl Pts',(179.578957390265,504.747719503281,-34.921036523388)) ;
#66900 = CARTESIAN_POINT('Ctrl Pts',(181.486962223605,504.858941749138,-35.6237458806624)) ;
#66901 = CARTESIAN_POINT('Ctrl Pts',(181.929880081602,504.970163994995,-37.6082175286907)) ;
#66902 = CARTESIAN_POINT('Ctrl Pts',(180.501703329591,505.081386240852,-39.0554984152621)) ;
#66903 = CARTESIAN_POINT('Ctrl Pts',(178.511575302249,505.192608486711,-38.6390457065327)) ;
#66904 = CARTESIAN_POINT('Ctrl Pts',(177.783417854041,505.303830732568,-36.7404936898641)) ;
#66905 = CARTESIAN_POINT('Ctrl Pts',(178.985140312065,505.415052978424,-35.1000812829108)) ;
#66906 = CARTESIAN_POINT('Ctrl Pts',(181.014285321822,505.526275224282,-35.221006732575)) ;
#66907 = CARTESIAN_POINT('Ctrl Pts',(182.013375148374,505.63749747014,-36.9927326397374)) ;
#66908 = CARTESIAN_POINT('Ctrl Pts',(181.061687986699,505.74873567991,-38.7897834929524)) ;
#66909 = CARTESIAN_POINT('Ctrl Pts',(179.715982499526,505.822899807729,-38.9072400621277)) ;
#66910 = CARTESIAN_POINT('Ctrl Pts',(179.168247151989,505.859989853596,-38.6674231483047)) ;
#66911 = CARTESIAN_POINT('Ctrl Pts',(181.139090558262,503.558458987411,-38.4913791195165)) ;
#66912 = CARTESIAN_POINT('Ctrl Pts',(180.64999108413,503.595547381672,-38.9077158576513)) ;
#66913 = CARTESIAN_POINT('Ctrl Pts',(179.229441964241,503.669709857884,-39.2037973108709)) ;
#66914 = CARTESIAN_POINT('Ctrl Pts',(177.693782789108,503.780946416049,-37.6502231025421)) ;
#66915 = CARTESIAN_POINT('Ctrl Pts',(178.172524851497,503.892168661906,-35.5182744713817)) ;
#66916 = CARTESIAN_POINT('Ctrl Pts',(180.222246458154,504.003390907763,-34.7652088989327)) ;
#66917 = CARTESIAN_POINT('Ctrl Pts',(181.966585225987,504.11461315362,-36.0802198422706)) ;
#66918 = CARTESIAN_POINT('Ctrl Pts',(181.805819369072,504.225835399478,-38.2586805686856)) ;
#66919 = CARTESIAN_POINT('Ctrl Pts',(179.887792719443,504.337057645335,-39.3036383080886)) ;
#66920 = CARTESIAN_POINT('Ctrl Pts',(177.970359171432,504.448279891193,-38.2574446331264)) ;
#66921 = CARTESIAN_POINT('Ctrl Pts',(177.811106237618,504.55950213705,-36.0789811342541)) ;
#66922 = CARTESIAN_POINT('Ctrl Pts',(179.555970965639,504.670724382908,-34.7650224274098)) ;
#66923 = CARTESIAN_POINT('Ctrl Pts',(181.605650302248,504.781946628764,-35.5199098491192)) ;
#66924 = CARTESIAN_POINT('Ctrl Pts',(182.081456005406,504.893168874622,-37.6517338675809)) ;
#66925 = CARTESIAN_POINT('Ctrl Pts',(180.547233278882,505.00439112048,-39.2064792621645)) ;
#66926 = CARTESIAN_POINT('Ctrl Pts',(178.409332879691,505.115613366337,-38.7591038169648)) ;
#66927 = CARTESIAN_POINT('Ctrl Pts',(177.627107777683,505.226835612195,-36.7195791941492)) ;
#66928 = CARTESIAN_POINT('Ctrl Pts',(178.918061368321,505.338057858052,-34.9573617430708)) ;
#66929 = CARTESIAN_POINT('Ctrl Pts',(181.097875866069,505.449280103909,-35.0872662334139)) ;
#66930 = CARTESIAN_POINT('Ctrl Pts',(182.171150806007,505.560502349766,-36.9905475661418)) ;
#66931 = CARTESIAN_POINT('Ctrl Pts',(181.14879830662,505.671740559538,-38.9210342904481)) ;
#66932 = CARTESIAN_POINT('Ctrl Pts',(179.703170558711,505.745904687357,-39.0472123265731)) ;
#66933 = CARTESIAN_POINT('Ctrl Pts',(179.114764384806,505.782994733223,-38.7895883603002)) ;
#66934 = CARTESIAN_POINT('Ctrl Pts',(181.225529875457,503.481463867038,-38.5929320116703)) ;
#66935 = CARTESIAN_POINT('Ctrl Pts',(180.702623686385,503.518552261299,-39.0380460807347)) ;
#66936 = CARTESIAN_POINT('Ctrl Pts',(179.183885748694,503.592714737512,-39.3545927804265)) ;
#66937 = CARTESIAN_POINT('Ctrl Pts',(177.542081311253,503.703951295676,-37.6936350168609)) ;
#66938 = CARTESIAN_POINT('Ctrl Pts',(178.053914180908,503.815173541534,-35.4143254019966)) ;
#66939 = CARTESIAN_POINT('Ctrl Pts',(180.245313212556,503.926395787391,-34.6092076919268)) ;
#66940 = CARTESIAN_POINT('Ctrl Pts',(182.110221244107,504.037618033248,-36.0151126199319)) ;
#66941 = CARTESIAN_POINT('Ctrl Pts',(181.938343198804,504.148840279104,-38.3441492612223)) ;
#66942 = CARTESIAN_POINT('Ctrl Pts',(179.887741922503,504.260062524963,-39.4613348198873)) ;
#66943 = CARTESIAN_POINT('Ctrl Pts',(177.837774743198,504.371284770819,-38.3428278973948)) ;
#66944 = CARTESIAN_POINT('Ctrl Pts',(177.667514194734,504.482507016678,-36.0137882920138)) ;
#66945 = CARTESIAN_POINT('Ctrl Pts',(179.53298454101,504.593729262535,-34.6090083314316)) ;
#66946 = CARTESIAN_POINT('Ctrl Pts',(181.724338380893,504.704951508392,-35.4160738175759)) ;
#66947 = CARTESIAN_POINT('Ctrl Pts',(182.233031929209,504.816173754249,-37.6952502064713)) ;
#66948 = CARTESIAN_POINT('Ctrl Pts',(180.592763228173,504.927396000106,-39.357460109067)) ;
#66949 = CARTESIAN_POINT('Ctrl Pts',(178.307090457134,505.038618245965,-38.879161927397)) ;
#66950 = CARTESIAN_POINT('Ctrl Pts',(177.470797701326,505.149840491822,-36.6986646984343)) ;
#66951 = CARTESIAN_POINT('Ctrl Pts',(178.850982424577,505.261062737679,-34.8146422032309)) ;
#66952 = CARTESIAN_POINT('Ctrl Pts',(181.181466410316,505.372284983536,-34.9535257342527)) ;
#66953 = CARTESIAN_POINT('Ctrl Pts',(182.328926463639,505.483507229393,-36.9883624925461)) ;
#66954 = CARTESIAN_POINT('Ctrl Pts',(181.235908626542,505.594745439164,-39.0522850879437)) ;
#66955 = CARTESIAN_POINT('Ctrl Pts',(179.690358617895,505.668909566983,-39.1871845910186)) ;
#66956 = CARTESIAN_POINT('Ctrl Pts',(179.061281617622,505.70599961285,-38.9117535722958)) ;
#66957 = CARTESIAN_POINT('Origin',(87.3885276254222,618.710565160552,-31.0221601717549)) ;
#66958 = CARTESIAN_POINT('',(87.2635276254222,618.585565160552,-31.0221601717549)) ;
#66959 = CARTESIAN_POINT('',(87.2635276254222,618.710565160552,-31.0221601717549)) ;
#66960 = CARTESIAN_POINT('',(73.5135276254222,618.585565160554,-31.0221601717549)) ;
#66961 = CARTESIAN_POINT('',(73.5135276254222,618.710565160554,-31.0221601717549)) ;
#66962 = CARTESIAN_POINT('',(149.888527625422,618.585565160541,-31.0221601717549)) ;
#66963 = CARTESIAN_POINT('Origin',(73.3885276254222,618.710565160554,-31.0221601717549)) ;
#66964 = CARTESIAN_POINT('',(73.3885276254222,618.585565160554,-31.1471601717549)) ;
#66965 = CARTESIAN_POINT('',(73.3885276254222,618.710565160554,-31.1471601717549)) ;
#66966 = CARTESIAN_POINT('',(73.3885276254222,618.585565160554,-39.8971601717549)) ;
#66967 = CARTESIAN_POINT('',(73.3885276254222,618.710565160554,-39.8971601717549)) ;
#66968 = CARTESIAN_POINT('',(73.3885276254222,618.585565160554,-40.272160171758)) ;
#66969 = CARTESIAN_POINT('Origin',(73.3885276254222,618.710565160554,-40.0221601717549)) ;
#66970 = CARTESIAN_POINT('',(87.2635276254222,618.585565160552,-40.0221601717549)) ;
#66971 = CARTESIAN_POINT('',(87.2635276254222,618.710565160552,-40.0221601717549)) ;
#66972 = CARTESIAN_POINT('',(73.5135276254222,618.585565160554,-40.0221601717549)) ;
#66973 = CARTESIAN_POINT('',(142.888527625422,618.585565160542,-40.0221601717549)) ;
#66974 = CARTESIAN_POINT('',(73.5135276254222,618.710565160554,-40.0221601717549)) ;
#66975 = CARTESIAN_POINT('Origin',(87.3885276254222,618.710565160552,-40.0221601717549)) ;
#66976 = CARTESIAN_POINT('',(87.3885276254222,618.585565160552,-31.1471601717549)) ;
#66977 = CARTESIAN_POINT('',(87.3885276254222,618.710565160552,-31.1471601717549)) ;
#66978 = CARTESIAN_POINT('',(87.3885276254222,618.585565160552,-39.8971601717549)) ;
#66979 = CARTESIAN_POINT('',(87.3885276254222,618.585565160552,-44.772160171758)) ;
#66980 = CARTESIAN_POINT('',(87.3885276254222,618.710565160552,-39.8971601717549)) ;
#66981 = CARTESIAN_POINT('Origin',(73.5135276254222,618.710565160554,-39.8971601717549)) ;
#66982 = CARTESIAN_POINT('Origin',(73.5135276254222,618.585565160554,-39.8971601717549)) ;
#66983 = CARTESIAN_POINT('Origin',(87.2635276254222,618.710565160552,-39.8971601717549)) ;
#66984 = CARTESIAN_POINT('Origin',(87.2635276254222,618.585565160552,-39.8971601717549)) ;
#66985 = CARTESIAN_POINT('Origin',(142.888527625422,618.585565160542,-40.1471601717549)) ;
#66986 = CARTESIAN_POINT('Origin',(87.2635276254222,618.585565160552,-40.1471601717549)) ;
#66987 = CARTESIAN_POINT('Origin',(73.5135276254222,618.585565160554,-40.1471601717549)) ;
#66988 = CARTESIAN_POINT('Origin',(73.5135276254222,618.710565160554,-31.1471601717549)) ;
#66989 = CARTESIAN_POINT('Origin',(73.5135276254222,618.585565160554,-31.1471601717549)) ;
#66990 = CARTESIAN_POINT('Origin',(149.888527625422,618.585565160541,-30.8971601717549)) ;
#66991 = CARTESIAN_POINT('Origin',(73.5135276254222,618.585565160554,-30.8971601717549)) ;
#66992 = CARTESIAN_POINT('Origin',(87.2635276254222,618.585565160552,-30.8971601717549)) ;
#66993 = CARTESIAN_POINT('Origin',(87.2635276254222,618.710565160552,-31.1471601717549)) ;
#66994 = CARTESIAN_POINT('Origin',(87.2635276254222,618.585565160552,-31.1471601717549)) ;
#66995 = CARTESIAN_POINT('Origin',(87.5135276254222,618.585565160552,-44.772160171758)) ;
#66996 = CARTESIAN_POINT('Origin',(87.5135276254222,618.585565160552,-31.1471601717549)) ;
#66997 = CARTESIAN_POINT('Origin',(87.5135276254222,618.585565160552,-39.8971601717549)) ;
#66998 = CARTESIAN_POINT('Origin',(87.2635276254222,618.585565160552,-31.1471601717549)) ;
#66999 = CARTESIAN_POINT('Origin',(73.2635276254222,618.585565160554,-40.272160171758)) ;
#67000 = CARTESIAN_POINT('Origin',(73.2635276254222,618.585565160554,-39.8971601717549)) ;
#67001 = CARTESIAN_POINT('Origin',(73.2635276254222,618.585565160554,-31.1471601717549)) ;
#67002 = CARTESIAN_POINT('Origin',(73.5135276254222,618.585565160554,-31.1471601717549)) ;
#67003 = CARTESIAN_POINT('Origin',(87.2635276254222,618.585565160552,-39.8971601717549)) ;
#67004 = CARTESIAN_POINT('Origin',(73.5135276254222,618.585565160554,-39.8971601717549)) ;
#67005 = CARTESIAN_POINT('Origin',(95.6885276254225,618.21056516055,-24.1221601717559)) ;
#67006 = CARTESIAN_POINT('',(97.6885276254217,613.46056516055,-24.122160171756)) ;
#67007 = CARTESIAN_POINT('Origin',(97.688527625422,615.46056516055,-24.122160171756)) ;
#67008 = CARTESIAN_POINT('',(124.688527625422,613.460565160546,-24.1221601717572)) ;
#67009 = CARTESIAN_POINT('',(154.038527625422,613.46056516054,-24.1221601717586)) ;
#67010 = CARTESIAN_POINT('Origin',(124.688527625422,615.460565160545,-24.1221601717572)) ;
#67011 = CARTESIAN_POINT('Origin',(173.388527625422,618.210565160537,-37.2221601717594)) ;
#67012 = CARTESIAN_POINT('Origin',(171.388527625402,506.960565160537,-37.2221601717594)) ;
#67013 = CARTESIAN_POINT('Origin',(171.388527625402,506.960565160537,-45.8221601717594)) ;
#67014 = CARTESIAN_POINT('',(171.388527625403,508.960565160537,-38.1221601717594)) ;
#67015 = CARTESIAN_POINT('Origin',(171.388527625402,506.960565160537,-38.1221601717594)) ;
#67016 = CARTESIAN_POINT('',(171.388527625402,508.960565160537,-45.8221601717594)) ;
#67017 = CARTESIAN_POINT('Origin',(171.388527625422,618.210565160537,-30.2221601717593)) ;
#67018 = CARTESIAN_POINT('Origin',(171.388527625403,506.960565160537,-30.2221601717594)) ;
#67019 = CARTESIAN_POINT('Origin',(171.388527625402,506.960565160537,-45.8221601717594)) ;
#67020 = CARTESIAN_POINT('',(171.388527625402,508.960565160537,-45.8221601717594)) ;
#67021 = CARTESIAN_POINT('Origin',(124.688527625421,615.460565160545,-36.8221601717572)) ;
#67022 = CARTESIAN_POINT('',(124.688527625421,613.460565160545,-38.1221601717572)) ;
#67023 = CARTESIAN_POINT('Origin',(124.688527625421,615.460565160545,-38.1221601717572)) ;
#67024 = CARTESIAN_POINT('',(124.688527625421,613.460565160545,-36.8221601717572)) ;
#67025 = CARTESIAN_POINT('Origin',(87.9885276254024,506.960565160552,-36.8221601717556)) ;
#67026 = CARTESIAN_POINT('',(87.9885276254026,508.960565160552,-38.1221601717555)) ;
#67027 = CARTESIAN_POINT('Origin',(87.9885276254023,506.960565160552,-38.1221601717555)) ;
#67028 = CARTESIAN_POINT('',(87.9885276254027,508.960565160552,-36.8221601717556)) ;
#67029 = CARTESIAN_POINT('Origin',(212.388527625402,508.96056516053,-49.5221601717612)) ;
#67030 = CARTESIAN_POINT('',(169.388527625402,508.960565160538,-40.1221604692946)) ;
#67031 = CARTESIAN_POINT('Origin',(169.388527625403,508.960565160538,-38.1221601717593)) ;
#67032 = CARTESIAN_POINT('',(89.9885276254026,508.960565160552,-40.1221604695632)) ;
#67033 = CARTESIAN_POINT('',(158.688527625403,508.96056516054,-40.1221607671016)) ;
#67034 = CARTESIAN_POINT('Origin',(89.9885276254027,508.960565160552,-38.1221601717556)) ;
#67035 = CARTESIAN_POINT('Ctrl Pts',(87.9885276254048,508.960565160552,-38.122160171761)) ;
#67036 = CARTESIAN_POINT('Ctrl Pts',(87.9885276253991,508.960565160552,-40.1221601717586)) ;
#67037 = CARTESIAN_POINT('Ctrl Pts',(89.9885276253967,508.960565160552,-40.1221601717529)) ;
#67038 = CARTESIAN_POINT('Ctrl Pts',(85.9885276254019,508.960565160554,-38.122160171761)) ;
#67039 = CARTESIAN_POINT('Ctrl Pts',(85.9885276253905,508.960565160553,-42.1221601717673)) ;
#67040 = CARTESIAN_POINT('Ctrl Pts',(89.9885276253967,508.960565160554,-42.1221601717558)) ;
#67041 = CARTESIAN_POINT('Ctrl Pts',(85.9885276254023,506.960565160551,-38.1221601717605)) ;
#67042 = CARTESIAN_POINT('Ctrl Pts',(85.9885276253908,506.96056516055,-42.1221601717667)) ;
#67043 = CARTESIAN_POINT('Ctrl Pts',(89.988527625397,506.960565160551,-42.1221601717552)) ;
#67044 = CARTESIAN_POINT('Origin',(89.9885276254022,506.960565160552,-40.1221607670984)) ;
#67045 = CARTESIAN_POINT('Origin',(158.688527625402,506.960565160539,-40.1221607671016)) ;
#67046 = CARTESIAN_POINT('Origin',(169.388527625402,506.960565160538,-40.1221601717593)) ;
#67047 = CARTESIAN_POINT('Ctrl Pts',(173.388527625402,506.960565160537,-38.1221601717599)) ;
#67048 = CARTESIAN_POINT('Ctrl Pts',(173.388527625405,506.960565160535,-42.1221601717625)) ;
#67049 = CARTESIAN_POINT('Ctrl Pts',(169.388527625403,506.960565160538,-42.1221601717592)) ;
#67050 = CARTESIAN_POINT('Ctrl Pts',(173.388527625403,508.960565160538,-38.1221601717607)) ;
#67051 = CARTESIAN_POINT('Ctrl Pts',(173.388527625407,508.960565160536,-42.1221601717633)) ;
#67052 = CARTESIAN_POINT('Ctrl Pts',(169.388527625404,508.960565160539,-42.12216017176)) ;
#67053 = CARTESIAN_POINT('Ctrl Pts',(171.388527625402,508.960565160537,-38.1221601717607)) ;
#67054 = CARTESIAN_POINT('Ctrl Pts',(171.388527625404,508.960565160537,-40.1221601717605)) ;
#67055 = CARTESIAN_POINT('Ctrl Pts',(169.388527625404,508.960565160538,-40.1221601717589)) ;
#67056 = CARTESIAN_POINT('Origin',(212.38852762542,613.46056516053,-49.5221601717612)) ;
#67057 = CARTESIAN_POINT('',(122.688527625421,613.460565160546,-40.1221604695633)) ;
#67058 = CARTESIAN_POINT('Origin',(122.688527625421,613.460565160546,-38.1221601717571)) ;
#67059 = CARTESIAN_POINT('',(97.688527625421,613.46056516055,-38.122160171756)) ;
#67060 = CARTESIAN_POINT('',(97.6885276254207,613.46056516055,-45.822160171756)) ;
#67061 = CARTESIAN_POINT('',(99.6885276254209,613.46056516055,-40.12216046929)) ;
#67062 = CARTESIAN_POINT('Origin',(99.688527625421,613.46056516055,-38.1221601717561)) ;
#67063 = CARTESIAN_POINT('',(158.688527625421,613.46056516054,-40.1221607670988)) ;
#67064 = CARTESIAN_POINT('Origin',(97.688527625421,615.46056516055,-45.822160171756)) ;
#67065 = CARTESIAN_POINT('Origin',(97.6885276254213,615.46056516055,-38.122160171756)) ;
#67066 = CARTESIAN_POINT('Ctrl Pts',(122.688527625423,615.460565160547,-42.1221601717572)) ;
#67067 = CARTESIAN_POINT('Ctrl Pts',(126.688527625424,615.460565160546,-42.1221601717601)) ;
#67068 = CARTESIAN_POINT('Ctrl Pts',(126.688527625421,615.460565160545,-38.1221601717583)) ;
#67069 = CARTESIAN_POINT('Ctrl Pts',(122.688527625422,613.460565160545,-42.1221601717582)) ;
#67070 = CARTESIAN_POINT('Ctrl Pts',(126.688527625425,613.460565160545,-42.1221601717611)) ;
#67071 = CARTESIAN_POINT('Ctrl Pts',(126.688527625422,613.460565160544,-38.1221601717587)) ;
#67072 = CARTESIAN_POINT('Ctrl Pts',(122.688527625422,613.460565160546,-40.1221601717567)) ;
#67073 = CARTESIAN_POINT('Ctrl Pts',(124.688527625422,613.460565160546,-40.1221601717582)) ;
#67074 = CARTESIAN_POINT('Ctrl Pts',(124.68852762542,613.460565160545,-38.1221601717587)) ;
#67075 = CARTESIAN_POINT('Origin',(122.688527625421,615.460565160546,-40.1221607670971)) ;
#67076 = CARTESIAN_POINT('Origin',(158.688527625421,615.460565160539,-40.1221607670988)) ;
#67077 = CARTESIAN_POINT('Origin',(99.6885276254213,615.46056516055,-40.1221601717561)) ;
#67078 = CARTESIAN_POINT('Ctrl Pts',(99.6885276254238,613.46056516055,-40.1221601717561)) ;
#67079 = CARTESIAN_POINT('Ctrl Pts',(97.6885276254219,613.46056516055,-40.1221601717552)) ;
#67080 = CARTESIAN_POINT('Ctrl Pts',(97.688527625421,613.46056516055,-38.1221601717534)) ;
#67081 = CARTESIAN_POINT('Ctrl Pts',(99.6885276254238,613.46056516055,-42.122160171757)) ;
#67082 = CARTESIAN_POINT('Ctrl Pts',(95.688527625422,613.460565160549,-42.1221601717552)) ;
#67083 = CARTESIAN_POINT('Ctrl Pts',(95.6885276254202,613.46056516055,-38.1221601717534)) ;
#67084 = CARTESIAN_POINT('Ctrl Pts',(99.6885276254231,615.460565160551,-42.1221601717564)) ;
#67085 = CARTESIAN_POINT('Ctrl Pts',(95.6885276254227,615.46056516055,-42.1221601717546)) ;
#67086 = CARTESIAN_POINT('Ctrl Pts',(95.6885276254209,615.460565160551,-38.1221601717541)) ;
#67087 = CARTESIAN_POINT('Ctrl Pts',(180.41923219887,533.719746184936,-49.5189826834674)) ;
#67088 = CARTESIAN_POINT('Ctrl Pts',(181.08204398532,533.89640864105,-49.4818916555201)) ;
#67089 = CARTESIAN_POINT('Ctrl Pts',(182.205016276376,534.964329959553,-49.4077265456203)) ;
#67090 = CARTESIAN_POINT('Ctrl Pts',(181.773238631581,537.25679369829,-49.296487353768)) ;
#67091 = CARTESIAN_POINT('Ctrl Pts',(179.609931126086,538.131245101682,-49.1852651079104)) ;
#67092 = CARTESIAN_POINT('Ctrl Pts',(177.703506856333,536.788339278838,-49.0740428620531)) ;
#67093 = CARTESIAN_POINT('Ctrl Pts',(177.798995298387,534.457518489788,-48.9628206161957)) ;
#67094 = CARTESIAN_POINT('Ctrl Pts',(179.810021293082,533.275522950702,-48.8515983703383)) ;
#67095 = CARTESIAN_POINT('Ctrl Pts',(181.892831047736,534.325447947475,-48.7403761244811)) ;
#67096 = CARTESIAN_POINT('Ctrl Pts',(182.138589015903,536.645014490742,-48.6291538786237)) ;
#67097 = CARTESIAN_POINT('Ctrl Pts',(180.32194054985,538.108083264837,-48.5179316327663)) ;
#67098 = CARTESIAN_POINT('Ctrl Pts',(178.1080419789,537.373637216578,-48.4067093869088)) ;
#67099 = CARTESIAN_POINT('Ctrl Pts',(177.526099138551,535.114854267548,-48.2954871410515)) ;
#67100 = CARTESIAN_POINT('Ctrl Pts',(179.109509196157,533.402080354734,-48.1842648951941)) ;
#67101 = CARTESIAN_POINT('Ctrl Pts',(181.406949090904,533.805262519012,-48.0730426493369)) ;
#67102 = CARTESIAN_POINT('Ctrl Pts',(182.31256717773,535.954749633126,-47.9618204034795)) ;
#67103 = CARTESIAN_POINT('Ctrl Pts',(180.996337743865,537.880594664061,-47.850598157622)) ;
#67104 = CARTESIAN_POINT('Ctrl Pts',(178.664426082464,537.817099808701,-47.7393759117645)) ;
#67105 = CARTESIAN_POINT('Ctrl Pts',(177.454493283379,535.82363243575,-47.6281536659072)) ;
#67106 = CARTESIAN_POINT('Ctrl Pts',(178.474265342102,533.724911499449,-47.5169314200499)) ;
#67107 = CARTESIAN_POINT('Ctrl Pts',(180.790760669799,533.450291962028,-47.4056948389639)) ;
#67108 = CARTESIAN_POINT('Ctrl Pts',(181.779696394841,534.643306150536,-47.3315323398303)) ;
#67109 = CARTESIAN_POINT('Ctrl Pts',(181.910843734302,535.316553593751,-47.2944439226492)) ;
#67110 = CARTESIAN_POINT('Ctrl Pts',(180.385086881284,533.847834672537,-49.5955171281681)) ;
#67111 = CARTESIAN_POINT('Ctrl Pts',(181.005253625502,534.013130737684,-49.5584261002209)) ;
#67112 = CARTESIAN_POINT('Ctrl Pts',(182.055974333595,535.012342430532,-49.484260990321)) ;
#67113 = CARTESIAN_POINT('Ctrl Pts',(181.651977087812,537.157309979624,-49.3730217984687)) ;
#67114 = CARTESIAN_POINT('Ctrl Pts',(179.62785591216,537.975499533435,-49.2617995526112)) ;
#67115 = CARTESIAN_POINT('Ctrl Pts',(177.844090208774,536.718995728027,-49.1505773067538)) ;
#67116 = CARTESIAN_POINT('Ctrl Pts',(177.933434963089,534.538139005725,-49.0393550608965)) ;
#67117 = CARTESIAN_POINT('Ctrl Pts',(179.815072358748,533.432192581505,-48.9281328150392)) ;
#67118 = CARTESIAN_POINT('Ctrl Pts',(181.763874976287,534.414565828681,-48.8169105691819)) ;
#67119 = CARTESIAN_POINT('Ctrl Pts',(181.99382097619,536.584892398823,-48.7056883233245)) ;
#67120 = CARTESIAN_POINT('Ctrl Pts',(180.294054937609,537.953827919806,-48.594466077467)) ;
#67121 = CARTESIAN_POINT('Ctrl Pts',(178.222597705189,537.266635833207,-48.4832438316095)) ;
#67122 = CARTESIAN_POINT('Ctrl Pts',(177.67809683179,535.153182065438,-48.3720215857521)) ;
#67123 = CARTESIAN_POINT('Ctrl Pts',(179.159630926782,533.550607333357,-48.2607993398948)) ;
#67124 = CARTESIAN_POINT('Ctrl Pts',(181.309254468017,533.927848920271,-48.1495770940376)) ;
#67125 = CARTESIAN_POINT('Ctrl Pts',(182.15660545346,535.939038902933,-48.0383548481802)) ;
#67126 = CARTESIAN_POINT('Ctrl Pts',(180.925061688953,537.740975843584,-47.9271326023229)) ;
#67127 = CARTESIAN_POINT('Ctrl Pts',(178.743184280586,537.681566221535,-47.8159103564653)) ;
#67128 = CARTESIAN_POINT('Ctrl Pts',(177.611098068376,535.816357732999,-47.704688110608)) ;
#67129 = CARTESIAN_POINT('Ctrl Pts',(178.565258405338,533.852667652805,-47.5934658647506)) ;
#67130 = CARTESIAN_POINT('Ctrl Pts',(180.732711360678,533.595717025337,-47.4822292836646)) ;
#67131 = CARTESIAN_POINT('Ctrl Pts',(181.658019361195,534.711973163531,-47.4080667845311)) ;
#67132 = CARTESIAN_POINT('Ctrl Pts',(181.780728733884,535.34190413858,-47.37097836735)) ;
#67133 = CARTESIAN_POINT('Ctrl Pts',(180.350941563697,533.975923160139,-49.6720515728689)) ;
#67134 = CARTESIAN_POINT('Ctrl Pts',(180.928463265684,534.129852834319,-49.6349605449215)) ;
#67135 = CARTESIAN_POINT('Ctrl Pts',(181.906932390813,535.06035490151,-49.5607954350218)) ;
#67136 = CARTESIAN_POINT('Ctrl Pts',(181.530715544042,537.057826260956,-49.4495562431695)) ;
#67137 = CARTESIAN_POINT('Ctrl Pts',(179.645780698234,537.81975396519,-49.338333997312)) ;
#67138 = CARTESIAN_POINT('Ctrl Pts',(177.984673561212,536.649652177216,-49.2271117514546)) ;
#67139 = CARTESIAN_POINT('Ctrl Pts',(178.067874627792,534.618759521662,-49.1158895055972)) ;
#67140 = CARTESIAN_POINT('Ctrl Pts',(179.820123424414,533.58886221231,-49.0046672597399)) ;
#67141 = CARTESIAN_POINT('Ctrl Pts',(181.634918904837,534.503683709888,-48.8934450138826)) ;
#67142 = CARTESIAN_POINT('Ctrl Pts',(181.849052936478,536.524770306902,-48.7822227680253)) ;
#67143 = CARTESIAN_POINT('Ctrl Pts',(180.266169325365,537.799572574774,-48.6710005221678)) ;
#67144 = CARTESIAN_POINT('Ctrl Pts',(178.337153431476,537.159634449835,-48.5597782763103)) ;
#67145 = CARTESIAN_POINT('Ctrl Pts',(177.83009452503,535.191509863326,-48.4485560304529)) ;
#67146 = CARTESIAN_POINT('Ctrl Pts',(179.209752657406,533.699134311977,-48.3373337845956)) ;
#67147 = CARTESIAN_POINT('Ctrl Pts',(181.21155984513,534.05043532153,-48.2261115387384)) ;
#67148 = CARTESIAN_POINT('Ctrl Pts',(182.000643729191,535.923328172739,-48.114889292881)) ;
#67149 = CARTESIAN_POINT('Ctrl Pts',(180.853785634043,537.601357023106,-48.0036670470236)) ;
#67150 = CARTESIAN_POINT('Ctrl Pts',(178.821942478709,537.546032634367,-47.8924448011661)) ;
#67151 = CARTESIAN_POINT('Ctrl Pts',(177.767702853372,535.809083030247,-47.7812225553087)) ;
#67152 = CARTESIAN_POINT('Ctrl Pts',(178.656251468576,533.980423806161,-47.6700003094514)) ;
#67153 = CARTESIAN_POINT('Ctrl Pts',(180.674662051555,533.741142088646,-47.5587637283654)) ;
#67154 = CARTESIAN_POINT('Ctrl Pts',(181.53634232755,534.780640176528,-47.4846012292319)) ;
#67155 = CARTESIAN_POINT('Ctrl Pts',(181.650613733467,535.367254683408,-47.4475128120508)) ;
#67156 = CARTESIAN_POINT('Ctrl Pts',(180.316796246111,534.104011647741,-49.7485860175697)) ;
#67157 = CARTESIAN_POINT('Ctrl Pts',(180.851672905866,534.246574930955,-49.7114949896223)) ;
#67158 = CARTESIAN_POINT('Ctrl Pts',(181.757890448032,535.108367372488,-49.6373298797226)) ;
#67159 = CARTESIAN_POINT('Ctrl Pts',(181.409454000273,536.958342542287,-49.5260906878703)) ;
#67160 = CARTESIAN_POINT('Ctrl Pts',(179.663705484307,537.664008396944,-49.4148684420128)) ;
#67161 = CARTESIAN_POINT('Ctrl Pts',(178.125256913651,536.580308626405,-49.3036461961554)) ;
#67162 = CARTESIAN_POINT('Ctrl Pts',(178.202314292494,534.699380037599,-49.192423950298)) ;
#67163 = CARTESIAN_POINT('Ctrl Pts',(179.825174490079,533.745531843113,-49.0812017044407)) ;
#67164 = CARTESIAN_POINT('Ctrl Pts',(181.505962833386,534.592801591096,-48.9699794585834)) ;
#67165 = CARTESIAN_POINT('Ctrl Pts',(181.704284896765,536.464648214983,-48.858757212726)) ;
#67166 = CARTESIAN_POINT('Ctrl Pts',(180.238283713123,537.645317229742,-48.7475349668686)) ;
#67167 = CARTESIAN_POINT('Ctrl Pts',(178.451709157764,537.052633066464,-48.6363127210111)) ;
#67168 = CARTESIAN_POINT('Ctrl Pts',(177.982092218269,535.229837661215,-48.5250904751537)) ;
#67169 = CARTESIAN_POINT('Ctrl Pts',(179.25987438803,533.847661290597,-48.4138682292964)) ;
#67170 = CARTESIAN_POINT('Ctrl Pts',(181.113865222243,534.173021722788,-48.3026459834391)) ;
#67171 = CARTESIAN_POINT('Ctrl Pts',(181.844682004921,535.907617442545,-48.1914237375818)) ;
#67172 = CARTESIAN_POINT('Ctrl Pts',(180.782509579131,537.461738202629,-48.0802014917245)) ;
#67173 = CARTESIAN_POINT('Ctrl Pts',(178.900700676832,537.410499047199,-47.9689792458669)) ;
#67174 = CARTESIAN_POINT('Ctrl Pts',(177.924307638369,535.801808327496,-47.8577570000095)) ;
#67175 = CARTESIAN_POINT('Ctrl Pts',(178.747244531814,534.108179959515,-47.7465347541522)) ;
#67176 = CARTESIAN_POINT('Ctrl Pts',(180.616612742433,533.886567151955,-47.6352981730662)) ;
#67177 = CARTESIAN_POINT('Ctrl Pts',(181.414665293904,534.849307189524,-47.5611356739326)) ;
#67178 = CARTESIAN_POINT('Ctrl Pts',(181.52049873305,535.392605228237,-47.5240472567515)) ;
#67179 = CARTESIAN_POINT('Ctrl Pts',(181.523656952658,535.391334705907,-47.5221601717598)) ;
#67180 = CARTESIAN_POINT('Ctrl Pts',(181.518699643216,535.327493994687,-47.5221601717599)) ;
#67181 = CARTESIAN_POINT('Ctrl Pts',(181.509766310845,535.264222574159,-47.5221601717597)) ;
#67182 = CARTESIAN_POINT('Ctrl Pts',(181.497157990989,535.201755695665,-47.5221601717597)) ;
#67183 = CARTESIAN_POINT('Ctrl Pts',(181.484549671134,535.139288817172,-47.5221601717597)) ;
#67184 = CARTESIAN_POINT('Ctrl Pts',(181.468266021405,535.077625700605,-47.5221601717599)) ;
#67185 = CARTESIAN_POINT('Ctrl Pts',(181.448552578097,535.016991237747,-47.5221601717599)) ;
#67186 = CARTESIAN_POINT('Ctrl Pts',(181.430731424601,534.962177065872,-47.5221601717599)) ;
#67187 = CARTESIAN_POINT('Ctrl Pts',(181.410106447755,534.908202995365,-47.5221601717595)) ;
#67188 = CARTESIAN_POINT('Ctrl Pts',(181.386823585982,534.855235972333,-47.5221601717596)) ;
#67189 = CARTESIAN_POINT('Ctrl Pts',(181.375123803509,534.828619714685,-47.5221601717596)) ;
#67190 = CARTESIAN_POINT('Ctrl Pts',(181.362752363877,534.802257809648,-47.5221601717599)) ;
#67191 = CARTESIAN_POINT('Ctrl Pts',(181.349724849682,534.776172131308,-47.52216017176)) ;
#67192 = CARTESIAN_POINT('Ctrl Pts',(181.343830429245,534.764369422577,-47.52216017176)) ;
#67193 = CARTESIAN_POINT('Ctrl Pts',(181.337800833022,534.752621939525,-47.5221601717597)) ;
#67194 = CARTESIAN_POINT('Ctrl Pts',(181.33164761352,534.74095038958,-47.5221601717597)) ;
#67195 = CARTESIAN_POINT('Ctrl Pts',(181.300422339755,534.681721665141,-47.5221601717597)) ;
#67196 = CARTESIAN_POINT('Ctrl Pts',(181.265964241246,534.624338180145,-47.5221601717599)) ;
#67197 = CARTESIAN_POINT('Ctrl Pts',(181.228541247385,534.569040430327,-47.5221601717598)) ;
#67198 = CARTESIAN_POINT('Ctrl Pts',(181.190437292971,534.51273646528,-47.5221601717597)) ;
#67199 = CARTESIAN_POINT('Ctrl Pts',(181.149259248045,534.45859387379,-47.5221601717597)) ;
#67200 = CARTESIAN_POINT('Ctrl Pts',(181.105236814465,534.406874481233,-47.5221601717596)) ;
#67201 = CARTESIAN_POINT('Ctrl Pts',(181.068311305258,534.36349285167,-47.5221601717596)) ;
#67202 = CARTESIAN_POINT('Ctrl Pts',(181.029383499007,534.321815942503,-47.5221601717598)) ;
#67203 = CARTESIAN_POINT('Ctrl Pts',(180.988563640333,534.282010110072,-47.5221601717598)) ;
#67204 = CARTESIAN_POINT('Ctrl Pts',(180.969705409454,534.263620345808,-47.5221601717598)) ;
#67205 = CARTESIAN_POINT('Ctrl Pts',(180.950443053091,534.245630122635,-47.5221601717599)) ;
#67206 = CARTESIAN_POINT('Ctrl Pts',(180.93078597856,534.228057025436,-47.5221601717598)) ;
#67207 = CARTESIAN_POINT('Ctrl Pts',(180.92231760162,534.220486437511,-47.5221601717597)) ;
#67208 = CARTESIAN_POINT('Ctrl Pts',(180.913776338193,534.212993731098,-47.5221601717599)) ;
#67209 = CARTESIAN_POINT('Ctrl Pts',(180.905173315045,534.20558895583,-47.5221601717599)) ;
#67210 = CARTESIAN_POINT('Ctrl Pts',(180.85193819082,534.159768536138,-47.5221601717599)) ;
#67211 = CARTESIAN_POINT('Ctrl Pts',(180.796243425943,534.11722427461,-47.5221601717599)) ;
#67212 = CARTESIAN_POINT('Ctrl Pts',(180.738340695584,534.078223544828,-47.5221601717599)) ;
#67213 = CARTESIAN_POINT('Ctrl Pts',(180.686274773575,534.043154232163,-47.5221601717599)) ;
#67214 = CARTESIAN_POINT('Ctrl Pts',(180.632422628309,534.010949703227,-47.5221601717598)) ;
#67215 = CARTESIAN_POINT('Ctrl Pts',(180.576936503322,533.981823088212,-47.5221601717599)) ;
#67216 = CARTESIAN_POINT('Ctrl Pts',(180.516798861993,533.950254728962,-47.52216017176)) ;
#67217 = CARTESIAN_POINT('Ctrl Pts',(180.454741783477,533.922300623552,-47.5221601717598)) ;
#67218 = CARTESIAN_POINT('Ctrl Pts',(180.391083335664,533.897902195449,-47.5221601717597)) ;
#67219 = CARTESIAN_POINT('Ctrl Pts',(180.366784181766,533.888589037813,-47.5221601717597)) ;
#67220 = CARTESIAN_POINT('Ctrl Pts',(180.34225140207,533.879794410572,-47.5221601717596)) ;
#67221 = CARTESIAN_POINT('Ctrl Pts',(180.317501726775,533.871516767415,-47.5221601717599)) ;
#67222 = CARTESIAN_POINT('Ctrl Pts',(180.306601299242,533.867871069106,-47.52216017176)) ;
#67223 = CARTESIAN_POINT('Ctrl Pts',(180.295659742371,533.864326067602,-47.5221601717597)) ;
#67224 = CARTESIAN_POINT('Ctrl Pts',(180.284690809148,533.860885251216,-47.5221601717597)) ;
#67225 = CARTESIAN_POINT('Ctrl Pts',(180.217926491994,533.839942124679,-47.5221601717597)) ;
#67226 = CARTESIAN_POINT('Ctrl Pts',(180.150032205707,533.82281505825,-47.5221601717595)) ;
#67227 = CARTESIAN_POINT('Ctrl Pts',(180.081372094379,533.80939571116,-47.5221601717596)) ;
#67228 = CARTESIAN_POINT('Ctrl Pts',(180.011138794992,533.795668890688,-47.5221601717597)) ;
#67229 = CARTESIAN_POINT('Ctrl Pts',(179.940103346079,533.785821371076,-47.5221601717597)) ;
#67230 = CARTESIAN_POINT('Ctrl Pts',(179.868623579727,533.779783474225,-47.5221601717596)) ;
#67231 = CARTESIAN_POINT('Ctrl Pts',(179.814610960391,533.775221027523,-47.5221601717596)) ;
#67232 = CARTESIAN_POINT('Ctrl Pts',(179.760343876057,533.772834758855,-47.5221601717598)) ;
#67233 = CARTESIAN_POINT('Ctrl Pts',(179.705969657728,533.772612887654,-47.5221601717596)) ;
#67234 = CARTESIAN_POINT('Ctrl Pts',(179.672275133079,533.77247539888,-47.5221601717595)) ;
#67235 = CARTESIAN_POINT('Ctrl Pts',(179.638539369937,533.7731693538,-47.5221601717597)) ;
#67236 = CARTESIAN_POINT('Ctrl Pts',(179.604796964325,533.774695061605,-47.5221601717595)) ;
#67237 = CARTESIAN_POINT('Ctrl Pts',(179.59189526542,533.775278429102,-47.5221601717594)) ;
#67238 = CARTESIAN_POINT('Ctrl Pts',(179.578990310459,533.775983572458,-47.5221601717595)) ;
#67239 = CARTESIAN_POINT('Ctrl Pts',(179.566091482587,533.776810113921,-47.5221601717595)) ;
#67240 = CARTESIAN_POINT('Ctrl Pts',(179.489521093383,533.781716652879,-47.5221601717596)) ;
#67241 = CARTESIAN_POINT('Ctrl Pts',(179.413353319935,533.790883056781,-47.5221601717595)) ;
#67242 = CARTESIAN_POINT('Ctrl Pts',(179.338001691281,533.80424141487,-47.5221601717595)) ;
#67243 = CARTESIAN_POINT('Ctrl Pts',(179.281487969791,533.814260183437,-47.5221601717596)) ;
#67244 = CARTESIAN_POINT('Ctrl Pts',(179.225432662501,533.826638060617,-47.5221601717597)) ;
#67245 = CARTESIAN_POINT('Ctrl Pts',(179.170006835869,533.841367503496,-47.5221601717597)) ;
#67246 = CARTESIAN_POINT('Ctrl Pts',(179.150343573577,533.846593025899,-47.5221601717597)) ;
#67247 = CARTESIAN_POINT('Ctrl Pts',(179.130759536777,533.852114683679,-47.5221601717597)) ;
#67248 = CARTESIAN_POINT('Ctrl Pts',(179.111262400932,533.857932697529,-47.5221601717595)) ;
#67249 = CARTESIAN_POINT('Ctrl Pts',(179.096495204142,533.862339280944,-47.5221601717594)) ;
#67250 = CARTESIAN_POINT('Ctrl Pts',(179.081782737386,533.866914487841,-47.5221601717595)) ;
#67251 = CARTESIAN_POINT('Ctrl Pts',(179.067135903331,533.87165551767,-47.5221601717595)) ;
#67252 = CARTESIAN_POINT('Ctrl Pts',(178.995485989662,533.894847859212,-47.5221601717595)) ;
#67253 = CARTESIAN_POINT('Ctrl Pts',(178.925350981393,533.922020779554,-47.5221601717598)) ;
#67254 = CARTESIAN_POINT('Ctrl Pts',(178.857109801498,533.95314226278,-47.5221601717595)) ;
#67255 = CARTESIAN_POINT('Ctrl Pts',(178.801970214503,533.978288746683,-47.5221601717592)) ;
#67256 = CARTESIAN_POINT('Ctrl Pts',(178.748066676868,534.0060141123,-47.5221601717596)) ;
#67257 = CARTESIAN_POINT('Ctrl Pts',(178.695602917514,534.036326095524,-47.5221601717597)) ;
#67258 = CARTESIAN_POINT('Ctrl Pts',(178.685262867438,534.042300265662,-47.5221601717597)) ;
#67259 = CARTESIAN_POINT('Ctrl Pts',(178.674978767005,534.048374980139,-47.52216017176)) ;
#67260 = CARTESIAN_POINT('Ctrl Pts',(178.66475115082,534.054548898047,-47.5221601717599)) ;
#67261 = CARTESIAN_POINT('',(181.15861657589,536.79152871558,-49.5230400807548)) ;
#67262 = CARTESIAN_POINT('Ctrl Pts',(181.157234110517,536.790352109262,-49.5230400807548)) ;
#67263 = CARTESIAN_POINT('Ctrl Pts',(181.152240231553,536.796219717345,-49.5227467777565)) ;
#67264 = CARTESIAN_POINT('Ctrl Pts',(181.147205646513,536.802052680774,-49.5224534747582)) ;
#67265 = CARTESIAN_POINT('Ctrl Pts',(181.142130839976,536.807850438129,-49.5221601717599)) ;
#67266 = CARTESIAN_POINT('Ctrl Pts',(180.418697842595,533.725390834864,-49.5221601717599)) ;
#67267 = CARTESIAN_POINT('Ctrl Pts',(180.487297636394,533.750790795206,-49.5221601717598)) ;
#67268 = CARTESIAN_POINT('Ctrl Pts',(180.554195025763,533.780091250273,-49.5221601717596)) ;
#67269 = CARTESIAN_POINT('Ctrl Pts',(180.61920218942,533.812995292462,-49.5221601717597)) ;
#67270 = CARTESIAN_POINT('Ctrl Pts',(180.686073023045,533.846842650308,-49.5221601717599)) ;
#67271 = CARTESIAN_POINT('Ctrl Pts',(180.750944469885,533.88450386658,-49.5221601717598)) ;
#67272 = CARTESIAN_POINT('Ctrl Pts',(180.813580887979,533.925700546046,-49.5221601717598)) ;
#67273 = CARTESIAN_POINT('Ctrl Pts',(180.866572112173,533.960553472571,-49.5221601717597)) ;
#67274 = CARTESIAN_POINT('Ctrl Pts',(180.917963310832,533.997937920844,-49.5221601717599)) ;
#67275 = CARTESIAN_POINT('Ctrl Pts',(180.967588972733,534.037703430217,-49.5221601717599)) ;
#67276 = CARTESIAN_POINT('Ctrl Pts',(180.989598162914,534.0553396012,-49.5221601717598)) ;
#67277 = CARTESIAN_POINT('Ctrl Pts',(181.01125977542,534.073444296496,-49.5221601717595)) ;
#67278 = CARTESIAN_POINT('Ctrl Pts',(181.03255782176,534.092005111688,-49.5221601717594)) ;
#67279 = CARTESIAN_POINT('Ctrl Pts',(181.04422687788,534.1021744573,-49.5221601717594)) ;
#67280 = CARTESIAN_POINT('Ctrl Pts',(181.055786778592,534.112480730719,-49.5221601717597)) ;
#67281 = CARTESIAN_POINT('Ctrl Pts',(181.067234761772,534.12292193265,-49.5221601717597)) ;
#67282 = CARTESIAN_POINT('Ctrl Pts',(181.077875659478,534.132627027419,-49.5221601717597)) ;
#67283 = CARTESIAN_POINT('Ctrl Pts',(181.088421379634,534.142450292378,-49.5221601717595)) ;
#67284 = CARTESIAN_POINT('Ctrl Pts',(181.098853624774,534.152374457357,-49.5221601717595)) ;
#67285 = CARTESIAN_POINT('Ctrl Pts',(181.151929238903,534.202865137353,-49.5221601717596)) ;
#67286 = CARTESIAN_POINT('Ctrl Pts',(181.202164898294,534.25604865759,-49.5221601717595)) ;
#67287 = CARTESIAN_POINT('Ctrl Pts',(181.24934253704,534.311661892117,-49.5221601717596)) ;
#67288 = CARTESIAN_POINT('Ctrl Pts',(181.296166128424,534.366857773857,-49.5221601717597)) ;
#67289 = CARTESIAN_POINT('Ctrl Pts',(181.339977934579,534.424447930197,-49.5221601717597)) ;
#67290 = CARTESIAN_POINT('Ctrl Pts',(181.380519947539,534.484199350413,-49.5221601717596)) ;
#67291 = CARTESIAN_POINT('Ctrl Pts',(181.414273339383,534.533945600105,-49.5221601717595)) ;
#67292 = CARTESIAN_POINT('Ctrl Pts',(181.445759651354,534.585190575276,-49.5221601717597)) ;
#67293 = CARTESIAN_POINT('Ctrl Pts',(181.47480219779,534.637806255418,-49.5221601717596)) ;
#67294 = CARTESIAN_POINT('Ctrl Pts',(181.486863052554,534.659656614784,-49.5221601717596)) ;
#67295 = CARTESIAN_POINT('Ctrl Pts',(181.498502135439,534.681743402877,-49.5221601717599)) ;
#67296 = CARTESIAN_POINT('Ctrl Pts',(181.509705364919,534.704057527305,-49.5221601717596)) ;
#67297 = CARTESIAN_POINT('Ctrl Pts',(181.514930645526,534.714465022915,-49.5221601717594)) ;
#67298 = CARTESIAN_POINT('Ctrl Pts',(181.520061099594,534.724921972449,-49.5221601717596)) ;
#67299 = CARTESIAN_POINT('Ctrl Pts',(181.525095232284,534.735427451061,-49.5221601717597)) ;
#67300 = CARTESIAN_POINT('Ctrl Pts',(181.530288327452,534.746264660481,-49.5221601717599)) ;
#67301 = CARTESIAN_POINT('Ctrl Pts',(181.535375235005,534.757145877216,-49.5221601717596)) ;
#67302 = CARTESIAN_POINT('Ctrl Pts',(181.540353141824,534.768066253231,-49.5221601717596)) ;
#67303 = CARTESIAN_POINT('Ctrl Pts',(181.568894008366,534.830678312034,-49.52216017176)) ;
#67304 = CARTESIAN_POINT('Ctrl Pts',(181.593874352498,534.894615755507,-49.5221601717597)) ;
#67305 = CARTESIAN_POINT('Ctrl Pts',(181.615071096175,534.959670773429,-49.5221601717597)) ;
#67306 = CARTESIAN_POINT('Ctrl Pts',(181.634418034443,535.019048545549,-49.5221601717597)) ;
#67307 = CARTESIAN_POINT('Ctrl Pts',(181.650612654374,535.079357955261,-49.5221601717597)) ;
#67308 = CARTESIAN_POINT('Ctrl Pts',(181.663447662517,535.140445795219,-49.5221601717599)) ;
#67309 = CARTESIAN_POINT('Ctrl Pts',(181.678533132294,535.21224464047,-49.5221601717601)) ;
#67310 = CARTESIAN_POINT('Ctrl Pts',(181.688978110915,535.285120344497,-49.5221601717598)) ;
#67311 = CARTESIAN_POINT('Ctrl Pts',(181.694857599082,535.358651547933,-49.5221601717599)) ;
#67312 = CARTESIAN_POINT('Ctrl Pts',(181.696161835107,535.374962839277,-49.5221601717599)) ;
#67313 = CARTESIAN_POINT('Ctrl Pts',(181.697241186125,535.39130630221,-49.52216017176)) ;
#67314 = CARTESIAN_POINT('Ctrl Pts',(181.698096091594,535.407677166896,-49.52216017176)) ;
#67315 = CARTESIAN_POINT('Ctrl Pts',(181.698933016579,535.423703717419,-49.52216017176)) ;
#67316 = CARTESIAN_POINT('Ctrl Pts',(181.699554835009,535.439761827546,-49.5221601717599)) ;
#67317 = CARTESIAN_POINT('Ctrl Pts',(181.699961459045,535.455815776155,-49.5221601717599)) ;
#67318 = CARTESIAN_POINT('Ctrl Pts',(181.701697562433,535.524358980973,-49.5221601717597)) ;
#67319 = CARTESIAN_POINT('Ctrl Pts',(181.699522602882,535.592920300968,-49.5221601717599)) ;
#67320 = CARTESIAN_POINT('Ctrl Pts',(181.693557308922,535.661163908554,-49.5221601717598)) ;
#67321 = CARTESIAN_POINT('Ctrl Pts',(181.687592743364,535.72939918315,-49.5221601717597)) ;
#67322 = CARTESIAN_POINT('Ctrl Pts',(181.677838315832,535.79731788866,-49.5221601717597)) ;
#67323 = CARTESIAN_POINT('Ctrl Pts',(181.664365101627,535.864569235536,-49.5221601717598)) ;
#67324 = CARTESIAN_POINT('Ctrl Pts',(181.654515187308,535.91373493531,-49.52216017176)) ;
#67325 = CARTESIAN_POINT('Ctrl Pts',(181.642676644468,535.962543698494,-49.5221601717599)) ;
#67326 = CARTESIAN_POINT('Ctrl Pts',(181.628862533981,536.010848459207,-49.5221601717601)) ;
#67327 = CARTESIAN_POINT('Ctrl Pts',(181.623150206523,536.03082315184,-49.5221601717602)) ;
#67328 = CARTESIAN_POINT('Ctrl Pts',(181.617099932002,536.050711540705,-49.52216017176)) ;
#67329 = CARTESIAN_POINT('Ctrl Pts',(181.610712076097,536.070502654402,-49.5221601717599)) ;
#67330 = CARTESIAN_POINT('Ctrl Pts',(181.605971227629,536.085190942998,-49.5221601717597)) ;
#67331 = CARTESIAN_POINT('Ctrl Pts',(181.601044429239,536.099825644399,-49.52216017176)) ;
#67332 = CARTESIAN_POINT('Ctrl Pts',(181.595931721971,536.114402135746,-49.5221601717599)) ;
#67333 = CARTESIAN_POINT('Ctrl Pts',(181.591629159901,536.126668877315,-49.5221601717598)) ;
#67334 = CARTESIAN_POINT('Ctrl Pts',(181.587197704363,536.138886424694,-49.5221601717601)) ;
#67335 = CARTESIAN_POINT('Ctrl Pts',(181.582639148766,536.151048855726,-49.5221601717601)) ;
#67336 = CARTESIAN_POINT('Ctrl Pts',(181.559528847451,536.212708177395,-49.52216017176)) ;
#67337 = CARTESIAN_POINT('Ctrl Pts',(181.533144770481,536.272982567931,-49.52216017176)) ;
#67338 = CARTESIAN_POINT('Ctrl Pts',(181.503537114218,536.331539926083,-49.5221601717599)) ;
#67339 = CARTESIAN_POINT('Ctrl Pts',(181.482573948164,536.373000405483,-49.5221601717599)) ;
#67340 = CARTESIAN_POINT('Ctrl Pts',(181.459993913709,536.413599596872,-49.5221601717601)) ;
#67341 = CARTESIAN_POINT('Ctrl Pts',(181.435804180235,536.453208026963,-49.5221601717603)) ;
#67342 = CARTESIAN_POINT('Ctrl Pts',(181.42807699997,536.465860563199,-49.5221601717603)) ;
#67343 = CARTESIAN_POINT('Ctrl Pts',(181.420184269904,536.478413807954,-49.5221601717601)) ;
#67344 = CARTESIAN_POINT('Ctrl Pts',(181.412130015855,536.490857193274,-49.5221601717601)) ;
#67345 = CARTESIAN_POINT('Ctrl Pts',(181.377866042633,536.543793172047,-49.5221601717601)) ;
#67346 = CARTESIAN_POINT('Ctrl Pts',(181.340745918553,536.594646264424,-49.5221601717597)) ;
#67347 = CARTESIAN_POINT('Ctrl Pts',(181.300803879855,536.643102920757,-49.52216017176)) ;
#67348 = CARTESIAN_POINT('Ctrl Pts',(181.263594869918,536.688243936733,-49.5221601717603)) ;
#67349 = CARTESIAN_POINT('Ctrl Pts',(181.223936346045,536.731305409684,-49.5221601717598)) ;
#67350 = CARTESIAN_POINT('Ctrl Pts',(181.181833737656,536.771999681009,-49.5221601717601)) ;
#67351 = CARTESIAN_POINT('Ctrl Pts',(181.174644864848,536.7789480852,-49.5221601717601)) ;
#67352 = CARTESIAN_POINT('Ctrl Pts',(181.167384690605,536.78582738569,-49.5221601717596)) ;
#67353 = CARTESIAN_POINT('Ctrl Pts',(181.160054448737,536.792637064758,-49.5221601717595)) ;
#67354 = CARTESIAN_POINT('Ctrl Pts',(178.622419190323,536.788246779922,-49.5202730914232)) ;
#67355 = CARTESIAN_POINT('Ctrl Pts',(178.263637748317,536.36676207672,-49.4831846742774)) ;
#67356 = CARTESIAN_POINT('Ctrl Pts',(178.008514861325,535.14256091782,-49.4090221751792)) ;
#67357 = CARTESIAN_POINT('Ctrl Pts',(179.347310763183,533.819203307332,-49.2977855941286)) ;
#67358 = CARTESIAN_POINT('Ctrl Pts',(181.184535504429,534.231765349117,-49.1865633482713)) ;
#67359 = CARTESIAN_POINT('Ctrl Pts',(181.833489463951,535.998142408068,-49.075341102414)) ;
#67360 = CARTESIAN_POINT('Ctrl Pts',(180.700261197456,537.501346936019,-48.9641188565566)) ;
#67361 = CARTESIAN_POINT('Ctrl Pts',(178.822946992655,537.362808329003,-48.8528966106991)) ;
#67362 = CARTESIAN_POINT('Ctrl Pts',(177.922442264761,535.709930020042,-48.7416743648417)) ;
#67363 = CARTESIAN_POINT('Ctrl Pts',(178.824009613428,534.057562707726,-48.6304521189843)) ;
#67364 = CARTESIAN_POINT('Ctrl Pts',(180.701322763348,533.920325250683,-48.519229873127)) ;
#67365 = CARTESIAN_POINT('Ctrl Pts',(181.833640222805,535.42398090139,-48.4080076272697)) ;
#67366 = CARTESIAN_POINT('Ctrl Pts',(181.183108346156,537.190313662327,-48.2967853814123)) ;
#67367 = CARTESIAN_POINT('Ctrl Pts',(179.345987355079,537.600344449737,-48.1855631355549)) ;
#67368 = CARTESIAN_POINT('Ctrl Pts',(178.00617051876,536.278212737651,-48.0743408896974)) ;
#67369 = CARTESIAN_POINT('Ctrl Pts',(178.39170274318,534.435855450606,-47.9631186438401)) ;
#67370 = CARTESIAN_POINT('Ctrl Pts',(180.149288064919,533.761766876316,-47.8518963979828)) ;
#67371 = CARTESIAN_POINT('Ctrl Pts',(181.667901731917,534.874260780677,-47.7406741521255)) ;
#67372 = CARTESIAN_POINT('Ctrl Pts',(181.555965320099,536.752744050679,-47.6294519062681)) ;
#67373 = CARTESIAN_POINT('Ctrl Pts',(179.91579713902,537.677649735568,-47.5182296604107)) ;
#67374 = CARTESIAN_POINT('Ctrl Pts',(178.252194934696,536.796634656889,-47.4069913524144)) ;
#67375 = CARTESIAN_POINT('Ctrl Pts',(178.143425297585,535.55082917805,-47.3328271263707)) ;
#67376 = CARTESIAN_POINT('Ctrl Pts',(178.365436513798,535.043765566178,-47.2957369822794)) ;
#67377 = CARTESIAN_POINT('Ctrl Pts',(178.520858913152,536.874692490996,-49.597273851344)) ;
#67378 = CARTESIAN_POINT('Ctrl Pts',(178.133297990902,536.419398595709,-49.5601854341982)) ;
#67379 = CARTESIAN_POINT('Ctrl Pts',(177.857710544637,535.096998731576,-49.4860229350999)) ;
#67380 = CARTESIAN_POINT('Ctrl Pts',(179.303897313739,533.667488628938,-49.3747863540493)) ;
#67381 = CARTESIAN_POINT('Ctrl Pts',(181.288494151068,534.113144135825,-49.263564108192)) ;
#67382 = CARTESIAN_POINT('Ctrl Pts',(181.989503639305,536.021210278212,-49.1523418623347)) ;
#67383 = CARTESIAN_POINT('Ctrl Pts',(180.765374014243,537.644993632014,-49.0411196164771)) ;
#67384 = CARTESIAN_POINT('Ctrl Pts',(178.737471956384,537.495342217487,-48.9298973706197)) ;
#67385 = CARTESIAN_POINT('Ctrl Pts',(177.764733676274,535.709879072554,-48.8186751247623)) ;
#67386 = CARTESIAN_POINT('Ctrl Pts',(178.73861981477,533.924967913615,-48.707452878905)) ;
#67387 = CARTESIAN_POINT('Ctrl Pts',(180.76652073313,533.776722020178,-48.5962306330477)) ;
#67388 = CARTESIAN_POINT('Ctrl Pts',(181.989666491209,535.400992683332,-48.4850083871904)) ;
#67389 = CARTESIAN_POINT('Ctrl Pts',(181.286952513983,537.30901097436,-48.3737861413329)) ;
#67390 = CARTESIAN_POINT('Ctrl Pts',(179.302467749094,537.751932183525,-48.2625638954756)) ;
#67391 = CARTESIAN_POINT('Ctrl Pts',(177.855178151765,536.323746314136,-48.151341649618)) ;
#67392 = CARTESIAN_POINT('Ctrl Pts',(178.271635657531,534.333605226323,-48.0401194037607)) ;
#67393 = CARTESIAN_POINT('Ctrl Pts',(180.170204837748,533.605444962321,-47.9288971579034)) ;
#67394 = CARTESIAN_POINT('Ctrl Pts',(181.810633367249,534.807177028397,-47.8176749120461)) ;
#67395 = CARTESIAN_POINT('Ctrl Pts',(181.689718030172,536.836341927457,-47.7064526661887)) ;
#67396 = CARTESIAN_POINT('Ctrl Pts',(179.917984549896,537.835438475557,-47.5952304203312)) ;
#67397 = CARTESIAN_POINT('Ctrl Pts',(178.120937297508,536.883753197465,-47.483992112335)) ;
#67398 = CARTESIAN_POINT('Ctrl Pts',(178.003442756441,535.538016033293,-47.4098278862913)) ;
#67399 = CARTESIAN_POINT('Ctrl Pts',(178.243262495234,534.990278558474,-47.3727377422)) ;
#67400 = CARTESIAN_POINT('Ctrl Pts',(178.419298635981,536.961138202069,-49.6742746112646)) ;
#67401 = CARTESIAN_POINT('Ctrl Pts',(178.002958233487,536.4720351147,-49.6371861941188)) ;
#67402 = CARTESIAN_POINT('Ctrl Pts',(177.706906227949,535.051436545331,-49.5630236950206)) ;
#67403 = CARTESIAN_POINT('Ctrl Pts',(179.260483864295,533.515773950542,-49.45178711397)) ;
#67404 = CARTESIAN_POINT('Ctrl Pts',(181.392452797707,533.994522922533,-49.3405648681127)) ;
#67405 = CARTESIAN_POINT('Ctrl Pts',(182.14551781466,536.044278148355,-49.2293426222554)) ;
#67406 = CARTESIAN_POINT('Ctrl Pts',(180.830486831031,537.788640328009,-49.1181203763979)) ;
#67407 = CARTESIAN_POINT('Ctrl Pts',(178.651996920114,537.627876105971,-49.0068981305405)) ;
#67408 = CARTESIAN_POINT('Ctrl Pts',(177.607025087785,535.709828125064,-48.895675884683)) ;
#67409 = CARTESIAN_POINT('Ctrl Pts',(178.653230016112,533.792373119504,-48.7844536388257)) ;
#67410 = CARTESIAN_POINT('Ctrl Pts',(180.831718702914,533.633118789673,-48.6732313929684)) ;
#67411 = CARTESIAN_POINT('Ctrl Pts',(182.145692759613,535.378004465272,-48.5620091471111)) ;
#67412 = CARTESIAN_POINT('Ctrl Pts',(181.390796681811,537.427708286391,-48.4507869012537)) ;
#67413 = CARTESIAN_POINT('Ctrl Pts',(179.258948143106,537.903519917313,-48.3395646553962)) ;
#67414 = CARTESIAN_POINT('Ctrl Pts',(177.704185784769,536.369279890622,-48.2283424095388)) ;
#67415 = CARTESIAN_POINT('Ctrl Pts',(178.151568571882,534.231355002041,-48.1171201636814)) ;
#67416 = CARTESIAN_POINT('Ctrl Pts',(180.191121610576,533.449123048327,-48.0058979178242)) ;
#67417 = CARTESIAN_POINT('Ctrl Pts',(181.953365002583,534.740093276118,-47.8946756719669)) ;
#67418 = CARTESIAN_POINT('Ctrl Pts',(181.823470740244,536.919939804236,-47.7834534261095)) ;
#67419 = CARTESIAN_POINT('Ctrl Pts',(179.920171960771,537.993227215544,-47.672231180252)) ;
#67420 = CARTESIAN_POINT('Ctrl Pts',(177.98967966032,536.970871738042,-47.5609928722558)) ;
#67421 = CARTESIAN_POINT('Ctrl Pts',(177.863460215298,535.525202888537,-47.486828646212)) ;
#67422 = CARTESIAN_POINT('Ctrl Pts',(178.12108847667,534.936791550772,-47.4497385021208)) ;
#67423 = CARTESIAN_POINT('Ctrl Pts',(178.31773835881,537.047583913142,-49.7512753711853)) ;
#67424 = CARTESIAN_POINT('Ctrl Pts',(177.872618476071,536.52467163369,-49.7141869540395)) ;
#67425 = CARTESIAN_POINT('Ctrl Pts',(177.556101911261,535.005874359087,-49.6400244549413)) ;
#67426 = CARTESIAN_POINT('Ctrl Pts',(179.217070414851,533.364059272146,-49.5287878738906)) ;
#67427 = CARTESIAN_POINT('Ctrl Pts',(181.496411444346,533.875901709242,-49.4175656280333)) ;
#67428 = CARTESIAN_POINT('Ctrl Pts',(182.301531990017,536.067346018498,-49.306343382176)) ;
#67429 = CARTESIAN_POINT('Ctrl Pts',(180.895599647818,537.932287024005,-49.1951211363185)) ;
#67430 = CARTESIAN_POINT('Ctrl Pts',(178.566521883845,537.760409994454,-49.0838988904611)) ;
#67431 = CARTESIAN_POINT('Ctrl Pts',(177.449316499298,535.709777177576,-48.9726766446036)) ;
#67432 = CARTESIAN_POINT('Ctrl Pts',(178.567840217455,533.659778325394,-48.8614543987463)) ;
#67433 = CARTESIAN_POINT('Ctrl Pts',(180.896916672697,533.489515559168,-48.750232152889)) ;
#67434 = CARTESIAN_POINT('Ctrl Pts',(182.301719028018,535.355016247213,-48.6390099070317)) ;
#67435 = CARTESIAN_POINT('Ctrl Pts',(181.494640849637,537.546405598424,-48.5277876611743)) ;
#67436 = CARTESIAN_POINT('Ctrl Pts',(179.215428537121,538.0551076511,-48.4165654153168)) ;
#67437 = CARTESIAN_POINT('Ctrl Pts',(177.553193417773,536.414813467106,-48.3053431694594)) ;
#67438 = CARTESIAN_POINT('Ctrl Pts',(178.031501486233,534.129104777759,-48.194120923602)) ;
#67439 = CARTESIAN_POINT('Ctrl Pts',(180.212038383404,533.292801134333,-48.0828986777447)) ;
#67440 = CARTESIAN_POINT('Ctrl Pts',(182.096096637916,534.673009523839,-47.9716764318875)) ;
#67441 = CARTESIAN_POINT('Ctrl Pts',(181.957223450317,537.003537681016,-47.8604541860301)) ;
#67442 = CARTESIAN_POINT('Ctrl Pts',(179.922359371647,538.151015955532,-47.7492319401726)) ;
#67443 = CARTESIAN_POINT('Ctrl Pts',(177.858422023132,537.057990278619,-47.6379936321763)) ;
#67444 = CARTESIAN_POINT('Ctrl Pts',(177.723477674154,535.512389743781,-47.5638294061326)) ;
#67445 = CARTESIAN_POINT('Ctrl Pts',(177.998914458105,534.883304543068,-47.5267392620414)) ;
#67446 = CARTESIAN_POINT('',(179.941771410307,537.377530426179,-47.5212802703069)) ;
#67447 = CARTESIAN_POINT('Ctrl Pts',(178.005900115743,534.887332980433,-47.5221601717595)) ;
#67448 = CARTESIAN_POINT('Ctrl Pts',(177.982987331993,534.956803076843,-47.5221601717592)) ;
#67449 = CARTESIAN_POINT('Ctrl Pts',(177.964185509426,535.027374098354,-47.5221601717594)) ;
#67450 = CARTESIAN_POINT('Ctrl Pts',(177.949379621047,535.098714081534,-47.5221601717595)) ;
#67451 = CARTESIAN_POINT('Ctrl Pts',(177.934149267583,535.172099286938,-47.5221601717595)) ;
#67452 = CARTESIAN_POINT('Ctrl Pts',(177.923147305685,535.246299210421,-47.5221601717596)) ;
#67453 = CARTESIAN_POINT('Ctrl Pts',(177.916302997627,535.320956043131,-47.5221601717597)) ;
#67454 = CARTESIAN_POINT('Ctrl Pts',(177.910512624069,535.384116693759,-47.5221601717597)) ;
#67455 = CARTESIAN_POINT('Ctrl Pts',(177.907699073298,535.447604771906,-47.5221601717597)) ;
#67456 = CARTESIAN_POINT('Ctrl Pts',(177.907847905046,535.511197065041,-47.5221601717597)) ;
#67457 = CARTESIAN_POINT('Ctrl Pts',(177.907913912551,535.539400513806,-47.5221601717596)) ;
#67458 = CARTESIAN_POINT('Ctrl Pts',(177.908562938165,535.567624335509,-47.5221601717597)) ;
#67459 = CARTESIAN_POINT('Ctrl Pts',(177.909795252389,535.595848295825,-47.5221601717594)) ;
#67460 = CARTESIAN_POINT('Ctrl Pts',(177.910470429113,535.61131201497,-47.5221601717592)) ;
#67461 = CARTESIAN_POINT('Ctrl Pts',(177.911320717597,535.626775766067,-47.5221601717594)) ;
#67462 = CARTESIAN_POINT('Ctrl Pts',(177.912346276888,535.64223614306,-47.5221601717594)) ;
#67463 = CARTESIAN_POINT('Ctrl Pts',(177.913299533898,535.65660655817,-47.5221601717594)) ;
#67464 = CARTESIAN_POINT('Ctrl Pts',(177.914404522285,535.670976238378,-47.5221601717596)) ;
#67465 = CARTESIAN_POINT('Ctrl Pts',(177.915659147972,535.685320110379,-47.5221601717596)) ;
#67466 = CARTESIAN_POINT('Ctrl Pts',(177.92204224511,535.75829671947,-47.5221601717597)) ;
#67467 = CARTESIAN_POINT('Ctrl Pts',(177.932301372236,535.830731920874,-47.5221601717597)) ;
#67468 = CARTESIAN_POINT('Ctrl Pts',(177.946366771134,535.902291167493,-47.5221601717596)) ;
#67469 = CARTESIAN_POINT('Ctrl Pts',(177.960217864007,535.972760108906,-47.5221601717596)) ;
#67470 = CARTESIAN_POINT('Ctrl Pts',(177.977760553777,536.04238048792,-47.5221601717593)) ;
#67471 = CARTESIAN_POINT('Ctrl Pts',(177.998973857845,536.110813461122,-47.5221601717592)) ;
#67472 = CARTESIAN_POINT('Ctrl Pts',(178.016940288639,536.168772196503,-47.5221601717591)) ;
#67473 = CARTESIAN_POINT('Ctrl Pts',(178.037540545391,536.225879158725,-47.5221601717595)) ;
#67474 = CARTESIAN_POINT('Ctrl Pts',(178.060784890946,536.281910303999,-47.5221601717594)) ;
#67475 = CARTESIAN_POINT('Ctrl Pts',(178.070348369247,536.304963336004,-47.5221601717594)) ;
#67476 = CARTESIAN_POINT('Ctrl Pts',(178.080359665454,536.327834024376,-47.5221601717598)) ;
#67477 = CARTESIAN_POINT('Ctrl Pts',(178.090820450542,536.35050569072,-47.5221601717597)) ;
#67478 = CARTESIAN_POINT('Ctrl Pts',(178.095699449288,536.361079947886,-47.5221601717597)) ;
#67479 = CARTESIAN_POINT('Ctrl Pts',(178.100676236072,536.371610900689,-47.5221601717599)) ;
#67480 = CARTESIAN_POINT('Ctrl Pts',(178.105751019838,536.382096803783,-47.5221601717599)) ;
#67481 = CARTESIAN_POINT('Ctrl Pts',(178.110986048596,536.392913817235,-47.5221601717598)) ;
#67482 = CARTESIAN_POINT('Ctrl Pts',(178.116321690533,536.403675247986,-47.5221601717598)) ;
#67483 = CARTESIAN_POINT('Ctrl Pts',(178.121755909257,536.414375873961,-47.5221601717598)) ;
#67484 = CARTESIAN_POINT('Ctrl Pts',(178.152913046783,536.475728000555,-47.5221601717598)) ;
#67485 = CARTESIAN_POINT('Ctrl Pts',(178.18732636127,536.535122762543,-47.5221601717595)) ;
#67486 = CARTESIAN_POINT('Ctrl Pts',(178.224972467088,536.592256182975,-47.5221601717596)) ;
#67487 = CARTESIAN_POINT('Ctrl Pts',(178.259333258394,536.644403662598,-47.5221601717597)) ;
#67488 = CARTESIAN_POINT('Ctrl Pts',(178.296387871761,536.694667427142,-47.5221601717599)) ;
#67489 = CARTESIAN_POINT('Ctrl Pts',(178.336145770263,536.742789884874,-47.5221601717597)) ;
#67490 = CARTESIAN_POINT('Ctrl Pts',(178.382874729947,536.799350026934,-47.5221601717594)) ;
#67491 = CARTESIAN_POINT('Ctrl Pts',(178.433338910899,536.852953497548,-47.5221601717598)) ;
#67492 = CARTESIAN_POINT('Ctrl Pts',(178.487162118891,536.903396221338,-47.5221601717598)) ;
#67493 = CARTESIAN_POINT('Ctrl Pts',(178.499101622087,536.914585837943,-47.5221601717598)) ;
#67494 = CARTESIAN_POINT('Ctrl Pts',(178.511206491567,536.925619691031,-47.52216017176)) ;
#67495 = CARTESIAN_POINT('Ctrl Pts',(178.523472724127,536.936495150239,-47.5221601717599)) ;
#67496 = CARTESIAN_POINT('Ctrl Pts',(178.535480971503,536.947141875209,-47.5221601717598)) ;
#67497 = CARTESIAN_POINT('Ctrl Pts',(178.547648009925,536.957640100201,-47.5221601717596)) ;
#67498 = CARTESIAN_POINT('Ctrl Pts',(178.55994596626,536.967967484784,-47.5221601717596)) ;
#67499 = CARTESIAN_POINT('Ctrl Pts',(178.612452758427,537.012060813882,-47.5221601717597)) ;
#67500 = CARTESIAN_POINT('Ctrl Pts',(178.66741222166,537.053107645582,-47.5221601717598)) ;
#67501 = CARTESIAN_POINT('Ctrl Pts',(178.724486522341,537.090992984155,-47.5221601717597)) ;
#67502 = CARTESIAN_POINT('Ctrl Pts',(178.781553853922,537.128873696712,-47.5221601717596)) ;
#67503 = CARTESIAN_POINT('Ctrl Pts',(178.840736622279,537.163593998352,-47.5221601717598)) ;
#67504 = CARTESIAN_POINT('Ctrl Pts',(178.901716254342,537.194990744259,-47.5221601717599)) ;
#67505 = CARTESIAN_POINT('Ctrl Pts',(178.946296867578,537.217944083576,-47.52216017176)) ;
#67506 = CARTESIAN_POINT('Ctrl Pts',(178.991838306226,537.239120104217,-47.5221601717598)) ;
#67507 = CARTESIAN_POINT('Ctrl Pts',(179.038217446212,537.258437323501,-47.5221601717598)) ;
#67508 = CARTESIAN_POINT('Ctrl Pts',(179.057395867761,537.266425263223,-47.5221601717598)) ;
#67509 = CARTESIAN_POINT('Ctrl Pts',(179.076717520864,537.274095175778,-47.5221601717596)) ;
#67510 = CARTESIAN_POINT('Ctrl Pts',(179.096173599739,537.28144050651,-47.5221601717598)) ;
#67511 = CARTESIAN_POINT('Ctrl Pts',(179.110613234786,537.28689195928,-47.5221601717599)) ;
#67512 = CARTESIAN_POINT('Ctrl Pts',(179.125126911539,537.292164619533,-47.5221601717598)) ;
#67513 = CARTESIAN_POINT('Ctrl Pts',(179.139710990113,537.297255637053,-47.5221601717597)) ;
#67514 = CARTESIAN_POINT('Ctrl Pts',(179.151984119639,537.301539947312,-47.5221601717596)) ;
#67515 = CARTESIAN_POINT('Ctrl Pts',(179.164299151377,537.305692812503,-47.5221601717595)) ;
#67516 = CARTESIAN_POINT('Ctrl Pts',(179.176650337018,537.309711942362,-47.5221601717596)) ;
#67517 = CARTESIAN_POINT('Ctrl Pts',(179.239266573345,537.330087539685,-47.5221601717596)) ;
#67518 = CARTESIAN_POINT('Ctrl Pts',(179.302841192719,537.347040105753,-47.5221601717595)) ;
#67519 = CARTESIAN_POINT('Ctrl Pts',(179.367083250977,537.360401823903,-47.5221601717597)) ;
#67520 = CARTESIAN_POINT('Ctrl Pts',(179.412568679346,537.369862346966,-47.5221601717598)) ;
#67521 = CARTESIAN_POINT('Ctrl Pts',(179.45838882661,537.377521747157,-47.5221601717597)) ;
#67522 = CARTESIAN_POINT('Ctrl Pts',(179.504437996434,537.383304904446,-47.5221601717596)) ;
#67523 = CARTESIAN_POINT('Ctrl Pts',(179.519147966194,537.385152279093,-47.5221601717596)) ;
#67524 = CARTESIAN_POINT('Ctrl Pts',(179.533883525363,537.386808314458,-47.5221601717597)) ;
#67525 = CARTESIAN_POINT('Ctrl Pts',(179.548633901525,537.388269569041,-47.5221601717598)) ;
#67526 = CARTESIAN_POINT('Ctrl Pts',(179.61138415443,537.394485959298,-47.52216017176)) ;
#67527 = CARTESIAN_POINT('Ctrl Pts',(179.67428672212,537.397170662507,-47.5221601717597)) ;
#67528 = CARTESIAN_POINT('Ctrl Pts',(179.737075115641,537.396154950622,-47.5221601717598)) ;
#67529 = CARTESIAN_POINT('Ctrl Pts',(179.795567221839,537.395208738685,-47.52216017176)) ;
#67530 = CARTESIAN_POINT('Ctrl Pts',(179.853960722779,537.39105084576,-47.5221601717601)) ;
#67531 = CARTESIAN_POINT('Ctrl Pts',(179.912027332698,537.383506164524,-47.5221601717599)) ;
#67532 = CARTESIAN_POINT('Ctrl Pts',(179.921942002788,537.382217936651,-47.5221601717599)) ;
#67533 = CARTESIAN_POINT('Ctrl Pts',(179.931847101145,537.380830877618,-47.52216017176)) ;
#67534 = CARTESIAN_POINT('Ctrl Pts',(179.94174145373,537.379345629264,-47.52216017176)) ;
#67535 = CARTESIAN_POINT('Ctrl Pts',(178.619456745554,536.789923813584,-49.5221601717597)) ;
#67536 = CARTESIAN_POINT('Ctrl Pts',(178.574187252732,536.747692181376,-49.5221601717596)) ;
#67537 = CARTESIAN_POINT('Ctrl Pts',(178.531651301387,536.702886203401,-49.5221601717594)) ;
#67538 = CARTESIAN_POINT('Ctrl Pts',(178.491845127613,536.655851978916,-49.5221601717595)) ;
#67539 = CARTESIAN_POINT('Ctrl Pts',(178.449308935779,536.605592016557,-49.5221601717595)) ;
#67540 = CARTESIAN_POINT('Ctrl Pts',(178.409889057913,536.552787473376,-49.5221601717596)) ;
#67541 = CARTESIAN_POINT('Ctrl Pts',(178.373610042644,536.497805513443,-49.5221601717596)) ;
#67542 = CARTESIAN_POINT('Ctrl Pts',(178.341865904283,536.449696298502,-49.5221601717596)) ;
#67543 = CARTESIAN_POINT('Ctrl Pts',(178.31252673872,536.399918761028,-49.52216017176)) ;
#67544 = CARTESIAN_POINT('Ctrl Pts',(178.285632078592,536.348691089427,-49.5221601717597)) ;
#67545 = CARTESIAN_POINT('Ctrl Pts',(178.272117344439,536.322948865519,-49.5221601717596)) ;
#67546 = CARTESIAN_POINT('Ctrl Pts',(178.259220242575,536.296840105165,-49.5221601717596)) ;
#67547 = CARTESIAN_POINT('Ctrl Pts',(178.246948159264,536.270390629596,-49.5221601717598)) ;
#67548 = CARTESIAN_POINT('Ctrl Pts',(178.241395541397,536.258423319165,-49.5221601717599)) ;
#67549 = CARTESIAN_POINT('Ctrl Pts',(178.235970381399,536.246384756721,-49.5221601717596)) ;
#67550 = CARTESIAN_POINT('Ctrl Pts',(178.230681666114,536.234296885241,-49.5221601717596)) ;
#67551 = CARTESIAN_POINT('Ctrl Pts',(178.203843422477,536.17295547766,-49.5221601717596)) ;
#67552 = CARTESIAN_POINT('Ctrl Pts',(178.180463478443,536.110237033969,-49.5221601717599)) ;
#67553 = CARTESIAN_POINT('Ctrl Pts',(178.160562809962,536.046500976405,-49.5221601717598)) ;
#67554 = CARTESIAN_POINT('Ctrl Pts',(178.140300022872,535.981605158178,-49.5221601717598)) ;
#67555 = CARTESIAN_POINT('Ctrl Pts',(178.123643729798,535.915653513645,-49.5221601717599)) ;
#67556 = CARTESIAN_POINT('Ctrl Pts',(178.110655417353,535.848988876354,-49.5221601717597)) ;
#67557 = CARTESIAN_POINT('Ctrl Pts',(178.099760971122,535.793071349764,-49.5221601717596)) ;
#67558 = CARTESIAN_POINT('Ctrl Pts',(178.091447740656,535.736651240133,-49.5221601717597)) ;
#67559 = CARTESIAN_POINT('Ctrl Pts',(178.085777052212,535.679918461616,-49.5221601717597)) ;
#67560 = CARTESIAN_POINT('Ctrl Pts',(178.083157269475,535.653708671526,-49.5221601717597)) ;
#67561 = CARTESIAN_POINT('Ctrl Pts',(178.081101828741,535.627432033194,-49.52216017176)) ;
#67562 = CARTESIAN_POINT('Ctrl Pts',(178.079618613066,535.601106865551,-49.5221601717599)) ;
#67563 = CARTESIAN_POINT('Ctrl Pts',(178.078979635639,535.589765839312,-49.5221601717599)) ;
#67564 = CARTESIAN_POINT('Ctrl Pts',(178.078446992385,535.578416386461,-49.5221601717598)) ;
#67565 = CARTESIAN_POINT('Ctrl Pts',(178.078021602998,535.567073472083,-49.5221601717598)) ;
#67566 = CARTESIAN_POINT('Ctrl Pts',(178.075389312044,535.496884013118,-49.52216017176)) ;
#67567 = CARTESIAN_POINT('Ctrl Pts',(178.076851985684,535.4268141808,-49.5221601717599)) ;
#67568 = CARTESIAN_POINT('Ctrl Pts',(178.082461748157,535.357227447347,-49.5221601717599)) ;
#67569 = CARTESIAN_POINT('Ctrl Pts',(178.087506025577,535.294655317063,-49.5221601717599)) ;
#67570 = CARTESIAN_POINT('Ctrl Pts',(178.095903772788,535.232472824493,-49.52216017176)) ;
#67571 = CARTESIAN_POINT('Ctrl Pts',(178.107726699417,535.170931882839,-49.52216017176)) ;
#67572 = CARTESIAN_POINT('Ctrl Pts',(178.120540767056,535.104231833544,-49.5221601717599)) ;
#67573 = CARTESIAN_POINT('Ctrl Pts',(178.137377321743,535.038284558039,-49.52216017176)) ;
#67574 = CARTESIAN_POINT('Ctrl Pts',(178.157992254397,534.97330220996,-49.5221601717597)) ;
#67575 = CARTESIAN_POINT('Ctrl Pts',(178.165861208992,534.948497707562,-49.5221601717596)) ;
#67576 = CARTESIAN_POINT('Ctrl Pts',(178.17428123032,534.923833847552,-49.5221601717598)) ;
#67577 = CARTESIAN_POINT('Ctrl Pts',(178.183240678315,534.899322746024,-49.5221601717597)) ;
#67578 = CARTESIAN_POINT('Ctrl Pts',(178.187186661782,534.888527393294,-49.5221601717596)) ;
#67579 = CARTESIAN_POINT('Ctrl Pts',(178.191237016904,534.877762667777,-49.5221601717597)) ;
#67580 = CARTESIAN_POINT('Ctrl Pts',(178.195385896106,534.867041496919,-49.5221601717597)) ;
#67581 = CARTESIAN_POINT('Ctrl Pts',(178.220638770266,534.801785227622,-49.5221601717595)) ;
#67582 = CARTESIAN_POINT('Ctrl Pts',(178.249579684661,534.73802478725,-49.5221601717595)) ;
#67583 = CARTESIAN_POINT('Ctrl Pts',(178.281896894921,534.675977325775,-49.5221601717595)) ;
#67584 = CARTESIAN_POINT('Ctrl Pts',(178.314954579631,534.612508189609,-49.5221601717596)) ;
#67585 = CARTESIAN_POINT('Ctrl Pts',(178.351545356018,534.550830612049,-49.5221601717594)) ;
#67586 = CARTESIAN_POINT('Ctrl Pts',(178.391391642872,534.491180913923,-49.5221601717596)) ;
#67587 = CARTESIAN_POINT('Ctrl Pts',(178.421500896408,534.446107507438,-49.5221601717597)) ;
#67588 = CARTESIAN_POINT('Ctrl Pts',(178.453470210955,534.402191977027,-49.5221601717595)) ;
#67589 = CARTESIAN_POINT('Ctrl Pts',(178.487198516698,534.359542165663,-49.5221601717594)) ;
#67590 = CARTESIAN_POINT('Ctrl Pts',(178.508099216798,534.333113001879,-49.5221601717593)) ;
#67591 = CARTESIAN_POINT('Ctrl Pts',(178.529675677596,534.307169993219,-49.5221601717598)) ;
#67592 = CARTESIAN_POINT('Ctrl Pts',(178.551906570558,534.281740380727,-49.5221601717596)) ;
#67593 = CARTESIAN_POINT('Ctrl Pts',(178.560406742799,534.272017150689,-49.5221601717596)) ;
#67594 = CARTESIAN_POINT('Ctrl Pts',(178.569004153348,534.262367300958,-49.5221601717594)) ;
#67595 = CARTESIAN_POINT('Ctrl Pts',(178.57769265657,534.252797932049,-49.5221601717594)) ;
#67596 = CARTESIAN_POINT('Ctrl Pts',(178.629269599752,534.19599196859,-49.5221601717595)) ;
#67597 = CARTESIAN_POINT('Ctrl Pts',(178.683926012683,534.14215676504,-49.5221601717594)) ;
#67598 = CARTESIAN_POINT('Ctrl Pts',(178.741350969432,534.091573289781,-49.5221601717595)) ;
#67599 = CARTESIAN_POINT('Ctrl Pts',(178.784419686994,534.053635683337,-49.5221601717596)) ;
#67600 = CARTESIAN_POINT('Ctrl Pts',(178.829047013371,534.017527359659,-49.5221601717598)) ;
#67601 = CARTESIAN_POINT('Ctrl Pts',(178.875120393075,533.98337736097,-49.5221601717596)) ;
#67602 = CARTESIAN_POINT('Ctrl Pts',(178.891465719858,533.971262059427,-49.5221601717596)) ;
#67603 = CARTESIAN_POINT('Ctrl Pts',(178.907993178436,533.959393336413,-49.5221601717597)) ;
#67604 = CARTESIAN_POINT('Ctrl Pts',(178.924698155776,533.947777330454,-49.5221601717595)) ;
#67605 = CARTESIAN_POINT('Ctrl Pts',(178.937350560939,533.938979329069,-49.5221601717593)) ;
#67606 = CARTESIAN_POINT('Ctrl Pts',(178.950100677659,533.930329252443,-49.5221601717598)) ;
#67607 = CARTESIAN_POINT('Ctrl Pts',(178.962939518692,533.921833878502,-49.5221601717598)) ;
#67608 = CARTESIAN_POINT('Ctrl Pts',(179.025745012568,533.880275909628,-49.5221601717594)) ;
#67609 = CARTESIAN_POINT('Ctrl Pts',(179.090718120166,533.842384191777,-49.5221601717596)) ;
#67610 = CARTESIAN_POINT('Ctrl Pts',(179.157597555806,533.808435017296,-49.5221601717596)) ;
#67611 = CARTESIAN_POINT('Ctrl Pts',(179.211636829747,533.781003734088,-49.5221601717595)) ;
#67612 = CARTESIAN_POINT('Ctrl Pts',(179.266921689961,533.756146738752,-49.5221601717597)) ;
#67613 = CARTESIAN_POINT('Ctrl Pts',(179.323331161757,533.734028136155,-49.5221601717596)) ;
#67614 = CARTESIAN_POINT('Ctrl Pts',(179.333816071531,533.729916919631,-49.5221601717596)) ;
#67615 = CARTESIAN_POINT('Ctrl Pts',(179.344339870159,533.725900363626,-49.5221601717973)) ;
#67616 = CARTESIAN_POINT('Ctrl Pts',(179.354901398821,533.721978117668,-49.5221601717672)) ;
#67617 = CARTESIAN_POINT('Ctrl Pts',(179.941713456053,537.375715984761,-47.5212802703069)) ;
#67618 = CARTESIAN_POINT('Ctrl Pts',(179.949414502833,537.375470009103,-47.5215735707912)) ;
#67619 = CARTESIAN_POINT('Ctrl Pts',(179.957113843187,537.375170608489,-47.5218668712755)) ;
#67620 = CARTESIAN_POINT('Ctrl Pts',(179.964810736065,537.374817811737,-47.5221601717598)) ;
#67621 = CARTESIAN_POINT('Ctrl Pts',(30.4192289578182,533.719780492321,-49.5190019961068)) ;
#67622 = CARTESIAN_POINT('Ctrl Pts',(31.0820274042068,533.896441620623,-49.4819110709933)) ;
#67623 = CARTESIAN_POINT('Ctrl Pts',(32.2049962015177,534.964137330925,-49.4077460639272)) ;
#67624 = CARTESIAN_POINT('Ctrl Pts',(31.7732154512908,537.256615082637,-49.2965069749086)) ;
#67625 = CARTESIAN_POINT('Ctrl Pts',(29.6099672236945,538.131053118425,-49.1852847290511)) ;
#67626 = CARTESIAN_POINT('Ctrl Pts',(27.7035979429832,536.788246892714,-49.0740624831937)) ;
#67627 = CARTESIAN_POINT('Ctrl Pts',(27.7990747419387,534.457523563324,-48.9628402373363)) ;
#67628 = CARTESIAN_POINT('Ctrl Pts',(29.8100295710541,533.275586941982,-48.851617991479)) ;
#67629 = CARTESIAN_POINT('Ctrl Pts',(31.8927661072245,534.32548376863,-48.7403957456217)) ;
#67630 = CARTESIAN_POINT('Ctrl Pts',(32.1385149627165,536.644977564754,-48.6291734997644)) ;
#67631 = CARTESIAN_POINT('Ctrl Pts',(30.3219274024078,538.107999152117,-48.5179512539069)) ;
#67632 = CARTESIAN_POINT('Ctrl Pts',(28.1081040068838,537.373579279037,-48.4067290080494)) ;
#67633 = CARTESIAN_POINT('Ctrl Pts',(27.5261821604246,535.114873113739,-48.295506762192)) ;
#67634 = CARTESIAN_POINT('Ctrl Pts',(29.1095409923539,533.402156751141,-48.1842845163347)) ;
#67635 = CARTESIAN_POINT('Ctrl Pts',(31.4069089296102,533.805324868808,-48.0730622704775)) ;
#67636 = CARTESIAN_POINT('Ctrl Pts',(32.3125038989418,535.954737015706,-47.9618400246202)) ;
#67637 = CARTESIAN_POINT('Ctrl Pts',(30.9963380933565,537.880515059464,-47.8506177787627)) ;
#67638 = CARTESIAN_POINT('Ctrl Pts',(28.664524458328,537.817015226414,-47.7393955329052)) ;
#67639 = CARTESIAN_POINT('Ctrl Pts',(27.4546872795412,535.823609498753,-47.6281732870478)) ;
#67640 = CARTESIAN_POINT('Ctrl Pts',(28.4744419640535,533.724946792159,-47.5169510411904)) ;
#67641 = CARTESIAN_POINT('Ctrl Pts',(30.7909517769799,533.450325076242,-47.405714548837)) ;
#67642 = CARTESIAN_POINT('Ctrl Pts',(31.7796627542034,534.643320901683,-47.3315521384358)) ;
#67643 = CARTESIAN_POINT('Ctrl Pts',(31.9108094354616,535.316555260834,-47.2944638099872)) ;
#67644 = CARTESIAN_POINT('Ctrl Pts',(30.3850879802084,533.847851274574,-49.5955259181223)) ;
#67645 = CARTESIAN_POINT('Ctrl Pts',(31.005247402468,534.013147472626,-49.5584349930087)) ;
#67646 = CARTESIAN_POINT('Ctrl Pts',(32.0559735837837,535.0121563847,-49.4842699859427)) ;
#67647 = CARTESIAN_POINT('Ctrl Pts',(31.6519700710076,537.157154891849,-49.3730308969241)) ;
#67648 = CARTESIAN_POINT('Ctrl Pts',(29.6278875187022,537.975338745523,-49.2618086510667)) ;
#67649 = CARTESIAN_POINT('Ctrl Pts',(27.8441584255201,536.718917675618,-49.1505864052093)) ;
#67650 = CARTESIAN_POINT('Ctrl Pts',(27.9334930291271,534.538133998049,-49.0393641593519)) ;
#67651 = CARTESIAN_POINT('Ctrl Pts',(29.8150794930204,533.43223349959,-48.9281419134946)) ;
#67652 = CARTESIAN_POINT('Ctrl Pts',(31.7638298167847,534.414588562422,-48.8169196676373)) ;
#67653 = CARTESIAN_POINT('Ctrl Pts',(31.9937692034465,536.584865122932,-48.70569742178)) ;
#67654 = CARTESIAN_POINT('Ctrl Pts',(30.2940460100332,537.95376788261,-48.5944751759224)) ;
#67655 = CARTESIAN_POINT('Ctrl Pts',(28.2226418819252,537.266594569717,-48.483252930065)) ;
#67656 = CARTESIAN_POINT('Ctrl Pts',(27.678156121485,535.153195061679,-48.3720306842076)) ;
#67657 = CARTESIAN_POINT('Ctrl Pts',(29.1596546129031,533.550660843757,-48.2608084383503)) ;
#67658 = CARTESIAN_POINT('Ctrl Pts',(31.3092287111068,533.927892426434,-48.149586192493)) ;
#67659 = CARTESIAN_POINT('Ctrl Pts',(32.1565651163773,535.939028998164,-48.0383639466357)) ;
#67660 = CARTESIAN_POINT('Ctrl Pts',(30.9250706401349,537.740918253523,-47.9271417007783)) ;
#67661 = CARTESIAN_POINT('Ctrl Pts',(28.7432667982648,537.681503479708,-47.8159194549208)) ;
#67662 = CARTESIAN_POINT('Ctrl Pts',(27.6112606357387,535.816337151797,-47.7046972090634)) ;
#67663 = CARTESIAN_POINT('Ctrl Pts',(28.5654126550131,533.85268521699,-47.593474963206)) ;
#67664 = CARTESIAN_POINT('Ctrl Pts',(30.7328971973664,533.595730413291,-47.4822384708525)) ;
#67665 = CARTESIAN_POINT('Ctrl Pts',(31.6580026072502,534.711978657226,-47.4080760604514)) ;
#67666 = CARTESIAN_POINT('Ctrl Pts',(31.7807123850468,535.341902631084,-47.3709877320027)) ;
#67667 = CARTESIAN_POINT('Ctrl Pts',(30.3509470025985,533.975922056826,-49.6720498401378)) ;
#67668 = CARTESIAN_POINT('Ctrl Pts',(30.9284674007291,534.12985332463,-49.6349589150241)) ;
#67669 = CARTESIAN_POINT('Ctrl Pts',(31.9069509660495,535.060175438473,-49.5607939079581)) ;
#67670 = CARTESIAN_POINT('Ctrl Pts',(31.5307246907242,537.057694701061,-49.4495548189396)) ;
#67671 = CARTESIAN_POINT('Ctrl Pts',(29.6458078137101,537.819624372623,-49.3383325730821)) ;
#67672 = CARTESIAN_POINT('Ctrl Pts',(27.984718908057,536.649588458522,-49.2271103272247)) ;
#67673 = CARTESIAN_POINT('Ctrl Pts',(28.0679113163154,534.618744432776,-49.1158880813673)) ;
#67674 = CARTESIAN_POINT('Ctrl Pts',(29.8201294149866,533.5888800572,-49.00466583551)) ;
#67675 = CARTESIAN_POINT('Ctrl Pts',(31.6348935263451,534.503693356214,-48.8934435896527)) ;
#67676 = CARTESIAN_POINT('Ctrl Pts',(31.8490234441765,536.524752681109,-48.7822213437953)) ;
#67677 = CARTESIAN_POINT('Ctrl Pts',(30.2661646176585,537.799536613104,-48.6709990979379)) ;
#67678 = CARTESIAN_POINT('Ctrl Pts',(28.3371797569666,537.159609860397,-48.5597768520804)) ;
#67679 = CARTESIAN_POINT('Ctrl Pts',(27.8301300825456,535.191517009621,-48.448554606223)) ;
#67680 = CARTESIAN_POINT('Ctrl Pts',(29.2097682334523,533.699164936375,-48.3373323603657)) ;
#67681 = CARTESIAN_POINT('Ctrl Pts',(31.2115484926033,534.050459984059,-48.2261101145084)) ;
#67682 = CARTESIAN_POINT('Ctrl Pts',(32.000626333813,535.92332098062,-48.1148878686511)) ;
#67683 = CARTESIAN_POINT('Ctrl Pts',(30.8538031869134,537.601321447584,-48.0036656227937)) ;
#67684 = CARTESIAN_POINT('Ctrl Pts',(28.8220091382015,537.545991733002,-47.8924433769362)) ;
#67685 = CARTESIAN_POINT('Ctrl Pts',(27.7678339919361,535.809064804842,-47.7812211310788)) ;
#67686 = CARTESIAN_POINT('Ctrl Pts',(28.6563833459727,533.980423641819,-47.6699988852214)) ;
#67687 = CARTESIAN_POINT('Ctrl Pts',(30.674842617753,533.741135750339,-47.558762392868)) ;
#67688 = CARTESIAN_POINT('Ctrl Pts',(31.536342460297,534.780636412768,-47.4845999824669)) ;
#67689 = CARTESIAN_POINT('Ctrl Pts',(31.6506153346321,535.367250001332,-47.4475116540181)) ;
#67690 = CARTESIAN_POINT('Ctrl Pts',(30.3168060249887,534.103992839079,-49.7485737621533)) ;
#67691 = CARTESIAN_POINT('Ctrl Pts',(30.8516873989902,534.246559176633,-49.7114828370396)) ;
#67692 = CARTESIAN_POINT('Ctrl Pts',(31.7579283483155,535.108194492247,-49.6373178299737)) ;
#67693 = CARTESIAN_POINT('Ctrl Pts',(31.4094793104411,536.958234510272,-49.5260787409551)) ;
#67694 = CARTESIAN_POINT('Ctrl Pts',(29.663728108718,537.663909999721,-49.4148564950976)) ;
#67695 = CARTESIAN_POINT('Ctrl Pts',(28.1252793905938,536.580259241425,-49.3036342492401)) ;
#67696 = CARTESIAN_POINT('Ctrl Pts',(28.2023296035037,534.699354867503,-49.1924120033828)) ;
#67697 = CARTESIAN_POINT('Ctrl Pts',(29.825179336953,533.74552661481,-49.0811897575255)) ;
#67698 = CARTESIAN_POINT('Ctrl Pts',(31.5059572359054,534.592798150006,-48.9699675116682)) ;
#67699 = CARTESIAN_POINT('Ctrl Pts',(31.7042776849064,536.464640239286,-48.8587452658108)) ;
#67700 = CARTESIAN_POINT('Ctrl Pts',(30.238283225284,537.645305343598,-48.7475230199534)) ;
#67701 = CARTESIAN_POINT('Ctrl Pts',(28.451717632008,537.052625151078,-48.6363007740959)) ;
#67702 = CARTESIAN_POINT('Ctrl Pts',(27.9821040436063,535.229838957562,-48.5250785282385)) ;
#67703 = CARTESIAN_POINT('Ctrl Pts',(29.2598818540015,533.847669028992,-48.4138562823812)) ;
#67704 = CARTESIAN_POINT('Ctrl Pts',(31.1138682740999,534.173027541684,-48.3026340365239)) ;
#67705 = CARTESIAN_POINT('Ctrl Pts',(31.8446875512484,535.907612963078,-48.1914117906666)) ;
#67706 = CARTESIAN_POINT('Ctrl Pts',(30.782535733692,537.461724641643,-48.0801895448092)) ;
#67707 = CARTESIAN_POINT('Ctrl Pts',(28.9007514781382,537.410479986295,-47.9689672989517)) ;
#67708 = CARTESIAN_POINT('Ctrl Pts',(27.9244073481337,535.801792457886,-47.8577450530943)) ;
#67709 = CARTESIAN_POINT('Ctrl Pts',(28.7473540369323,534.108162066649,-47.7465228072369)) ;
#67710 = CARTESIAN_POINT('Ctrl Pts',(30.6167880381395,533.886541087388,-47.6352863148834)) ;
#67711 = CARTESIAN_POINT('Ctrl Pts',(31.4146823133438,534.84929416831,-47.5611239044823)) ;
#67712 = CARTESIAN_POINT('Ctrl Pts',(31.5205182842175,535.392597371584,-47.5240355760335)) ;
#67713 = CARTESIAN_POINT('Ctrl Pts',(31.5236569526584,535.391334705934,-47.522160171753)) ;
#67714 = CARTESIAN_POINT('Ctrl Pts',(31.5186994705276,535.327491770809,-47.522160171753)) ;
#67715 = CARTESIAN_POINT('Ctrl Pts',(31.5097667931575,535.264218142824,-47.522160171753)) ;
#67716 = CARTESIAN_POINT('Ctrl Pts',(31.4971597796669,535.201749103154,-47.522160171753)) ;
#67717 = CARTESIAN_POINT('Ctrl Pts',(31.4845527661763,535.139280063483,-47.522160171753)) ;
#67718 = CARTESIAN_POINT('Ctrl Pts',(31.468271074477,535.077614831876,-47.522160171753)) ;
#67719 = CARTESIAN_POINT('Ctrl Pts',(31.4485600751653,535.016978328503,-47.522160171753)) ;
#67720 = CARTESIAN_POINT('Ctrl Pts',(31.4307419234247,534.962164749493,-47.522160171753)) ;
#67721 = CARTESIAN_POINT('Ctrl Pts',(31.4101205948598,534.908191257982,-47.5221601717531)) ;
#67722 = CARTESIAN_POINT('Ctrl Pts',(31.386841891083,534.855224799164,-47.522160171753)) ;
#67723 = CARTESIAN_POINT('Ctrl Pts',(31.375142881693,534.828605829954,-47.5221601717529)) ;
#67724 = CARTESIAN_POINT('Ctrl Pts',(31.3627721928826,534.802241266862,-47.522160171753)) ;
#67725 = CARTESIAN_POINT('Ctrl Pts',(31.3497453957004,534.776152991293,-47.522160171753)) ;
#67726 = CARTESIAN_POINT('Ctrl Pts',(31.3438540878375,534.764354691155,-47.5221601717529)) ;
#67727 = CARTESIAN_POINT('Ctrl Pts',(31.337827729337,534.752611584923,-47.522160171753)) ;
#67728 = CARTESIAN_POINT('Ctrl Pts',(31.3316778572707,534.740944357343,-47.522160171753)) ;
#67729 = CARTESIAN_POINT('Ctrl Pts',(31.3004561004906,534.68171201269,-47.5221601717531)) ;
#67730 = CARTESIAN_POINT('Ctrl Pts',(31.2660015749929,534.624325135799,-47.5221601717529)) ;
#67731 = CARTESIAN_POINT('Ctrl Pts',(31.2285820548354,534.569024272131,-47.522160171753)) ;
#67732 = CARTESIAN_POINT('Ctrl Pts',(31.1904826176123,534.51271858529,-47.5221601717531)) ;
#67733 = CARTESIAN_POINT('Ctrl Pts',(31.1493091452131,534.458574448788,-47.5221601717529)) ;
#67734 = CARTESIAN_POINT('Ctrl Pts',(31.1052911573092,534.406853723098,-47.522160171753)) ;
#67735 = CARTESIAN_POINT('Ctrl Pts',(31.0683720694782,534.363474138857,-47.5221601717531)) ;
#67736 = CARTESIAN_POINT('Ctrl Pts',(31.0294508873193,534.321799175608,-47.5221601717531)) ;
#67737 = CARTESIAN_POINT('Ctrl Pts',(30.9886377240086,534.281995176134,-47.5221601717531)) ;
#67738 = CARTESIAN_POINT('Ctrl Pts',(30.9697790441985,534.263602804155,-47.5221601717531)) ;
#67739 = CARTESIAN_POINT('Ctrl Pts',(30.9505161023597,534.245610099233,-47.5221601717531)) ;
#67740 = CARTESIAN_POINT('Ctrl Pts',(30.9308582982733,534.228034654789,-47.5221601717529)) ;
#67741 = CARTESIAN_POINT('Ctrl Pts',(30.9223934077021,534.220466453717,-47.5221601717529)) ;
#67742 = CARTESIAN_POINT('Ctrl Pts',(30.9138556834697,534.212976101739,-47.5221601717529)) ;
#67743 = CARTESIAN_POINT('Ctrl Pts',(30.9052562285359,534.205573628438,-47.5221601717529)) ;
#67744 = CARTESIAN_POINT('Ctrl Pts',(30.8520268008585,534.159753350261,-47.5221601717529)) ;
#67745 = CARTESIAN_POINT('Ctrl Pts',(30.7963374348611,534.117209332328,-47.5221601717531)) ;
#67746 = CARTESIAN_POINT('Ctrl Pts',(30.7384395986102,534.078208963547,-47.522160171753)) ;
#67747 = CARTESIAN_POINT('Ctrl Pts',(30.6863848595582,534.043144544024,-47.5221601717529)) ;
#67748 = CARTESIAN_POINT('Ctrl Pts',(30.6325439543738,534.010944257277,-47.522160171753)) ;
#67749 = CARTESIAN_POINT('Ctrl Pts',(30.5770689192711,533.981821161704,-47.5221601717529)) ;
#67750 = CARTESIAN_POINT('Ctrl Pts',(30.5169372524336,533.950253443414,-47.5221601717529)) ;
#67751 = CARTESIAN_POINT('Ctrl Pts',(30.4548855870198,533.922299856533,-47.522160171753)) ;
#67752 = CARTESIAN_POINT('Ctrl Pts',(30.3912320560275,533.897901819146,-47.5221601717529)) ;
#67753 = CARTESIAN_POINT('Ctrl Pts',(30.3669330318675,533.88858814101,-47.5221601717528)) ;
#67754 = CARTESIAN_POINT('Ctrl Pts',(30.3424002759375,533.879793049169,-47.5221601717531)) ;
#67755 = CARTESIAN_POINT('Ctrl Pts',(30.3176505254538,533.871514996581,-47.522160171753)) ;
#67756 = CARTESIAN_POINT('Ctrl Pts',(30.3067503928447,533.867869227667,-47.522160171753)) ;
#67757 = CARTESIAN_POINT('Ctrl Pts',(30.2958091142617,533.864324160259,-47.5221601717527)) ;
#67758 = CARTESIAN_POINT('Ctrl Pts',(30.2848404431185,533.86088328274,-47.5221601717527)) ;
#67759 = CARTESIAN_POINT('Ctrl Pts',(30.2180806724344,533.839940709925,-47.5221601717528)) ;
#67760 = CARTESIAN_POINT('Ctrl Pts',(30.1501904337754,533.822814034984,-47.5221601717527)) ;
#67761 = CARTESIAN_POINT('Ctrl Pts',(30.081533941393,533.809394915133,-47.5221601717529)) ;
#67762 = CARTESIAN_POINT('Ctrl Pts',(30.0113036312589,533.795668187825,-47.522160171753)) ;
#67763 = CARTESIAN_POINT('Ctrl Pts',(29.940270706767,533.785820668202,-47.5221601717528)) ;
#67764 = CARTESIAN_POINT('Ctrl Pts',(29.8687930800881,533.779782670237,-47.5221601717529)) ;
#67765 = CARTESIAN_POINT('Ctrl Pts',(29.8147780369742,533.775219805806,-47.522160171753)) ;
#67766 = CARTESIAN_POINT('Ctrl Pts',(29.7605082709567,533.772833387046,-47.5221601717526)) ;
#67767 = CARTESIAN_POINT('Ctrl Pts',(29.7061311783795,533.772611627013,-47.5221601717528)) ;
#67768 = CARTESIAN_POINT('Ctrl Pts',(29.6724350241176,533.772474207745,-47.522160171753)) ;
#67769 = CARTESIAN_POINT('Ctrl Pts',(29.6386975577268,533.773168325095,-47.5221601717526)) ;
#67770 = CARTESIAN_POINT('Ctrl Pts',(29.604953389941,533.774694287495,-47.522160171753)) ;
#67771 = CARTESIAN_POINT('Ctrl Pts',(29.5920528858034,533.77527766784,-47.5221601717531)) ;
#67772 = CARTESIAN_POINT('Ctrl Pts',(29.5791491157432,533.775982802408,-47.5221601717528)) ;
#67773 = CARTESIAN_POINT('Ctrl Pts',(29.5662514687581,533.77680931295,-47.5221601717528)) ;
#67774 = CARTESIAN_POINT('Ctrl Pts',(29.4896818934395,533.781716065419,-47.522160171753)) ;
#67775 = CARTESIAN_POINT('Ctrl Pts',(29.413514639897,533.79088260525,-47.5221601717528)) ;
#67776 = CARTESIAN_POINT('Ctrl Pts',(29.3381633346069,533.804241013433,-47.5221601717528)) ;
#67777 = CARTESIAN_POINT('Ctrl Pts',(29.2816498556393,533.81425981957,-47.5221601717527)) ;
#67778 = CARTESIAN_POINT('Ctrl Pts',(29.225594680158,533.826637686017,-47.5221601717529)) ;
#67779 = CARTESIAN_POINT('Ctrl Pts',(29.1701689140933,533.8413670658,-47.5221601717527)) ;
#67780 = CARTESIAN_POINT('Ctrl Pts',(29.1504944696968,533.846595543169,-47.5221601717526)) ;
#67781 = CARTESIAN_POINT('Ctrl Pts',(29.1308993321089,533.852120486841,-47.5221601717527)) ;
#67782 = CARTESIAN_POINT('Ctrl Pts',(29.1113911916752,533.857942117771,-47.5221601717528)) ;
#67783 = CARTESIAN_POINT('Ctrl Pts',(29.0966180285685,533.862350733936,-47.5221601717529)) ;
#67784 = CARTESIAN_POINT('Ctrl Pts',(29.0818996663657,533.86692809925,-47.5221601717528)) ;
#67785 = CARTESIAN_POINT('Ctrl Pts',(29.0672469809268,533.871671421633,-47.5221601717528)) ;
#67786 = CARTESIAN_POINT('Ctrl Pts',(28.9955972326579,533.894865658355,-47.522160171753)) ;
#67787 = CARTESIAN_POINT('Ctrl Pts',(28.9254624202921,533.92204042568,-47.5221601717529)) ;
#67788 = CARTESIAN_POINT('Ctrl Pts',(28.8572215630825,533.953163710321,-47.5221601717529)) ;
#67789 = CARTESIAN_POINT('Ctrl Pts',(28.8020993751403,533.978303833343,-47.522160171753)) ;
#67790 = CARTESIAN_POINT('Ctrl Pts',(28.7482125513535,534.00602120663,-47.5221601717529)) ;
#67791 = CARTESIAN_POINT('Ctrl Pts',(28.6957646816156,534.036323556823,-47.5221601717531)) ;
#67792 = CARTESIAN_POINT('Ctrl Pts',(28.6854183011059,534.042301295232,-47.5221601717531)) ;
#67793 = CARTESIAN_POINT('Ctrl Pts',(28.6751279406135,534.048379698197,-47.5221601717528)) ;
#67794 = CARTESIAN_POINT('Ctrl Pts',(28.6648941356016,534.054557422396,-47.5221601717531)) ;
#67795 = CARTESIAN_POINT('',(31.1586577691864,536.791421537165,-49.5230216451333)) ;
#67796 = CARTESIAN_POINT('Ctrl Pts',(31.1573042373964,536.790269707588,-49.5230216451333)) ;
#67797 = CARTESIAN_POINT('Ctrl Pts',(31.1524161449685,536.796013776525,-49.5227344873399)) ;
#67798 = CARTESIAN_POINT('Ctrl Pts',(31.1474890446894,536.801724650524,-49.5224473295465)) ;
#67799 = CARTESIAN_POINT('Ctrl Pts',(31.1425233909828,536.807401802874,-49.5221601717531)) ;
#67800 = CARTESIAN_POINT('Ctrl Pts',(30.4186978425951,533.72539083489,-49.5221601717531)) ;
#67801 = CARTESIAN_POINT('Ctrl Pts',(30.4873018263811,533.750792346629,-49.522160171753)) ;
#67802 = CARTESIAN_POINT('Ctrl Pts',(30.554203302766,533.780093658899,-49.5221601717531)) ;
#67803 = CARTESIAN_POINT('Ctrl Pts',(30.6192143952837,533.812998021653,-49.5221601717532)) ;
#67804 = CARTESIAN_POINT('Ctrl Pts',(30.6860861306996,533.84684412014,-49.5221601717532)) ;
#67805 = CARTESIAN_POINT('Ctrl Pts',(30.7509584997066,533.884503151209,-49.5221601717529)) ;
#67806 = CARTESIAN_POINT('Ctrl Pts',(30.8135958271794,533.925696927834,-49.522160171753)) ;
#67807 = CARTESIAN_POINT('Ctrl Pts',(30.8665864966189,533.960546527715,-49.5221601717532)) ;
#67808 = CARTESIAN_POINT('Ctrl Pts',(30.9179772112377,533.997927008956,-49.5221601717531)) ;
#67809 = CARTESIAN_POINT('Ctrl Pts',(30.9676024509393,534.037688046095,-49.522160171753)) ;
#67810 = CARTESIAN_POINT('Ctrl Pts',(30.9896090562751,534.055320312606,-49.522160171753)) ;
#67811 = CARTESIAN_POINT('Ctrl Pts',(31.0112681718102,534.073420901991,-49.5221601717529)) ;
#67812 = CARTESIAN_POINT('Ctrl Pts',(31.0325638136025,534.091977425642,-49.522160171753)) ;
#67813 = CARTESIAN_POINT('Ctrl Pts',(31.0442342273179,534.102146750908,-49.5221601717531)) ;
#67814 = CARTESIAN_POINT('Ctrl Pts',(31.0557954633371,534.112453011021,-49.5221601717531)) ;
#67815 = CARTESIAN_POINT('Ctrl Pts',(31.0672447584333,534.122894207908,-49.5221601717531)) ;
#67816 = CARTESIAN_POINT('Ctrl Pts',(31.0778839828076,534.132596659935,-49.5221601717531)) ;
#67817 = CARTESIAN_POINT('Ctrl Pts',(31.0884280589244,534.142417222811,-49.5221601717532)) ;
#67818 = CARTESIAN_POINT('Ctrl Pts',(31.0988586971619,534.152338637124,-49.5221601717532)) ;
#67819 = CARTESIAN_POINT('Ctrl Pts',(31.1519351779608,534.202823923289,-49.5221601717531)) ;
#67820 = CARTESIAN_POINT('Ctrl Pts',(31.2021716876196,534.256001695126,-49.5221601717531)) ;
#67821 = CARTESIAN_POINT('Ctrl Pts',(31.2493501345782,534.311609028577,-49.5221601717531)) ;
#67822 = CARTESIAN_POINT('Ctrl Pts',(31.2961737783185,534.366798169778,-49.5221601717531)) ;
#67823 = CARTESIAN_POINT('Ctrl Pts',(31.3399856917906,534.424381358109,-49.5221601717529)) ;
#67824 = CARTESIAN_POINT('Ctrl Pts',(31.3805278530913,534.484125791624,-49.5221601717529)) ;
#67825 = CARTESIAN_POINT('Ctrl Pts',(31.4142815272287,534.533866458518,-49.5221601717529)) ;
#67826 = CARTESIAN_POINT('Ctrl Pts',(31.4457681286474,534.585105851876,-49.5221601717531)) ;
#67827 = CARTESIAN_POINT('Ctrl Pts',(31.4748109615605,534.63771607303,-49.522160171753)) ;
#67828 = CARTESIAN_POINT('Ctrl Pts',(31.4868723497301,534.659564916114,-49.522160171753)) ;
#67829 = CARTESIAN_POINT('Ctrl Pts',(31.498511936526,534.681650225412,-49.522160171753)) ;
#67830 = CARTESIAN_POINT('Ctrl Pts',(31.5097156382178,534.703962916598,-49.522160171753)) ;
#67831 = CARTESIAN_POINT('Ctrl Pts',(31.5149427851672,534.714373022015,-49.522160171753)) ;
#67832 = CARTESIAN_POINT('Ctrl Pts',(31.5200750389261,534.724832622436,-49.5221601717529)) ;
#67833 = CARTESIAN_POINT('Ctrl Pts',(31.5251109030024,534.735340792977,-49.522160171753)) ;
#67834 = CARTESIAN_POINT('Ctrl Pts',(31.5303022079443,534.746173316816,-49.522160171753)) ;
#67835 = CARTESIAN_POINT('Ctrl Pts',(31.5353873889545,534.757049810725,-49.5221601717531)) ;
#67836 = CARTESIAN_POINT('Ctrl Pts',(31.5403636460063,534.767965454351,-49.5221601717531)) ;
#67837 = CARTESIAN_POINT('Ctrl Pts',(31.5689045556854,534.830571223217,-49.522160171753)) ;
#67838 = CARTESIAN_POINT('Ctrl Pts',(31.5938849702325,534.894502684949,-49.522160171753)) ;
#67839 = CARTESIAN_POINT('Ctrl Pts',(31.6150817999401,534.959552218106,-49.5221601717531)) ;
#67840 = CARTESIAN_POINT('Ctrl Pts',(31.6344288124596,535.018924971001,-49.5221601717531)) ;
#67841 = CARTESIAN_POINT('Ctrl Pts',(31.6506235210653,535.079229774877,-49.5221601717531)) ;
#67842 = CARTESIAN_POINT('Ctrl Pts',(31.6634586243526,535.140313572021,-49.5221601717531)) ;
#67843 = CARTESIAN_POINT('Ctrl Pts',(31.6785443557651,535.212108378556,-49.522160171753)) ;
#67844 = CARTESIAN_POINT('Ctrl Pts',(31.6889895128008,535.284980843413,-49.5221601717531)) ;
#67845 = CARTESIAN_POINT('Ctrl Pts',(31.6948691143251,535.358509502156,-49.5221601717531)) ;
#67846 = CARTESIAN_POINT('Ctrl Pts',(31.6961734172464,535.374820751141,-49.5221601717531)) ;
#67847 = CARTESIAN_POINT('Ctrl Pts',(31.6972528175616,535.391164207973,-49.5221601717531)) ;
#67848 = CARTESIAN_POINT('Ctrl Pts',(31.6981077549656,535.407535101245,-49.5221601717531)) ;
#67849 = CARTESIAN_POINT('Ctrl Pts',(31.6989446641061,535.423560777691,-49.5221601717531)) ;
#67850 = CARTESIAN_POINT('Ctrl Pts',(31.6995664742495,535.439618043232,-49.522160171753)) ;
#67851 = CARTESIAN_POINT('Ctrl Pts',(31.6999730977482,535.455671178293,-49.522160171753)) ;
#67852 = CARTESIAN_POINT('Ctrl Pts',(31.7017092506482,535.524212954849,-49.5221601717531)) ;
#67853 = CARTESIAN_POINT('Ctrl Pts',(31.6995342482065,535.592773413081,-49.5221601717531)) ;
#67854 = CARTESIAN_POINT('Ctrl Pts',(31.6935688364705,535.66101662413,-49.522160171753)) ;
#67855 = CARTESIAN_POINT('Ctrl Pts',(31.6876125268821,535.729155708289,-49.522160171753)) ;
#67856 = CARTESIAN_POINT('Ctrl Pts',(31.6778769035789,535.796979569927,-49.5221601717531)) ;
#67857 = CARTESIAN_POINT('Ctrl Pts',(31.6644327909043,535.864138816221,-49.5221601717531)) ;
#67858 = CARTESIAN_POINT('Ctrl Pts',(31.65457150191,535.913400284968,-49.5221601717531)) ;
#67859 = CARTESIAN_POINT('Ctrl Pts',(31.6427139028012,535.962303925143,-49.522160171753)) ;
#67860 = CARTESIAN_POINT('Ctrl Pts',(31.6288731470677,536.010701797538,-49.522160171753)) ;
#67861 = CARTESIAN_POINT('Ctrl Pts',(31.6231607179449,536.030676820657,-49.522160171753)) ;
#67862 = CARTESIAN_POINT('Ctrl Pts',(31.6171103358191,536.050565567194,-49.5221601717531)) ;
#67863 = CARTESIAN_POINT('Ctrl Pts',(31.6107223668049,536.070357063039,-49.522160171753)) ;
#67864 = CARTESIAN_POINT('Ctrl Pts',(31.605982706735,536.085041693219,-49.522160171753)) ;
#67865 = CARTESIAN_POINT('Ctrl Pts',(31.6010571935044,536.099672778431,-49.5221601717531)) ;
#67866 = CARTESIAN_POINT('Ctrl Pts',(31.5959458683123,536.114245698436,-49.5221601717531)) ;
#67867 = CARTESIAN_POINT('Ctrl Pts',(31.5916425233631,536.12651498269,-49.5221601717531)) ;
#67868 = CARTESIAN_POINT('Ctrl Pts',(31.5872102325381,536.138735072304,-49.5221601717531)) ;
#67869 = CARTESIAN_POINT('Ctrl Pts',(31.5826507943598,536.150900029629,-49.5221601717531)) ;
#67870 = CARTESIAN_POINT('Ctrl Pts',(31.5595404376064,536.212560368616,-49.5221601717531)) ;
#67871 = CARTESIAN_POINT('Ctrl Pts',(31.5331563054528,536.272836005059,-49.5221601717531)) ;
#67872 = CARTESIAN_POINT('Ctrl Pts',(31.5035486090204,536.331394754774,-49.5221601717531)) ;
#67873 = CARTESIAN_POINT('Ctrl Pts',(31.4825856728236,536.372855708579,-49.5221601717531)) ;
#67874 = CARTESIAN_POINT('Ctrl Pts',(31.4600059155797,536.413455468647,-49.5221601717531)) ;
#67875 = CARTESIAN_POINT('Ctrl Pts',(31.4358165118334,536.453064537015,-49.5221601717531)) ;
#67876 = CARTESIAN_POINT('Ctrl Pts',(31.4280894921966,536.465717186592,-49.5221601717531)) ;
#67877 = CARTESIAN_POINT('Ctrl Pts',(31.4201969312163,536.478270552164,-49.5221601717531)) ;
#67878 = CARTESIAN_POINT('Ctrl Pts',(31.4121428522646,536.490714068894,-49.5221601717531)) ;
#67879 = CARTESIAN_POINT('Ctrl Pts',(31.3778791836545,536.543651286935,-49.5221601717531)) ;
#67880 = CARTESIAN_POINT('Ctrl Pts',(31.3407594282531,536.594505707453,-49.5221601717532)) ;
#67881 = CARTESIAN_POINT('Ctrl Pts',(31.300817835818,536.64296371139,-49.5221601717531)) ;
#67882 = CARTESIAN_POINT('Ctrl Pts',(31.2636079488606,536.68810755115,-49.5221601717531)) ;
#67883 = CARTESIAN_POINT('Ctrl Pts',(31.2239484452003,536.731171720598,-49.5221601717532)) ;
#67884 = CARTESIAN_POINT('Ctrl Pts',(31.1818447665004,536.771868473735,-49.522160171753)) ;
#67885 = CARTESIAN_POINT('Ctrl Pts',(31.1746559175354,536.778817101995,-49.522160171753)) ;
#67886 = CARTESIAN_POINT('Ctrl Pts',(31.1673957685906,536.785696624249,-49.522160171753)) ;
#67887 = CARTESIAN_POINT('Ctrl Pts',(31.1600655534529,536.792506522884,-49.5221601717531)) ;
#67888 = CARTESIAN_POINT('Ctrl Pts',(28.6224008556909,536.788257168284,-49.5202847734518)) ;
#67889 = CARTESIAN_POINT('Ctrl Pts',(28.2636169540964,536.366767265057,-49.4831964450485)) ;
#67890 = CARTESIAN_POINT('Ctrl Pts',(28.0083851733653,535.142681732903,-49.4090340346928)) ;
#67891 = CARTESIAN_POINT('Ctrl Pts',(29.3472284941806,533.81927777062,-49.2977975423846)) ;
#67892 = CARTESIAN_POINT('Ctrl Pts',(31.1844609256909,534.231833414637,-49.1865752965273)) ;
#67893 = CARTESIAN_POINT('Ctrl Pts',(31.8334428866778,535.998170240813,-49.07535305067)) ;
#67894 = CARTESIAN_POINT('Ctrl Pts',(30.7002342883442,537.501358927502,-48.9641308048125)) ;
#67895 = CARTESIAN_POINT('Ctrl Pts',(28.8229400342555,537.362809870203,-48.8529085589551)) ;
#67896 = CARTESIAN_POINT('Ctrl Pts',(27.922444913608,535.709936033526,-48.7416863130977)) ;
#67897 = CARTESIAN_POINT('Ctrl Pts',(28.8240110099946,534.0575733704,-48.6304640672403)) ;
#67898 = CARTESIAN_POINT('Ctrl Pts',(30.7013164038052,533.92033530544,-48.519241821383)) ;
#67899 = CARTESIAN_POINT('Ctrl Pts',(31.8336287497696,535.423982591803,-48.4080195755257)) ;
#67900 = CARTESIAN_POINT('Ctrl Pts',(31.1830993569614,537.190305869038,-48.2967973296683)) ;
#67901 = CARTESIAN_POINT('Ctrl Pts',(29.3459856170836,537.600333837421,-48.1855750838108)) ;
#67902 = CARTESIAN_POINT('Ctrl Pts',(28.0061713207052,536.278206215794,-48.0743528379535)) ;
#67903 = CARTESIAN_POINT('Ctrl Pts',(28.3916956359744,534.435855981822,-47.9631305920961)) ;
#67904 = CARTESIAN_POINT('Ctrl Pts',(30.1492588407991,533.761763155306,-47.8519083462388)) ;
#67905 = CARTESIAN_POINT('Ctrl Pts',(31.6678491066124,534.874247564052,-47.7406861003814)) ;
#67906 = CARTESIAN_POINT('Ctrl Pts',(31.5558742796478,536.752700386808,-47.6294638545241)) ;
#67907 = CARTESIAN_POINT('Ctrl Pts',(29.9156968899049,537.677602163744,-47.5182416086666)) ;
#67908 = CARTESIAN_POINT('Ctrl Pts',(28.2520400432131,536.796558566173,-47.4070036656182)) ;
#67909 = CARTESIAN_POINT('Ctrl Pts',(28.1434047061733,535.55083948989,-47.3328398045222)) ;
#67910 = CARTESIAN_POINT('Ctrl Pts',(28.3654110025038,535.043772234511,-47.2957500253787)) ;
#67911 = CARTESIAN_POINT('Ctrl Pts',(28.52086835799,536.874678815716,-49.5972643150057)) ;
#67912 = CARTESIAN_POINT('Ctrl Pts',(28.1333130675147,536.419389040585,-49.5601759866023)) ;
#67913 = CARTESIAN_POINT('Ctrl Pts',(27.8576138890395,535.097142357075,-49.4860135762466)) ;
#67914 = CARTESIAN_POINT('Ctrl Pts',(29.3038209507092,533.667612757949,-49.3747770839385)) ;
#67915 = CARTESIAN_POINT('Ctrl Pts',(31.2883836512653,534.113251822979,-49.2635548380812)) ;
#67916 = CARTESIAN_POINT('Ctrl Pts',(31.9894083942532,536.021233699266,-49.1523325922239)) ;
#67917 = CARTESIAN_POINT('Ctrl Pts',(30.7653261945102,537.644965214308,-49.0411103463664)) ;
#67918 = CARTESIAN_POINT('Ctrl Pts',(28.7374890571207,537.495305712007,-48.929888100509)) ;
#67919 = CARTESIAN_POINT('Ctrl Pts',(27.764781958215,535.709885582938,-48.8186658546515)) ;
#67920 = CARTESIAN_POINT('Ctrl Pts',(28.7386459159201,533.925017619152,-48.7074436087942)) ;
#67921 = CARTESIAN_POINT('Ctrl Pts',(30.7664950863416,533.77677423952,-48.5962213629369)) ;
#67922 = CARTESIAN_POINT('Ctrl Pts',(31.9896091619694,535.401001129993,-48.4849991170796)) ;
#67923 = CARTESIAN_POINT('Ctrl Pts',(31.2869128964124,537.308968370831,-48.3737768712222)) ;
#67924 = CARTESIAN_POINT('Ctrl Pts',(29.3024784055384,537.75187706234,-48.2625546253647)) ;
#67925 = CARTESIAN_POINT('Ctrl Pts',(27.8552225044011,536.323726155436,-48.1513323795073)) ;
#67926 = CARTESIAN_POINT('Ctrl Pts',(28.2716625601711,534.333635248594,-48.04011013365)) ;
#67927 = CARTESIAN_POINT('Ctrl Pts',(30.1701672459924,533.60548596423,-47.9288878877926)) ;
#67928 = CARTESIAN_POINT('Ctrl Pts',(31.810535414588,534.80718207229,-47.8176656419354)) ;
#67929 = CARTESIAN_POINT('Ctrl Pts',(31.6895811677632,536.836270685608,-47.706443396078)) ;
#67930 = CARTESIAN_POINT('Ctrl Pts',(29.9178756316795,537.835341645114,-47.5952211502205)) ;
#67931 = CARTESIAN_POINT('Ctrl Pts',(28.120807787762,536.883645914451,-47.4839832071721)) ;
#67932 = CARTESIAN_POINT('Ctrl Pts',(28.0034608292857,535.538030862288,-47.409819346076)) ;
#67933 = CARTESIAN_POINT('Ctrl Pts',(28.24327012474,534.990301166012,-47.3727295669326)) ;
#67934 = CARTESIAN_POINT('Ctrl Pts',(28.419335860289,536.961100463147,-49.6742438565595)) ;
#67935 = CARTESIAN_POINT('Ctrl Pts',(28.0030091809332,536.472010816113,-49.6371555281562)) ;
#67936 = CARTESIAN_POINT('Ctrl Pts',(27.7068426047137,535.051602981246,-49.5629931178004)) ;
#67937 = CARTESIAN_POINT('Ctrl Pts',(29.2604134072377,533.515947745279,-49.4517566254923)) ;
#67938 = CARTESIAN_POINT('Ctrl Pts',(31.3923063768398,533.994670231322,-49.340534379635)) ;
#67939 = CARTESIAN_POINT('Ctrl Pts',(32.1453739018286,536.044297157719,-49.2293121337776)) ;
#67940 = CARTESIAN_POINT('Ctrl Pts',(30.8304181006761,537.788571501115,-49.1180898879202)) ;
#67941 = CARTESIAN_POINT('Ctrl Pts',(28.652038079986,537.62780155381,-49.0068676420627)) ;
#67942 = CARTESIAN_POINT('Ctrl Pts',(27.6071190028218,535.709835132352,-48.8956453962053)) ;
#67943 = CARTESIAN_POINT('Ctrl Pts',(28.6532808218456,533.792461867905,-48.784423150348)) ;
#67944 = CARTESIAN_POINT('Ctrl Pts',(30.8316737688779,533.633213173601,-48.6732009044907)) ;
#67945 = CARTESIAN_POINT('Ctrl Pts',(32.1455895741691,535.378019668185,-48.5619786586334)) ;
#67946 = CARTESIAN_POINT('Ctrl Pts',(31.3907264358632,537.427630872625,-48.450756412776)) ;
#67947 = CARTESIAN_POINT('Ctrl Pts',(29.2589711939935,537.903420287258,-48.3395341669185)) ;
#67948 = CARTESIAN_POINT('Ctrl Pts',(27.704273688097,536.369246095077,-48.2283119210611)) ;
#67949 = CARTESIAN_POINT('Ctrl Pts',(28.151629484368,534.231414515366,-48.1170896752037)) ;
#67950 = CARTESIAN_POINT('Ctrl Pts',(30.1910756511857,533.449208773154,-48.0058674293464)) ;
#67951 = CARTESIAN_POINT('Ctrl Pts',(31.9532217225635,534.740116580527,-47.8946451834892)) ;
#67952 = CARTESIAN_POINT('Ctrl Pts',(31.8232880558788,536.919840984407,-47.7834229376318)) ;
#67953 = CARTESIAN_POINT('Ctrl Pts',(29.9200543734541,537.993081126484,-47.6722006917743)) ;
#67954 = CARTESIAN_POINT('Ctrl Pts',(27.989575532311,536.97073326273,-47.5609627487258)) ;
#67955 = CARTESIAN_POINT('Ctrl Pts',(27.8635169523983,535.525222234686,-47.4867988876299)) ;
#67956 = CARTESIAN_POINT('Ctrl Pts',(28.1211292469763,534.936830097514,-47.4497091084864)) ;
#67957 = CARTESIAN_POINT('Ctrl Pts',(28.3178033625881,537.047522110579,-49.7512233981133)) ;
#67958 = CARTESIAN_POINT('Ctrl Pts',(27.8727052943514,536.524632591642,-49.71413506971)) ;
#67959 = CARTESIAN_POINT('Ctrl Pts',(27.5560713203878,535.006063605417,-49.6399726593542)) ;
#67960 = CARTESIAN_POINT('Ctrl Pts',(29.2170058637665,533.364282732609,-49.5287361670461)) ;
#67961 = CARTESIAN_POINT('Ctrl Pts',(31.4962291024142,533.876088639664,-49.4175139211888)) ;
#67962 = CARTESIAN_POINT('Ctrl Pts',(32.3013394094041,536.067360616172,-49.3062916753315)) ;
#67963 = CARTESIAN_POINT('Ctrl Pts',(30.8955100068421,537.932177787921,-49.195069429474)) ;
#67964 = CARTESIAN_POINT('Ctrl Pts',(28.5665871028512,537.760297395612,-49.0838471836165)) ;
#67965 = CARTESIAN_POINT('Ctrl Pts',(27.4494560474289,535.709784681764,-48.9726249377591)) ;
#67966 = CARTESIAN_POINT('Ctrl Pts',(28.5679157277713,533.659906116657,-48.8614026919018)) ;
#67967 = CARTESIAN_POINT('Ctrl Pts',(30.8968524514142,533.489652107681,-48.7501804460445)) ;
#67968 = CARTESIAN_POINT('Ctrl Pts',(32.3015699863689,535.355038206375,-48.6389582001872)) ;
#67969 = CARTESIAN_POINT('Ctrl Pts',(31.4945399753143,537.546293374418,-48.5277359543298)) ;
#67970 = CARTESIAN_POINT('Ctrl Pts',(29.2154639824486,538.054963512177,-48.4165137084723)) ;
#67971 = CARTESIAN_POINT('Ctrl Pts',(27.553324871793,536.414766034718,-48.305291462615)) ;
#67972 = CARTESIAN_POINT('Ctrl Pts',(28.0315964085647,534.129193782138,-48.1940692167575)) ;
#67973 = CARTESIAN_POINT('Ctrl Pts',(30.2119840563792,533.292931582077,-48.0828469709002)) ;
#67974 = CARTESIAN_POINT('Ctrl Pts',(32.0959080305391,534.673051088765,-47.971624725043)) ;
#67975 = CARTESIAN_POINT('Ctrl Pts',(31.9569949439941,537.003411283205,-47.8604024791856)) ;
#67976 = CARTESIAN_POINT('Ctrl Pts',(29.9222331152288,538.150820607853,-47.7491802333281)) ;
#67977 = CARTESIAN_POINT('Ctrl Pts',(27.8583432768598,537.057820611007,-47.6379422902796)) ;
#67978 = CARTESIAN_POINT('Ctrl Pts',(27.723573075511,535.512413607084,-47.5637784291836)) ;
#67979 = CARTESIAN_POINT('Ctrl Pts',(27.9989883692128,534.883359029015,-47.5266886500402)) ;
#67980 = CARTESIAN_POINT('',(29.9416619236741,537.377495804614,-47.5212987075501)) ;
#67981 = CARTESIAN_POINT('Ctrl Pts',(28.0059001157431,534.88733298046,-47.522160171753)) ;
#67982 = CARTESIAN_POINT('Ctrl Pts',(27.9829859323478,534.956807320503,-47.5221601717529)) ;
#67983 = CARTESIAN_POINT('Ctrl Pts',(27.9641822315392,535.027382072257,-47.5221601717529)) ;
#67984 = CARTESIAN_POINT('Ctrl Pts',(27.9493741439311,535.098725327386,-47.5221601717529)) ;
#67985 = CARTESIAN_POINT('Ctrl Pts',(27.934145219614,535.172096113787,-47.5221601717529)) ;
#67986 = CARTESIAN_POINT('Ctrl Pts',(27.9231422999915,535.246280738549,-47.5221601717529)) ;
#67987 = CARTESIAN_POINT('Ctrl Pts',(27.9162948670505,535.320921706951,-47.5221601717529)) ;
#67988 = CARTESIAN_POINT('Ctrl Pts',(27.9104995242757,535.384094285734,-47.5221601717529)) ;
#67989 = CARTESIAN_POINT('Ctrl Pts',(27.9076818396783,535.447594149968,-47.5221601717529)) ;
#67990 = CARTESIAN_POINT('Ctrl Pts',(27.9078274713952,535.511198010894,-47.5221601717529)) ;
#67991 = CARTESIAN_POINT('Ctrl Pts',(27.9078920377234,535.539397003841,-47.5221601717529)) ;
#67992 = CARTESIAN_POINT('Ctrl Pts',(27.9085394098575,535.567616312829,-47.5221601717528)) ;
#67993 = CARTESIAN_POINT('Ctrl Pts',(27.9097698678232,535.595835716945,-47.5221601717528)) ;
#67994 = CARTESIAN_POINT('Ctrl Pts',(27.9104441820957,535.611300484931,-47.5221601717528)) ;
#67995 = CARTESIAN_POINT('Ctrl Pts',(27.9112936275329,535.62676527183,-47.5221601717528)) ;
#67996 = CARTESIAN_POINT('Ctrl Pts',(27.912318364823,535.642226671488,-47.5221601717528)) ;
#67997 = CARTESIAN_POINT('Ctrl Pts',(27.9132705988578,535.656594130466,-47.5221601717529)) ;
#67998 = CARTESIAN_POINT('Ctrl Pts',(27.9143744996085,535.670960840443,-47.5221601717528)) ;
#67999 = CARTESIAN_POINT('Ctrl Pts',(27.9156279765185,535.685301740957,-47.5221601717528)) ;
#68000 = CARTESIAN_POINT('Ctrl Pts',(27.9220008875486,535.758213561142,-47.5221601717528)) ;
#68001 = CARTESIAN_POINT('Ctrl Pts',(27.9322429746534,535.830584659191,-47.5221601717528)) ;
#68002 = CARTESIAN_POINT('Ctrl Pts',(27.9462848097153,535.902081453107,-47.5221601717528)) ;
#68003 = CARTESIAN_POINT('Ctrl Pts',(27.9601366899147,535.97261105409,-47.5221601717528)) ;
#68004 = CARTESIAN_POINT('Ctrl Pts',(27.9776866254573,536.042290755737,-47.5221601717529)) ;
#68005 = CARTESIAN_POINT('Ctrl Pts',(27.9989137274389,536.110780927498,-47.5221601717528)) ;
#68006 = CARTESIAN_POINT('Ctrl Pts',(28.0168750590771,536.168733948594,-47.5221601717528)) ;
#68007 = CARTESIAN_POINT('Ctrl Pts',(28.0374699981699,536.225835262571,-47.5221601717528)) ;
#68008 = CARTESIAN_POINT('Ctrl Pts',(28.0607089111533,536.281860922513,-47.5221601717528)) ;
#68009 = CARTESIAN_POINT('Ctrl Pts',(28.0702708712446,536.30491342608,-47.5221601717528)) ;
#68010 = CARTESIAN_POINT('Ctrl Pts',(28.0802806969461,536.327783586327,-47.5221601717528)) ;
#68011 = CARTESIAN_POINT('Ctrl Pts',(28.0907400669133,536.350454728169,-47.5221601717528)) ;
#68012 = CARTESIAN_POINT('Ctrl Pts',(28.0956199427452,536.361032072454,-47.5221601717528)) ;
#68013 = CARTESIAN_POINT('Ctrl Pts',(28.100597680306,536.371566085872,-47.5221601717528)) ;
#68014 = CARTESIAN_POINT('Ctrl Pts',(28.1056734895392,536.382055021761,-47.5221601717528)) ;
#68015 = CARTESIAN_POINT('Ctrl Pts',(28.1109059706895,536.392867713255,-47.5221601717529)) ;
#68016 = CARTESIAN_POINT('Ctrl Pts',(28.1162389961769,536.403624848622,-47.5221601717528)) ;
#68017 = CARTESIAN_POINT('Ctrl Pts',(28.1216705430934,536.414321233288,-47.5221601717528)) ;
#68018 = CARTESIAN_POINT('Ctrl Pts',(28.1528227355498,536.475669471426,-47.5221601717529)) ;
#68019 = CARTESIAN_POINT('Ctrl Pts',(28.1872313289458,536.535060558472,-47.5221601717528)) ;
#68020 = CARTESIAN_POINT('Ctrl Pts',(28.2248730925408,536.592190626077,-47.5221601717528)) ;
#68021 = CARTESIAN_POINT('Ctrl Pts',(28.2592299129734,536.64433503395,-47.5221601717528)) ;
#68022 = CARTESIAN_POINT('Ctrl Pts',(28.2962808697179,536.694595995804,-47.5221601717528)) ;
#68023 = CARTESIAN_POINT('Ctrl Pts',(28.3360355478087,536.742716006994,-47.5221601717528)) ;
#68024 = CARTESIAN_POINT('Ctrl Pts',(28.3827611865145,536.799273835288,-47.5221601717527)) ;
#68025 = CARTESIAN_POINT('Ctrl Pts',(28.4332227235773,536.852875425638,-47.5221601717527)) ;
#68026 = CARTESIAN_POINT('Ctrl Pts',(28.4870438712866,536.903316651351,-47.5221601717528)) ;
#68027 = CARTESIAN_POINT('Ctrl Pts',(28.4989832996611,536.914506293846,-47.5221601717528)) ;
#68028 = CARTESIAN_POINT('Ctrl Pts',(28.5110881336462,536.925540181673,-47.522160171753)) ;
#68029 = CARTESIAN_POINT('Ctrl Pts',(28.5233543686585,536.936415683673,-47.5221601717529)) ;
#68030 = CARTESIAN_POINT('Ctrl Pts',(28.5353619424006,536.947061851149,-47.5221601717527)) ;
#68031 = CARTESIAN_POINT('Ctrl Pts',(28.5475283255332,536.957559542949,-47.5221601717527)) ;
#68032 = CARTESIAN_POINT('Ctrl Pts',(28.5598256460145,536.967886419756,-47.5221601717527)) ;
#68033 = CARTESIAN_POINT('Ctrl Pts',(28.6123312906609,537.011978897036,-47.5221601717529)) ;
#68034 = CARTESIAN_POINT('Ctrl Pts',(28.667290106961,537.053025157918,-47.5221601717527)) ;
#68035 = CARTESIAN_POINT('Ctrl Pts',(28.7243641711787,537.090910157219,-47.5221601717528)) ;
#68036 = CARTESIAN_POINT('Ctrl Pts',(28.7814313798004,537.128790605868,-47.5221601717528)) ;
#68037 = CARTESIAN_POINT('Ctrl Pts',(28.8406144442193,537.163510862665,-47.5221601717531)) ;
#68038 = CARTESIAN_POINT('Ctrl Pts',(28.9015947041635,537.194907734422,-47.5221601717529)) ;
#68039 = CARTESIAN_POINT('Ctrl Pts',(28.9461752574605,537.217860898545,-47.5221601717528)) ;
#68040 = CARTESIAN_POINT('Ctrl Pts',(28.9917167912542,537.239036876612,-47.5221601717527)) ;
#68041 = CARTESIAN_POINT('Ctrl Pts',(29.0380961522282,537.258354169963,-47.522160171753)) ;
#68042 = CARTESIAN_POINT('Ctrl Pts',(29.057274895643,537.266342236311,-47.522160171753)) ;
#68043 = CARTESIAN_POINT('Ctrl Pts',(29.0765968955737,537.2740122878,-47.5221601717531)) ;
#68044 = CARTESIAN_POINT('Ctrl Pts',(29.0960533438445,537.281357768422,-47.522160171753)) ;
#68045 = CARTESIAN_POINT('Ctrl Pts',(29.110489377956,537.286807869456,-47.5221601717529)) ;
#68046 = CARTESIAN_POINT('Ctrl Pts',(29.1249994264623,537.292079279947,-47.5221601717527)) ;
#68047 = CARTESIAN_POINT('Ctrl Pts',(29.1395798514287,537.297169151436,-47.5221601717527)) ;
#68048 = CARTESIAN_POINT('Ctrl Pts',(29.1518554570994,537.301454434989,-47.5221601717527)) ;
#68049 = CARTESIAN_POINT('Ctrl Pts',(29.164172997307,537.30560823222,-47.5221601717528)) ;
#68050 = CARTESIAN_POINT('Ctrl Pts',(29.1765267084414,537.309628247203,-47.5221601717528)) ;
#68051 = CARTESIAN_POINT('Ctrl Pts',(29.239143774932,537.330004435599,-47.5221601717528)) ;
#68052 = CARTESIAN_POINT('Ctrl Pts',(29.3027194030454,537.346957735481,-47.5221601717529)) ;
#68053 = CARTESIAN_POINT('Ctrl Pts',(29.3669625745666,537.360320290012,-47.5221601717529)) ;
#68054 = CARTESIAN_POINT('Ctrl Pts',(29.4124482306339,537.36978128867,-47.5221601717529)) ;
#68055 = CARTESIAN_POINT('Ctrl Pts',(29.4582686497801,537.37744126027,-47.5221601717528)) ;
#68056 = CARTESIAN_POINT('Ctrl Pts',(29.5043181131541,537.383225073432,-47.5221601717529)) ;
#68057 = CARTESIAN_POINT('Ctrl Pts',(29.5190280710151,537.385072644319,-47.5221601717529)) ;
#68058 = CARTESIAN_POINT('Ctrl Pts',(29.5337636188551,537.38672888721,-47.5221601717531)) ;
#68059 = CARTESIAN_POINT('Ctrl Pts',(29.5485139882223,537.388190360635,-47.522160171753)) ;
#68060 = CARTESIAN_POINT('Ctrl Pts',(29.6112650202864,537.39440776194,-47.5221601717527)) ;
#68061 = CARTESIAN_POINT('Ctrl Pts',(29.674168396674,537.397093581716,-47.522160171753)) ;
#68062 = CARTESIAN_POINT('Ctrl Pts',(29.7369575657226,537.396079059198,-47.522160171753)) ;
#68063 = CARTESIAN_POINT('Ctrl Pts',(29.7954524273515,537.395133922397,-47.5221601717529)) ;
#68064 = CARTESIAN_POINT('Ctrl Pts',(29.8538486482669,537.390976944829,-47.5221601717529)) ;
#68065 = CARTESIAN_POINT('Ctrl Pts',(29.9119178667258,537.383432974238,-47.5221601717531)) ;
#68066 = CARTESIAN_POINT('Ctrl Pts',(29.921832697167,537.382144904737,-47.5221601717531)) ;
#68067 = CARTESIAN_POINT('Ctrl Pts',(29.9317379531658,537.380758003776,-47.5221601717528)) ;
#68068 = CARTESIAN_POINT('Ctrl Pts',(29.941632460783,537.379272913244,-47.5221601717531)) ;
#68069 = CARTESIAN_POINT('Ctrl Pts',(28.6194567455546,536.789923813611,-49.5221601717528)) ;
#68070 = CARTESIAN_POINT('Ctrl Pts',(28.5741835241712,536.747688703051,-49.5221601717528)) ;
#68071 = CARTESIAN_POINT('Ctrl Pts',(28.5316436333847,536.702879617092,-49.5221601717529)) ;
#68072 = CARTESIAN_POINT('Ctrl Pts',(28.4918334298705,536.655842595265,-49.5221601717528)) ;
#68073 = CARTESIAN_POINT('Ctrl Pts',(28.4492968452567,536.605584267442,-49.5221601717527)) ;
#68074 = CARTESIAN_POINT('Ctrl Pts',(28.4098758983343,536.552782180805,-49.522160171753)) ;
#68075 = CARTESIAN_POINT('Ctrl Pts',(28.3735952737005,536.497803325823,-49.522160171753)) ;
#68076 = CARTESIAN_POINT('Ctrl Pts',(28.341849727146,536.449696827713,-49.522160171753)) ;
#68077 = CARTESIAN_POINT('Ctrl Pts',(28.3125087393969,536.399922503953,-49.5221601717529)) ;
#68078 = CARTESIAN_POINT('Ctrl Pts',(28.2856119276886,536.348698435406,-49.522160171753)) ;
#68079 = CARTESIAN_POINT('Ctrl Pts',(28.2720945912425,536.322955125151,-49.522160171753)) ;
#68080 = CARTESIAN_POINT('Ctrl Pts',(28.2591949428059,536.296845294405,-49.5221601717529)) ;
#68081 = CARTESIAN_POINT('Ctrl Pts',(28.2469203815683,536.270394759938,-49.5221601717529)) ;
#68082 = CARTESIAN_POINT('Ctrl Pts',(28.2413692702196,536.258432632802,-49.5221601717529)) ;
#68083 = CARTESIAN_POINT('Ctrl Pts',(28.2359455138467,536.246399331703,-49.522160171753)) ;
#68084 = CARTESIAN_POINT('Ctrl Pts',(28.2306580911855,536.234316773402,-49.522160171753)) ;
#68085 = CARTESIAN_POINT('Ctrl Pts',(28.203570951268,536.172418573045,-49.522160171753)) ;
#68086 = CARTESIAN_POINT('Ctrl Pts',(28.1800053268915,536.109118453109,-49.5221601717528)) ;
#68087 = CARTESIAN_POINT('Ctrl Pts',(28.1599830712663,536.044785442915,-49.5221601717528)) ;
#68088 = CARTESIAN_POINT('Ctrl Pts',(28.139960815641,535.98045243272,-49.5221601717528)) ;
#68089 = CARTESIAN_POINT('Ctrl Pts',(28.1234814998453,535.915085598446,-49.5221601717529)) ;
#68090 = CARTESIAN_POINT('Ctrl Pts',(28.1106053005632,535.849018425769,-49.5221601717529)) ;
#68091 = CARTESIAN_POINT('Ctrl Pts',(28.0997084494549,535.793107195442,-49.5221601717529)) ;
#68092 = CARTESIAN_POINT('Ctrl Pts',(28.0913926099977,535.73669347859,-49.5221601717529)) ;
#68093 = CARTESIAN_POINT('Ctrl Pts',(28.0857191798105,535.679967078133,-49.5221601717529)) ;
#68094 = CARTESIAN_POINT('Ctrl Pts',(28.0830976380087,535.65375531115,-49.5221601717529)) ;
#68095 = CARTESIAN_POINT('Ctrl Pts',(28.0810406218419,535.627476667704,-49.5221601717529)) ;
#68096 = CARTESIAN_POINT('Ctrl Pts',(28.0795560257393,535.60114946616,-49.5221601717529)) ;
#68097 = CARTESIAN_POINT('Ctrl Pts',(28.0789167406597,535.589812654008,-49.5221601717529)) ;
#68098 = CARTESIAN_POINT('Ctrl Pts',(28.0783837314708,535.578467436334,-49.5221601717529)) ;
#68099 = CARTESIAN_POINT('Ctrl Pts',(28.0779579170341,535.567128747108,-49.5221601717529)) ;
#68100 = CARTESIAN_POINT('Ctrl Pts',(28.0753221846355,535.496943830925,-49.5221601717529)) ;
#68101 = CARTESIAN_POINT('Ctrl Pts',(28.0767816822343,535.426878372279,-49.5221601717529)) ;
#68102 = CARTESIAN_POINT('Ctrl Pts',(28.0823886751965,535.357295690998,-49.5221601717529)) ;
#68103 = CARTESIAN_POINT('Ctrl Pts',(28.0874298054729,535.294735355418,-49.5221601717529)) ;
#68104 = CARTESIAN_POINT('Ctrl Pts',(28.0958238609977,535.232564296308,-49.5221601717529)) ;
#68105 = CARTESIAN_POINT('Ctrl Pts',(28.107642624543,535.171034219996,-49.5221601717529)) ;
#68106 = CARTESIAN_POINT('Ctrl Pts',(28.1204534679983,535.10433924193,-49.5221601717529)) ;
#68107 = CARTESIAN_POINT('Ctrl Pts',(28.1372870528362,535.038396522335,-49.522160171753)) ;
#68108 = CARTESIAN_POINT('Ctrl Pts',(28.1578992251687,534.973418262404,-49.522160171753)) ;
#68109 = CARTESIAN_POINT('Ctrl Pts',(28.165767691918,534.948613536855,-49.5221601717529)) ;
#68110 = CARTESIAN_POINT('Ctrl Pts',(28.1741873351911,534.92394940569,-49.5221601717529)) ;
#68111 = CARTESIAN_POINT('Ctrl Pts',(28.1831465099758,534.899437990031,-49.5221601717529)) ;
#68112 = CARTESIAN_POINT('Ctrl Pts',(28.1870922543454,534.888642823885,-49.5221601717529)) ;
#68113 = CARTESIAN_POINT('Ctrl Pts',(28.1911423844193,534.877878274877,-49.5221601717529)) ;
#68114 = CARTESIAN_POINT('Ctrl Pts',(28.1952910524112,534.867157270828,-49.5221601717529)) ;
#68115 = CARTESIAN_POINT('Ctrl Pts',(28.2205415246478,534.801904901726,-49.522160171753)) ;
#68116 = CARTESIAN_POINT('Ctrl Pts',(28.2494802213268,534.738147870322,-49.522160171753)) ;
#68117 = CARTESIAN_POINT('Ctrl Pts',(28.2817953527524,534.676103380191,-49.522160171753)) ;
#68118 = CARTESIAN_POINT('Ctrl Pts',(28.3148512464585,534.612636639368,-49.5221601717529)) ;
#68119 = CARTESIAN_POINT('Ctrl Pts',(28.3514404488416,534.550961035581,-49.522160171753)) ;
#68120 = CARTESIAN_POINT('Ctrl Pts',(28.3912853225522,534.491312947336,-49.522160171753)) ;
#68121 = CARTESIAN_POINT('Ctrl Pts',(28.421395761063,534.446237384883,-49.522160171753)) ;
#68122 = CARTESIAN_POINT('Ctrl Pts',(28.4533666306937,534.402319663736,-49.5221601717529)) ;
#68123 = CARTESIAN_POINT('Ctrl Pts',(28.4870968158936,534.359667673985,-49.522160171753)) ;
#68124 = CARTESIAN_POINT('Ctrl Pts',(28.5079985866382,534.333237279183,-49.522160171753)) ;
#68125 = CARTESIAN_POINT('Ctrl Pts',(28.5295762366623,534.307293039875,-49.5221601717528)) ;
#68126 = CARTESIAN_POINT('Ctrl Pts',(28.5518084276599,534.281862208131,-49.5221601717529)) ;
#68127 = CARTESIAN_POINT('Ctrl Pts',(28.5603078651189,534.272139920122,-49.5221601717529)) ;
#68128 = CARTESIAN_POINT('Ctrl Pts',(28.5689045301256,534.262490991216,-49.522160171753)) ;
#68129 = CARTESIAN_POINT('Ctrl Pts',(28.5775922730039,534.252922526196,-49.522160171753)) ;
#68130 = CARTESIAN_POINT('Ctrl Pts',(28.6291688757767,534.196117332211,-49.522160171753)) ;
#68131 = CARTESIAN_POINT('Ctrl Pts',(28.683825070941,534.142282619883,-49.5221601717529)) ;
#68132 = CARTESIAN_POINT('Ctrl Pts',(28.7412498653522,534.091699428638,-49.5221601717528)) ;
#68133 = CARTESIAN_POINT('Ctrl Pts',(28.7843184611605,534.053762035204,-49.5221601717528)) ;
#68134 = CARTESIAN_POINT('Ctrl Pts',(28.8289456970457,534.017653807843,-49.5221601717529)) ;
#68135 = CARTESIAN_POINT('Ctrl Pts',(28.87501898973,533.983503817113,-49.5221601717528)) ;
#68136 = CARTESIAN_POINT('Ctrl Pts',(28.8913736012136,533.971381613597,-49.5221601717528)) ;
#68137 = CARTESIAN_POINT('Ctrl Pts',(28.9079105525739,533.959506258588,-49.5221601717527)) ;
#68138 = CARTESIAN_POINT('Ctrl Pts',(28.9246252217011,533.947883902412,-49.5221601717529)) ;
#68139 = CARTESIAN_POINT('Ctrl Pts',(28.9372829380326,533.939082502488,-49.5221601717531)) ;
#68140 = CARTESIAN_POINT('Ctrl Pts',(28.9500384200079,533.930429161134,-49.522160171753)) ;
#68141 = CARTESIAN_POINT('Ctrl Pts',(28.9628827037222,533.921930640592,-49.522160171753)) ;
#68142 = CARTESIAN_POINT('Ctrl Pts',(29.0256895766991,533.880373983011,-49.522160171753)) ;
#68143 = CARTESIAN_POINT('Ctrl Pts',(29.0906640066724,533.842483570269,-49.5221601717531)) ;
#68144 = CARTESIAN_POINT('Ctrl Pts',(29.1575446499793,533.808535771635,-49.522160171753)) ;
#68145 = CARTESIAN_POINT('Ctrl Pts',(29.2115680980119,533.781114128471,-49.522160171753)) ;
#68146 = CARTESIAN_POINT('Ctrl Pts',(29.2668362837646,533.756265219817,-49.522160171753)) ;
#68147 = CARTESIAN_POINT('Ctrl Pts',(29.3232283120257,533.734153036032,-49.5221601717528)) ;
#68148 = CARTESIAN_POINT('Ctrl Pts',(29.3337310402553,533.730034754353,-49.5221601717528)) ;
#68149 = CARTESIAN_POINT('Ctrl Pts',(29.3442727870821,533.726011456111,-49.5221601717526)) ;
#68150 = CARTESIAN_POINT('Ctrl Pts',(29.3548523877517,533.722082788819,-49.5221601717526)) ;
#68151 = CARTESIAN_POINT('Ctrl Pts',(29.9416053009762,537.375719435804,-47.5212987075501)) ;
#68152 = CARTESIAN_POINT('Ctrl Pts',(29.9491437898387,537.375479142474,-47.5215858622844)) ;
#68153 = CARTESIAN_POINT('Ctrl Pts',(29.9566806468873,537.37518765597,-47.5218730170187)) ;
#68154 = CARTESIAN_POINT('Ctrl Pts',(29.9642151770171,537.374845003176,-47.522160171753)) ;
#68155 = CARTESIAN_POINT('Ctrl Pts',(30.4192300785532,583.719768248152,-49.5189951107294)) ;
#68156 = CARTESIAN_POINT('Ctrl Pts',(31.0820332975824,583.896429840045,-49.4819041482875)) ;
#68157 = CARTESIAN_POINT('Ctrl Pts',(32.2050033717352,584.964207263547,-49.4077391038933)) ;
#68158 = CARTESIAN_POINT('Ctrl Pts',(31.7732242756362,587.256677742684,-49.2964999775465)) ;
#68159 = CARTESIAN_POINT('Ctrl Pts',(29.6099548125204,588.131120449431,-49.185277731689)) ;
#68160 = CARTESIAN_POINT('Ctrl Pts',(27.7035655963549,586.788278335697,-49.0740554858316)) ;
#68161 = CARTESIAN_POINT('Ctrl Pts',(27.7990464989561,584.45752039736,-48.9628332399742)) ;
#68162 = CARTESIAN_POINT('Ctrl Pts',(29.8100268470855,583.275562917911,-48.8516109941169)) ;
#68163 = CARTESIAN_POINT('Ctrl Pts',(31.8927897096346,584.325470257128,-48.7403887482596)) ;
#68164 = CARTESIAN_POINT('Ctrl Pts',(32.1385417975513,586.644990498722,-48.6291665024023)) ;
#68165 = CARTESIAN_POINT('Ctrl Pts',(30.3219322734697,588.10802924709,-48.5179442565448)) ;
#68166 = CARTESIAN_POINT('Ctrl Pts',(28.1080818049476,587.373600016883,-48.4067220106873)) ;
#68167 = CARTESIAN_POINT('Ctrl Pts',(27.5261524671424,585.114866204111,-48.2954997648299)) ;
#68168 = CARTESIAN_POINT('Ctrl Pts',(29.1095299162611,583.402129097654,-48.1842775189726)) ;
#68169 = CARTESIAN_POINT('Ctrl Pts',(31.4069240173951,583.805302241545,-48.0730552731154)) ;
#68170 = CARTESIAN_POINT('Ctrl Pts',(32.312527681685,585.954741369732,-47.961833027258)) ;
#68171 = CARTESIAN_POINT('Ctrl Pts',(30.9963393282325,587.880543452508,-47.8506107814006)) ;
#68172 = CARTESIAN_POINT('Ctrl Pts',(28.66449088512,587.817045356221,-47.7393885355431)) ;
#68173 = CARTESIAN_POINT('Ctrl Pts',(27.4546192595412,585.823617294928,-47.6281662896857)) ;
#68174 = CARTESIAN_POINT('Ctrl Pts',(28.4743800506003,583.724933720291,-47.5169440438284)) ;
#68175 = CARTESIAN_POINT('Ctrl Pts',(30.7908823865385,583.450313172167,-47.4057075193723)) ;
#68176 = CARTESIAN_POINT('Ctrl Pts',(31.7796747638363,584.643315655865,-47.3315450768686)) ;
#68177 = CARTESIAN_POINT('Ctrl Pts',(31.9108216721039,585.31655469127,-47.2944567163174)) ;
#68178 = CARTESIAN_POINT('Ctrl Pts',(30.3850875462748,583.847845379583,-49.5955228059578)) ;
#68179 = CARTESIAN_POINT('Ctrl Pts',(31.0052495825354,584.013141517883,-49.5584318435159)) ;
#68180 = CARTESIAN_POINT('Ctrl Pts',(32.0559738214225,585.012223903455,-49.4842667991217)) ;
#68181 = CARTESIAN_POINT('Ctrl Pts',(31.6519730625794,587.157209201643,-49.3730276727749)) ;
#68182 = CARTESIAN_POINT('Ctrl Pts',(29.6278766841831,587.975394982943,-49.2618054269174)) ;
#68183 = CARTESIAN_POINT('Ctrl Pts',(27.8441342637189,586.718944085118,-49.15058318106)) ;
#68184 = CARTESIAN_POINT('Ctrl Pts',(27.9334724402411,584.538134536265,-49.0393609352026)) ;
#68185 = CARTESIAN_POINT('Ctrl Pts',(29.8150771635899,583.432217823454,-48.9281386893453)) ;
#68186 = CARTESIAN_POINT('Ctrl Pts',(31.7638463017036,584.41457978954,-48.8169164434881)) ;
#68187 = CARTESIAN_POINT('Ctrl Pts',(31.9937880263092,586.584874614423,-48.7056941976306)) ;
#68188 = CARTESIAN_POINT('Ctrl Pts',(30.2940493569722,587.953789343964,-48.5944719517732)) ;
#68189 = CARTESIAN_POINT('Ctrl Pts',(28.2226260821331,587.266609327605,-48.4832497059157)) ;
#68190 = CARTESIAN_POINT('Ctrl Pts',(27.6781349379567,585.153190260705,-48.3720274600584)) ;
#68191 = CARTESIAN_POINT('Ctrl Pts',(29.1596464255638,583.550641418117,-48.260805214201)) ;
#68192 = CARTESIAN_POINT('Ctrl Pts',(31.3092385864758,583.927876577365,-48.1495829683438)) ;
#68193 = CARTESIAN_POINT('Ctrl Pts',(32.1565805974484,585.939032389956,-48.0383607224865)) ;
#68194 = CARTESIAN_POINT('Ctrl Pts',(30.9250687007873,587.740938757941,-47.927138476629)) ;
#68195 = CARTESIAN_POINT('Ctrl Pts',(28.7432388043513,587.681525786548,-47.8159162307715)) ;
#68196 = CARTESIAN_POINT('Ctrl Pts',(27.6112037909547,585.816344130607,-47.7046939849141)) ;
#68197 = CARTESIAN_POINT('Ctrl Pts',(28.5653586751273,583.852678533116,-47.5934717390568)) ;
#68198 = CARTESIAN_POINT('Ctrl Pts',(30.7328297501203,583.595725589265,-47.4822352146008)) ;
#68199 = CARTESIAN_POINT('Ctrl Pts',(31.658008561174,584.711976730347,-47.4080727720971)) ;
#68200 = CARTESIAN_POINT('Ctrl Pts',(31.7807181850044,585.34190319887,-47.3709844115459)) ;
#68201 = CARTESIAN_POINT('Ctrl Pts',(30.3509450139963,583.975922511015,-49.6720505011861)) ;
#68202 = CARTESIAN_POINT('Ctrl Pts',(30.9284658674885,584.12985319572,-49.6349595387444)) ;
#68203 = CARTESIAN_POINT('Ctrl Pts',(31.90694427111,585.060240543361,-49.56079449435)) ;
#68204 = CARTESIAN_POINT('Ctrl Pts',(31.5307218495225,587.0577406606,-49.4495553680033)) ;
#68205 = CARTESIAN_POINT('Ctrl Pts',(29.6457985558456,587.819669516452,-49.3383331221458)) ;
#68206 = CARTESIAN_POINT('Ctrl Pts',(27.9847029310828,586.649609834538,-49.2271108762884)) ;
#68207 = CARTESIAN_POINT('Ctrl Pts',(28.0678983815261,584.618748675169,-49.115888630431)) ;
#68208 = CARTESIAN_POINT('Ctrl Pts',(29.8201274800944,583.588872728996,-49.0046663845737)) ;
#68209 = CARTESIAN_POINT('Ctrl Pts',(31.6349028937727,584.503689321952,-48.8934441387164)) ;
#68210 = CARTESIAN_POINT('Ctrl Pts',(31.8490342550673,586.524758730124,-48.782221892859)) ;
#68211 = CARTESIAN_POINT('Ctrl Pts',(30.2661664404749,587.799549440838,-48.6709996470017)) ;
#68212 = CARTESIAN_POINT('Ctrl Pts',(28.3371703593188,587.159618638329,-48.5597774011441)) ;
#68213 = CARTESIAN_POINT('Ctrl Pts',(27.830117408771,585.191514317299,-48.4485551552867)) ;
#68214 = CARTESIAN_POINT('Ctrl Pts',(29.2097629348664,583.699153738578,-48.3373329094294)) ;
#68215 = CARTESIAN_POINT('Ctrl Pts',(31.2115531555567,584.050450913185,-48.2261106635721)) ;
#68216 = CARTESIAN_POINT('Ctrl Pts',(32.0006335132117,585.92332341018,-48.1148884177148)) ;
#68217 = CARTESIAN_POINT('Ctrl Pts',(30.8537980733421,587.601334063374,-48.0036661718574)) ;
#68218 = CARTESIAN_POINT('Ctrl Pts',(28.8219867235824,587.546006216873,-47.892443926)) ;
#68219 = CARTESIAN_POINT('Ctrl Pts',(27.7677883223683,585.809070966287,-47.7812216801425)) ;
#68220 = CARTESIAN_POINT('Ctrl Pts',(28.6563372996543,583.980423345943,-47.6699994342852)) ;
#68221 = CARTESIAN_POINT('Ctrl Pts',(30.6747771137021,583.741138006364,-47.5587629098291)) ;
#68222 = CARTESIAN_POINT('Ctrl Pts',(31.5363423585119,584.78063780483,-47.4846004673254)) ;
#68223 = CARTESIAN_POINT('Ctrl Pts',(31.6506146979047,585.367251706467,-47.4475121067741)) ;
#68224 = CARTESIAN_POINT('Ctrl Pts',(30.3168024817179,584.103999642447,-49.7485781964146)) ;
#68225 = CARTESIAN_POINT('Ctrl Pts',(30.8516821524416,584.246564873558,-49.7114872339728)) ;
#68226 = CARTESIAN_POINT('Ctrl Pts',(31.7579147207974,585.108257183268,-49.6373221895785)) ;
#68227 = CARTESIAN_POINT('Ctrl Pts',(31.4094706364656,586.958272119558,-49.5260830632317)) ;
#68228 = CARTESIAN_POINT('Ctrl Pts',(29.6637204275083,587.663944049963,-49.4148608173743)) ;
#68229 = CARTESIAN_POINT('Ctrl Pts',(28.1252715984466,586.580275583958,-49.3036385715168)) ;
#68230 = CARTESIAN_POINT('Ctrl Pts',(28.2023243228111,584.699362814073,-49.1924163256595)) ;
#68231 = CARTESIAN_POINT('Ctrl Pts',(29.8251777965987,583.745527634539,-49.0811940798022)) ;
#68232 = CARTESIAN_POINT('Ctrl Pts',(31.5059594858419,584.592798854365,-48.9699718339449)) ;
#68233 = CARTESIAN_POINT('Ctrl Pts',(31.7042804838254,586.464642845826,-48.8587495880875)) ;
#68234 = CARTESIAN_POINT('Ctrl Pts',(30.2382835239775,587.645309537712,-48.7475273422301)) ;
#68235 = CARTESIAN_POINT('Ctrl Pts',(28.4517146365045,587.052627949051,-48.6363050963726)) ;
#68236 = CARTESIAN_POINT('Ctrl Pts',(27.9820998795853,585.229838373894,-48.5250828505152)) ;
#68237 = CARTESIAN_POINT('Ctrl Pts',(29.2598794441691,583.84766605904,-48.4138606046579)) ;
#68238 = CARTESIAN_POINT('Ctrl Pts',(31.1138677246376,584.173025249005,-48.3026383588006)) ;
#68239 = CARTESIAN_POINT('Ctrl Pts',(31.844686428975,585.907614430404,-48.1914161129433)) ;
#68240 = CARTESIAN_POINT('Ctrl Pts',(30.7825274458969,587.461729368807,-48.0801938670858)) ;
#68241 = CARTESIAN_POINT('Ctrl Pts',(28.9007346428137,587.410486647199,-47.9689716212284)) ;
#68242 = CARTESIAN_POINT('Ctrl Pts',(27.9243728537819,585.801797801967,-47.857749375371)) ;
#68243 = CARTESIAN_POINT('Ctrl Pts',(28.7473159241813,584.108168158769,-47.7465271295137)) ;
#68244 = CARTESIAN_POINT('Ctrl Pts',(30.616724477284,583.886550423464,-47.6352906050575)) ;
#68245 = CARTESIAN_POINT('Ctrl Pts',(31.4146761558497,584.849298879313,-47.5611281625539)) ;
#68246 = CARTESIAN_POINT('Ctrl Pts',(31.5205112108052,585.392600214065,-47.5240398020026)) ;
#68247 = CARTESIAN_POINT('Ctrl Pts',(31.5236569526671,585.391334705933,-47.522160171753)) ;
#68248 = CARTESIAN_POINT('Ctrl Pts',(31.5188401675311,585.329303680336,-47.522160171753)) ;
#68249 = CARTESIAN_POINT('Ctrl Pts',(31.510269991655,585.26781004648,-47.522160171753)) ;
#68250 = CARTESIAN_POINT('Ctrl Pts',(31.4982232071401,585.207069811533,-47.522160171753)) ;
#68251 = CARTESIAN_POINT('Ctrl Pts',(31.4857315767339,585.144086650771,-47.522160171753)) ;
#68252 = CARTESIAN_POINT('Ctrl Pts',(31.4695018364279,585.081912853305,-47.522160171753)) ;
#68253 = CARTESIAN_POINT('Ctrl Pts',(31.449786324334,585.020778555998,-47.5221601717531)) ;
#68254 = CARTESIAN_POINT('Ctrl Pts',(31.4316885056168,584.964660438202,-47.5221601717531)) ;
#68255 = CARTESIAN_POINT('Ctrl Pts',(31.4106526261513,584.909417627139,-47.5221601717531)) ;
#68256 = CARTESIAN_POINT('Ctrl Pts',(31.3868352669909,584.855228845485,-47.522160171753)) ;
#68257 = CARTESIAN_POINT('Ctrl Pts',(31.3751359799049,584.828610860294,-47.5221601717529)) ;
#68258 = CARTESIAN_POINT('Ctrl Pts',(31.3627650218181,584.80224726166,-47.5221601717531)) ;
#68259 = CARTESIAN_POINT('Ctrl Pts',(31.3497379680007,584.776159928329,-47.5221601717531)) ;
#68260 = CARTESIAN_POINT('Ctrl Pts',(31.3438455310544,584.764360025687,-47.5221601717531)) ;
#68261 = CARTESIAN_POINT('Ctrl Pts',(31.3378179980786,584.752615328467,-47.5221601717531)) ;
#68262 = CARTESIAN_POINT('Ctrl Pts',(31.3316669117536,584.740946529661,-47.5221601717531)) ;
#68263 = CARTESIAN_POINT('Ctrl Pts',(31.3001600716856,584.681177090842,-47.522160171753)) ;
#68264 = CARTESIAN_POINT('Ctrl Pts',(31.2653614871049,584.623286734142,-47.522160171753)) ;
#68265 = CARTESIAN_POINT('Ctrl Pts',(31.2275461136954,584.567522616136,-47.5221601717531)) ;
#68266 = CARTESIAN_POINT('Ctrl Pts',(31.1897307402858,584.51175849813,-47.5221601717532)) ;
#68267 = CARTESIAN_POINT('Ctrl Pts',(31.1488981152621,584.45811970133,-47.5221601717531)) ;
#68268 = CARTESIAN_POINT('Ctrl Pts',(31.1052715103391,584.406861182841,-47.5221601717531)) ;
#68269 = CARTESIAN_POINT('Ctrl Pts',(31.0683501055194,584.363480852996,-47.5221601717531)) ;
#68270 = CARTESIAN_POINT('Ctrl Pts',(31.0294265346734,584.321805179775,-47.5221601717531)) ;
#68271 = CARTESIAN_POINT('Ctrl Pts',(30.988610958903,584.28200051088,-47.5221601717531)) ;
#68272 = CARTESIAN_POINT('Ctrl Pts',(30.9697524459878,584.263609079465,-47.5221601717531)) ;
#68273 = CARTESIAN_POINT('Ctrl Pts',(30.9504897208788,584.245617269463,-47.5221601717533)) ;
#68274 = CARTESIAN_POINT('Ctrl Pts',(30.9308321861222,584.228042671206,-47.5221601717532)) ;
#68275 = CARTESIAN_POINT('Ctrl Pts',(30.9223660422836,584.220473610355,-47.5221601717531)) ;
#68276 = CARTESIAN_POINT('Ctrl Pts',(30.9138270458502,584.212982410202,-47.522160171753)) ;
#68277 = CARTESIAN_POINT('Ctrl Pts',(30.9052263083889,584.205579107581,-47.522160171753)) ;
#68278 = CARTESIAN_POINT('Ctrl Pts',(30.8519948284383,584.159758762896,-47.522160171753)) ;
#68279 = CARTESIAN_POINT('Ctrl Pts',(30.7963035204994,584.117214641986,-47.5221601717532)) ;
#68280 = CARTESIAN_POINT('Ctrl Pts',(30.7384039283002,584.078214128361,-47.5221601717532)) ;
#68281 = CARTESIAN_POINT('Ctrl Pts',(30.6863451657001,584.043147931813,-47.5221601717533)) ;
#68282 = CARTESIAN_POINT('Ctrl Pts',(30.6325002196233,584.010946103046,-47.5221601717531)) ;
#68283 = CARTESIAN_POINT('Ctrl Pts',(30.5770212017373,583.981821726431,-47.5221601717531)) ;
#68284 = CARTESIAN_POINT('Ctrl Pts',(30.5168873937906,583.950253761881,-47.5221601717532)) ;
#68285 = CARTESIAN_POINT('Ctrl Pts',(30.4548337940956,583.922299973818,-47.5221601717531)) ;
#68286 = CARTESIAN_POINT('Ctrl Pts',(30.3911785114919,583.897901782336,-47.522160171753)) ;
#68287 = CARTESIAN_POINT('Ctrl Pts',(30.3668794535727,583.888588288723,-47.5221601717529)) ;
#68288 = CARTESIAN_POINT('Ctrl Pts',(30.3423467027344,583.879793361185,-47.5221601717531)) ;
#68289 = CARTESIAN_POINT('Ctrl Pts',(30.3175969936173,583.871515452949,-47.5221601717533)) ;
#68290 = CARTESIAN_POINT('Ctrl Pts',(30.3066967610943,583.867869708098,-47.5221601717534)) ;
#68291 = CARTESIAN_POINT('Ctrl Pts',(30.2957553887351,583.864324663052,-47.522160171753)) ;
#68292 = CARTESIAN_POINT('Ctrl Pts',(30.2847866297612,583.860883806162,-47.522160171753)) ;
#68293 = CARTESIAN_POINT('Ctrl Pts',(30.2180252438734,583.839941019909,-47.522160171753)) ;
#68294 = CARTESIAN_POINT('Ctrl Pts',(30.150133573222,583.822814191443,-47.5221601717531)) ;
#68295 = CARTESIAN_POINT('Ctrl Pts',(30.0814758060322,583.809394978751,-47.522160171753)) ;
#68296 = CARTESIAN_POINT('Ctrl Pts',(30.0112444562779,583.795668208153,-47.522160171753)) ;
#68297 = CARTESIAN_POINT('Ctrl Pts',(29.9402106626795,583.785820679544,-47.5221601717534)) ;
#68298 = CARTESIAN_POINT('Ctrl Pts',(29.8687323076889,583.779782709858,-47.5221601717533)) ;
#68299 = CARTESIAN_POINT('Ctrl Pts',(29.8147182254866,583.775219994459,-47.5221601717533)) ;
#68300 = CARTESIAN_POINT('Ctrl Pts',(29.7604495150754,583.772833624314,-47.5221601717531)) ;
#68301 = CARTESIAN_POINT('Ctrl Pts',(29.7060735484461,583.772611814858,-47.5221601717532)) ;
#68302 = CARTESIAN_POINT('Ctrl Pts',(29.6723780247881,583.77247436469,-47.5221601717532)) ;
#68303 = CARTESIAN_POINT('Ctrl Pts',(29.6386412158712,583.773168416777,-47.5221601717529)) ;
#68304 = CARTESIAN_POINT('Ctrl Pts',(29.6048977269777,583.774694279834,-47.5221601717531)) ;
#68305 = CARTESIAN_POINT('Ctrl Pts',(29.5919967889767,583.775277653555,-47.5221601717532)) ;
#68306 = CARTESIAN_POINT('Ctrl Pts',(29.5790925886481,583.775982789546,-47.5221601717528)) ;
#68307 = CARTESIAN_POINT('Ctrl Pts',(29.5661945128201,583.776809309743,-47.5221601717529)) ;
#68308 = CARTESIAN_POINT('Ctrl Pts',(29.4896246981783,583.781715971724,-47.5221601717529)) ;
#68309 = CARTESIAN_POINT('Ctrl Pts',(29.4134573117978,583.790882449776,-47.5221601717532)) ;
#68310 = CARTESIAN_POINT('Ctrl Pts',(29.3381059440092,583.804240827962,-47.5221601717532)) ;
#68311 = CARTESIAN_POINT('Ctrl Pts',(29.2815924181677,583.814259611602,-47.5221601717532)) ;
#68312 = CARTESIAN_POINT('Ctrl Pts',(29.2255372354374,583.826637473437,-47.5221601717532)) ;
#68313 = CARTESIAN_POINT('Ctrl Pts',(29.1701114870961,583.841366868005,-47.5221601717533)) ;
#68314 = CARTESIAN_POINT('Ctrl Pts',(29.1504411817609,583.846594252339,-47.5221601717533)) ;
#68315 = CARTESIAN_POINT('Ctrl Pts',(29.1308501530702,583.852117980893,-47.5221601717531)) ;
#68316 = CARTESIAN_POINT('Ctrl Pts',(29.1113460858728,583.857938274527,-47.5221601717531)) ;
#68317 = CARTESIAN_POINT('Ctrl Pts',(29.096575143476,583.862346135776,-47.5221601717531)) ;
#68318 = CARTESIAN_POINT('Ctrl Pts',(29.0818589756558,583.86692269961,-47.5221601717531)) ;
#68319 = CARTESIAN_POINT('Ctrl Pts',(29.0672084681585,583.871665170823,-47.5221601717531)) ;
#68320 = CARTESIAN_POINT('Ctrl Pts',(28.9955587082349,583.894858696637,-47.5221601717532)) ;
#68321 = CARTESIAN_POINT('Ctrl Pts',(28.9254238704092,583.922032771105,-47.5221601717531)) ;
#68322 = CARTESIAN_POINT('Ctrl Pts',(28.8571829382313,583.953155379993,-47.522160171753)) ;
#68323 = CARTESIAN_POINT('Ctrl Pts',(28.8020543600867,583.978297843927,-47.522160171753)) ;
#68324 = CARTESIAN_POINT('Ctrl Pts',(28.7481613973935,584.006018160781,-47.5221601717531)) ;
#68325 = CARTESIAN_POINT('Ctrl Pts',(28.6957076913023,584.036324060624,-47.5221601717529)) ;
#68326 = CARTESIAN_POINT('Ctrl Pts',(28.6853634342856,584.042300607192,-47.5221601717529)) ;
#68327 = CARTESIAN_POINT('Ctrl Pts',(28.6750751736428,584.048377778284,-47.522160171753)) ;
#68328 = CARTESIAN_POINT('Ctrl Pts',(28.6648434444544,584.05455423117,-47.5221601717531)) ;
#68329 = CARTESIAN_POINT('',(31.158643478419,586.791459225795,-49.5230281993293)) ;
#68330 = CARTESIAN_POINT('Ctrl Pts',(31.1572796596168,586.790298588641,-49.5230281993293)) ;
#68331 = CARTESIAN_POINT('Ctrl Pts',(31.1523539815153,586.796086558105,-49.5227388568039)) ;
#68332 = CARTESIAN_POINT('Ctrl Pts',(31.1473886962525,586.801840821075,-49.5224495142784)) ;
#68333 = CARTESIAN_POINT('Ctrl Pts',(31.1423842688183,586.807560838673,-49.5221601717531)) ;
#68334 = CARTESIAN_POINT('Ctrl Pts',(30.4186978426039,583.72539083489,-49.5221601717529)) ;
#68335 = CARTESIAN_POINT('Ctrl Pts',(30.4873003083186,583.750791784544,-49.5221601717532)) ;
#68336 = CARTESIAN_POINT('Ctrl Pts',(30.554200304582,583.780092786686,-49.5221601717532)) ;
#68337 = CARTESIAN_POINT('Ctrl Pts',(30.6192099749106,583.812997033709,-49.5221601717531)) ;
#68338 = CARTESIAN_POINT('Ctrl Pts',(30.6860813906505,583.846843591785,-49.522160171753)) ;
#68339 = CARTESIAN_POINT('Ctrl Pts',(30.7509534329247,583.884503418489,-49.5221601717532)) ;
#68340 = CARTESIAN_POINT('Ctrl Pts',(30.8135904385567,583.925698250773,-49.5221601717532)) ;
#68341 = CARTESIAN_POINT('Ctrl Pts',(30.8665813102266,583.960549055804,-49.5221601717531)) ;
#68342 = CARTESIAN_POINT('Ctrl Pts',(30.9179722019561,583.997930973722,-49.5221601717531)) ;
#68343 = CARTESIAN_POINT('Ctrl Pts',(30.9675975968691,584.037693629774,-49.5221601717531)) ;
#68344 = CARTESIAN_POINT('Ctrl Pts',(30.9896051368742,584.05532730796,-49.5221601717531)) ;
#68345 = CARTESIAN_POINT('Ctrl Pts',(31.0112651554311,584.073429381718,-49.522160171753)) ;
#68346 = CARTESIAN_POINT('Ctrl Pts',(31.0325616669576,584.09198745669,-49.5221601717529)) ;
#68347 = CARTESIAN_POINT('Ctrl Pts',(31.0442315898504,584.102156789056,-49.5221601717529)) ;
#68348 = CARTESIAN_POINT('Ctrl Pts',(31.055792343147,584.112463053672,-49.5221601717529)) ;
#68349 = CARTESIAN_POINT('Ctrl Pts',(31.0672411640197,584.122904252017,-49.5221601717529)) ;
#68350 = CARTESIAN_POINT('Ctrl Pts',(31.0778809940872,584.132607659672,-49.522160171753)) ;
#68351 = CARTESIAN_POINT('Ctrl Pts',(31.0884256653329,584.142429199591,-49.5221601717529)) ;
#68352 = CARTESIAN_POINT('Ctrl Pts',(31.0988568852982,584.152351608469,-49.5221601717529)) ;
#68353 = CARTESIAN_POINT('Ctrl Pts',(31.1519330615585,584.202838850063,-49.5221601717529)) ;
#68354 = CARTESIAN_POINT('Ctrl Pts',(31.2021692727164,584.256018704938,-49.522160171753)) ;
#68355 = CARTESIAN_POINT('Ctrl Pts',(31.2493474364414,584.311628175327,-49.522160171753)) ;
#68356 = CARTESIAN_POINT('Ctrl Pts',(31.2961710704225,584.366819757232,-49.522160171753)) ;
#68357 = CARTESIAN_POINT('Ctrl Pts',(31.339982954292,584.424405467255,-49.522160171753)) ;
#68358 = CARTESIAN_POINT('Ctrl Pts',(31.3805250711276,584.484152427248,-49.522160171753)) ;
#68359 = CARTESIAN_POINT('Ctrl Pts',(31.414278646109,584.533895106008,-49.5221601717531)) ;
#68360 = CARTESIAN_POINT('Ctrl Pts',(31.4457651463981,584.585136509089,-49.5221601717531)) ;
#68361 = CARTESIAN_POINT('Ctrl Pts',(31.474807879904,584.637748693389,-49.5221601717531)) ;
#68362 = CARTESIAN_POINT('Ctrl Pts',(31.4868690766659,584.659598079804,-49.5221601717531)) ;
#68363 = CARTESIAN_POINT('Ctrl Pts',(31.4985084828501,584.681683918493,-49.522160171753)) ;
#68364 = CARTESIAN_POINT('Ctrl Pts',(31.5097120155267,584.703997122186,-49.522160171753)) ;
#68365 = CARTESIAN_POINT('Ctrl Pts',(31.5149384960288,584.714406296454,-49.522160171753)) ;
#68366 = CARTESIAN_POINT('Ctrl Pts',(31.5200701071974,584.724864950923,-49.522160171753)) ;
#68367 = CARTESIAN_POINT('Ctrl Pts',(31.525105353132,584.735372160716,-49.522160171753)) ;
#68368 = CARTESIAN_POINT('Ctrl Pts',(31.5302972980837,584.746206359393,-49.522160171753)) ;
#68369 = CARTESIAN_POINT('Ctrl Pts',(31.5353830964004,584.757084541308,-49.5221601717531)) ;
#68370 = CARTESIAN_POINT('Ctrl Pts',(31.5403599433786,584.768001876211,-49.5221601717531)) ;
#68371 = CARTESIAN_POINT('Ctrl Pts',(31.5689008468457,584.830609909557,-49.522160171753)) ;
#68372 = CARTESIAN_POINT('Ctrl Pts',(31.5938812454169,584.894543521471,-49.5221601717529)) ;
#68373 = CARTESIAN_POINT('Ctrl Pts',(31.6150780535725,584.959595021631,-49.5221601717529)) ;
#68374 = CARTESIAN_POINT('Ctrl Pts',(31.6344250442579,585.018969563233,-49.522160171753)) ;
#68375 = CARTESIAN_POINT('Ctrl Pts',(31.6506197270796,585.079276003087,-49.5221601717531)) ;
#68376 = CARTESIAN_POINT('Ctrl Pts',(31.6634548036038,585.140361228952,-49.522160171753)) ;
#68377 = CARTESIAN_POINT('Ctrl Pts',(31.6785404513754,585.212157466372,-49.522160171753)) ;
#68378 = CARTESIAN_POINT('Ctrl Pts',(31.6889855555218,585.285031068209,-49.522160171753)) ;
#68379 = CARTESIAN_POINT('Ctrl Pts',(31.6948651281539,585.358560609028,-49.522160171753)) ;
#68380 = CARTESIAN_POINT('Ctrl Pts',(31.6961694101108,585.374871871663,-49.522160171753)) ;
#68381 = CARTESIAN_POINT('Ctrl Pts',(31.6972487956621,585.391215328875,-49.522160171753)) ;
#68382 = CARTESIAN_POINT('Ctrl Pts',(31.698103724415,585.407586209828,-49.522160171753)) ;
#68383 = CARTESIAN_POINT('Ctrl Pts',(31.6989406415282,585.423612189046,-49.522160171753)) ;
#68384 = CARTESIAN_POINT('Ctrl Pts',(31.6995624570579,585.4396697465,-49.522160171753)) ;
#68385 = CARTESIAN_POINT('Ctrl Pts',(31.6999690832809,585.455723162103,-49.522160171753)) ;
#68386 = CARTESIAN_POINT('Ctrl Pts',(31.7017073058113,585.524347385327,-49.522160171753)) ;
#68387 = CARTESIAN_POINT('Ctrl Pts',(31.6995250570887,585.592990128663,-49.522160171753)) ;
#68388 = CARTESIAN_POINT('Ctrl Pts',(31.6935434789382,585.661314289035,-49.522160171753)) ;
#68389 = CARTESIAN_POINT('Ctrl Pts',(31.6875769121955,585.729466982645,-49.522160171753)) ;
#68390 = CARTESIAN_POINT('Ctrl Pts',(31.6778295899244,585.797303747662,-49.522160171753)) ;
#68391 = CARTESIAN_POINT('Ctrl Pts',(31.6643723151243,585.864474977224,-49.522160171753)) ;
#68392 = CARTESIAN_POINT('Ctrl Pts',(31.6545223425228,585.913640560942,-49.5221601717531)) ;
#68393 = CARTESIAN_POINT('Ctrl Pts',(31.642683744479,585.9624493375,-49.522160171753)) ;
#68394 = CARTESIAN_POINT('Ctrl Pts',(31.628869585479,586.01075422025,-49.522160171753)) ;
#68395 = CARTESIAN_POINT('Ctrl Pts',(31.6231571947481,586.030729114449,-49.522160171753)) ;
#68396 = CARTESIAN_POINT('Ctrl Pts',(31.617106852988,586.050617722158,-49.522160171753)) ;
#68397 = CARTESIAN_POINT('Ctrl Pts',(31.6107189261506,586.070409070264,-49.522160171753)) ;
#68398 = CARTESIAN_POINT('Ctrl Pts',(31.6059788613649,586.08509494169,-49.522160171753)) ;
#68399 = CARTESIAN_POINT('Ctrl Pts',(31.6010529102216,586.099727253392,-49.5221601717529)) ;
#68400 = CARTESIAN_POINT('Ctrl Pts',(31.5959411138607,586.11430138426,-49.522160171753)) ;
#68401 = CARTESIAN_POINT('Ctrl Pts',(31.5916380395207,586.126569785451,-49.522160171753)) ;
#68402 = CARTESIAN_POINT('Ctrl Pts',(31.5872060372536,586.138788991967,-49.522160171753)) ;
#68403 = CARTESIAN_POINT('Ctrl Pts',(31.5826469038171,586.150953071513,-49.522160171753)) ;
#68404 = CARTESIAN_POINT('Ctrl Pts',(31.5595365757891,586.212613005881,-49.522160171753)) ;
#68405 = CARTESIAN_POINT('Ctrl Pts',(31.5331524711879,586.272888155243,-49.5221601717529)) ;
#68406 = CARTESIAN_POINT('Ctrl Pts',(31.5035447956668,586.33144636608,-49.5221601717529)) ;
#68407 = CARTESIAN_POINT('Ctrl Pts',(31.4825817796702,586.372907125458,-49.522160171753)) ;
#68408 = CARTESIAN_POINT('Ctrl Pts',(31.4600019247098,586.413506657349,-49.5221601717529)) ;
#68409 = CARTESIAN_POINT('Ctrl Pts',(31.4358124034094,586.453115472938,-49.5221601717529)) ;
#68410 = CARTESIAN_POINT('Ctrl Pts',(31.4280853247628,586.465768076904,-49.5221601717529)) ;
#68411 = CARTESIAN_POINT('Ctrl Pts',(31.4201927015562,586.478321394194,-49.5221601717531)) ;
#68412 = CARTESIAN_POINT('Ctrl Pts',(31.4121385580784,586.490764858801,-49.5221601717531)) ;
#68413 = CARTESIAN_POINT('Ctrl Pts',(31.3778747803058,586.543701599648,-49.522160171753)) ;
#68414 = CARTESIAN_POINT('Ctrl Pts',(31.3407548909434,586.594555512031,-49.5221601717529)) ;
#68415 = CARTESIAN_POINT('Ctrl Pts',(31.3008131347297,586.643013002544,-49.522160171753)) ;
#68416 = CARTESIAN_POINT('Ctrl Pts',(31.2636035879197,586.688155766219,-49.522160171753)) ;
#68417 = CARTESIAN_POINT('Ctrl Pts',(31.2239444633598,586.731218909947,-49.5221601717528)) ;
#68418 = CARTESIAN_POINT('Ctrl Pts',(31.1818411981515,586.771914720393,-49.5221601717528)) ;
#68419 = CARTESIAN_POINT('Ctrl Pts',(31.1746523415314,586.778863263336,-49.5221601717528)) ;
#68420 = CARTESIAN_POINT('Ctrl Pts',(31.1673921843832,586.785742701195,-49.522160171753)) ;
#68421 = CARTESIAN_POINT('Ctrl Pts',(31.1600619605025,586.792552516318,-49.522160171753)) ;
#68422 = CARTESIAN_POINT('Ctrl Pts',(28.6224074890457,586.788253409867,-49.5202805469744)) ;
#68423 = CARTESIAN_POINT('Ctrl Pts',(28.2636244773615,586.366765387965,-49.4831921864647)) ;
#68424 = CARTESIAN_POINT('Ctrl Pts',(28.0084321078388,585.14263785445,-49.4090297440025)) ;
#68425 = CARTESIAN_POINT('Ctrl Pts',(29.3472570216431,583.819251769591,-49.297793219588)) ;
#68426 = CARTESIAN_POINT('Ctrl Pts',(31.1844866118933,584.231809776485,-49.1865709737307)) ;
#68427 = CARTESIAN_POINT('Ctrl Pts',(31.8334585912461,585.998161231894,-49.0753487278734)) ;
#68428 = CARTESIAN_POINT('Ctrl Pts',(30.7002431513819,587.50135539588,-48.9641264820159)) ;
#68429 = CARTESIAN_POINT('Ctrl Pts',(28.822941880499,587.362809908455,-48.8529042361585)) ;
#68430 = CARTESIAN_POINT('Ctrl Pts',(27.9224434628909,585.709934174676,-48.7416819903011)) ;
#68431 = CARTESIAN_POINT('Ctrl Pts',(28.8240101900071,584.057569634295,-48.6304597444437)) ;
#68432 = CARTESIAN_POINT('Ctrl Pts',(30.7013185437651,583.920331685552,-48.5192374985864)) ;
#68433 = CARTESIAN_POINT('Ctrl Pts',(31.8336328053599,585.423981994271,-48.4080152527291)) ;
#68434 = CARTESIAN_POINT('Ctrl Pts',(31.1831024500014,587.190308717922,-48.2967930068717)) ;
#68435 = CARTESIAN_POINT('Ctrl Pts',(29.3459859094712,587.600337651261,-48.1855707610142)) ;
#68436 = CARTESIAN_POINT('Ctrl Pts',(28.0061704677458,586.27820841406,-48.0743485151568)) ;
#68437 = CARTESIAN_POINT('Ctrl Pts',(28.3916973927331,584.435855412722,-47.9631262692994)) ;
#68438 = CARTESIAN_POINT('Ctrl Pts',(30.1492683457755,583.761763980669,-47.8519040234422)) ;
#68439 = CARTESIAN_POINT('Ctrl Pts',(31.6678667421111,584.874251660798,-47.7406817775848)) ;
#68440 = CARTESIAN_POINT('Ctrl Pts',(31.5559056918524,586.752715612336,-47.6294595317275)) ;
#68441 = CARTESIAN_POINT('Ctrl Pts',(29.9157317041138,587.677618832294,-47.51823728587)) ;
#68442 = CARTESIAN_POINT('Ctrl Pts',(28.2520962180047,586.796586291543,-47.4069992157278)) ;
#68443 = CARTESIAN_POINT('Ctrl Pts',(28.1434121707751,585.550835925276,-47.3328352275381)) ;
#68444 = CARTESIAN_POINT('Ctrl Pts',(28.3654201435781,585.043770024595,-47.2957453213009)) ;
#68445 = CARTESIAN_POINT('Ctrl Pts',(28.5208652057457,586.874683537923,-49.5972675643953)) ;
#68446 = CARTESIAN_POINT('Ctrl Pts',(28.1333079528429,586.419392360303,-49.5601792038856)) ;
#68447 = CARTESIAN_POINT('Ctrl Pts',(27.8576492664693,585.09709033194,-49.4860167614234)) ;
#68448 = CARTESIAN_POINT('Ctrl Pts',(29.3038473550471,583.667569259663,-49.3747802370089)) ;
#68449 = CARTESIAN_POINT('Ctrl Pts',(31.2884219579716,584.113214238963,-49.2635579911516)) ;
#68450 = CARTESIAN_POINT('Ctrl Pts',(31.9894412073173,586.021226311511,-49.1523357452942)) ;
#68451 = CARTESIAN_POINT('Ctrl Pts',(30.7653423829074,587.644975992522,-49.0411134994368)) ;
#68452 = CARTESIAN_POINT('Ctrl Pts',(28.7374823680225,587.49531921737,-48.9298912535793)) ;
#68453 = CARTESIAN_POINT('Ctrl Pts',(27.7647643696611,585.709883569883,-48.8186690077219)) ;
#68454 = CARTESIAN_POINT('Ctrl Pts',(28.7386363554878,583.925000113285,-48.7074467618646)) ;
#68455 = CARTESIAN_POINT('Ctrl Pts',(30.7665040212914,583.776755740845,-48.5962245160073)) ;
#68456 = CARTESIAN_POINT('Ctrl Pts',(31.9896293933272,585.400998149198,-48.48500227015)) ;
#68457 = CARTESIAN_POINT('Ctrl Pts',(31.2869267868988,587.308983506512,-48.3737800242926)) ;
#68458 = CARTESIAN_POINT('Ctrl Pts',(29.3024743002329,587.751896581659,-48.2625577784351)) ;
#68459 = CARTESIAN_POINT('Ctrl Pts',(27.8552062438262,586.323733155674,-48.1513355325777)) ;
#68460 = CARTESIAN_POINT('Ctrl Pts',(28.2716522602271,584.333624246324,-48.0401132867203)) ;
#68461 = CARTESIAN_POINT('Ctrl Pts',(30.170179637946,583.605470975117,-47.9288910408631)) ;
#68462 = CARTESIAN_POINT('Ctrl Pts',(31.8105689640286,584.807179682491,-47.8176687950058)) ;
#68463 = CARTESIAN_POINT('Ctrl Pts',(31.6896286863195,586.836295624513,-47.7064465491484)) ;
#68464 = CARTESIAN_POINT('Ctrl Pts',(29.9179134593728,587.83537567974,-47.5952243032909)) ;
#68465 = CARTESIAN_POINT('Ctrl Pts',(28.1208551321083,586.883684713078,-47.4839862331486)) ;
#68466 = CARTESIAN_POINT('Ctrl Pts',(28.0034546716436,585.538025710199,-47.409822244959)) ;
#68467 = CARTESIAN_POINT('Ctrl Pts',(28.2432675871385,584.990293345207,-47.3727323387218)) ;
#68468 = CARTESIAN_POINT('Ctrl Pts',(28.4193229224455,586.961113665978,-49.6742545818162)) ;
#68469 = CARTESIAN_POINT('Ctrl Pts',(28.0029914283242,586.472019332639,-49.6371662213065)) ;
#68470 = CARTESIAN_POINT('Ctrl Pts',(27.7068664251,585.051542809432,-49.5630037788443)) ;
#68471 = CARTESIAN_POINT('Ctrl Pts',(29.2604376884511,583.515886749735,-49.4517672544297)) ;
#68472 = CARTESIAN_POINT('Ctrl Pts',(31.3923573040497,583.99461870144,-49.3405450085725)) ;
#68473 = CARTESIAN_POINT('Ctrl Pts',(32.1454238233885,586.044291391129,-49.2293227627151)) ;
#68474 = CARTESIAN_POINT('Ctrl Pts',(30.8304416144329,587.788596589164,-49.1181005168577)) ;
#68475 = CARTESIAN_POINT('Ctrl Pts',(28.652022855546,587.627828526282,-49.0068782710002)) ;
#68476 = CARTESIAN_POINT('Ctrl Pts',(27.6070852764312,585.70983296509,-48.8956560251428)) ;
#68477 = CARTESIAN_POINT('Ctrl Pts',(28.6532625209683,583.792430592273,-48.7844337792855)) ;
#68478 = CARTESIAN_POINT('Ctrl Pts',(30.8316894988174,583.633179796137,-48.6732115334282)) ;
#68479 = CARTESIAN_POINT('Ctrl Pts',(32.1456259812944,585.378014304122,-48.5619892875709)) ;
#68480 = CARTESIAN_POINT('Ctrl Pts',(31.3907511237965,587.4276582951,-48.4507670417135)) ;
#68481 = CARTESIAN_POINT('Ctrl Pts',(29.2589626909946,587.903455512057,-48.339544795856)) ;
#68482 = CARTESIAN_POINT('Ctrl Pts',(27.7042420199065,586.369257897288,-48.2283225499986)) ;
#68483 = CARTESIAN_POINT('Ctrl Pts',(28.1516071277209,584.231393079927,-48.1171003041412)) ;
#68484 = CARTESIAN_POINT('Ctrl Pts',(30.1910909301166,583.449177969564,-48.0058780582839)) ;
#68485 = CARTESIAN_POINT('Ctrl Pts',(31.9532711859459,584.740107704183,-47.8946558124267)) ;
#68486 = CARTESIAN_POINT('Ctrl Pts',(31.8233516807864,586.91987563669,-47.7834335665693)) ;
#68487 = CARTESIAN_POINT('Ctrl Pts',(29.9200952146318,587.993132527187,-47.6722113207118)) ;
#68488 = CARTESIAN_POINT('Ctrl Pts',(27.9896140462121,586.970783134613,-47.5609732505695)) ;
#68489 = CARTESIAN_POINT('Ctrl Pts',(27.863497172512,585.525215495121,-47.4868092623798)) ;
#68490 = CARTESIAN_POINT('Ctrl Pts',(28.1211150306988,584.936816665818,-47.4497193561427)) ;
#68491 = CARTESIAN_POINT('Ctrl Pts',(28.3177806391455,587.047543794034,-49.7512415992371)) ;
#68492 = CARTESIAN_POINT('Ctrl Pts',(27.8726749038054,586.524646304977,-49.7141532387274)) ;
#68493 = CARTESIAN_POINT('Ctrl Pts',(27.5560835837305,585.005995286921,-49.6399907962651)) ;
#68494 = CARTESIAN_POINT('Ctrl Pts',(29.2170280218552,583.364204239807,-49.5287542718506)) ;
#68495 = CARTESIAN_POINT('Ctrl Pts',(31.4962926501278,583.876023163918,-49.4175320259934)) ;
#68496 = CARTESIAN_POINT('Ctrl Pts',(32.3014064394596,586.067356470747,-49.306309780136)) ;
#68497 = CARTESIAN_POINT('Ctrl Pts',(30.8955408459586,587.932217185805,-49.1950875342786)) ;
#68498 = CARTESIAN_POINT('Ctrl Pts',(28.5665633430695,587.760337835196,-49.0838652884211)) ;
#68499 = CARTESIAN_POINT('Ctrl Pts',(27.4494061832013,585.709782360297,-48.9726430425637)) ;
#68500 = CARTESIAN_POINT('Ctrl Pts',(28.567888686449,583.659861071261,-48.8614207967064)) ;
#68501 = CARTESIAN_POINT('Ctrl Pts',(30.8968749763436,583.489603851428,-48.7501985508491)) ;
#68502 = CARTESIAN_POINT('Ctrl Pts',(32.3016225692617,585.355030459046,-48.6389763049918)) ;
#68503 = CARTESIAN_POINT('Ctrl Pts',(31.4945754606939,587.546333083691,-48.5277540591344)) ;
#68504 = CARTESIAN_POINT('Ctrl Pts',(29.2154510817562,588.055014442455,-48.4165318132769)) ;
#68505 = CARTESIAN_POINT('Ctrl Pts',(27.5532777959871,586.414782638902,-48.3053095674195)) ;
#68506 = CARTESIAN_POINT('Ctrl Pts',(28.0315619952149,584.129161913529,-48.1940873215621)) ;
#68507 = CARTESIAN_POINT('Ctrl Pts',(30.2120022222872,583.292884964012,-48.0828650757048)) ;
#68508 = CARTESIAN_POINT('Ctrl Pts',(32.0959734078635,584.673035725876,-47.9716428298476)) ;
#68509 = CARTESIAN_POINT('Ctrl Pts',(31.9570746752535,587.003455648867,-47.8604205839902)) ;
#68510 = CARTESIAN_POINT('Ctrl Pts',(29.9222769698908,588.150889374633,-47.7491983381327)) ;
#68511 = CARTESIAN_POINT('Ctrl Pts',(27.8583729603156,587.057881556148,-47.6379602679904)) ;
#68512 = CARTESIAN_POINT('Ctrl Pts',(27.7235396733805,585.512405280044,-47.5637962798008)) ;
#68513 = CARTESIAN_POINT('Ctrl Pts',(27.9989624742593,584.88333998643,-47.5267063735636)) ;
#68514 = CARTESIAN_POINT('',(29.9417003027147,587.377508131277,-47.5212921527489)) ;
#68515 = CARTESIAN_POINT('Ctrl Pts',(28.0059001157518,584.887332980459,-47.522160171753)) ;
#68516 = CARTESIAN_POINT('Ctrl Pts',(27.982867140185,584.957167490777,-47.522160171753)) ;
#68517 = CARTESIAN_POINT('Ctrl Pts',(27.9639876910789,585.028114081953,-47.5221601717529)) ;
#68518 = CARTESIAN_POINT('Ctrl Pts',(27.9491451721318,585.099835637674,-47.5221601717529)) ;
#68519 = CARTESIAN_POINT('Ctrl Pts',(27.9339594575577,585.173215572568,-47.5221601717529)) ;
#68520 = CARTESIAN_POINT('Ctrl Pts',(27.9229996253534,585.247407769229,-47.5221601717529)) ;
#68521 = CARTESIAN_POINT('Ctrl Pts',(27.9161953558799,585.32205465925,-47.5221601717529)) ;
#68522 = CARTESIAN_POINT('Ctrl Pts',(27.9104710901557,585.384853264689,-47.5221601717529)) ;
#68523 = CARTESIAN_POINT('Ctrl Pts',(27.9076889433615,585.447974061067,-47.5221601717529)) ;
#68524 = CARTESIAN_POINT('Ctrl Pts',(27.9078348642577,585.511197697194,-47.5221601717529)) ;
#68525 = CARTESIAN_POINT('Ctrl Pts',(27.9078999515837,585.539398301253,-47.5221601717529)) ;
#68526 = CARTESIAN_POINT('Ctrl Pts',(27.9085479212935,585.567619241939,-47.5221601717529)) ;
#68527 = CARTESIAN_POINT('Ctrl Pts',(27.9097790499397,585.59584029347,-47.5221601717529)) ;
#68528 = CARTESIAN_POINT('Ctrl Pts',(27.9104536758238,585.6113046821,-47.5221601717529)) ;
#68529 = CARTESIAN_POINT('Ctrl Pts',(27.9113034257906,585.626769094357,-47.5221601717528)) ;
#68530 = CARTESIAN_POINT('Ctrl Pts',(27.9123284599295,585.64223012412,-47.5221601717529)) ;
#68531 = CARTESIAN_POINT('Ctrl Pts',(27.9132810635077,585.656598652656,-47.5221601717529)) ;
#68532 = CARTESIAN_POINT('Ctrl Pts',(27.914385357136,585.670966437285,-47.5221601717529)) ;
#68533 = CARTESIAN_POINT('Ctrl Pts',(27.9156392489812,585.685308412897,-47.5221601717529)) ;
#68534 = CARTESIAN_POINT('Ctrl Pts',(27.9220137363149,585.758219599158,-47.5221601717529)) ;
#68535 = CARTESIAN_POINT('Ctrl Pts',(27.9322573244265,585.830590171318,-47.5221601717529)) ;
#68536 = CARTESIAN_POINT('Ctrl Pts',(27.9463005260323,585.902086531053,-47.5221601717529)) ;
#68537 = CARTESIAN_POINT('Ctrl Pts',(27.9602626500392,585.973170110758,-47.5221601717529)) ;
#68538 = CARTESIAN_POINT('Ctrl Pts',(27.9779810064621,586.043390504702,-47.5221601717529)) ;
#68539 = CARTESIAN_POINT('Ctrl Pts',(27.9994343190645,586.112399884924,-47.5221601717528)) ;
#68540 = CARTESIAN_POINT('Ctrl Pts',(28.0172796994433,586.169803543864,-47.5221601717528)) ;
#68541 = CARTESIAN_POINT('Ctrl Pts',(28.0377103276275,586.22636917177,-47.5221601717529)) ;
#68542 = CARTESIAN_POINT('Ctrl Pts',(28.0607363394367,586.281878854015,-47.5221601717529)) ;
#68543 = CARTESIAN_POINT('Ctrl Pts',(28.070298843717,586.304931546703,-47.5221601717529)) ;
#68544 = CARTESIAN_POINT('Ctrl Pts',(28.0803091959749,586.32780189582,-47.5221601717529)) ;
#68545 = CARTESIAN_POINT('Ctrl Pts',(28.0907690720635,586.35047322507,-47.5221601717529)) ;
#68546 = CARTESIAN_POINT('Ctrl Pts',(28.0956486353482,586.36104946755,-47.5221601717529)) ;
#68547 = CARTESIAN_POINT('Ctrl Pts',(28.1006260339097,586.371582388587,-47.5221601717529)) ;
#68548 = CARTESIAN_POINT('Ctrl Pts',(28.1057014773282,586.382070241986,-47.5221601717529)) ;
#68549 = CARTESIAN_POINT('Ctrl Pts',(28.1109348689906,586.392884478302,-47.522160171753)) ;
#68550 = CARTESIAN_POINT('Ctrl Pts',(28.1162688294438,586.403643148949,-47.5221601717528)) ;
#68551 = CARTESIAN_POINT('Ctrl Pts',(28.1217013309573,586.414341049525,-47.5221601717528)) ;
#68552 = CARTESIAN_POINT('Ctrl Pts',(28.1528552979291,586.475690694877,-47.5221601717528)) ;
#68553 = CARTESIAN_POINT('Ctrl Pts',(28.1872655825553,586.535083110227,-47.522160171753)) ;
#68554 = CARTESIAN_POINT('Ctrl Pts',(28.2249088976231,586.592214387545,-47.522160171753)) ;
#68555 = CARTESIAN_POINT('Ctrl Pts',(28.2592671302627,586.644359893688,-47.5221601717529)) ;
#68556 = CARTESIAN_POINT('Ctrl Pts',(28.2963193822463,586.694621855483,-47.5221601717527)) ;
#68557 = CARTESIAN_POINT('Ctrl Pts',(28.3360751941218,586.742742736611,-47.5221601717528)) ;
#68558 = CARTESIAN_POINT('Ctrl Pts',(28.3828020037815,586.799301391738,-47.5221601717529)) ;
#68559 = CARTESIAN_POINT('Ctrl Pts',(28.4332644628052,586.852903649694,-47.5221601717529)) ;
#68560 = CARTESIAN_POINT('Ctrl Pts',(28.487086318189,586.903345402823,-47.5221601717529)) ;
#68561 = CARTESIAN_POINT('Ctrl Pts',(28.4990257703044,586.914535037439,-47.5221601717529)) ;
#68562 = CARTESIAN_POINT('Ctrl Pts',(28.511130613787,586.925568913959,-47.5221601717527)) ;
#68563 = CARTESIAN_POINT('Ctrl Pts',(28.5233968445569,586.936444401515,-47.5221601717528)) ;
#68564 = CARTESIAN_POINT('Ctrl Pts',(28.5354046498584,586.94709076384,-47.522160171753)) ;
#68565 = CARTESIAN_POINT('Ctrl Pts',(28.5475712576655,586.957588641698,-47.5221601717528)) ;
#68566 = CARTESIAN_POINT('Ctrl Pts',(28.5598687955868,586.967915695398,-47.5221601717528)) ;
#68567 = CARTESIAN_POINT('Ctrl Pts',(28.6123748171967,587.012008464876,-47.5221601717527)) ;
#68568 = CARTESIAN_POINT('Ctrl Pts',(28.6673338270958,587.053054915024,-47.5221601717528)) ;
#68569 = CARTESIAN_POINT('Ctrl Pts',(28.7244079349294,587.090940018963,-47.5221601717528)) ;
#68570 = CARTESIAN_POINT('Ctrl Pts',(28.7814751479459,587.128820546206,-47.5221601717527)) ;
#68571 = CARTESIAN_POINT('Ctrl Pts',(28.8406580638171,587.163540801281,-47.5221601717531)) ;
#68572 = CARTESIAN_POINT('Ctrl Pts',(28.9016380545588,587.194937608893,-47.5221601717529)) ;
#68573 = CARTESIAN_POINT('Ctrl Pts',(28.9462186128203,587.217890830006,-47.5221601717528)) ;
#68574 = CARTESIAN_POINT('Ctrl Pts',(28.9917600957509,587.23906681561,-47.5221601717529)) ;
#68575 = CARTESIAN_POINT('Ctrl Pts',(29.038139360794,587.258384072901,-47.5221601717529)) ;
#68576 = CARTESIAN_POINT('Ctrl Pts',(29.0573179795054,587.26637208892,-47.5221601717529)) ;
#68577 = CARTESIAN_POINT('Ctrl Pts',(29.0766398457555,587.274042085443,-47.5221601717531)) ;
#68578 = CARTESIAN_POINT('Ctrl Pts',(29.0960961522501,587.281387506957,-47.5221601717531)) ;
#68579 = CARTESIAN_POINT('Ctrl Pts',(29.110533411056,587.286838066212,-47.5221601717531)) ;
#68580 = CARTESIAN_POINT('Ctrl Pts',(29.125044693437,587.292109899721,-47.522160171753)) ;
#68581 = CARTESIAN_POINT('Ctrl Pts',(29.1396263608139,587.297200158435,-47.522160171753)) ;
#68582 = CARTESIAN_POINT('Ctrl Pts',(29.1519011062021,587.30148510254,-47.5221601717531)) ;
#68583 = CARTESIAN_POINT('Ctrl Pts',(29.1642177748965,587.305638574356,-47.522160171753)) ;
#68584 = CARTESIAN_POINT('Ctrl Pts',(29.1765706085811,587.309658279919,-47.522160171753)) ;
#68585 = CARTESIAN_POINT('Ctrl Pts',(29.2391873407233,587.330034238421,-47.5221601717529)) ;
#68586 = CARTESIAN_POINT('Ctrl Pts',(29.3027625707403,587.34698725607,-47.5221601717527)) ;
#68587 = CARTESIAN_POINT('Ctrl Pts',(29.3670053078069,587.360349490877,-47.5221601717528)) ;
#68588 = CARTESIAN_POINT('Ctrl Pts',(29.412490861665,587.369810305885,-47.5221601717529)) ;
#68589 = CARTESIAN_POINT('Ctrl Pts',(29.4583111633863,587.377470058772,-47.522160171753)) ;
#68590 = CARTESIAN_POINT('Ctrl Pts',(29.5043605024696,587.38325362236,-47.5221601717531)) ;
#68591 = CARTESIAN_POINT('Ctrl Pts',(29.519070461532,587.385101118661,-47.5221601717531)) ;
#68592 = CARTESIAN_POINT('Ctrl Pts',(29.533806010492,587.386757282783,-47.5221601717531)) ;
#68593 = CARTESIAN_POINT('Ctrl Pts',(29.5485563794087,587.388218673244,-47.522160171753)) ;
#68594 = CARTESIAN_POINT('Ctrl Pts',(29.6113071063726,587.394435691563,-47.5221601717528)) ;
#68595 = CARTESIAN_POINT('Ctrl Pts',(29.6742101689315,587.397121089668,-47.5221601717529)) ;
#68596 = CARTESIAN_POINT('Ctrl Pts',(29.7369990386124,587.396106118865,-47.5221601717529)) ;
#68597 = CARTESIAN_POINT('Ctrl Pts',(29.7954928462785,587.395160576969,-47.5221601717529)) ;
#68598 = CARTESIAN_POINT('Ctrl Pts',(29.8538880283258,587.391003256213,-47.522160171753)) ;
#68599 = CARTESIAN_POINT('Ctrl Pts',(29.911956251404,587.383459021148,-47.5221601717529)) ;
#68600 = CARTESIAN_POINT('Ctrl Pts',(29.9218710199011,587.382170892457,-47.5221601717529)) ;
#68601 = CARTESIAN_POINT('Ctrl Pts',(29.9317762150191,587.380783932454,-47.5221601717531)) ;
#68602 = CARTESIAN_POINT('Ctrl Pts',(29.9416706627822,587.379298783007,-47.5221601717529)) ;
#68603 = CARTESIAN_POINT('Ctrl Pts',(28.6194567455633,586.789923813611,-49.522160171753)) ;
#68604 = CARTESIAN_POINT('Ctrl Pts',(28.5741848796632,586.747689967573,-49.5221601717529)) ;
#68605 = CARTESIAN_POINT('Ctrl Pts',(28.5316464199738,586.702882011821,-49.522160171753)) ;
#68606 = CARTESIAN_POINT('Ctrl Pts',(28.4918376792449,586.655846007778,-49.5221601717529)) ;
#68607 = CARTESIAN_POINT('Ctrl Pts',(28.4493012350658,586.605587086654,-49.5221601717528)) ;
#68608 = CARTESIAN_POINT('Ctrl Pts',(28.4098806731104,586.552784108491,-49.5221601717529)) ;
#68609 = CARTESIAN_POINT('Ctrl Pts',(28.373600628434,586.497804127081,-49.5221601717529)) ;
#68610 = CARTESIAN_POINT('Ctrl Pts',(28.3418555893421,586.449696643347,-49.522160171753)) ;
#68611 = CARTESIAN_POINT('Ctrl Pts',(28.312515258461,586.399921153953,-49.5221601717529)) ;
#68612 = CARTESIAN_POINT('Ctrl Pts',(28.2856192221846,586.348695779004,-49.5221601717528)) ;
#68613 = CARTESIAN_POINT('Ctrl Pts',(28.2721028283307,586.322952865215,-49.5221601717528)) ;
#68614 = CARTESIAN_POINT('Ctrl Pts',(28.2592041019405,586.296843425323,-49.5221601717528)) ;
#68615 = CARTESIAN_POINT('Ctrl Pts',(28.2469304374914,586.270393277738,-49.5221601717528)) ;
#68616 = CARTESIAN_POINT('Ctrl Pts',(28.2413787772024,586.25842926857,-49.5221601717528)) ;
#68617 = CARTESIAN_POINT('Ctrl Pts',(28.2359545091969,586.246394057129,-49.5221601717529)) ;
#68618 = CARTESIAN_POINT('Ctrl Pts',(28.2306666151602,586.234309569701,-49.5221601717529)) ;
#68619 = CARTESIAN_POINT('Ctrl Pts',(28.2038251620089,586.172968476081,-49.5221601717528)) ;
#68620 = CARTESIAN_POINT('Ctrl Pts',(28.1804420988066,586.11025046575,-49.5221601717529)) ;
#68621 = CARTESIAN_POINT('Ctrl Pts',(28.1605384877892,586.046514903665,-49.5221601717529)) ;
#68622 = CARTESIAN_POINT('Ctrl Pts',(28.1402140591507,585.981431794767,-49.5221601717529)) ;
#68623 = CARTESIAN_POINT('Ctrl Pts',(28.123517190455,585.915286818455,-49.5221601717529)) ;
#68624 = CARTESIAN_POINT('Ctrl Pts',(28.1105100613261,585.848425691796,-49.5221601717529)) ;
#68625 = CARTESIAN_POINT('Ctrl Pts',(28.099669740957,585.792702708959,-49.5221601717529)) ;
#68626 = CARTESIAN_POINT('Ctrl Pts',(28.0913928086545,585.736481350659,-49.5221601717529)) ;
#68627 = CARTESIAN_POINT('Ctrl Pts',(28.0857400408894,585.679949476623,-49.5221601717529)) ;
#68628 = CARTESIAN_POINT('Ctrl Pts',(28.0831191304622,585.653738426693,-49.5221601717529)) ;
#68629 = CARTESIAN_POINT('Ctrl Pts',(28.0810626789015,585.627460510806,-49.5221601717529)) ;
#68630 = CARTESIAN_POINT('Ctrl Pts',(28.0795785764974,585.601134047563,-49.5221601717529)) ;
#68631 = CARTESIAN_POINT('Ctrl Pts',(28.078939400595,585.58979571885,-49.5221601717529)) ;
#68632 = CARTESIAN_POINT('Ctrl Pts',(28.0784065214721,585.578448977045,-49.5221601717529)) ;
#68633 = CARTESIAN_POINT('Ctrl Pts',(28.077980858293,585.567108767372,-49.5221601717529)) ;
#68634 = CARTESIAN_POINT('Ctrl Pts',(28.0753463536225,585.496922204811,-49.5221601717529)) ;
#68635 = CARTESIAN_POINT('Ctrl Pts',(28.0768069816538,585.426855163324,-49.5221601717529)) ;
#68636 = CARTESIAN_POINT('Ctrl Pts',(28.0824149563513,585.357271018537,-49.5221601717529)) ;
#68637 = CARTESIAN_POINT('Ctrl Pts',(28.0874572060543,585.294706429303,-49.5221601717529)) ;
#68638 = CARTESIAN_POINT('Ctrl Pts',(28.0958525755181,585.232531249517,-49.5221601717529)) ;
#68639 = CARTESIAN_POINT('Ctrl Pts',(28.107672820771,585.170997260696,-49.5221601717529)) ;
#68640 = CARTESIAN_POINT('Ctrl Pts',(28.1204848067534,585.10430045489,-49.5221601717529)) ;
#68641 = CARTESIAN_POINT('Ctrl Pts',(28.1373194403939,585.038356097394,-49.522160171753)) ;
#68642 = CARTESIAN_POINT('Ctrl Pts',(28.1579325844387,584.973376371762,-49.522160171753)) ;
#68643 = CARTESIAN_POINT('Ctrl Pts',(28.1658012165057,584.948571734891,-49.522160171753)) ;
#68644 = CARTESIAN_POINT('Ctrl Pts',(28.1742209850587,584.923907710175,-49.5221601717529)) ;
#68645 = CARTESIAN_POINT('Ctrl Pts',(28.1831802469027,584.899396416888,-49.5221601717529)) ;
#68646 = CARTESIAN_POINT('Ctrl Pts',(28.1871260725044,584.888601187295,-49.5221601717529)) ;
#68647 = CARTESIAN_POINT('Ctrl Pts',(28.1911762786592,584.877836578581,-49.5221601717529)) ;
#68648 = CARTESIAN_POINT('Ctrl Pts',(28.195325017675,584.867115518396,-49.5221601717529)) ;
#68649 = CARTESIAN_POINT('Ctrl Pts',(28.2208657004741,584.801113970358,-49.5221601717529)) ;
#68650 = CARTESIAN_POINT('Ctrl Pts',(28.2501794469246,584.736642414895,-49.522160171753)) ;
#68651 = CARTESIAN_POINT('Ctrl Pts',(28.2829439666236,584.673925582888,-49.522160171753)) ;
#68652 = CARTESIAN_POINT('Ctrl Pts',(28.3157084863227,584.611208750882,-49.522160171753)) ;
#68653 = CARTESIAN_POINT('Ctrl Pts',(28.351924280498,584.550245857175,-49.5221601717529)) ;
#68654 = CARTESIAN_POINT('Ctrl Pts',(28.3913232488784,584.491265452053,-49.5221601717529)) ;
#68655 = CARTESIAN_POINT('Ctrl Pts',(28.4214332043401,584.446190734508,-49.5221601717529)) ;
#68656 = CARTESIAN_POINT('Ctrl Pts',(28.4534034533065,584.402273869669,-49.5221601717529)) ;
#68657 = CARTESIAN_POINT('Ctrl Pts',(28.4871328972782,584.359622730065,-49.5221601717528)) ;
#68658 = CARTESIAN_POINT('Ctrl Pts',(28.5080342503109,584.333192809463,-49.5221601717528)) ;
#68659 = CARTESIAN_POINT('Ctrl Pts',(28.5296114389798,584.307249043923,-49.522160171753)) ;
#68660 = CARTESIAN_POINT('Ctrl Pts',(28.5518431286008,584.28181868143,-49.522160171753)) ;
#68661 = CARTESIAN_POINT('Ctrl Pts',(28.5603428315767,584.272096049842,-49.522160171753)) ;
#68662 = CARTESIAN_POINT('Ctrl Pts',(28.5689397661541,584.262446785189,-49.522160171753)) ;
#68663 = CARTESIAN_POINT('Ctrl Pts',(28.577627784156,584.252877990672,-49.522160171753)) ;
#68664 = CARTESIAN_POINT('Ctrl Pts',(28.6292044653751,584.196072553074,-49.5221601717531)) ;
#68665 = CARTESIAN_POINT('Ctrl Pts',(28.6838606950433,584.142237698305,-49.5221601717529)) ;
#68666 = CARTESIAN_POINT('Ctrl Pts',(28.7412855049599,584.091654439445,-49.5221601717529)) ;
#68667 = CARTESIAN_POINT('Ctrl Pts',(28.7843541123974,584.0537169953,-49.522160171753)) ;
#68668 = CARTESIAN_POINT('Ctrl Pts',(28.8289813491942,584.017608759369,-49.522160171753)) ;
#68669 = CARTESIAN_POINT('Ctrl Pts',(28.8750546423904,583.983458791694,-49.522160171753)) ;
#68670 = CARTESIAN_POINT('Ctrl Pts',(28.8914058161742,583.971339144553,-49.522160171753)) ;
#68671 = CARTESIAN_POINT('Ctrl Pts',(28.9079392531401,583.959466246145,-49.5221601717529)) ;
#68672 = CARTESIAN_POINT('Ctrl Pts',(28.9246503345323,583.947846242436,-49.5221601717531)) ;
#68673 = CARTESIAN_POINT('Ctrl Pts',(28.9373060740742,583.939046109341,-49.5221601717531)) ;
#68674 = CARTESIAN_POINT('Ctrl Pts',(28.9500595592467,583.93039398515,-49.5221601717528)) ;
#68675 = CARTESIAN_POINT('Ctrl Pts',(28.9629018175317,583.921896637889,-49.5221601717528)) ;
#68676 = CARTESIAN_POINT('Ctrl Pts',(29.0257081415723,583.880339527472,-49.5221601717527)) ;
#68677 = CARTESIAN_POINT('Ctrl Pts',(29.0906820453539,583.842448662337,-49.5221601717529)) ;
#68678 = CARTESIAN_POINT('Ctrl Pts',(29.1575622067351,583.808500383244,-49.522160171753)) ;
#68679 = CARTESIAN_POINT('Ctrl Pts',(29.2115914739247,583.78107520059,-49.522160171753)) ;
#68680 = CARTESIAN_POINT('Ctrl Pts',(29.2668657935751,583.756223325128,-49.522160171753)) ;
#68681 = CARTESIAN_POINT('Ctrl Pts',(29.3232642411662,583.734108789472,-49.5221601717531)) ;
#68682 = CARTESIAN_POINT('Ctrl Pts',(29.3337596629877,583.729993403499,-49.5221601717531)) ;
#68683 = CARTESIAN_POINT('Ctrl Pts',(29.3442940503372,583.725972868921,-49.522160171753)) ;
#68684 = CARTESIAN_POINT('Ctrl Pts',(29.3548662403592,583.722046833005,-49.5221601717529)) ;
#68685 = CARTESIAN_POINT('Ctrl Pts',(29.9416432077809,587.375718227073,-47.5212921527489)) ;
#68686 = CARTESIAN_POINT('Ctrl Pts',(29.9492394590292,587.375475919433,-47.5215814924169)) ;
#68687 = CARTESIAN_POINT('Ctrl Pts',(29.9568340521747,587.375181631047,-47.521870832085)) ;
#68688 = CARTESIAN_POINT('Ctrl Pts',(29.9644262760118,587.374835389473,-47.522160171753)) ;
#68689 = CARTESIAN_POINT('Origin',(212.388527625401,504.21056516053,-49.5221601717613)) ;
#68690 = CARTESIAN_POINT('',(184.88852762542,611.385991641078,-49.52216017176)) ;
#68691 = CARTESIAN_POINT('',(182.13852762542,609.798278400806,-49.5221601717599)) ;
#68692 = CARTESIAN_POINT('',(171.996867127016,603.942987982024,-49.5221601717594)) ;
#68693 = CARTESIAN_POINT('',(182.13852762542,606.622851920264,-49.5221601717599)) ;
#68694 = CARTESIAN_POINT('',(182.13852762542,557.004421780668,-49.5221601717599)) ;
#68695 = CARTESIAN_POINT('',(184.88852762542,605.035138679992,-49.52216017176)) ;
#68696 = CARTESIAN_POINT('',(215.655188123809,587.271998959181,-49.5221601717614)) ;
#68697 = CARTESIAN_POINT('',(187.63852762542,606.622851920264,-49.5221601717601)) ;
#68698 = CARTESIAN_POINT('',(173.371867127016,598.385991641073,-49.5221601717595)) ;
#68699 = CARTESIAN_POINT('',(187.63852762542,609.798278400806,-49.5221601717601)) ;
#68700 = CARTESIAN_POINT('',(187.63852762542,555.416708540397,-49.5221601717601)) ;
#68701 = CARTESIAN_POINT('',(219.780188123809,591.24128205986,-49.5221601717616)) ;
#68702 = CARTESIAN_POINT('',(7.38852762541949,611.385991641109,-49.5221601717519)) ;
#68703 = CARTESIAN_POINT('',(4.63852762541949,609.798278400838,-49.5221601717518)) ;
#68704 = CARTESIAN_POINT('',(61.0593671270093,642.372865274985,-49.5221601717544)) ;
#68705 = CARTESIAN_POINT('',(4.63852762541949,606.622851920295,-49.5221601717518)) ;
#68706 = CARTESIAN_POINT('',(4.63852762541951,557.004421780684,-49.5221601717518)) ;
#68707 = CARTESIAN_POINT('',(7.38852762541949,605.035138680023,-49.5221601717519)) ;
#68708 = CARTESIAN_POINT('',(104.717688123816,548.842121666274,-49.5221601717564)) ;
#68709 = CARTESIAN_POINT('',(10.1385276254195,606.622851920295,-49.522160171752)) ;
#68710 = CARTESIAN_POINT('',(62.4343671270093,636.815868934035,-49.5221601717544)) ;
#68711 = CARTESIAN_POINT('',(10.1385276254195,609.798278400838,-49.522160171752)) ;
#68712 = CARTESIAN_POINT('',(10.1385276254195,555.416708540412,-49.5221601717521)) ;
#68713 = CARTESIAN_POINT('',(108.842688123816,552.811404766952,-49.5221601717565)) ;
#68714 = CARTESIAN_POINT('',(7.38852762540283,516.385991641109,-49.5221601717519)) ;
#68715 = CARTESIAN_POINT('',(4.63852762540283,514.798278400837,-49.5221601717518)) ;
#68716 = CARTESIAN_POINT('',(81.6274704668794,559.247865274989,-49.5221601717553)) ;
#68717 = CARTESIAN_POINT('',(4.63852762540283,511.622851920295,-49.5221601717518)) ;
#68718 = CARTESIAN_POINT('',(4.63852762540284,509.504421780684,-49.5221601717518)) ;
#68719 = CARTESIAN_POINT('',(7.38852762540283,510.035138680023,-49.5221601717519)) ;
#68720 = CARTESIAN_POINT('',(84.149584783925,465.71712166627,-49.5221601717554)) ;
#68721 = CARTESIAN_POINT('',(10.1385276254028,511.622851920295,-49.5221601717521)) ;
#68722 = CARTESIAN_POINT('',(83.0024704668793,553.690868934039,-49.5221601717554)) ;
#68723 = CARTESIAN_POINT('',(10.1385276254028,514.798278400837,-49.5221601717521)) ;
#68724 = CARTESIAN_POINT('',(10.1385276254028,507.916708540412,-49.5221601717521)) ;
#68725 = CARTESIAN_POINT('',(88.274584783925,469.686404766949,-49.5221601717556)) ;
#68726 = CARTESIAN_POINT('Ctrl Pts',(178.619456745563,586.789923813584,-49.5221601717599)) ;
#68727 = CARTESIAN_POINT('Ctrl Pts',(178.574188300298,586.747693158636,-49.5221601717599)) ;
#68728 = CARTESIAN_POINT('Ctrl Pts',(178.531653457537,586.702888053417,-49.5221601717598)) ;
#68729 = CARTESIAN_POINT('Ctrl Pts',(178.491848419612,586.655854613672,-49.5221601717598)) ;
#68730 = CARTESIAN_POINT('Ctrl Pts',(178.449312342082,586.605594190776,-49.5221601717598)) ;
#68731 = CARTESIAN_POINT('Ctrl Pts',(178.409892770719,586.552788955222,-49.5221601717599)) ;
#68732 = CARTESIAN_POINT('Ctrl Pts',(178.373614216098,586.497806119515,-49.5221601717597)) ;
#68733 = CARTESIAN_POINT('Ctrl Pts',(178.341870480804,586.449696138271,-49.5221601717596)) ;
#68734 = CARTESIAN_POINT('Ctrl Pts',(178.312531836416,586.399917693953,-49.5221601717595)) ;
#68735 = CARTESIAN_POINT('Ctrl Pts',(178.285637791918,586.348689004949,-49.5221601717596)) ;
#68736 = CARTESIAN_POINT('Ctrl Pts',(178.272123794534,586.322947083936,-49.5221601717597)) ;
#68737 = CARTESIAN_POINT('Ctrl Pts',(178.259227414255,586.296838621709,-49.5221601717596)) ;
#68738 = CARTESIAN_POINT('Ctrl Pts',(178.246956033732,586.27038944072,-49.5221601717597)) ;
#68739 = CARTESIAN_POINT('Ctrl Pts',(178.241402994952,586.258420670992,-49.5221601717597)) ;
#68740 = CARTESIAN_POINT('Ctrl Pts',(178.235977443094,586.246380627231,-49.5221601717596)) ;
#68741 = CARTESIAN_POINT('Ctrl Pts',(178.230688367278,586.234291259783,-49.5221601717597)) ;
#68742 = CARTESIAN_POINT('Ctrl Pts',(178.203851554736,586.172949713692,-49.5221601717599)) ;
#68743 = CARTESIAN_POINT('Ctrl Pts',(178.180473003136,586.11023107781,-49.5221601717597)) ;
#68744 = CARTESIAN_POINT('Ctrl Pts',(178.160573650426,586.046494799319,-49.5221601717599)) ;
#68745 = CARTESIAN_POINT('Ctrl Pts',(178.140312058258,585.98159829239,-49.52216017176)) ;
#68746 = CARTESIAN_POINT('Ctrl Pts',(178.123656932244,585.915645914293,-49.52216017176)) ;
#68747 = CARTESIAN_POINT('Ctrl Pts',(178.110669719504,585.848980531874,-49.5221601717598)) ;
#68748 = CARTESIAN_POINT('Ctrl Pts',(178.099775969142,585.793061217362,-49.5221601717596)) ;
#68749 = CARTESIAN_POINT('Ctrl Pts',(178.091463494471,585.736639290757,-49.5221601717596)) ;
#68750 = CARTESIAN_POINT('Ctrl Pts',(178.085793601831,585.679904697295,-49.5221601717596)) ;
#68751 = CARTESIAN_POINT('Ctrl Pts',(178.083174326351,585.653695465663,-49.5221601717595)) ;
#68752 = CARTESIAN_POINT('Ctrl Pts',(178.081119341285,585.627419393335,-49.5221601717596)) ;
#68753 = CARTESIAN_POINT('Ctrl Pts',(178.079636526497,585.601094799355,-49.5221601717597)) ;
#68754 = CARTESIAN_POINT('Ctrl Pts',(178.078997639764,585.589752564316,-49.5221601717597)) ;
#68755 = CARTESIAN_POINT('Ctrl Pts',(178.078465104061,585.578401896586,-49.5221601717596)) ;
#68756 = CARTESIAN_POINT('Ctrl Pts',(178.078039839316,585.567057770085,-49.5221601717596)) ;
#68757 = CARTESIAN_POINT('Ctrl Pts',(178.075408552685,585.496867027165,-49.5221601717596)) ;
#68758 = CARTESIAN_POINT('Ctrl Pts',(178.076872157339,585.426795955192,-49.5221601717597)) ;
#68759 = CARTESIAN_POINT('Ctrl Pts',(178.082482737992,585.357208068564,-49.5221601717599)) ;
#68760 = CARTESIAN_POINT('Ctrl Pts',(178.087527938951,585.294632571642,-49.52216017176)) ;
#68761 = CARTESIAN_POINT('Ctrl Pts',(178.095926768028,585.232446811339,-49.5221601717598)) ;
#68762 = CARTESIAN_POINT('Ctrl Pts',(178.107750914516,585.170902758999,-49.5221601717598)) ;
#68763 = CARTESIAN_POINT('Ctrl Pts',(178.120565934992,585.104201260358,-49.5221601717598)) ;
#68764 = CARTESIAN_POINT('Ctrl Pts',(178.137403372988,585.03825267637,-49.5221601717599)) ;
#68765 = CARTESIAN_POINT('Ctrl Pts',(178.158019131495,584.973269147845,-49.5221601717598)) ;
#68766 = CARTESIAN_POINT('Ctrl Pts',(178.165888242172,584.948464696534,-49.5221601717597)) ;
#68767 = CARTESIAN_POINT('Ctrl Pts',(178.174308388922,584.923800900598,-49.5221601717596)) ;
#68768 = CARTESIAN_POINT('Ctrl Pts',(178.18326793304,584.89928987474,-49.5221601717596)) ;
#68769 = CARTESIAN_POINT('Ctrl Pts',(178.187213992827,584.888494462361,-49.5221601717596)) ;
#68770 = CARTESIAN_POINT('Ctrl Pts',(178.191264420398,584.877729679907,-49.52216017176)) ;
#68771 = CARTESIAN_POINT('Ctrl Pts',(178.19541336821,584.86700845477,-49.52216017176)) ;
#68772 = CARTESIAN_POINT('Ctrl Pts',(178.220666969342,584.801751055667,-49.5221601717596)) ;
#68773 = CARTESIAN_POINT('Ctrl Pts',(178.249608559619,584.737989620282,-49.5221601717598)) ;
#68774 = CARTESIAN_POINT('Ctrl Pts',(178.28192640687,584.67594128411,-49.5221601717598)) ;
#68775 = CARTESIAN_POINT('Ctrl Pts',(178.314984652773,584.612471426755,-49.5221601717598)) ;
#68776 = CARTESIAN_POINT('Ctrl Pts',(178.351575930346,584.550793244105,-49.5221601717599)) ;
#68777 = CARTESIAN_POINT('Ctrl Pts',(178.39142267349,584.491143041426,-49.5221601717599)) ;
#68778 = CARTESIAN_POINT('Ctrl Pts',(178.421531675276,584.446070146698,-49.5221601717599)) ;
#68779 = CARTESIAN_POINT('Ctrl Pts',(178.453500638765,584.40215513963,-49.5221601717599)) ;
#68780 = CARTESIAN_POINT('Ctrl Pts',(178.487228506351,584.359505850618,-49.5221601717599)) ;
#68781 = CARTESIAN_POINT('Ctrl Pts',(178.508128949918,584.333076991578,-49.5221601717599)) ;
#68782 = CARTESIAN_POINT('Ctrl Pts',(178.529705121679,584.30713428798,-49.5221601717597)) ;
#68783 = CARTESIAN_POINT('Ctrl Pts',(178.551935695738,584.281704977885,-49.5221601717598)) ;
#68784 = CARTESIAN_POINT('Ctrl Pts',(178.560436077436,584.271981484396,-49.5221601717599)) ;
#68785 = CARTESIAN_POINT('Ctrl Pts',(178.569033700254,584.262331376981,-49.5221601717599)) ;
#68786 = CARTESIAN_POINT('Ctrl Pts',(178.577722419645,584.252761755006,-49.5221601717599)) ;
#68787 = CARTESIAN_POINT('Ctrl Pts',(178.629299529824,584.195955518691,-49.52216017176)) ;
#68788 = CARTESIAN_POINT('Ctrl Pts',(178.683956074342,584.142120120314,-49.52216017176)) ;
#68789 = CARTESIAN_POINT('Ctrl Pts',(178.741381145388,584.091536509087,-49.5221601717598)) ;
#68790 = CARTESIAN_POINT('Ctrl Pts',(178.784449948673,584.053598800666,-49.5221601717597)) ;
#68791 = CARTESIAN_POINT('Ctrl Pts',(178.829077351025,584.017490408156,-49.5221601717598)) ;
#68792 = CARTESIAN_POINT('Ctrl Pts',(178.875150804438,583.983340366146,-49.5221601717598)) ;
#68793 = CARTESIAN_POINT('Ctrl Pts',(178.891493617505,583.971226931804,-49.5221601717598)) ;
#68794 = CARTESIAN_POINT('Ctrl Pts',(178.908018505489,583.959360002586,-49.5221601717597)) ;
#68795 = CARTESIAN_POINT('Ctrl Pts',(178.924720857825,583.947745713805,-49.5221601717597)) ;
#68796 = CARTESIAN_POINT('Ctrl Pts',(178.937371839859,583.938948620093,-49.5221601717597)) ;
#68797 = CARTESIAN_POINT('Ctrl Pts',(178.950120518772,583.930299415061,-49.5221601717595)) ;
#68798 = CARTESIAN_POINT('Ctrl Pts',(178.962957900953,583.921804880912,-49.5221601717595)) ;
#68799 = CARTESIAN_POINT('Ctrl Pts',(179.025763082393,583.880246504684,-49.5221601717595)) ;
#68800 = CARTESIAN_POINT('Ctrl Pts',(179.090735890326,583.842354383869,-49.5221601717597)) ;
#68801 = CARTESIAN_POINT('Ctrl Pts',(179.157615054692,583.808404790033,-49.5221601717597)) ;
#68802 = CARTESIAN_POINT('Ctrl Pts',(179.211658678873,583.78097084842,-49.5221601717596)) ;
#68803 = CARTESIAN_POINT('Ctrl Pts',(179.266948118332,583.75611161908,-49.5221601717595)) ;
#68804 = CARTESIAN_POINT('Ctrl Pts',(179.32336237667,583.733991238111,-49.5221601717598)) ;
#68805 = CARTESIAN_POINT('Ctrl Pts',(179.333841264731,583.729882401039,-49.5221601717599)) ;
#68806 = CARTESIAN_POINT('Ctrl Pts',(179.344358997566,583.725868115481,-49.5221601717977)) ;
#68807 = CARTESIAN_POINT('Ctrl Pts',(179.354914418328,583.721948031586,-49.5221601717676)) ;
#68808 = CARTESIAN_POINT('',(181.158603910567,586.791560837527,-49.5230454887661)) ;
#68809 = CARTESIAN_POINT('Ctrl Pts',(180.418697842604,583.725390834864,-49.5221601717597)) ;
#68810 = CARTESIAN_POINT('Ctrl Pts',(180.487296450736,583.750790356198,-49.5221601717599)) ;
#68811 = CARTESIAN_POINT('Ctrl Pts',(180.554192682413,583.780090567917,-49.5221601717597)) ;
#68812 = CARTESIAN_POINT('Ctrl Pts',(180.619198732011,583.812994518591,-49.5221601717598)) ;
#68813 = CARTESIAN_POINT('Ctrl Pts',(180.686069299032,583.846842227418,-49.52216017176)) ;
#68814 = CARTESIAN_POINT('Ctrl Pts',(180.750940472857,583.884504055634,-49.5221601717598)) ;
#68815 = CARTESIAN_POINT('Ctrl Pts',(180.813576621044,583.925701550019,-49.5221601717597)) ;
#68816 = CARTESIAN_POINT('Ctrl Pts',(180.866567999829,583.960555417843,-49.5221601717596)) ;
#68817 = CARTESIAN_POINT('Ctrl Pts',(180.917959332204,583.997940989355,-49.5221601717597)) ;
#68818 = CARTESIAN_POINT('Ctrl Pts',(180.967585109464,584.037707766149,-49.5221601717599)) ;
#68819 = CARTESIAN_POINT('Ctrl Pts',(180.989595033746,584.0553450465,-49.5221601717599)) ;
#68820 = CARTESIAN_POINT('Ctrl Pts',(181.011257355173,584.073450908606,-49.5221601717598)) ;
#68821 = CARTESIAN_POINT('Ctrl Pts',(181.03255608396,584.092012943614,-49.5221601717598)) ;
#68822 = CARTESIAN_POINT('Ctrl Pts',(181.044224754291,584.102182295473,-49.5221601717598)) ;
#68823 = CARTESIAN_POINT('Ctrl Pts',(181.055784275477,584.112488573221,-49.5221601717599)) ;
#68824 = CARTESIAN_POINT('Ctrl Pts',(181.067231885704,584.122929777226,-49.5221601717597)) ;
#68825 = CARTESIAN_POINT('Ctrl Pts',(181.077873257536,584.132635622549,-49.5221601717596)) ;
#68826 = CARTESIAN_POINT('Ctrl Pts',(181.08841944345,584.142459654982,-49.5221601717598)) ;
#68827 = CARTESIAN_POINT('Ctrl Pts',(181.098852143756,584.152384601306,-49.5221601717598)) ;
#68828 = CARTESIAN_POINT('Ctrl Pts',(181.151927496952,584.202876805252,-49.5221601717598)) ;
#68829 = CARTESIAN_POINT('Ctrl Pts',(181.202162899846,584.25606195107,-49.52216017176)) ;
#68830 = CARTESIAN_POINT('Ctrl Pts',(181.249340293922,584.311676856567,-49.5221601717599)) ;
#68831 = CARTESIAN_POINT('Ctrl Pts',(181.296163855244,584.366874647563,-49.5221601717598)) ;
#68832 = CARTESIAN_POINT('Ctrl Pts',(181.339975615632,584.424466779741,-49.5221601717597)) ;
#68833 = CARTESIAN_POINT('Ctrl Pts',(181.380517571197,584.484220184186,-49.5221601717597)) ;
#68834 = CARTESIAN_POINT('Ctrl Pts',(181.414270877463,584.533968030153,-49.5221601717597)) ;
#68835 = CARTESIAN_POINT('Ctrl Pts',(181.445757100861,584.585214604105,-49.5221601717599)) ;
#68836 = CARTESIAN_POINT('Ctrl Pts',(181.474799558564,584.637831851519,-49.52216017176)) ;
#68837 = CARTESIAN_POINT('Ctrl Pts',(181.486860259247,584.659682649351,-49.52216017176)) ;
#68838 = CARTESIAN_POINT('Ctrl Pts',(181.498499196222,584.681769865865,-49.5221601717599)) ;
#68839 = CARTESIAN_POINT('Ctrl Pts',(181.509702288582,584.704084406422,-49.52216017176)) ;
#68840 = CARTESIAN_POINT('Ctrl Pts',(181.514927026246,584.714491142058,-49.52216017176)) ;
#68841 = CARTESIAN_POINT('Ctrl Pts',(181.520056956668,584.724947319877,-49.5221601717599)) ;
#68842 = CARTESIAN_POINT('Ctrl Pts',(181.525090585488,584.735452015056,-49.5221601717597)) ;
#68843 = CARTESIAN_POINT('Ctrl Pts',(181.530284200014,584.746290584888,-49.5221601717596)) ;
#68844 = CARTESIAN_POINT('Ctrl Pts',(181.535371608344,584.757173173073,-49.5221601717597)) ;
#68845 = CARTESIAN_POINT('Ctrl Pts',(181.540349993555,584.768094923541,-49.5221601717597)) ;
#68846 = CARTESIAN_POINT('Ctrl Pts',(181.568890832369,584.830708784548,-49.5221601717597)) ;
#68847 = CARTESIAN_POINT('Ctrl Pts',(181.593871140868,584.894647947158,-49.52216017176)) ;
#68848 = CARTESIAN_POINT('Ctrl Pts',(181.615067844391,584.959704548492,-49.52216017176)) ;
#68849 = CARTESIAN_POINT('Ctrl Pts',(181.634414752743,585.019083786513,-49.52216017176)) ;
#68850 = CARTESIAN_POINT('Ctrl Pts',(181.650609336792,585.079394549769,-49.5221601717599)) ;
#68851 = CARTESIAN_POINT('Ctrl Pts',(181.663444305221,585.140483589067,-49.5221601717599)) ;
#68852 = CARTESIAN_POINT('Ctrl Pts',(181.678529682811,585.212283627337,-49.5221601717598)) ;
#68853 = CARTESIAN_POINT('Ctrl Pts',(181.688974591945,585.285160304771,-49.5221601717599)) ;
#68854 = CARTESIAN_POINT('Ctrl Pts',(181.69485402845,585.358692290302,-49.5221601717597)) ;
#68855 = CARTESIAN_POINT('Ctrl Pts',(181.696158240314,585.375003596294,-49.5221601717597)) ;
#68856 = CARTESIAN_POINT('Ctrl Pts',(181.697237572428,585.391347063828,-49.5221601717598)) ;
#68857 = CARTESIAN_POINT('Ctrl Pts',(181.698092464185,585.407717923508,-49.5221601717599)) ;
#68858 = CARTESIAN_POINT('Ctrl Pts',(181.698929390057,585.42374474318,-49.5221601717599)) ;
#68859 = CARTESIAN_POINT('Ctrl Pts',(181.699551206998,585.439803114389,-49.5221601717596)) ;
#68860 = CARTESIAN_POINT('Ctrl Pts',(181.699957827124,585.455857315496,-49.5221601717596)) ;
#68861 = CARTESIAN_POINT('Ctrl Pts',(181.701693898361,585.524400987964,-49.5221601717595)) ;
#68862 = CARTESIAN_POINT('Ctrl Pts',(181.699518932262,585.592962618904,-49.5221601717596)) ;
#68863 = CARTESIAN_POINT('Ctrl Pts',(181.69355365263,585.661206408135,-49.5221601717596)) ;
#68864 = CARTESIAN_POINT('Ctrl Pts',(181.687589105054,585.72944182252,-49.5221601717596)) ;
#68865 = CARTESIAN_POINT('Ctrl Pts',(181.677834721031,585.797360538863,-49.5221601717599)) ;
#68866 = CARTESIAN_POINT('Ctrl Pts',(181.664361571398,585.864611794249,-49.5221601717597)) ;
#68867 = CARTESIAN_POINT('Ctrl Pts',(181.654511676375,585.913777566451,-49.5221601717596)) ;
#68868 = CARTESIAN_POINT('Ctrl Pts',(181.642673152834,585.962586345324,-49.5221601717598)) ;
#68869 = CARTESIAN_POINT('Ctrl Pts',(181.6288590601,586.010891074006,-49.5221601717596)) ;
#68870 = CARTESIAN_POINT('Ctrl Pts',(181.623146758882,586.03086568731,-49.5221601717596)) ;
#68871 = CARTESIAN_POINT('Ctrl Pts',(181.617096512571,586.050753989256,-49.5221601717595)) ;
#68872 = CARTESIAN_POINT('Ctrl Pts',(181.610708686729,586.07054500919,-49.5221601717596)) ;
#68873 = CARTESIAN_POINT('Ctrl Pts',(181.605967464192,586.085234456283,-49.5221601717597)) ;
#68874 = CARTESIAN_POINT('Ctrl Pts',(181.60104026166,586.099870303452,-49.5221601717596)) ;
#68875 = CARTESIAN_POINT('Ctrl Pts',(181.595927120135,586.114447926979,-49.5221601717595)) ;
#68876 = CARTESIAN_POINT('Ctrl Pts',(181.591624798445,586.126713894112,-49.5221601717595)) ;
#68877 = CARTESIAN_POINT('Ctrl Pts',(181.587193599639,586.138930667478,-49.5221601717596)) ;
#68878 = CARTESIAN_POINT('Ctrl Pts',(181.582635315551,586.151092329678,-49.5221601717596)) ;
#68879 = CARTESIAN_POINT('Ctrl Pts',(181.559525016203,586.212751420818,-49.5221601717596)) ;
#68880 = CARTESIAN_POINT('Ctrl Pts',(181.533140942791,586.273025515692,-49.5221601717595)) ;
#68881 = CARTESIAN_POINT('Ctrl Pts',(181.503533287679,586.331582535562,-49.5221601717596)) ;
#68882 = CARTESIAN_POINT('Ctrl Pts',(181.482570051262,586.373042916223,-49.5221601717597)) ;
#68883 = CARTESIAN_POINT('Ctrl Pts',(181.459989934264,586.413641981649,-49.5221601717594)) ;
#68884 = CARTESIAN_POINT('Ctrl Pts',(181.435800104679,586.453250265223,-49.5221601717596)) ;
#68885 = CARTESIAN_POINT('Ctrl Pts',(181.428072880055,586.465902777017,-49.5221601717596)) ;
#68886 = CARTESIAN_POINT('Ctrl Pts',(181.420180103468,586.478455995157,-49.5221601717599)) ;
#68887 = CARTESIAN_POINT('Ctrl Pts',(181.41212580138,586.490899350876,-49.5221601717598)) ;
#68888 = CARTESIAN_POINT('Ctrl Pts',(181.377861739762,586.543835024558,-49.5221601717596)) ;
#68889 = CARTESIAN_POINT('Ctrl Pts',(181.340741511594,586.594687784843,-49.5221601717595)) ;
#68890 = CARTESIAN_POINT('Ctrl Pts',(181.300799349475,586.643144100953,-49.5221601717596)) ;
#68891 = CARTESIAN_POINT('Ctrl Pts',(181.263590552905,586.688284401652,-49.5221601717596)) ;
#68892 = CARTESIAN_POINT('Ctrl Pts',(181.223932268822,586.731345188883,-49.5221601717599)) ;
#68893 = CARTESIAN_POINT('Ctrl Pts',(181.181829923378,586.772038827239,-49.5221601717597)) ;
#68894 = CARTESIAN_POINT('Ctrl Pts',(181.174641042286,586.778987174755,-49.5221601717596)) ;
#68895 = CARTESIAN_POINT('Ctrl Pts',(181.16738085938,586.785866419088,-49.5221601717594)) ;
#68896 = CARTESIAN_POINT('Ctrl Pts',(181.160050608476,586.792676042491,-49.5221601717598)) ;
#68897 = CARTESIAN_POINT('Ctrl Pts',(181.157212958645,586.790376961384,-49.5230454887661)) ;
#68898 = CARTESIAN_POINT('Ctrl Pts',(181.15218800891,586.796280842063,-49.5227503830974)) ;
#68899 = CARTESIAN_POINT('Ctrl Pts',(181.147121847573,586.802149646446,-49.5224552774286)) ;
#68900 = CARTESIAN_POINT('Ctrl Pts',(181.142014968315,586.807982802636,-49.5221601717599)) ;
#68901 = CARTESIAN_POINT('Ctrl Pts',(180.419233204836,583.719736168872,-49.5189770331172)) ;
#68902 = CARTESIAN_POINT('Ctrl Pts',(181.082048866651,583.896399029745,-49.4818859761884)) ;
#68903 = CARTESIAN_POINT('Ctrl Pts',(182.205022110371,584.964384226175,-49.4077208373071)) ;
#68904 = CARTESIAN_POINT('Ctrl Pts',(181.773244511485,587.256847446489,-49.2964816164732)) ;
#68905 = CARTESIAN_POINT('Ctrl Pts',(179.609919830324,588.131303024858,-49.1852593706157)) ;
#68906 = CARTESIAN_POINT('Ctrl Pts',(177.703480010983,586.788368782476,-49.0740371247583)) ;
#68907 = CARTESIAN_POINT('Ctrl Pts',(177.798971922146,584.457519353846,-48.9628148789009)) ;
#68908 = CARTESIAN_POINT('Ctrl Pts',(179.810018459729,583.275506361501,-48.8515926330436)) ;
#68909 = CARTESIAN_POINT('Ctrl Pts',(181.892849241664,584.325438807312,-48.7403703871863)) ;
#68910 = CARTESIAN_POINT('Ctrl Pts',(182.138609898212,586.645025743417,-48.629148141329)) ;
#68911 = CARTESIAN_POINT('Ctrl Pts',(180.321944045418,588.108107728139,-48.5179258954715)) ;
#68912 = CARTESIAN_POINT('Ctrl Pts',(178.108023948598,587.373654057886,-48.406703649614)) ;
#68913 = CARTESIAN_POINT('Ctrl Pts',(177.52607497017,585.114849113815,-48.2954814037566)) ;
#68914 = CARTESIAN_POINT('Ctrl Pts',(179.109499392003,583.402058754468,-48.1842591578995)) ;
#68915 = CARTESIAN_POINT('Ctrl Pts',(181.406959449108,583.805244989922,-48.0730369120422)) ;
#68916 = CARTESIAN_POINT('Ctrl Pts',(182.312583535423,585.954753589864,-47.9618146661847)) ;
#68917 = CARTESIAN_POINT('Ctrl Pts',(180.996335289573,587.880617927167,-47.8505924203273)) ;
#68918 = CARTESIAN_POINT('Ctrl Pts',(178.664394818812,587.817124582104,-47.7393701744699)) ;
#68919 = CARTESIAN_POINT('Ctrl Pts',(177.454434725336,585.823639759907,-47.6281479286125)) ;
#68920 = CARTESIAN_POINT('Ctrl Pts',(178.474212119244,583.724901972206,-47.5169256827551)) ;
#68921 = CARTESIAN_POINT('Ctrl Pts',(180.790706847517,583.45028245465,-47.4056890764861)) ;
#68922 = CARTESIAN_POINT('Ctrl Pts',(181.779706210552,584.643301812666,-47.3315265521695)) ;
#68923 = CARTESIAN_POINT('Ctrl Pts',(181.91085375533,585.316553064795,-47.2944381098053)) ;
#68924 = CARTESIAN_POINT('Ctrl Pts',(180.385086629763,583.847829775303,-49.5955145204618)) ;
#68925 = CARTESIAN_POINT('Ctrl Pts',(181.005255510324,584.013125822117,-49.5584234635329)) ;
#68926 = CARTESIAN_POINT('Ctrl Pts',(182.055974585899,585.012394882708,-49.4842583246516)) ;
#68927 = CARTESIAN_POINT('Ctrl Pts',(181.651978353492,587.157356794404,-49.3730191038177)) ;
#68928 = CARTESIAN_POINT('Ctrl Pts',(179.627845969337,587.975548289235,-49.2617968579602)) ;
#68929 = CARTESIAN_POINT('Ctrl Pts',(177.844070001549,586.719020911042,-49.1505746121029)) ;
#68930 = CARTESIAN_POINT('Ctrl Pts',(177.933417787156,584.538142630417,-49.0393523662454)) ;
#68931 = CARTESIAN_POINT('Ctrl Pts',(179.815069884142,583.432182532455,-48.9281301203881)) ;
#68932 = CARTESIAN_POINT('Ctrl Pts',(181.763887494898,584.414560389673,-48.8169078745308)) ;
#68933 = CARTESIAN_POINT('Ctrl Pts',(181.993835457868,586.584900827298,-48.7056856286735)) ;
#68934 = CARTESIAN_POINT('Ctrl Pts',(180.294057234166,587.953845420656,-48.594463382816)) ;
#68935 = CARTESIAN_POINT('Ctrl Pts',(178.222584836642,587.266647853149,-48.4832411369586)) ;
#68936 = CARTESIAN_POINT('Ctrl Pts',(177.67807952802,585.153178582169,-48.3720188911011)) ;
#68937 = CARTESIAN_POINT('Ctrl Pts',(179.159623504295,583.550592311223,-48.2607966452439)) ;
#68938 = CARTESIAN_POINT('Ctrl Pts',(181.309260747095,583.927836801213,-48.1495743993865)) ;
#68939 = CARTESIAN_POINT('Ctrl Pts',(182.156615310626,585.939042056281,-48.0383521535292)) ;
#68940 = CARTESIAN_POINT('Ctrl Pts',(180.925056902766,587.740992732744,-47.9271299076718)) ;
#68941 = CARTESIAN_POINT('Ctrl Pts',(178.743157779671,587.681584666521,-47.8159076618144)) ;
#68942 = CARTESIAN_POINT('Ctrl Pts',(177.611048748572,585.816364331787,-47.7046854159569)) ;
#68943 = CARTESIAN_POINT('Ctrl Pts',(178.565211785502,583.85266320133,-47.5934631700996)) ;
#68944 = CARTESIAN_POINT('Ctrl Pts',(180.732658973646,583.595713209658,-47.4822265638306)) ;
#68945 = CARTESIAN_POINT('Ctrl Pts',(181.658024294933,584.711971503438,-47.408064039514)) ;
#68946 = CARTESIAN_POINT('Ctrl Pts',(181.780733564974,585.341904529203,-47.3709755971498)) ;
#68947 = CARTESIAN_POINT('Ctrl Pts',(180.35094005469,583.975923381734,-49.6720520078063)) ;
#68948 = CARTESIAN_POINT('Ctrl Pts',(180.928462153998,584.12985261449,-49.6349609508773)) ;
#68949 = CARTESIAN_POINT('Ctrl Pts',(181.906927061425,585.060405539239,-49.5607958119961)) ;
#68950 = CARTESIAN_POINT('Ctrl Pts',(181.530712195499,587.05786614232,-49.4495565911623)) ;
#68951 = CARTESIAN_POINT('Ctrl Pts',(179.645772108348,587.819793553612,-49.3383343453048)) ;
#68952 = CARTESIAN_POINT('Ctrl Pts',(177.984659992115,586.64967303961,-49.2271120994473)) ;
#68953 = CARTESIAN_POINT('Ctrl Pts',(178.067863652165,584.61876590699,-49.11588985359)) ;
#68954 = CARTESIAN_POINT('Ctrl Pts',(179.820121308555,583.58885870341,-49.0046676077327)) ;
#68955 = CARTESIAN_POINT('Ctrl Pts',(181.634925748135,584.503681972034,-48.8934453618754)) ;
#68956 = CARTESIAN_POINT('Ctrl Pts',(181.849061017523,586.52477591118,-48.782223116018)) ;
#68957 = CARTESIAN_POINT('Ctrl Pts',(180.266170422915,587.799583113174,-48.6710008701606)) ;
#68958 = CARTESIAN_POINT('Ctrl Pts',(178.337145724684,587.159641648412,-48.5597786243031)) ;
#68959 = CARTESIAN_POINT('Ctrl Pts',(177.830084085871,585.191508050522,-48.4485563784457)) ;
#68960 = CARTESIAN_POINT('Ctrl Pts',(179.209747616584,583.699125867978,-48.3373341325884)) ;
#68961 = CARTESIAN_POINT('Ctrl Pts',(181.211562045081,584.050428612505,-48.2261118867311)) ;
#68962 = CARTESIAN_POINT('Ctrl Pts',(182.000647085828,585.923330522697,-48.1148896408738)) ;
#68963 = CARTESIAN_POINT('Ctrl Pts',(180.853778515959,587.601367538321,-48.0036673950164)) ;
#68964 = CARTESIAN_POINT('Ctrl Pts',(178.82192074053,587.546044750939,-47.8924451491589)) ;
#68965 = CARTESIAN_POINT('Ctrl Pts',(177.767662771809,585.809088903666,-47.7812229033014)) ;
#68966 = CARTESIAN_POINT('Ctrl Pts',(178.65621145176,583.980424430455,-47.6700006574441)) ;
#68967 = CARTESIAN_POINT('Ctrl Pts',(180.674611099775,583.741143964668,-47.5587640511751)) ;
#68968 = CARTESIAN_POINT('Ctrl Pts',(181.536342379315,584.780641194212,-47.4846015268585)) ;
#68969 = CARTESIAN_POINT('Ctrl Pts',(181.650613374619,585.367255993608,-47.4475130844944)) ;
#68970 = CARTESIAN_POINT('Ctrl Pts',(180.316793479617,584.104016988166,-49.7485894951507)) ;
#68971 = CARTESIAN_POINT('Ctrl Pts',(180.851668797671,584.246579406862,-49.7114984382218)) ;
#68972 = CARTESIAN_POINT('Ctrl Pts',(181.757879536953,585.108416195771,-49.6373332993405)) ;
#68973 = CARTESIAN_POINT('Ctrl Pts',(181.409446037507,586.958375490236,-49.5260940785067)) ;
#68974 = CARTESIAN_POINT('Ctrl Pts',(179.66369824736,587.664038817989,-49.4148718326492)) ;
#68975 = CARTESIAN_POINT('Ctrl Pts',(178.125249982681,586.580325168177,-49.3036495867918)) ;
#68976 = CARTESIAN_POINT('Ctrl Pts',(178.202309517176,584.699389183561,-49.1924273409344)) ;
#68977 = CARTESIAN_POINT('Ctrl Pts',(179.825172732969,583.745534874366,-49.0812050950771)) ;
#68978 = CARTESIAN_POINT('Ctrl Pts',(181.505964001371,584.592803554395,-48.9699828492198)) ;
#68979 = CARTESIAN_POINT('Ctrl Pts',(181.704286577179,586.464650995062,-48.8587606033624)) ;
#68980 = CARTESIAN_POINT('Ctrl Pts',(180.238283611663,587.645320805693,-48.747538357505)) ;
#68981 = CARTESIAN_POINT('Ctrl Pts',(178.451706612729,587.052635443676,-48.6363161116476)) ;
#68982 = CARTESIAN_POINT('Ctrl Pts',(177.982088643721,585.229837518876,-48.5250938657901)) ;
#68983 = CARTESIAN_POINT('Ctrl Pts',(179.259871728876,583.847659424733,-48.4138716199328)) ;
#68984 = CARTESIAN_POINT('Ctrl Pts',(181.113863343068,584.173020423797,-48.3026493740755)) ;
#68985 = CARTESIAN_POINT('Ctrl Pts',(181.844678861032,585.907618989114,-48.1914271282182)) ;
#68986 = CARTESIAN_POINT('Ctrl Pts',(180.782500129152,587.461742343898,-48.0802048823608)) ;
#68987 = CARTESIAN_POINT('Ctrl Pts',(178.90068370139,587.410504835355,-47.9689826365033)) ;
#68988 = CARTESIAN_POINT('Ctrl Pts',(177.924276795045,585.801813475545,-47.8577603906459)) ;
#68989 = CARTESIAN_POINT('Ctrl Pts',(178.747211118018,584.108185659579,-47.7465381447886)) ;
#68990 = CARTESIAN_POINT('Ctrl Pts',(180.616563225904,583.886574719676,-47.6353015385195)) ;
#68991 = CARTESIAN_POINT('Ctrl Pts',(181.414660463695,584.849310884986,-47.561139014203)) ;
#68992 = CARTESIAN_POINT('Ctrl Pts',(181.520493184263,585.392607458014,-47.5240505718387)) ;
#68993 = CARTESIAN_POINT('Ctrl Pts',(181.523656952667,585.391334705907,-47.52216017176)) ;
#68994 = CARTESIAN_POINT('Ctrl Pts',(181.518864111216,585.329612029403,-47.5221601717599)) ;
#68995 = CARTESIAN_POINT('Ctrl Pts',(181.510354110053,585.268421425887,-47.5221601717598)) ;
#68996 = CARTESIAN_POINT('Ctrl Pts',(181.498399921215,585.207975725837,-47.5221601717598)) ;
#68997 = CARTESIAN_POINT('Ctrl Pts',(181.485625550261,585.143382819915,-47.5221601717598)) ;
#68998 = CARTESIAN_POINT('Ctrl Pts',(181.468918454449,585.079639831897,-47.5221601717598)) ;
#68999 = CARTESIAN_POINT('Ctrl Pts',(181.448550450063,585.016994878175,-47.5221601717598)) ;
#69000 = CARTESIAN_POINT('Ctrl Pts',(181.430728446226,584.962180543669,-47.5221601717598)) ;
#69001 = CARTESIAN_POINT('Ctrl Pts',(181.410102435538,584.908206315245,-47.5221601717598)) ;
#69002 = CARTESIAN_POINT('Ctrl Pts',(181.386818394606,584.855239139212,-47.5221601717598)) ;
#69003 = CARTESIAN_POINT('Ctrl Pts',(181.375118389598,584.828623646365,-47.5221601717598)) ;
#69004 = CARTESIAN_POINT('Ctrl Pts',(181.36274673317,584.802262491287,-47.5221601717597)) ;
#69005 = CARTESIAN_POINT('Ctrl Pts',(181.349719011124,584.776177545999,-47.5221601717597)) ;
#69006 = CARTESIAN_POINT('Ctrl Pts',(181.343823711948,584.764373597778,-47.5221601717597)) ;
#69007 = CARTESIAN_POINT('Ctrl Pts',(181.337793201643,584.752624884227,-47.5221601717598)) ;
#69008 = CARTESIAN_POINT('Ctrl Pts',(181.331639037062,584.740952119149,-47.5221601717598)) ;
#69009 = CARTESIAN_POINT('Ctrl Pts',(181.300412762748,584.681724427155,-47.5221601717601)) ;
#69010 = CARTESIAN_POINT('Ctrl Pts',(181.265953645831,584.624341910917,-47.5221601717599)) ;
#69011 = CARTESIAN_POINT('Ctrl Pts',(181.22852965889,584.569045052016,-47.5221601717601)) ;
#69012 = CARTESIAN_POINT('Ctrl Pts',(181.19042442106,584.512741591806,-47.5221601717603)) ;
#69013 = CARTESIAN_POINT('Ctrl Pts',(181.14924507502,584.458599455405,-47.52216017176)) ;
#69014 = CARTESIAN_POINT('Ctrl Pts',(181.105221373277,584.406880458077,-47.52216017176)) ;
#69015 = CARTESIAN_POINT('Ctrl Pts',(181.068294032599,584.363498258075,-47.5221601717601)) ;
#69016 = CARTESIAN_POINT('Ctrl Pts',(181.029364334819,584.321820807193,-47.5221601717601)) ;
#69017 = CARTESIAN_POINT('Ctrl Pts',(180.988542561273,584.28201446558,-47.52216017176)) ;
#69018 = CARTESIAN_POINT('Ctrl Pts',(180.969684450482,584.263625445822,-47.5221601717599)) ;
#69019 = CARTESIAN_POINT('Ctrl Pts',(180.95042225226,584.24563593154,-47.5221601717597)) ;
#69020 = CARTESIAN_POINT('Ctrl Pts',(180.930765375998,584.228063505193,-47.5221601717599)) ;
#69021 = CARTESIAN_POINT('Ctrl Pts',(180.922295997763,584.220492234801,-47.5221601717599)) ;
#69022 = CARTESIAN_POINT('Ctrl Pts',(180.913753717785,584.212998855305,-47.52216017176)) ;
#69023 = CARTESIAN_POINT('Ctrl Pts',(180.905149669589,584.205593422028,-47.52216017176)) ;
#69024 = CARTESIAN_POINT('Ctrl Pts',(180.851912915241,584.159772986898,-47.5221601717599)) ;
#69025 = CARTESIAN_POINT('Ctrl Pts',(180.796216600555,584.117228680269,-47.5221601717599)) ;
#69026 = CARTESIAN_POINT('Ctrl Pts',(180.738312458319,584.078227871123,-47.5221601717597)) ;
#69027 = CARTESIAN_POINT('Ctrl Pts',(180.68624332931,584.043157182146,-47.5221601717596)) ;
#69028 = CARTESIAN_POINT('Ctrl Pts',(180.632387955704,584.010951462255,-47.5221601717599)) ;
#69029 = CARTESIAN_POINT('Ctrl Pts',(180.576898639163,583.981823861986,-47.5221601717599)) ;
#69030 = CARTESIAN_POINT('Ctrl Pts',(180.516759270754,583.950255344068,-47.5221601717598)) ;
#69031 = CARTESIAN_POINT('Ctrl Pts',(180.45470061862,583.922301113456,-47.52216017176)) ;
#69032 = CARTESIAN_POINT('Ctrl Pts',(180.391040733099,583.897902595055,-47.5221601717598)) ;
#69033 = CARTESIAN_POINT('Ctrl Pts',(180.366741521824,583.888589591291,-47.5221601717597)) ;
#69034 = CARTESIAN_POINT('Ctrl Pts',(180.342208714014,583.879795102048,-47.5221601717597)) ;
#69035 = CARTESIAN_POINT('Ctrl Pts',(180.317459037939,583.871517581215,-47.5221601717597)) ;
#69036 = CARTESIAN_POINT('Ctrl Pts',(180.306558516397,583.867871905454,-47.5221601717597)) ;
#69037 = CARTESIAN_POINT('Ctrl Pts',(180.295616870051,583.864326925159,-47.5221601717597)) ;
#69038 = CARTESIAN_POINT('Ctrl Pts',(180.284647851826,583.860886128633,-47.5221601717597)) ;
#69039 = CARTESIAN_POINT('Ctrl Pts',(180.217882198215,583.839942866049,-47.5221601717599)) ;
#69040 = CARTESIAN_POINT('Ctrl Pts',(180.149986712694,583.822815707665,-47.5221601717597)) ;
#69041 = CARTESIAN_POINT('Ctrl Pts',(180.081325520431,583.809396313223,-47.5221601717599)) ;
#69042 = CARTESIAN_POINT('Ctrl Pts',(180.011091307362,583.795669481843,-47.52216017176)) ;
#69043 = CARTESIAN_POINT('Ctrl Pts',(179.940055072934,583.785821976791,-47.5221601717599)) ;
#69044 = CARTESIAN_POINT('Ctrl Pts',(179.868574627648,583.779784122078,-47.5221601717597)) ;
#69045 = CARTESIAN_POINT('Ctrl Pts',(179.814562564869,583.775221797564,-47.5221601717595)) ;
#69046 = CARTESIAN_POINT('Ctrl Pts',(179.760296108056,583.772835580708,-47.5221601717598)) ;
#69047 = CARTESIAN_POINT('Ctrl Pts',(179.70592257077,583.772613692646,-47.5221601717599)) ;
#69048 = CARTESIAN_POINT('Ctrl Pts',(179.672228443948,583.772476193324,-47.52216017176)) ;
#69049 = CARTESIAN_POINT('Ctrl Pts',(179.638493099144,583.773170112498,-47.5221601717597)) ;
#69050 = CARTESIAN_POINT('Ctrl Pts',(179.604751128406,583.774695759566,-47.5221601717598)) ;
#69051 = CARTESIAN_POINT('Ctrl Pts',(179.591849093273,583.775279126561,-47.5221601717598)) ;
#69052 = CARTESIAN_POINT('Ctrl Pts',(179.578943804841,583.775984275203,-47.52216017176)) ;
#69053 = CARTESIAN_POINT('Ctrl Pts',(179.566044644676,583.776810827873,-47.5221601717599)) ;
#69054 = CARTESIAN_POINT('Ctrl Pts',(179.489473938043,583.781717327302,-47.5221601717596)) ;
#69055 = CARTESIAN_POINT('Ctrl Pts',(179.413305930242,583.790883712635,-47.5221601717601)) ;
#69056 = CARTESIAN_POINT('Ctrl Pts',(179.337954124025,583.804242075326,-47.5221601717598)) ;
#69057 = CARTESIAN_POINT('Ctrl Pts',(179.281440269363,583.814260847344,-47.5221601717596)) ;
#69058 = CARTESIAN_POINT('Ctrl Pts',(179.22538486089,583.826638741016,-47.5221601717598)) ;
#69059 = CARTESIAN_POINT('Ctrl Pts',(179.16995895443,583.841368214518,-47.5221601717597)) ;
#69060 = CARTESIAN_POINT('Ctrl Pts',(179.150298717127,583.846592936365,-47.5221601717597)) ;
#69061 = CARTESIAN_POINT('Ctrl Pts',(179.130717683404,583.852113703417,-47.52216017176)) ;
#69062 = CARTESIAN_POINT('Ctrl Pts',(179.111223524679,583.857930736292,-47.5221601717599)) ;
#69063 = CARTESIAN_POINT('Ctrl Pts',(179.096457923615,583.862336773405,-47.5221601717599)) ;
#69064 = CARTESIAN_POINT('Ctrl Pts',(179.081747033544,583.866911400053,-47.5221601717598)) ;
#69065 = CARTESIAN_POINT('Ctrl Pts',(179.067101764441,583.871651813381,-47.5221601717598)) ;
#69066 = CARTESIAN_POINT('Ctrl Pts',(178.995451726963,583.894843657125,-47.5221601717601)) ;
#69067 = CARTESIAN_POINT('Ctrl Pts',(178.925316590381,583.922016092408,-47.5221601717601)) ;
#69068 = CARTESIAN_POINT('Ctrl Pts',(178.85707525169,583.953137102575,-47.52216017176)) ;
#69069 = CARTESIAN_POINT('Ctrl Pts',(178.801930877505,583.978285328893,-47.52216017176)) ;
#69070 = CARTESIAN_POINT('Ctrl Pts',(178.748022741564,584.006012880253,-47.5221601717596)) ;
#69071 = CARTESIAN_POINT('Ctrl Pts',(178.695554610711,584.036327495048,-47.5221601717598)) ;
#69072 = CARTESIAN_POINT('Ctrl Pts',(178.68521642417,584.042300609348,-47.5221601717598)) ;
#69073 = CARTESIAN_POINT('Ctrl Pts',(178.6749341666,584.048374232336,-47.5221601717599)) ;
#69074 = CARTESIAN_POINT('Ctrl Pts',(178.664708372347,584.054547023819,-47.5221601717602)) ;
#69075 = CARTESIAN_POINT('Ctrl Pts',(178.622424393781,586.788243831647,-49.5202697760045)) ;
#69076 = CARTESIAN_POINT('Ctrl Pts',(178.263643649736,586.36676060424,-49.4831813336731)) ;
#69077 = CARTESIAN_POINT('Ctrl Pts',(178.008551654752,585.142526919038,-49.4090188093893)) ;
#69078 = CARTESIAN_POINT('Ctrl Pts',(179.347336054222,583.819180735871,-49.2977822031531)) ;
#69079 = CARTESIAN_POINT('Ctrl Pts',(181.184558760889,584.231744443467,-49.1865599572958)) ;
#69080 = CARTESIAN_POINT('Ctrl Pts',(181.833504573659,585.99813274514,-49.0753377114385)) ;
#69081 = CARTESIAN_POINT('Ctrl Pts',(180.700270327141,587.501342130218,-48.9641154655811)) ;
#69082 = CARTESIAN_POINT('Ctrl Pts',(178.822950161505,587.362806835846,-48.8528932197236)) ;
#69083 = CARTESIAN_POINT('Ctrl Pts',(177.9224424202,585.7099277411,-48.7416709738662)) ;
#69084 = CARTESIAN_POINT('Ctrl Pts',(178.824009812191,584.057559465188,-48.6304487280089)) ;
#69085 = CARTESIAN_POINT('Ctrl Pts',(180.701324880746,583.920322366968,-48.5192264821516)) ;
#69086 = CARTESIAN_POINT('Ctrl Pts',(181.833643668398,585.423980393734,-48.4080042362942)) ;
#69087 = CARTESIAN_POINT('Ctrl Pts',(181.183111205273,587.190315812827,-48.2967819904368)) ;
#69088 = CARTESIAN_POINT('Ctrl Pts',(179.345988480579,587.600347497167,-48.1855597445794)) ;
#69089 = CARTESIAN_POINT('Ctrl Pts',(178.006171324865,586.278214874925,-48.0743374987219)) ;
#69090 = CARTESIAN_POINT('Ctrl Pts',(178.391706208018,584.435855966388,-47.9631152528646)) ;
#69091 = CARTESIAN_POINT('Ctrl Pts',(180.149298192699,583.761768844811,-47.8518930070073)) ;
#69092 = CARTESIAN_POINT('Ctrl Pts',(181.667918986456,584.874265675204,-47.74067076115)) ;
#69093 = CARTESIAN_POINT('Ctrl Pts',(181.555993617726,586.752757360581,-47.6294485152926)) ;
#69094 = CARTESIAN_POINT('Ctrl Pts',(179.915827865207,587.677664053704,-47.5182262694351)) ;
#69095 = CARTESIAN_POINT('Ctrl Pts',(178.252238680771,586.796655916462,-47.4069878500146)) ;
#69096 = CARTESIAN_POINT('Ctrl Pts',(178.143431118054,585.550825987599,-47.3328235125465)) ;
#69097 = CARTESIAN_POINT('Ctrl Pts',(178.365443895008,585.043763351793,-47.2957332570309)) ;
#69098 = CARTESIAN_POINT('Ctrl Pts',(178.52085580834,586.874696733313,-49.5972768795265)) ;
#69099 = CARTESIAN_POINT('Ctrl Pts',(178.133293167415,586.419401527445,-49.5601884371951)) ;
#69100 = CARTESIAN_POINT('Ctrl Pts',(177.857737333116,585.096958090823,-49.4860259129113)) ;
#69101 = CARTESIAN_POINT('Ctrl Pts',(179.303920903732,583.667451211978,-49.3747893066751)) ;
#69102 = CARTESIAN_POINT('Ctrl Pts',(181.288528204949,584.113111361584,-49.2635670608178)) ;
#69103 = CARTESIAN_POINT('Ctrl Pts',(181.989533365316,586.021201822019,-49.1523448149605)) ;
#69104 = CARTESIAN_POINT('Ctrl Pts',(180.765389470584,587.645000782295,-49.0411225691031)) ;
#69105 = CARTESIAN_POINT('Ctrl Pts',(178.737468035733,587.495351991384,-48.9299003232456)) ;
#69106 = CARTESIAN_POINT('Ctrl Pts',(177.764720294423,585.709876606414,-48.8186780773881)) ;
#69107 = CARTESIAN_POINT('Ctrl Pts',(178.738612693092,583.924953018886,-48.7074558315308)) ;
#69108 = CARTESIAN_POINT('Ctrl Pts',(180.766528621966,583.776706567251,-48.5962335856736)) ;
#69109 = CARTESIAN_POINT('Ctrl Pts',(181.989683618431,585.400990159884,-48.4850113398162)) ;
#69110 = CARTESIAN_POINT('Ctrl Pts',(181.286964524382,587.309023495424,-48.3737890939588)) ;
#69111 = CARTESIAN_POINT('Ctrl Pts',(179.302465225832,587.751948499301,-48.2625668481014)) ;
#69112 = CARTESIAN_POINT('Ctrl Pts',(177.855166049811,586.323752534949,-48.1513446022439)) ;
#69113 = CARTESIAN_POINT('Ctrl Pts',(178.271629084588,584.333596998508,-48.0401223563866)) ;
#69114 = CARTESIAN_POINT('Ctrl Pts',(180.170217575085,583.605433658112,-47.9289001105293)) ;
#69115 = CARTESIAN_POINT('Ctrl Pts',(181.810664268964,584.807176551974,-47.817677864672)) ;
#69116 = CARTESIAN_POINT('Ctrl Pts',(181.689760089429,586.836363487529,-47.7064556188146)) ;
#69117 = CARTESIAN_POINT('Ctrl Pts',(179.918017928915,587.835467498957,-47.5952333729571)) ;
#69118 = CARTESIAN_POINT('Ctrl Pts',(178.120973275767,586.883783647426,-47.4839949535366)) ;
#69119 = CARTESIAN_POINT('Ctrl Pts',(178.003437017037,585.538011486041,-47.4098306160686)) ;
#69120 = CARTESIAN_POINT('Ctrl Pts',(178.243259971819,584.990271571035,-47.3727403605529)) ;
#69121 = CARTESIAN_POINT('Ctrl Pts',(178.419287222901,586.961149634978,-49.6742839830486)) ;
#69122 = CARTESIAN_POINT('Ctrl Pts',(178.002942685092,586.472042450653,-49.6371955407171)) ;
#69123 = CARTESIAN_POINT('Ctrl Pts',(177.706923011481,585.051389262609,-49.5630330164334)) ;
#69124 = CARTESIAN_POINT('Ctrl Pts',(179.260505753241,583.515721688086,-49.4517964101971)) ;
#69125 = CARTESIAN_POINT('Ctrl Pts',(181.39249764901,583.994478279701,-49.3405741643399)) ;
#69126 = CARTESIAN_POINT('Ctrl Pts',(182.145562156973,586.044270898896,-49.2293519184826)) ;
#69127 = CARTESIAN_POINT('Ctrl Pts',(180.830508614027,587.788659434373,-49.1181296726251)) ;
#69128 = CARTESIAN_POINT('Ctrl Pts',(178.651985909963,587.627897146924,-49.0069074267677)) ;
#69129 = CARTESIAN_POINT('Ctrl Pts',(177.606998168646,585.70982547173,-48.8956851809102)) ;
#69130 = CARTESIAN_POINT('Ctrl Pts',(178.653215573992,583.792346572583,-48.7844629350528)) ;
#69131 = CARTESIAN_POINT('Ctrl Pts',(180.831732363186,583.633090767534,-48.6732406891957)) ;
#69132 = CARTESIAN_POINT('Ctrl Pts',(182.145723568463,585.377999926036,-48.5620184433382)) ;
#69133 = CARTESIAN_POINT('Ctrl Pts',(181.39081784349,587.427731178022,-48.4507961974808)) ;
#69134 = CARTESIAN_POINT('Ctrl Pts',(179.258941971085,587.903549501434,-48.3395739516234)) ;
#69135 = CARTESIAN_POINT('Ctrl Pts',(177.704160774758,586.369290194971,-48.228351705766)) ;
#69136 = CARTESIAN_POINT('Ctrl Pts',(178.151551961158,584.231338030628,-48.1171294599086)) ;
#69137 = CARTESIAN_POINT('Ctrl Pts',(180.191136957471,583.449098471413,-48.0059072140514)) ;
#69138 = CARTESIAN_POINT('Ctrl Pts',(181.953409551472,584.740087428744,-47.8946849681939)) ;
#69139 = CARTESIAN_POINT('Ctrl Pts',(181.823526561132,586.919969614479,-47.7834627223367)) ;
#69140 = CARTESIAN_POINT('Ctrl Pts',(179.920207992622,587.99327094421,-47.6722404764791)) ;
#69141 = CARTESIAN_POINT('Ctrl Pts',(177.989707870763,586.970911378389,-47.5610020570586)) ;
#69142 = CARTESIAN_POINT('Ctrl Pts',(177.863442916019,585.525196984482,-47.4868377195905)) ;
#69143 = CARTESIAN_POINT('Ctrl Pts',(178.12107604863,584.936779790278,-47.449747464075)) ;
#69144 = CARTESIAN_POINT('Ctrl Pts',(178.317718637461,587.047602536644,-49.7512910865705)) ;
#69145 = CARTESIAN_POINT('Ctrl Pts',(177.87259220277,586.52468337386,-49.7142026442391)) ;
#69146 = CARTESIAN_POINT('Ctrl Pts',(177.556108689845,585.005820434396,-49.6400401199553)) ;
#69147 = CARTESIAN_POINT('Ctrl Pts',(179.217090602751,583.363992164192,-49.5288035137192)) ;
#69148 = CARTESIAN_POINT('Ctrl Pts',(181.496467093069,583.875845197818,-49.4175812678619)) ;
#69149 = CARTESIAN_POINT('Ctrl Pts',(182.301590948631,586.067339975775,-49.3063590220046)) ;
#69150 = CARTESIAN_POINT('Ctrl Pts',(180.89562775747,587.932318086451,-49.1951367761471)) ;
#69151 = CARTESIAN_POINT('Ctrl Pts',(178.566503784192,587.760442302463,-49.0839145302897)) ;
#69152 = CARTESIAN_POINT('Ctrl Pts',(177.44927604287,585.709774337044,-48.9726922844322)) ;
#69153 = CARTESIAN_POINT('Ctrl Pts',(178.567818454894,583.65974012628,-48.8614700385749)) ;
#69154 = CARTESIAN_POINT('Ctrl Pts',(180.896936104404,583.489474967817,-48.7502477927177)) ;
#69155 = CARTESIAN_POINT('Ctrl Pts',(182.301763518496,585.355009692186,-48.6390255468602)) ;
#69156 = CARTESIAN_POINT('Ctrl Pts',(181.494671162598,587.546438860619,-48.5278033010028)) ;
#69157 = CARTESIAN_POINT('Ctrl Pts',(179.215418716338,588.055150503567,-48.4165810551454)) ;
#69158 = CARTESIAN_POINT('Ctrl Pts',(177.553155499703,586.414827854993,-48.305358809288)) ;
#69159 = CARTESIAN_POINT('Ctrl Pts',(178.031474837727,584.129079062749,-48.1941365634305)) ;
#69160 = CARTESIAN_POINT('Ctrl Pts',(180.212056339858,583.292763284713,-48.0829143175733)) ;
#69161 = CARTESIAN_POINT('Ctrl Pts',(182.096154833979,584.672998305515,-47.971692071716)) ;
#69162 = CARTESIAN_POINT('Ctrl Pts',(181.957293032835,587.003575741428,-47.8604698258587)) ;
#69163 = CARTESIAN_POINT('Ctrl Pts',(179.922398056331,588.151074389465,-47.7492475800012)) ;
#69164 = CARTESIAN_POINT('Ctrl Pts',(177.858442465759,587.058039109354,-47.6380091605806)) ;
#69165 = CARTESIAN_POINT('Ctrl Pts',(177.723448815003,585.512382482924,-47.5638448231125)) ;
#69166 = CARTESIAN_POINT('Ctrl Pts',(177.998892125441,584.883288009522,-47.526754567597)) ;
#69167 = CARTESIAN_POINT('',(179.941804423115,587.377540552573,-47.5212748618547)) ;
#69168 = CARTESIAN_POINT('Ctrl Pts',(178.005900115752,584.887332980433,-47.5221601717599)) ;
#69169 = CARTESIAN_POINT('Ctrl Pts',(177.982987728062,584.956801876012,-47.52216017176)) ;
#69170 = CARTESIAN_POINT('Ctrl Pts',(177.964186437101,585.027371840573,-47.52216017176)) ;
#69171 = CARTESIAN_POINT('Ctrl Pts',(177.94938117184,585.098710895595,-47.5221601717598)) ;
#69172 = CARTESIAN_POINT('Ctrl Pts',(177.934151259053,585.172096111404,-47.5221601717596)) ;
#69173 = CARTESIAN_POINT('Ctrl Pts',(177.923149945878,585.246296203004,-47.52216017176)) ;
#69174 = CARTESIAN_POINT('Ctrl Pts',(177.916306443315,585.320953332826,-47.5221601717598)) ;
#69175 = CARTESIAN_POINT('Ctrl Pts',(177.910516709373,585.384114691281,-47.5221601717596)) ;
#69176 = CARTESIAN_POINT('Ctrl Pts',(177.907703953494,585.447603574384,-47.5221601717599)) ;
#69177 = CARTESIAN_POINT('Ctrl Pts',(177.907853704318,585.511196748025,-47.5221601717599)) ;
#69178 = CARTESIAN_POINT('Ctrl Pts',(177.907920121497,585.539401462535,-47.5221601717599)) ;
#69179 = CARTESIAN_POINT('Ctrl Pts',(177.908569617401,585.567626566114,-47.52216017176)) ;
#69180 = CARTESIAN_POINT('Ctrl Pts',(177.909802459868,585.595851820656,-47.52216017176)) ;
#69181 = CARTESIAN_POINT('Ctrl Pts',(177.910477882035,585.611315242044,-47.52216017176)) ;
#69182 = CARTESIAN_POINT('Ctrl Pts',(177.911328410559,585.626778699084,-47.5221601717596)) ;
#69183 = CARTESIAN_POINT('Ctrl Pts',(177.912354204027,585.642238785753,-47.5221601717597)) ;
#69184 = CARTESIAN_POINT('Ctrl Pts',(177.913307752249,585.656610039442,-47.5221601717597)) ;
#69185 = CARTESIAN_POINT('Ctrl Pts',(177.914413050293,585.670980562236,-47.5221601717595)) ;
#69186 = CARTESIAN_POINT('Ctrl Pts',(177.915668003083,585.685325277191,-47.5221601717596)) ;
#69187 = CARTESIAN_POINT('Ctrl Pts',(177.922052454499,585.758302632532,-47.5221601717599)) ;
#69188 = CARTESIAN_POINT('Ctrl Pts',(177.932313012602,585.830738647026,-47.5221601717598)) ;
#69189 = CARTESIAN_POINT('Ctrl Pts',(177.946379870592,585.902298744286,-47.5221601717596)) ;
#69190 = CARTESIAN_POINT('Ctrl Pts',(177.96034122638,585.97332213691,-47.5221601717594)) ;
#69191 = CARTESIAN_POINT('Ctrl Pts',(177.978052380569,586.043483656018,-47.5221601717599)) ;
#69192 = CARTESIAN_POINT('Ctrl Pts',(177.999491975402,586.112436269997,-47.5221601717598)) ;
#69193 = CARTESIAN_POINT('Ctrl Pts',(178.017341563624,586.16984294097,-47.5221601717597)) ;
#69194 = CARTESIAN_POINT('Ctrl Pts',(178.037776407616,586.226411576796,-47.5221601717598)) ;
#69195 = CARTESIAN_POINT('Ctrl Pts',(178.060806550301,586.281924200616,-47.5221601717596)) ;
#69196 = CARTESIAN_POINT('Ctrl Pts',(178.070370467521,586.304977385573,-47.5221601717596)) ;
#69197 = CARTESIAN_POINT('Ctrl Pts',(178.080382189699,586.327848227021,-47.5221601717595)) ;
#69198 = CARTESIAN_POINT('Ctrl Pts',(178.090843385664,586.350520045651,-47.5221601717597)) ;
#69199 = CARTESIAN_POINT('Ctrl Pts',(178.095722128577,586.361093404073,-47.5221601717597)) ;
#69200 = CARTESIAN_POINT('Ctrl Pts',(178.100698638309,586.371623465901,-47.5221601717597)) ;
#69201 = CARTESIAN_POINT('Ctrl Pts',(178.105773123522,586.382108486179,-47.5221601717598)) ;
#69202 = CARTESIAN_POINT('Ctrl Pts',(178.111008892306,586.39292675435,-47.5221601717599)) ;
#69203 = CARTESIAN_POINT('Ctrl Pts',(178.116345294491,586.403689432172,-47.5221601717598)) ;
#69204 = CARTESIAN_POINT('Ctrl Pts',(178.121780289776,586.414391289583,-47.5221601717598)) ;
#69205 = CARTESIAN_POINT('Ctrl Pts',(178.152938853733,586.475744518271,-47.5221601717595)) ;
#69206 = CARTESIAN_POINT('Ctrl Pts',(178.187353534623,586.535140324373,-47.5221601717597)) ;
#69207 = CARTESIAN_POINT('Ctrl Pts',(178.225000903539,586.59227470075,-47.5221601717595)) ;
#69208 = CARTESIAN_POINT('Ctrl Pts',(178.259362859716,586.644423071108,-47.5221601717594)) ;
#69209 = CARTESIAN_POINT('Ctrl Pts',(178.296418553824,586.694687651655,-47.5221601717597)) ;
#69210 = CARTESIAN_POINT('Ctrl Pts',(178.336177414887,586.742810826234,-47.5221601717597)) ;
#69211 = CARTESIAN_POINT('Ctrl Pts',(178.382907364859,586.799371640113,-47.5221601717598)) ;
#69212 = CARTESIAN_POINT('Ctrl Pts',(178.433372350224,586.852975663353,-47.5221601717595)) ;
#69213 = CARTESIAN_POINT('Ctrl Pts',(178.487196201923,586.903418834412,-47.5221601717596)) ;
#69214 = CARTESIAN_POINT('Ctrl Pts',(178.499135731636,586.914608441262,-47.5221601717596)) ;
#69215 = CARTESIAN_POINT('Ctrl Pts',(178.5112406165,586.92564228244,-47.5221601717595)) ;
#69216 = CARTESIAN_POINT('Ctrl Pts',(178.523506853694,586.936517727807,-47.5221601717595)) ;
#69217 = CARTESIAN_POINT('Ctrl Pts',(178.535515310811,586.947164621165,-47.5221601717595)) ;
#69218 = CARTESIAN_POINT('Ctrl Pts',(178.547682554143,586.95766300766,-47.5221601717598)) ;
#69219 = CARTESIAN_POINT('Ctrl Pts',(178.559980710183,586.967990546505,-47.5221601717598)) ;
#69220 = CARTESIAN_POINT('Ctrl Pts',(178.612487888008,587.01208414207,-47.5221601717597)) ;
#69221 = CARTESIAN_POINT('Ctrl Pts',(178.667447598405,587.053131162542,-47.5221601717596)) ;
#69222 = CARTESIAN_POINT('Ctrl Pts',(178.72452203213,587.091016625585,-47.5221601717597)) ;
#69223 = CARTESIAN_POINT('Ctrl Pts',(178.781589461753,587.128897439372,-47.5221601717597)) ;
#69224 = CARTESIAN_POINT('Ctrl Pts',(178.840772211404,587.163617781791,-47.5221601717597)) ;
#69225 = CARTESIAN_POINT('Ctrl Pts',(178.901751731621,587.195014521141,-47.5221601717596)) ;
#69226 = CARTESIAN_POINT('Ctrl Pts',(178.946332389148,587.217967920568,-47.5221601717595)) ;
#69227 = CARTESIAN_POINT('Ctrl Pts',(178.991873827707,587.239143965964,-47.5221601717594)) ;
#69228 = CARTESIAN_POINT('Ctrl Pts',(179.038252931247,587.258461179061,-47.5221601717596)) ;
#69229 = CARTESIAN_POINT('Ctrl Pts',(179.057431274439,587.266449089866,-47.5221601717597)) ;
#69230 = CARTESIAN_POINT('Ctrl Pts',(179.076752842022,587.27411897031,-47.5221601717596)) ;
#69231 = CARTESIAN_POINT('Ctrl Pts',(179.09620882887,587.281464266111,-47.5221601717597)) ;
#69232 = CARTESIAN_POINT('Ctrl Pts',(179.110649603242,587.286916148875,-47.5221601717598)) ;
#69233 = CARTESIAN_POINT('Ctrl Pts',(179.125164428122,587.292189207664,-47.5221601717596)) ;
#69234 = CARTESIAN_POINT('Ctrl Pts',(179.139749662979,587.297280591696,-47.5221601717598)) ;
#69235 = CARTESIAN_POINT('Ctrl Pts',(179.152022037213,587.30156460706,-47.5221601717599)) ;
#69236 = CARTESIAN_POINT('Ctrl Pts',(179.164336303796,587.305717190402,-47.5221601717595)) ;
#69237 = CARTESIAN_POINT('Ctrl Pts',(179.176686719118,587.309736053194,-47.5221601717595)) ;
#69238 = CARTESIAN_POINT('Ctrl Pts',(179.239458582398,587.330162208845,-47.5221601717595)) ;
#69239 = CARTESIAN_POINT('Ctrl Pts',(179.30319355351,587.347148258287,-47.5221601717595)) ;
#69240 = CARTESIAN_POINT('Ctrl Pts',(179.367598526706,587.36052507701,-47.5221601717595)) ;
#69241 = CARTESIAN_POINT('Ctrl Pts',(179.412926408987,587.369939611855,-47.5221601717596)) ;
#69242 = CARTESIAN_POINT('Ctrl Pts',(179.458586283043,587.377565388163,-47.5221601717598)) ;
#69243 = CARTESIAN_POINT('Ctrl Pts',(179.50447356325,587.383328055194,-47.5221601717595)) ;
#69244 = CARTESIAN_POINT('Ctrl Pts',(179.519183541229,587.385175379872,-47.5221601717594)) ;
#69245 = CARTESIAN_POINT('Ctrl Pts',(179.533919108266,587.386831362232,-47.5221601717596)) ;
#69246 = CARTESIAN_POINT('Ctrl Pts',(179.548669490907,587.388292560769,-47.5221601717596)) ;
#69247 = CARTESIAN_POINT('Ctrl Pts',(179.611419560358,587.394508691691,-47.5221601717596)) ;
#69248 = CARTESIAN_POINT('Ctrl Pts',(179.674321933271,587.397193106461,-47.5221601717594)) ;
#69249 = CARTESIAN_POINT('Ctrl Pts',(179.737110137716,587.396177085949,-47.5221601717594)) ;
#69250 = CARTESIAN_POINT('Ctrl Pts',(179.795601551891,587.39523059485,-47.5221601717594)) ;
#69251 = CARTESIAN_POINT('Ctrl Pts',(179.853994367444,587.391072461822,-47.5221601717598)) ;
#69252 = CARTESIAN_POINT('Ctrl Pts',(179.912060318785,587.383527591442,-47.5221601717599)) ;
#69253 = CARTESIAN_POINT('Ctrl Pts',(179.921974949721,587.382239321749,-47.5221601717599)) ;
#69254 = CARTESIAN_POINT('Ctrl Pts',(179.931880009566,587.380852220923,-47.5221601717594)) ;
#69255 = CARTESIAN_POINT('Ctrl Pts',(179.941774324258,587.379366930793,-47.5221601717597)) ;
#69256 = CARTESIAN_POINT('Ctrl Pts',(179.941746076329,587.375714942532,-47.5212748618547)) ;
#69257 = CARTESIAN_POINT('Ctrl Pts',(179.949494858334,587.375467290232,-47.5215699651564)) ;
#69258 = CARTESIAN_POINT('Ctrl Pts',(179.95724191163,587.375165548564,-47.5218650684581)) ;
#69259 = CARTESIAN_POINT('Ctrl Pts',(179.964986481303,587.374809746934,-47.5221601717598)) ;
#69260 = CARTESIAN_POINT('Origin',(10.1385276254028,514.798278400837,-46.5221601717518)) ;
#69261 = CARTESIAN_POINT('',(7.38852762540283,516.385991641109,-47.5221601717519)) ;
#69262 = CARTESIAN_POINT('',(10.1385276254028,514.798278400837,-47.5221601717521)) ;
#69263 = CARTESIAN_POINT('',(88.274584783925,469.686404766948,-47.5221601717556)) ;
#69264 = CARTESIAN_POINT('',(7.38852762540283,516.385991641109,-46.5221601717517)) ;
#69265 = CARTESIAN_POINT('',(10.1385276254028,514.798278400837,-46.7721601717518)) ;
#69266 = CARTESIAN_POINT('Origin',(10.1385276254028,511.622851920294,-46.5221601717521)) ;
#69267 = CARTESIAN_POINT('',(10.1385276254028,511.622851920294,-47.5221601717521)) ;
#69268 = CARTESIAN_POINT('',(10.1385276254028,507.916708540412,-47.5221601717521)) ;
#69269 = CARTESIAN_POINT('',(10.1385276254028,511.622851920294,-46.7721601717521)) ;
#69270 = CARTESIAN_POINT('Origin',(7.38852762540283,516.385991641109,-46.5221601717517)) ;
#69271 = CARTESIAN_POINT('',(4.63852762540283,514.798278400837,-47.5221601717518)) ;
#69272 = CARTESIAN_POINT('',(81.6274704668795,559.247865274989,-47.5221601717553)) ;
#69273 = CARTESIAN_POINT('',(4.63852762540283,514.798278400837,-46.7721601717518)) ;
#69274 = CARTESIAN_POINT('Origin',(4.63852762540283,514.798278400837,-46.5221601717518)) ;
#69275 = CARTESIAN_POINT('',(4.63852762540283,511.622851920294,-47.5221601717518)) ;
#69276 = CARTESIAN_POINT('',(4.63852762540284,509.504421780684,-47.5221601717518)) ;
#69277 = CARTESIAN_POINT('',(4.63852762540283,511.622851920294,-46.7721601717521)) ;
#69278 = CARTESIAN_POINT('Origin',(4.63852762540283,511.622851920294,-46.5221601717521)) ;
#69279 = CARTESIAN_POINT('',(7.38852762540283,510.035138680023,-47.5221601717519)) ;
#69280 = CARTESIAN_POINT('',(84.149584783925,465.71712166627,-47.5221601717554)) ;
#69281 = CARTESIAN_POINT('',(7.38852762540283,510.035138680023,-46.5221601717522)) ;
#69282 = CARTESIAN_POINT('Origin',(7.38852762540283,510.035138680023,-46.5221601717522)) ;
#69283 = CARTESIAN_POINT('',(83.0024704668795,553.690868934038,-47.5221601717554)) ;
#69284 = CARTESIAN_POINT('Origin',(187.63852762542,609.798278400806,-46.5221601717598)) ;
#69285 = CARTESIAN_POINT('',(184.88852762542,611.385991641078,-47.52216017176)) ;
#69286 = CARTESIAN_POINT('',(187.63852762542,609.798278400806,-47.5221601717601)) ;
#69287 = CARTESIAN_POINT('',(219.780188123809,591.241282059859,-47.5221601717616)) ;
#69288 = CARTESIAN_POINT('',(184.88852762542,611.385991641078,-46.5221601717597)) ;
#69289 = CARTESIAN_POINT('',(187.63852762542,609.798278400806,-46.7721601717598)) ;
#69290 = CARTESIAN_POINT('Origin',(187.63852762542,606.622851920263,-46.5221601717601)) ;
#69291 = CARTESIAN_POINT('',(187.63852762542,606.622851920263,-47.5221601717601)) ;
#69292 = CARTESIAN_POINT('',(187.63852762542,555.416708540397,-47.5221601717601)) ;
#69293 = CARTESIAN_POINT('',(187.63852762542,606.622851920263,-46.7721601717601)) ;
#69294 = CARTESIAN_POINT('Origin',(184.88852762542,611.385991641078,-46.5221601717597)) ;
#69295 = CARTESIAN_POINT('',(182.13852762542,609.798278400806,-47.5221601717599)) ;
#69296 = CARTESIAN_POINT('',(171.996867127016,603.942987982023,-47.5221601717594)) ;
#69297 = CARTESIAN_POINT('',(182.13852762542,609.798278400806,-46.7721601717598)) ;
#69298 = CARTESIAN_POINT('Origin',(182.13852762542,609.798278400806,-46.5221601717598)) ;
#69299 = CARTESIAN_POINT('',(182.13852762542,606.622851920263,-47.5221601717599)) ;
#69300 = CARTESIAN_POINT('',(182.13852762542,557.004421780668,-47.5221601717599)) ;
#69301 = CARTESIAN_POINT('',(182.13852762542,606.622851920263,-46.7721601717601)) ;
#69302 = CARTESIAN_POINT('Origin',(182.13852762542,606.622851920263,-46.5221601717601)) ;
#69303 = CARTESIAN_POINT('',(184.88852762542,605.035138679992,-47.52216017176)) ;
#69304 = CARTESIAN_POINT('',(215.655188123809,587.271998959181,-47.5221601717614)) ;
#69305 = CARTESIAN_POINT('',(184.88852762542,605.035138679992,-46.5221601717602)) ;
#69306 = CARTESIAN_POINT('Origin',(184.88852762542,605.035138679992,-46.5221601717602)) ;
#69307 = CARTESIAN_POINT('',(173.371867127016,598.385991641073,-47.5221601717595)) ;
#69308 = CARTESIAN_POINT('Origin',(212.388527625401,504.21056516053,-47.5221601717613)) ;
#69309 = CARTESIAN_POINT('',(4.63852762541949,609.798278400837,-47.5221601717518)) ;
#69310 = CARTESIAN_POINT('',(7.38852762541949,611.385991641109,-47.5221601717519)) ;
#69311 = CARTESIAN_POINT('',(61.0593671270094,642.372865274985,-47.5221601717544)) ;
#69312 = CARTESIAN_POINT('',(10.1385276254195,609.798278400837,-47.5221601717521)) ;
#69313 = CARTESIAN_POINT('',(108.842688123816,552.811404766952,-47.5221601717566)) ;
#69314 = CARTESIAN_POINT('',(10.1385276254195,606.622851920294,-47.5221601717521)) ;
#69315 = CARTESIAN_POINT('',(10.1385276254195,555.416708540412,-47.5221601717521)) ;
#69316 = CARTESIAN_POINT('',(7.38852762541949,605.035138680023,-47.5221601717519)) ;
#69317 = CARTESIAN_POINT('',(62.4343671270094,636.815868934035,-47.5221601717544)) ;
#69318 = CARTESIAN_POINT('',(4.63852762541949,606.622851920294,-47.5221601717518)) ;
#69319 = CARTESIAN_POINT('',(104.717688123816,548.842121666274,-47.5221601717564)) ;
#69320 = CARTESIAN_POINT('',(4.63852762541951,557.004421780684,-47.5221601717518)) ;
#69321 = CARTESIAN_POINT('Origin',(10.1385276254195,609.798278400837,-46.5221601717518)) ;
#69322 = CARTESIAN_POINT('',(7.38852762541949,611.385991641109,-46.5221601717516)) ;
#69323 = CARTESIAN_POINT('',(10.1385276254195,609.798278400837,-46.7721601717518)) ;
#69324 = CARTESIAN_POINT('Origin',(10.1385276254195,606.622851920294,-46.522160171752)) ;
#69325 = CARTESIAN_POINT('',(10.1385276254195,606.622851920294,-46.772160171752)) ;
#69326 = CARTESIAN_POINT('Origin',(7.38852762541949,611.385991641109,-46.5221601717516)) ;
#69327 = CARTESIAN_POINT('',(4.63852762541949,609.798278400837,-46.7721601717518)) ;
#69328 = CARTESIAN_POINT('Origin',(4.63852762541949,609.798278400837,-46.5221601717518)) ;
#69329 = CARTESIAN_POINT('',(4.63852762541949,606.622851920294,-46.772160171752)) ;
#69330 = CARTESIAN_POINT('Origin',(4.63852762541949,606.622851920294,-46.522160171752)) ;
#69331 = CARTESIAN_POINT('',(7.38852762541949,605.035138680023,-46.5221601717522)) ;
#69332 = CARTESIAN_POINT('Origin',(7.38852762541949,605.035138680023,-46.5221601717522)) ;
#69333 = CARTESIAN_POINT('',(0.,0.,0.)) ;
#69334 = CARTESIAN_POINT('',(0.,0.,0.)) ;
#69335 = CARTESIAN_POINT('',(0.,0.,0.)) ;
#69336 = CARTESIAN_POINT('',(0.,0.,0.)) ;
#69337 = CARTESIAN_POINT('',(0.,0.,0.)) ;
#69338 = CARTESIAN_POINT('',(0.,0.,0.)) ;
#69339 = CARTESIAN_POINT('',(0.,0.,0.)) ;
#69340 = CARTESIAN_POINT('Origin',(194.588527625411,554.617826199637,-31.0221601717604)) ;
#69341 = CARTESIAN_POINT('',(194.588527625411,554.617826199637,-31.0221601717604)) ;
#69342 = CARTESIAN_POINT('',(194.58852762541,546.397107238503,-31.0221601717604)) ;
#69343 = CARTESIAN_POINT('',(194.588527625412,562.045191394428,-31.0221601717604)) ;
#69344 = CARTESIAN_POINT('',(197.588527625411,554.617826199637,-31.0221601717605)) ;
#69345 = CARTESIAN_POINT('',(194.588527625411,554.617826199637,-31.0221601717604)) ;
#69346 = CARTESIAN_POINT('',(197.58852762541,546.397107238503,-31.0221601717605)) ;
#69347 = CARTESIAN_POINT('',(197.588527625411,554.617826199637,-31.0221601717605)) ;
#69348 = CARTESIAN_POINT('',(194.58852762541,546.397107238503,-31.0221601717604)) ;
#69349 = CARTESIAN_POINT('Origin',(194.588527625411,554.617826199637,-41.5221601717604)) ;
#69350 = CARTESIAN_POINT('',(194.588527625411,554.617826199637,-41.5221601717604)) ;
#69351 = CARTESIAN_POINT('',(194.588527625411,554.617826199637,-37.7721601717604)) ;
#69352 = CARTESIAN_POINT('',(197.588527625411,554.617826199637,-41.5221601717605)) ;
#69353 = CARTESIAN_POINT('',(203.58852762541,554.617826199636,-41.5221601717608)) ;
#69354 = CARTESIAN_POINT('',(197.588527625411,554.617826199637,-41.5221601717605)) ;
#69355 = CARTESIAN_POINT('Origin',(194.58852762541,546.397107238503,-31.0221601717604)) ;
#69356 = CARTESIAN_POINT('',(194.588527625409,546.397107238503,-41.5221601717604)) ;
#69357 = CARTESIAN_POINT('',(194.58852762541,546.397107238503,-32.5221601717604)) ;
#69358 = CARTESIAN_POINT('',(197.588527625409,546.397107238503,-41.5221601717605)) ;
#69359 = CARTESIAN_POINT('',(197.58852762541,546.397107238503,-31.0221601717605)) ;
#69360 = CARTESIAN_POINT('',(203.588527625409,546.397107238502,-41.5221601717608)) ;
#69361 = CARTESIAN_POINT('Origin',(197.588527625413,569.472556589218,-34.0221601717605)) ;
#69362 = CARTESIAN_POINT('',(197.588527625409,547.972556589215,-41.5221601717605)) ;
#69363 = CARTESIAN_POINT('Origin',(194.588527625418,592.617826199638,-31.0221601717604)) ;
#69364 = CARTESIAN_POINT('',(194.588527625418,592.617826199638,-31.0221601717604)) ;
#69365 = CARTESIAN_POINT('',(194.588527625416,584.397107238503,-31.0221601717604)) ;
#69366 = CARTESIAN_POINT('',(194.588527625416,581.045191394428,-31.0221601717604)) ;
#69367 = CARTESIAN_POINT('',(197.588527625418,592.617826199637,-31.0221601717605)) ;
#69368 = CARTESIAN_POINT('',(194.588527625418,592.617826199638,-31.0221601717604)) ;
#69369 = CARTESIAN_POINT('',(197.588527625416,584.397107238503,-31.0221601717605)) ;
#69370 = CARTESIAN_POINT('',(197.588527625418,592.617826199637,-31.0221601717605)) ;
#69371 = CARTESIAN_POINT('',(194.588527625416,584.397107238503,-31.0221601717604)) ;
#69372 = CARTESIAN_POINT('Origin',(194.588527625417,592.617826199638,-41.5221601717604)) ;
#69373 = CARTESIAN_POINT('',(194.588527625417,592.617826199638,-41.5221601717604)) ;
#69374 = CARTESIAN_POINT('',(194.588527625417,592.617826199638,-37.7721601717604)) ;
#69375 = CARTESIAN_POINT('',(197.588527625417,592.617826199637,-41.5221601717605)) ;
#69376 = CARTESIAN_POINT('',(203.588527625417,592.617826199636,-41.5221601717608)) ;
#69377 = CARTESIAN_POINT('',(197.588527625417,592.617826199637,-41.5221601717605)) ;
#69378 = CARTESIAN_POINT('Origin',(194.588527625416,584.397107238503,-31.0221601717604)) ;
#69379 = CARTESIAN_POINT('',(194.588527625416,584.397107238503,-41.5221601717604)) ;
#69380 = CARTESIAN_POINT('',(194.588527625416,584.397107238503,-32.5221601717604)) ;
#69381 = CARTESIAN_POINT('',(197.588527625416,584.397107238503,-41.5221601717605)) ;
#69382 = CARTESIAN_POINT('',(197.588527625416,584.397107238503,-31.0221601717605)) ;
#69383 = CARTESIAN_POINT('',(203.588527625415,584.397107238502,-41.5221601717608)) ;
#69384 = CARTESIAN_POINT('Origin',(197.588527625414,569.472556589218,-34.0221601717605)) ;
#69385 = CARTESIAN_POINT('',(197.58852762541,547.972556589215,-41.5221601717605)) ;
#69386 = CARTESIAN_POINT('Origin',(194.588527625418,593.897107238503,-31.0221601717604)) ;
#69387 = CARTESIAN_POINT('',(194.588527625418,593.897107238503,-31.0221601717604)) ;
#69388 = CARTESIAN_POINT('',(194.588527625417,593.897107238503,-41.5221601717604)) ;
#69389 = CARTESIAN_POINT('',(194.588527625418,593.897107238503,-32.5221601717604)) ;
#69390 = CARTESIAN_POINT('',(197.588527625418,593.897107238503,-31.0221601717605)) ;
#69391 = CARTESIAN_POINT('',(194.588527625418,593.897107238503,-31.0221601717604)) ;
#69392 = CARTESIAN_POINT('',(197.588527625417,593.897107238503,-41.5221601717605)) ;
#69393 = CARTESIAN_POINT('',(197.588527625418,593.897107238503,-31.0221601717605)) ;
#69394 = CARTESIAN_POINT('',(203.588527625417,593.897107238502,-41.5221601717608)) ;
#69395 = CARTESIAN_POINT('Origin',(194.588527625419,602.117826199638,-31.0221601717604)) ;
#69396 = CARTESIAN_POINT('',(194.588527625419,602.117826199638,-31.0221601717604)) ;
#69397 = CARTESIAN_POINT('',(194.588527625417,585.795191394428,-31.0221601717604)) ;
#69398 = CARTESIAN_POINT('',(197.588527625419,602.117826199637,-31.0221601717605)) ;
#69399 = CARTESIAN_POINT('',(194.588527625419,602.117826199638,-31.0221601717604)) ;
#69400 = CARTESIAN_POINT('',(197.588527625419,602.117826199637,-31.0221601717605)) ;
#69401 = CARTESIAN_POINT('Origin',(194.588527625419,602.117826199638,-41.5221601717604)) ;
#69402 = CARTESIAN_POINT('',(194.588527625419,602.117826199638,-41.5221601717604)) ;
#69403 = CARTESIAN_POINT('',(194.588527625419,602.117826199638,-37.7721601717604)) ;
#69404 = CARTESIAN_POINT('',(197.588527625419,602.117826199637,-41.5221601717605)) ;
#69405 = CARTESIAN_POINT('',(203.588527625419,602.117826199636,-41.5221601717608)) ;
#69406 = CARTESIAN_POINT('',(197.588527625419,602.117826199637,-41.5221601717605)) ;
#69407 = CARTESIAN_POINT('Origin',(197.588527625414,569.472556589218,-34.0221601717605)) ;
#69408 = CARTESIAN_POINT('',(197.58852762541,547.972556589215,-41.5221601717605)) ;
#69409 = CARTESIAN_POINT('Origin',(194.588527625413,564.117826199637,-31.0221601717604)) ;
#69410 = CARTESIAN_POINT('',(194.588527625413,564.117826199637,-31.0221601717604)) ;
#69411 = CARTESIAN_POINT('',(194.588527625411,555.897107238503,-31.0221601717604)) ;
#69412 = CARTESIAN_POINT('',(194.588527625413,566.795191394428,-31.0221601717604)) ;
#69413 = CARTESIAN_POINT('',(197.588527625413,564.117826199637,-31.0221601717605)) ;
#69414 = CARTESIAN_POINT('',(194.588527625413,564.117826199637,-31.0221601717604)) ;
#69415 = CARTESIAN_POINT('',(197.588527625411,555.897107238503,-31.0221601717605)) ;
#69416 = CARTESIAN_POINT('',(197.588527625413,564.117826199637,-31.0221601717605)) ;
#69417 = CARTESIAN_POINT('',(194.588527625411,555.897107238503,-31.0221601717604)) ;
#69418 = CARTESIAN_POINT('Origin',(194.588527625412,564.117826199637,-41.5221601717604)) ;
#69419 = CARTESIAN_POINT('',(194.588527625412,564.117826199637,-41.5221601717604)) ;
#69420 = CARTESIAN_POINT('',(194.588527625412,564.117826199637,-37.7721601717604)) ;
#69421 = CARTESIAN_POINT('',(197.588527625412,564.117826199637,-41.5221601717605)) ;
#69422 = CARTESIAN_POINT('',(203.588527625412,564.117826199636,-41.5221601717608)) ;
#69423 = CARTESIAN_POINT('',(197.588527625412,564.117826199637,-41.5221601717605)) ;
#69424 = CARTESIAN_POINT('Origin',(194.588527625411,555.897107238503,-31.0221601717604)) ;
#69425 = CARTESIAN_POINT('',(194.588527625411,555.897107238503,-41.5221601717604)) ;
#69426 = CARTESIAN_POINT('',(194.588527625411,555.897107238503,-32.5221601717604)) ;
#69427 = CARTESIAN_POINT('',(197.588527625411,555.897107238503,-41.5221601717605)) ;
#69428 = CARTESIAN_POINT('',(197.588527625411,555.897107238503,-31.0221601717605)) ;
#69429 = CARTESIAN_POINT('',(203.588527625411,555.897107238502,-41.5221601717608)) ;
#69430 = CARTESIAN_POINT('Origin',(197.588527625413,569.472556589218,-34.0221601717605)) ;
#69431 = CARTESIAN_POINT('',(197.58852762541,547.972556589215,-41.5221601717605)) ;
#69432 = CARTESIAN_POINT('Origin',(194.588527625409,545.117826199637,-31.0221601717604)) ;
#69433 = CARTESIAN_POINT('',(194.588527625409,545.117826199637,-31.0221601717604)) ;
#69434 = CARTESIAN_POINT('',(194.588527625408,536.897107238503,-31.0221601717604)) ;
#69435 = CARTESIAN_POINT('',(194.588527625412,557.295191394428,-31.0221601717604)) ;
#69436 = CARTESIAN_POINT('',(197.588527625409,545.117826199637,-31.0221601717605)) ;
#69437 = CARTESIAN_POINT('',(194.588527625409,545.117826199637,-31.0221601717604)) ;
#69438 = CARTESIAN_POINT('',(197.588527625408,536.897107238502,-31.0221601717605)) ;
#69439 = CARTESIAN_POINT('',(197.588527625409,545.117826199637,-31.0221601717605)) ;
#69440 = CARTESIAN_POINT('',(194.588527625408,536.897107238503,-31.0221601717604)) ;
#69441 = CARTESIAN_POINT('Origin',(194.588527625409,545.117826199637,-41.5221601717604)) ;
#69442 = CARTESIAN_POINT('',(194.588527625409,545.117826199637,-41.5221601717604)) ;
#69443 = CARTESIAN_POINT('',(194.588527625409,545.117826199637,-37.7721601717604)) ;
#69444 = CARTESIAN_POINT('',(197.588527625409,545.117826199637,-41.5221601717605)) ;
#69445 = CARTESIAN_POINT('',(203.588527625409,545.117826199636,-41.5221601717608)) ;
#69446 = CARTESIAN_POINT('',(197.588527625409,545.117826199637,-41.5221601717605)) ;
#69447 = CARTESIAN_POINT('Origin',(194.588527625408,536.897107238503,-31.0221601717604)) ;
#69448 = CARTESIAN_POINT('',(194.588527625408,536.897107238503,-41.5221601717604)) ;
#69449 = CARTESIAN_POINT('',(194.588527625408,536.897107238503,-32.5221601717604)) ;
#69450 = CARTESIAN_POINT('',(197.588527625408,536.897107238502,-41.5221601717605)) ;
#69451 = CARTESIAN_POINT('',(197.588527625408,536.897107238502,-31.0221601717605)) ;
#69452 = CARTESIAN_POINT('',(203.588527625407,536.897107238502,-41.5221601717608)) ;
#69453 = CARTESIAN_POINT('Origin',(197.588527625413,569.472556589218,-34.0221601717605)) ;
#69454 = CARTESIAN_POINT('',(197.588527625409,547.972556589215,-41.5221601717605)) ;
#69455 = CARTESIAN_POINT('Origin',(194.588527625416,583.117826199638,-31.0221601717604)) ;
#69456 = CARTESIAN_POINT('',(194.588527625416,583.117826199638,-31.0221601717604)) ;
#69457 = CARTESIAN_POINT('',(194.588527625415,574.897107238503,-31.0221601717604)) ;
#69458 = CARTESIAN_POINT('',(194.588527625415,576.295191394428,-31.0221601717604)) ;
#69459 = CARTESIAN_POINT('',(197.588527625416,583.117826199637,-31.0221601717605)) ;
#69460 = CARTESIAN_POINT('',(194.588527625416,583.117826199638,-31.0221601717604)) ;
#69461 = CARTESIAN_POINT('',(197.588527625415,574.897107238503,-31.0221601717605)) ;
#69462 = CARTESIAN_POINT('',(197.588527625416,583.117826199637,-31.0221601717605)) ;
#69463 = CARTESIAN_POINT('',(194.588527625415,574.897107238503,-31.0221601717604)) ;
#69464 = CARTESIAN_POINT('Origin',(194.588527625416,583.117826199638,-41.5221601717604)) ;
#69465 = CARTESIAN_POINT('',(194.588527625416,583.117826199638,-41.5221601717604)) ;
#69466 = CARTESIAN_POINT('',(194.588527625416,583.117826199638,-37.7721601717604)) ;
#69467 = CARTESIAN_POINT('',(197.588527625416,583.117826199637,-41.5221601717605)) ;
#69468 = CARTESIAN_POINT('',(203.588527625415,583.117826199636,-41.5221601717608)) ;
#69469 = CARTESIAN_POINT('',(197.588527625416,583.117826199637,-41.5221601717605)) ;
#69470 = CARTESIAN_POINT('Origin',(194.588527625415,574.897107238503,-31.0221601717604)) ;
#69471 = CARTESIAN_POINT('',(194.588527625414,574.897107238503,-41.5221601717604)) ;
#69472 = CARTESIAN_POINT('',(194.588527625415,574.897107238503,-32.5221601717604)) ;
#69473 = CARTESIAN_POINT('',(197.588527625414,574.897107238503,-41.5221601717605)) ;
#69474 = CARTESIAN_POINT('',(197.588527625415,574.897107238503,-31.0221601717605)) ;
#69475 = CARTESIAN_POINT('',(203.588527625414,574.897107238502,-41.5221601717608)) ;
#69476 = CARTESIAN_POINT('Origin',(197.588527625414,569.472556589218,-34.0221601717605)) ;
#69477 = CARTESIAN_POINT('',(197.58852762541,547.972556589215,-41.5221601717605)) ;
#69478 = CARTESIAN_POINT('Origin',(194.58852762542,603.397107238503,-31.0221601717604)) ;
#69479 = CARTESIAN_POINT('',(194.58852762542,603.397107238503,-31.0221601717604)) ;
#69480 = CARTESIAN_POINT('',(194.588527625419,603.397107238503,-41.5221601717604)) ;
#69481 = CARTESIAN_POINT('',(194.58852762542,603.397107238503,-32.5221601717604)) ;
#69482 = CARTESIAN_POINT('',(197.58852762542,603.397107238503,-31.0221601717605)) ;
#69483 = CARTESIAN_POINT('',(194.58852762542,603.397107238503,-31.0221601717604)) ;
#69484 = CARTESIAN_POINT('',(197.588527625419,603.397107238503,-41.5221601717605)) ;
#69485 = CARTESIAN_POINT('',(197.58852762542,603.397107238503,-31.0221601717605)) ;
#69486 = CARTESIAN_POINT('',(203.588527625419,603.397107238502,-41.5221601717608)) ;
#69487 = CARTESIAN_POINT('Origin',(194.588527625421,611.617826199638,-31.0221601717604)) ;
#69488 = CARTESIAN_POINT('',(194.588527625421,611.617826199638,-31.0221601717604)) ;
#69489 = CARTESIAN_POINT('',(194.588527625417,590.545191394428,-31.0221601717604)) ;
#69490 = CARTESIAN_POINT('',(197.588527625421,611.617826199637,-31.0221601717605)) ;
#69491 = CARTESIAN_POINT('',(194.588527625421,611.617826199638,-31.0221601717604)) ;
#69492 = CARTESIAN_POINT('',(197.588527625421,611.617826199637,-31.0221601717605)) ;
#69493 = CARTESIAN_POINT('Origin',(194.588527625421,611.617826199638,-41.5221601717604)) ;
#69494 = CARTESIAN_POINT('',(194.588527625421,611.617826199638,-41.5221601717604)) ;
#69495 = CARTESIAN_POINT('',(194.588527625421,611.617826199638,-37.7721601717604)) ;
#69496 = CARTESIAN_POINT('',(197.588527625421,611.617826199637,-41.5221601717605)) ;
#69497 = CARTESIAN_POINT('',(203.58852762542,611.617826199636,-41.5221601717608)) ;
#69498 = CARTESIAN_POINT('',(197.588527625421,611.617826199637,-41.5221601717605)) ;
#69499 = CARTESIAN_POINT('Origin',(197.588527625414,569.472556589218,-34.0221601717605)) ;
#69500 = CARTESIAN_POINT('',(197.58852762541,547.972556589215,-41.5221601717605)) ;
#69501 = CARTESIAN_POINT('Origin',(194.588527625414,573.617826199637,-31.0221601717604)) ;
#69502 = CARTESIAN_POINT('',(194.588527625414,573.617826199637,-31.0221601717604)) ;
#69503 = CARTESIAN_POINT('',(194.588527625413,565.397107238503,-31.0221601717604)) ;
#69504 = CARTESIAN_POINT('',(194.588527625414,571.545191394428,-31.0221601717604)) ;
#69505 = CARTESIAN_POINT('',(197.588527625414,573.617826199637,-31.0221601717605)) ;
#69506 = CARTESIAN_POINT('',(194.588527625414,573.617826199637,-31.0221601717604)) ;
#69507 = CARTESIAN_POINT('',(197.588527625413,565.397107238503,-31.0221601717605)) ;
#69508 = CARTESIAN_POINT('',(197.588527625414,573.617826199637,-31.0221601717605)) ;
#69509 = CARTESIAN_POINT('',(194.588527625413,565.397107238503,-31.0221601717604)) ;
#69510 = CARTESIAN_POINT('Origin',(194.588527625414,573.617826199637,-41.5221601717604)) ;
#69511 = CARTESIAN_POINT('',(194.588527625414,573.617826199637,-41.5221601717604)) ;
#69512 = CARTESIAN_POINT('',(194.588527625414,573.617826199637,-37.7721601717604)) ;
#69513 = CARTESIAN_POINT('',(197.588527625414,573.617826199637,-41.5221601717605)) ;
#69514 = CARTESIAN_POINT('',(203.588527625414,573.617826199636,-41.5221601717608)) ;
#69515 = CARTESIAN_POINT('',(197.588527625414,573.617826199637,-41.5221601717605)) ;
#69516 = CARTESIAN_POINT('Origin',(194.588527625413,565.397107238503,-31.0221601717604)) ;
#69517 = CARTESIAN_POINT('',(194.588527625413,565.397107238503,-41.5221601717604)) ;
#69518 = CARTESIAN_POINT('',(194.588527625413,565.397107238503,-32.5221601717604)) ;
#69519 = CARTESIAN_POINT('',(197.588527625413,565.397107238503,-41.5221601717605)) ;
#69520 = CARTESIAN_POINT('',(197.588527625413,565.397107238503,-31.0221601717605)) ;
#69521 = CARTESIAN_POINT('',(203.588527625412,565.397107238502,-41.5221601717608)) ;
#69522 = CARTESIAN_POINT('Origin',(197.588527625414,569.472556589218,-34.0221601717605)) ;
#69523 = CARTESIAN_POINT('',(197.58852762541,547.972556589215,-41.5221601717605)) ;
#69524 = CARTESIAN_POINT('Origin',(194.588527625408,535.617826199637,-31.0221601717604)) ;
#69525 = CARTESIAN_POINT('',(194.588527625408,535.617826199637,-31.0221601717604)) ;
#69526 = CARTESIAN_POINT('',(194.588527625406,527.397107238503,-31.0221601717604)) ;
#69527 = CARTESIAN_POINT('',(194.588527625411,552.545191394428,-31.0221601717604)) ;
#69528 = CARTESIAN_POINT('',(197.588527625408,535.617826199637,-31.0221601717605)) ;
#69529 = CARTESIAN_POINT('',(194.588527625408,535.617826199637,-31.0221601717604)) ;
#69530 = CARTESIAN_POINT('',(197.588527625406,527.397107238502,-31.0221601717605)) ;
#69531 = CARTESIAN_POINT('',(197.588527625408,535.617826199637,-31.0221601717605)) ;
#69532 = CARTESIAN_POINT('',(194.588527625406,527.397107238503,-31.0221601717604)) ;
#69533 = CARTESIAN_POINT('Origin',(194.588527625407,535.617826199637,-41.5221601717604)) ;
#69534 = CARTESIAN_POINT('',(194.588527625407,535.617826199637,-41.5221601717604)) ;
#69535 = CARTESIAN_POINT('',(194.588527625408,535.617826199637,-37.7721601717604)) ;
#69536 = CARTESIAN_POINT('',(197.588527625407,535.617826199637,-41.5221601717605)) ;
#69537 = CARTESIAN_POINT('',(203.588527625407,535.617826199636,-41.5221601717608)) ;
#69538 = CARTESIAN_POINT('',(197.588527625407,535.617826199637,-41.5221601717605)) ;
#69539 = CARTESIAN_POINT('Origin',(194.588527625406,527.397107238503,-31.0221601717604)) ;
#69540 = CARTESIAN_POINT('',(194.588527625406,527.397107238503,-41.5221601717604)) ;
#69541 = CARTESIAN_POINT('',(194.588527625406,527.397107238503,-32.5221601717604)) ;
#69542 = CARTESIAN_POINT('',(197.588527625406,527.397107238502,-41.5221601717605)) ;
#69543 = CARTESIAN_POINT('',(197.588527625406,527.397107238502,-31.0221601717605)) ;
#69544 = CARTESIAN_POINT('',(203.588527625406,527.397107238502,-41.5221601717608)) ;
#69545 = CARTESIAN_POINT('Origin',(197.588527625413,569.472556589218,-34.0221601717605)) ;
#69546 = CARTESIAN_POINT('',(197.588527625409,547.972556589215,-41.5221601717605)) ;
#69547 = CARTESIAN_POINT('Origin',(212.588527625406,526.47255658921,-41.5221601717612)) ;
#69548 = CARTESIAN_POINT('',(194.588527625421,613.010565160533,-41.5221601717604)) ;
#69549 = CARTESIAN_POINT('',(194.588527625421,613.010565160533,-41.5221601717604)) ;
#69550 = CARTESIAN_POINT('',(194.588527625421,613.010565160533,-41.5221601717604)) ;
#69551 = CARTESIAN_POINT('',(194.588527625421,613.010565160533,-41.5221601717604)) ;
#69552 = CARTESIAN_POINT('',(194.588527625421,613.010565160533,-41.5221601717604)) ;
#69553 = CARTESIAN_POINT('',(194.588527625421,613.010565160533,-41.5221601717604)) ;
#69554 = CARTESIAN_POINT('',(194.588527625421,613.010565160533,-41.5221601717604)) ;
#69555 = CARTESIAN_POINT('',(194.588527625421,613.010565160533,-41.5221601717604)) ;
#69556 = CARTESIAN_POINT('',(212.588527625421,613.01056516053,-41.5221601717612)) ;
#69557 = CARTESIAN_POINT('',(212.388527625421,613.01056516053,-41.5221601717612)) ;
#69558 = CARTESIAN_POINT('',(212.58852762542,611.54800593993,-41.5221601717612)) ;
#69559 = CARTESIAN_POINT('',(212.588527625421,613.01056516053,-41.5221601717612)) ;
#69560 = CARTESIAN_POINT('',(199.088527625421,611.548005939932,-41.5221601717606)) ;
#69561 = CARTESIAN_POINT('',(212.58852762542,611.548005939915,-41.5221601717612)) ;
#69562 = CARTESIAN_POINT('',(199.088527625419,603.397107238502,-41.5221601717606)) ;
#69563 = CARTESIAN_POINT('',(199.088527625421,613.010565160532,-41.5221601717606)) ;
#69564 = CARTESIAN_POINT('',(212.588527625419,603.3971072385,-41.5221601717612)) ;
#69565 = CARTESIAN_POINT('',(205.838527625419,603.397107238493,-41.5221601717609)) ;
#69566 = CARTESIAN_POINT('',(212.588527625419,602.04800593993,-41.5221601717612)) ;
#69567 = CARTESIAN_POINT('',(212.588527625421,613.01056516053,-41.5221601717612)) ;
#69568 = CARTESIAN_POINT('',(199.088527625419,602.048005939932,-41.5221601717606)) ;
#69569 = CARTESIAN_POINT('',(212.588527625419,602.048005939935,-41.5221601717612)) ;
#69570 = CARTESIAN_POINT('',(199.088527625417,593.897107238502,-41.5221601717606)) ;
#69571 = CARTESIAN_POINT('',(199.088527625421,613.010565160532,-41.5221601717606)) ;
#69572 = CARTESIAN_POINT('',(212.588527625417,593.8971072385,-41.5221601717612)) ;
#69573 = CARTESIAN_POINT('',(205.838527625417,593.897107238493,-41.5221601717609)) ;
#69574 = CARTESIAN_POINT('',(212.588527625417,592.54800593993,-41.5221601717612)) ;
#69575 = CARTESIAN_POINT('',(212.588527625421,613.01056516053,-41.5221601717612)) ;
#69576 = CARTESIAN_POINT('',(199.088527625417,592.548005939932,-41.5221601717606)) ;
#69577 = CARTESIAN_POINT('',(212.588527625417,592.548005939935,-41.5221601717612)) ;
#69578 = CARTESIAN_POINT('',(199.088527625416,584.397107238502,-41.5221601717606)) ;
#69579 = CARTESIAN_POINT('',(199.088527625421,613.010565160532,-41.5221601717606)) ;
#69580 = CARTESIAN_POINT('',(212.588527625416,584.3971072385,-41.5221601717612)) ;
#69581 = CARTESIAN_POINT('',(205.838527625416,584.397107238493,-41.5221601717609)) ;
#69582 = CARTESIAN_POINT('',(212.588527625416,583.04800593993,-41.5221601717612)) ;
#69583 = CARTESIAN_POINT('',(212.588527625421,613.01056516053,-41.5221601717612)) ;
#69584 = CARTESIAN_POINT('',(199.088527625416,583.048005939932,-41.5221601717606)) ;
#69585 = CARTESIAN_POINT('',(212.588527625416,583.048005939935,-41.5221601717612)) ;
#69586 = CARTESIAN_POINT('',(199.088527625414,574.897107238502,-41.5221601717606)) ;
#69587 = CARTESIAN_POINT('',(199.088527625421,613.010565160532,-41.5221601717606)) ;
#69588 = CARTESIAN_POINT('',(212.588527625414,574.8971072385,-41.5221601717612)) ;
#69589 = CARTESIAN_POINT('',(205.838527625414,574.897107238493,-41.5221601717609)) ;
#69590 = CARTESIAN_POINT('',(212.588527625414,573.54800593993,-41.5221601717612)) ;
#69591 = CARTESIAN_POINT('',(212.588527625421,613.01056516053,-41.5221601717612)) ;
#69592 = CARTESIAN_POINT('',(199.088527625414,573.548005939932,-41.5221601717606)) ;
#69593 = CARTESIAN_POINT('',(212.588527625414,573.548005939935,-41.5221601717612)) ;
#69594 = CARTESIAN_POINT('',(199.088527625412,565.397107238502,-41.5221601717606)) ;
#69595 = CARTESIAN_POINT('',(199.088527625421,613.010565160532,-41.5221601717606)) ;
#69596 = CARTESIAN_POINT('',(212.588527625412,565.3971072385,-41.5221601717612)) ;
#69597 = CARTESIAN_POINT('',(205.838527625412,565.397107238497,-41.5221601717609)) ;
#69598 = CARTESIAN_POINT('',(212.588527625412,564.04800593993,-41.5221601717612)) ;
#69599 = CARTESIAN_POINT('',(212.588527625421,613.01056516053,-41.5221601717612)) ;
#69600 = CARTESIAN_POINT('',(199.088527625412,564.048005939932,-41.5221601717606)) ;
#69601 = CARTESIAN_POINT('',(212.588527625412,564.048005939928,-41.5221601717612)) ;
#69602 = CARTESIAN_POINT('',(199.088527625411,555.897107238502,-41.5221601717606)) ;
#69603 = CARTESIAN_POINT('',(199.088527625421,613.010565160532,-41.5221601717606)) ;
#69604 = CARTESIAN_POINT('',(212.588527625411,555.8971072385,-41.5221601717612)) ;
#69605 = CARTESIAN_POINT('',(205.838527625411,555.897107238496,-41.5221601717609)) ;
#69606 = CARTESIAN_POINT('',(212.588527625411,554.54800593993,-41.5221601717612)) ;
#69607 = CARTESIAN_POINT('',(212.588527625421,613.01056516053,-41.5221601717612)) ;
#69608 = CARTESIAN_POINT('',(199.088527625411,554.548005939932,-41.5221601717606)) ;
#69609 = CARTESIAN_POINT('',(212.588527625411,554.548005939928,-41.5221601717612)) ;
#69610 = CARTESIAN_POINT('',(199.088527625409,546.397107238502,-41.5221601717606)) ;
#69611 = CARTESIAN_POINT('',(199.088527625421,613.010565160532,-41.5221601717606)) ;
#69612 = CARTESIAN_POINT('',(212.588527625409,546.3971072385,-41.5221601717612)) ;
#69613 = CARTESIAN_POINT('',(205.838527625409,546.397107238497,-41.5221601717609)) ;
#69614 = CARTESIAN_POINT('',(212.588527625409,545.04800593993,-41.5221601717612)) ;
#69615 = CARTESIAN_POINT('',(212.588527625421,613.01056516053,-41.5221601717612)) ;
#69616 = CARTESIAN_POINT('',(199.088527625409,545.048005939932,-41.5221601717606)) ;
#69617 = CARTESIAN_POINT('',(212.588527625409,545.048005939928,-41.5221601717612)) ;
#69618 = CARTESIAN_POINT('',(199.088527625407,536.897107238502,-41.5221601717606)) ;
#69619 = CARTESIAN_POINT('',(199.088527625421,613.010565160532,-41.5221601717606)) ;
#69620 = CARTESIAN_POINT('',(212.588527625407,536.8971072385,-41.5221601717612)) ;
#69621 = CARTESIAN_POINT('',(205.838527625407,536.897107238496,-41.5221601717609)) ;
#69622 = CARTESIAN_POINT('',(212.588527625407,535.54800593993,-41.5221601717612)) ;
#69623 = CARTESIAN_POINT('',(212.588527625421,613.01056516053,-41.5221601717612)) ;
#69624 = CARTESIAN_POINT('',(199.088527625407,535.548005939932,-41.5221601717606)) ;
#69625 = CARTESIAN_POINT('',(212.588527625407,535.548005939928,-41.5221601717612)) ;
#69626 = CARTESIAN_POINT('',(199.088527625406,527.397107238502,-41.5221601717606)) ;
#69627 = CARTESIAN_POINT('',(199.088527625421,613.010565160532,-41.5221601717606)) ;
#69628 = CARTESIAN_POINT('',(212.588527625406,527.3971072385,-41.5221601717612)) ;
#69629 = CARTESIAN_POINT('',(205.838527625406,527.397107238497,-41.5221601717609)) ;
#69630 = CARTESIAN_POINT('',(212.588527625406,525.9345480179,-41.5221601717612)) ;
#69631 = CARTESIAN_POINT('',(212.588527625421,613.01056516053,-41.5221601717612)) ;
#69632 = CARTESIAN_POINT('',(194.588527625405,525.934548017903,-41.5221601717604)) ;
#69633 = CARTESIAN_POINT('',(199.088527625405,525.934548017902,-41.5221601717606)) ;
#69634 = CARTESIAN_POINT('',(194.588527625421,613.010565160533,-41.5221601717604)) ;
#69635 = CARTESIAN_POINT('',(194.588527625421,613.010565160533,-41.5221601717604)) ;
#69636 = CARTESIAN_POINT('',(194.588527625421,613.010565160533,-41.5221601717604)) ;
#69637 = CARTESIAN_POINT('Origin',(206.038527625421,607.472556589211,-40.3971601717609)) ;
#69638 = CARTESIAN_POINT('',(207.538527625421,607.472556589211,-40.397160171761)) ;
#69639 = CARTESIAN_POINT('Origin',(206.038527625421,607.472556589211,-40.3971601717609)) ;
#69640 = CARTESIAN_POINT('',(207.663527625421,607.472556589211,-40.522160171761)) ;
#69641 = CARTESIAN_POINT('Origin',(207.663527625421,607.472556589211,-40.397160171761)) ;
#69642 = CARTESIAN_POINT('Origin',(206.038527625421,607.472556589211,-40.5221601717609)) ;
#69643 = CARTESIAN_POINT('Origin',(206.038527625421,607.472556589211,-29.1521601717606)) ;
#69644 = CARTESIAN_POINT('',(207.538527625421,607.472556589211,-37.0052690928546)) ;
#69645 = CARTESIAN_POINT('Origin',(206.038527625421,607.472556589211,-37.0052690928546)) ;
#69646 = CARTESIAN_POINT('',(207.538527625421,607.472556589211,-29.1521601717607)) ;
#69647 = CARTESIAN_POINT('Origin',(205.838527625413,569.472556589214,-40.5221601717609)) ;
#69648 = CARTESIAN_POINT('',(212.588527625419,603.3971072385,-40.5221601717612)) ;
#69649 = CARTESIAN_POINT('',(212.588527625421,611.54800593993,-40.5221601717612)) ;
#69650 = CARTESIAN_POINT('',(212.588527625409,547.972556589211,-40.5221601717612)) ;
#69651 = CARTESIAN_POINT('',(199.088527625419,603.397107238502,-40.5221601717606)) ;
#69652 = CARTESIAN_POINT('',(209.213527625419,603.397107238493,-40.5221601717611)) ;
#69653 = CARTESIAN_POINT('',(199.088527625421,611.548005939932,-40.5221601717606)) ;
#69654 = CARTESIAN_POINT('',(199.088527625409,547.972556589214,-40.5221601717606)) ;
#69655 = CARTESIAN_POINT('',(202.463527625421,611.548005939916,-40.5221601717608)) ;
#69656 = CARTESIAN_POINT('',(202.262277625404,608.357556589212,-40.5221601717608)) ;
#69657 = CARTESIAN_POINT('',(201.559777625404,608.357556589212,-40.5221601717607)) ;
#69658 = CARTESIAN_POINT('',(212.018652625407,608.357556589212,-40.5221601717612)) ;
#69659 = CARTESIAN_POINT('',(201.184777625404,607.982556589212,-40.5221601717607)) ;
#69660 = CARTESIAN_POINT('Origin',(201.559777625404,607.982556589212,-40.5221601717607)) ;
#69661 = CARTESIAN_POINT('',(201.184777625405,606.962556589212,-40.5221601717607)) ;
#69662 = CARTESIAN_POINT('',(201.184777625405,624.170681589212,-40.5221601717607)) ;
#69663 = CARTESIAN_POINT('',(201.559777625405,606.587556589212,-40.5221601717607)) ;
#69664 = CARTESIAN_POINT('Origin',(201.559777625404,606.962556589212,-40.5221601717607)) ;
#69665 = CARTESIAN_POINT('',(202.262277625404,606.587556589212,-40.5221601717608)) ;
#69666 = CARTESIAN_POINT('',(212.844152625407,606.587556589212,-40.5221601717612)) ;
#69667 = CARTESIAN_POINT('',(202.637277625404,606.962556589212,-40.5221601717608)) ;
#69668 = CARTESIAN_POINT('Origin',(202.262277625404,606.962556589212,-40.5221601717608)) ;
#69669 = CARTESIAN_POINT('',(202.637277625404,607.982556589212,-40.5221601717608)) ;
#69670 = CARTESIAN_POINT('',(202.637277625404,624.170681589213,-40.5221601717608)) ;
#69671 = CARTESIAN_POINT('Origin',(202.262277625404,607.982556589212,-40.5221601717608)) ;
#69672 = CARTESIAN_POINT('Origin',(206.038527625419,597.972556589211,-40.3971601717609)) ;
#69673 = CARTESIAN_POINT('',(207.538527625419,597.972556589211,-40.397160171761)) ;
#69674 = CARTESIAN_POINT('Origin',(206.038527625419,597.972556589211,-40.3971601717609)) ;
#69675 = CARTESIAN_POINT('',(207.663527625419,597.972556589211,-40.522160171761)) ;
#69676 = CARTESIAN_POINT('Origin',(207.663527625419,597.972556589211,-40.397160171761)) ;
#69677 = CARTESIAN_POINT('Origin',(206.038527625419,597.972556589211,-40.5221601717609)) ;
#69678 = CARTESIAN_POINT('Origin',(206.038527625419,597.972556589211,-29.1521601717606)) ;
#69679 = CARTESIAN_POINT('',(207.538527625419,597.972556589211,-37.0052690928546)) ;
#69680 = CARTESIAN_POINT('Origin',(206.038527625419,597.972556589211,-37.0052690928546)) ;
#69681 = CARTESIAN_POINT('',(207.538527625419,597.972556589211,-29.1521601717607)) ;
#69682 = CARTESIAN_POINT('Origin',(205.838527625413,569.472556589214,-40.5221601717609)) ;
#69683 = CARTESIAN_POINT('',(212.588527625417,593.8971072385,-40.5221601717612)) ;
#69684 = CARTESIAN_POINT('',(212.588527625419,602.04800593993,-40.5221601717612)) ;
#69685 = CARTESIAN_POINT('',(212.588527625409,547.972556589211,-40.5221601717612)) ;
#69686 = CARTESIAN_POINT('',(199.088527625417,593.897107238502,-40.5221601717606)) ;
#69687 = CARTESIAN_POINT('',(209.213527625417,593.897107238493,-40.5221601717611)) ;
#69688 = CARTESIAN_POINT('',(199.088527625419,602.048005939932,-40.5221601717606)) ;
#69689 = CARTESIAN_POINT('',(199.088527625409,547.972556589214,-40.5221601717606)) ;
#69690 = CARTESIAN_POINT('',(202.463527625419,602.048005939937,-40.5221601717608)) ;
#69691 = CARTESIAN_POINT('',(202.262277625404,598.857556589212,-40.5221601717608)) ;
#69692 = CARTESIAN_POINT('',(201.559777625405,598.857556589212,-40.5221601717607)) ;
#69693 = CARTESIAN_POINT('',(212.018652625407,598.857556589212,-40.5221601717612)) ;
#69694 = CARTESIAN_POINT('',(201.184777625405,598.482556589212,-40.5221601717607)) ;
#69695 = CARTESIAN_POINT('Origin',(201.559777625405,598.482556589212,-40.5221601717607)) ;
#69696 = CARTESIAN_POINT('',(201.184777625405,597.462556589212,-40.5221601717607)) ;
#69697 = CARTESIAN_POINT('',(201.184777625405,614.670681589212,-40.5221601717607)) ;
#69698 = CARTESIAN_POINT('',(201.559777625405,597.087556589212,-40.5221601717607)) ;
#69699 = CARTESIAN_POINT('Origin',(201.559777625405,597.462556589212,-40.5221601717607)) ;
#69700 = CARTESIAN_POINT('',(202.262277625404,597.087556589212,-40.5221601717608)) ;
#69701 = CARTESIAN_POINT('',(212.844152625407,597.087556589212,-40.5221601717612)) ;
#69702 = CARTESIAN_POINT('',(202.637277625404,597.462556589212,-40.5221601717608)) ;
#69703 = CARTESIAN_POINT('Origin',(202.262277625404,597.462556589212,-40.5221601717608)) ;
#69704 = CARTESIAN_POINT('',(202.637277625404,598.482556589212,-40.5221601717608)) ;
#69705 = CARTESIAN_POINT('',(202.637277625404,614.670681589213,-40.5221601717608)) ;
#69706 = CARTESIAN_POINT('Origin',(202.262277625404,598.482556589212,-40.5221601717608)) ;
#69707 = CARTESIAN_POINT('Origin',(206.038527625417,588.472556589211,-40.3971601717609)) ;
#69708 = CARTESIAN_POINT('',(207.538527625417,588.472556589211,-40.397160171761)) ;
#69709 = CARTESIAN_POINT('Origin',(206.038527625417,588.472556589211,-40.3971601717609)) ;
#69710 = CARTESIAN_POINT('',(207.663527625417,588.472556589211,-40.522160171761)) ;
#69711 = CARTESIAN_POINT('Origin',(207.663527625417,588.472556589211,-40.397160171761)) ;
#69712 = CARTESIAN_POINT('Origin',(206.038527625417,588.472556589211,-40.5221601717609)) ;
#69713 = CARTESIAN_POINT('Origin',(206.038527625418,588.472556589211,-29.1521601717607)) ;
#69714 = CARTESIAN_POINT('',(207.538527625417,588.472556589211,-37.0052690928546)) ;
#69715 = CARTESIAN_POINT('Origin',(206.038527625417,588.472556589211,-37.0052690928546)) ;
#69716 = CARTESIAN_POINT('',(207.538527625418,588.472556589211,-29.1521601717608)) ;
#69717 = CARTESIAN_POINT('Origin',(205.838527625413,569.472556589214,-40.5221601717609)) ;
#69718 = CARTESIAN_POINT('',(212.588527625416,584.3971072385,-40.5221601717612)) ;
#69719 = CARTESIAN_POINT('',(212.588527625417,592.54800593993,-40.5221601717612)) ;
#69720 = CARTESIAN_POINT('',(212.588527625409,547.972556589211,-40.5221601717612)) ;
#69721 = CARTESIAN_POINT('',(199.088527625416,584.397107238502,-40.5221601717606)) ;
#69722 = CARTESIAN_POINT('',(209.213527625416,584.397107238493,-40.5221601717611)) ;
#69723 = CARTESIAN_POINT('',(199.088527625417,592.548005939932,-40.5221601717606)) ;
#69724 = CARTESIAN_POINT('',(199.088527625409,547.972556589214,-40.5221601717606)) ;
#69725 = CARTESIAN_POINT('',(202.463527625417,592.548005939937,-40.5221601717608)) ;
#69726 = CARTESIAN_POINT('',(202.262277625405,589.357556589212,-40.5221601717608)) ;
#69727 = CARTESIAN_POINT('',(201.559777625405,589.357556589212,-40.5221601717607)) ;
#69728 = CARTESIAN_POINT('',(212.018652625408,589.357556589212,-40.5221601717612)) ;
#69729 = CARTESIAN_POINT('',(201.184777625405,588.982556589212,-40.5221601717607)) ;
#69730 = CARTESIAN_POINT('Origin',(201.559777625405,588.982556589212,-40.5221601717607)) ;
#69731 = CARTESIAN_POINT('',(201.184777625405,587.962556589212,-40.5221601717607)) ;
#69732 = CARTESIAN_POINT('',(201.184777625405,605.170681589212,-40.5221601717607)) ;
#69733 = CARTESIAN_POINT('',(201.559777625405,587.587556589212,-40.5221601717607)) ;
#69734 = CARTESIAN_POINT('Origin',(201.559777625405,587.962556589212,-40.5221601717607)) ;
#69735 = CARTESIAN_POINT('',(202.262277625405,587.587556589212,-40.5221601717608)) ;
#69736 = CARTESIAN_POINT('',(212.844152625407,587.587556589212,-40.5221601717612)) ;
#69737 = CARTESIAN_POINT('',(202.637277625405,587.962556589212,-40.5221601717608)) ;
#69738 = CARTESIAN_POINT('Origin',(202.262277625405,587.962556589212,-40.5221601717608)) ;
#69739 = CARTESIAN_POINT('',(202.637277625405,588.982556589212,-40.5221601717608)) ;
#69740 = CARTESIAN_POINT('',(202.637277625405,605.170681589213,-40.5221601717608)) ;
#69741 = CARTESIAN_POINT('Origin',(202.262277625405,588.982556589212,-40.5221601717608)) ;
#69742 = CARTESIAN_POINT('Origin',(206.038527625415,578.972556589211,-40.3971601717609)) ;
#69743 = CARTESIAN_POINT('',(207.538527625415,578.972556589211,-40.397160171761)) ;
#69744 = CARTESIAN_POINT('Origin',(206.038527625415,578.972556589211,-40.3971601717609)) ;
#69745 = CARTESIAN_POINT('',(207.663527625415,578.972556589211,-40.522160171761)) ;
#69746 = CARTESIAN_POINT('Origin',(207.663527625415,578.972556589211,-40.397160171761)) ;
#69747 = CARTESIAN_POINT('Origin',(206.038527625415,578.972556589211,-40.5221601717609)) ;
#69748 = CARTESIAN_POINT('Origin',(206.038527625416,578.972556589211,-29.1521601717607)) ;
#69749 = CARTESIAN_POINT('',(207.538527625416,578.972556589211,-37.0052690928546)) ;
#69750 = CARTESIAN_POINT('Origin',(206.038527625416,578.972556589211,-37.0052690928546)) ;
#69751 = CARTESIAN_POINT('',(207.538527625416,578.972556589211,-29.1521601717608)) ;
#69752 = CARTESIAN_POINT('Origin',(205.838527625413,569.472556589214,-40.5221601717609)) ;
#69753 = CARTESIAN_POINT('',(212.588527625414,574.8971072385,-40.5221601717612)) ;
#69754 = CARTESIAN_POINT('',(212.588527625416,583.04800593993,-40.5221601717612)) ;
#69755 = CARTESIAN_POINT('',(212.588527625409,547.972556589211,-40.5221601717612)) ;
#69756 = CARTESIAN_POINT('',(199.088527625414,574.897107238502,-40.5221601717606)) ;
#69757 = CARTESIAN_POINT('',(209.213527625414,574.897107238493,-40.5221601717611)) ;
#69758 = CARTESIAN_POINT('',(199.088527625416,583.048005939932,-40.5221601717606)) ;
#69759 = CARTESIAN_POINT('',(199.088527625409,547.972556589214,-40.5221601717606)) ;
#69760 = CARTESIAN_POINT('',(202.463527625416,583.048005939937,-40.5221601717608)) ;
#69761 = CARTESIAN_POINT('',(202.262277625405,579.857556589212,-40.5221601717608)) ;
#69762 = CARTESIAN_POINT('',(201.559777625405,579.857556589212,-40.5221601717607)) ;
#69763 = CARTESIAN_POINT('',(212.018652625408,579.857556589212,-40.5221601717612)) ;
#69764 = CARTESIAN_POINT('',(201.184777625405,579.482556589212,-40.5221601717607)) ;
#69765 = CARTESIAN_POINT('Origin',(201.559777625405,579.482556589212,-40.5221601717607)) ;
#69766 = CARTESIAN_POINT('',(201.184777625406,578.462556589212,-40.5221601717607)) ;
#69767 = CARTESIAN_POINT('',(201.184777625406,595.670681589212,-40.5221601717607)) ;
#69768 = CARTESIAN_POINT('',(201.559777625406,578.087556589212,-40.5221601717607)) ;
#69769 = CARTESIAN_POINT('Origin',(201.559777625405,578.462556589212,-40.5221601717607)) ;
#69770 = CARTESIAN_POINT('',(202.262277625405,578.087556589212,-40.5221601717608)) ;
#69771 = CARTESIAN_POINT('',(212.844152625408,578.087556589212,-40.5221601717612)) ;
#69772 = CARTESIAN_POINT('',(202.637277625405,578.462556589212,-40.5221601717608)) ;
#69773 = CARTESIAN_POINT('Origin',(202.262277625405,578.462556589212,-40.5221601717608)) ;
#69774 = CARTESIAN_POINT('',(202.637277625405,579.482556589212,-40.5221601717608)) ;
#69775 = CARTESIAN_POINT('',(202.637277625405,595.670681589213,-40.5221601717608)) ;
#69776 = CARTESIAN_POINT('Origin',(202.262277625405,579.482556589212,-40.5221601717608)) ;
#69777 = CARTESIAN_POINT('Origin',(206.038527625414,569.472556589211,-40.3971601717609)) ;
#69778 = CARTESIAN_POINT('',(207.538527625414,569.472556589211,-40.397160171761)) ;
#69779 = CARTESIAN_POINT('Origin',(206.038527625414,569.472556589211,-40.3971601717609)) ;
#69780 = CARTESIAN_POINT('',(207.663527625414,569.472556589211,-40.522160171761)) ;
#69781 = CARTESIAN_POINT('Origin',(207.663527625414,569.472556589211,-40.397160171761)) ;
#69782 = CARTESIAN_POINT('Origin',(206.038527625414,569.472556589211,-40.5221601717609)) ;
#69783 = CARTESIAN_POINT('Origin',(206.038527625414,569.472556589211,-29.1521601717607)) ;
#69784 = CARTESIAN_POINT('',(207.538527625414,569.472556589211,-37.0052690928546)) ;
#69785 = CARTESIAN_POINT('Origin',(206.038527625414,569.472556589211,-37.0052690928546)) ;
#69786 = CARTESIAN_POINT('',(207.538527625414,569.472556589211,-29.1521601717608)) ;
#69787 = CARTESIAN_POINT('Origin',(205.838527625413,569.472556589214,-40.5221601717609)) ;
#69788 = CARTESIAN_POINT('',(199.088527625414,573.548005939932,-40.5221601717606)) ;
#69789 = CARTESIAN_POINT('',(199.088527625412,565.397107238502,-40.5221601717606)) ;
#69790 = CARTESIAN_POINT('',(199.088527625409,547.972556589214,-40.5221601717606)) ;
#69791 = CARTESIAN_POINT('',(212.588527625414,573.54800593993,-40.5221601717612)) ;
#69792 = CARTESIAN_POINT('',(202.463527625414,573.548005939937,-40.5221601717608)) ;
#69793 = CARTESIAN_POINT('',(212.588527625412,565.3971072385,-40.5221601717612)) ;
#69794 = CARTESIAN_POINT('',(212.588527625409,547.972556589211,-40.5221601717612)) ;
#69795 = CARTESIAN_POINT('',(209.213527625412,565.397107238496,-40.5221601717611)) ;
#69796 = CARTESIAN_POINT('',(202.262277625405,570.357556589212,-40.5221601717608)) ;
#69797 = CARTESIAN_POINT('',(201.559777625406,570.357556589212,-40.5221601717607)) ;
#69798 = CARTESIAN_POINT('',(212.018652625408,570.357556589212,-40.5221601717612)) ;
#69799 = CARTESIAN_POINT('',(201.184777625406,569.982556589212,-40.5221601717607)) ;
#69800 = CARTESIAN_POINT('Origin',(201.559777625406,569.982556589212,-40.5221601717607)) ;
#69801 = CARTESIAN_POINT('',(201.184777625406,568.962556589212,-40.5221601717607)) ;
#69802 = CARTESIAN_POINT('',(201.184777625406,586.170681589212,-40.5221601717607)) ;
#69803 = CARTESIAN_POINT('',(201.559777625406,568.587556589212,-40.5221601717607)) ;
#69804 = CARTESIAN_POINT('Origin',(201.559777625406,568.962556589212,-40.5221601717607)) ;
#69805 = CARTESIAN_POINT('',(202.262277625405,568.587556589212,-40.5221601717608)) ;
#69806 = CARTESIAN_POINT('',(212.844152625408,568.587556589212,-40.5221601717612)) ;
#69807 = CARTESIAN_POINT('',(202.637277625405,568.962556589212,-40.5221601717608)) ;
#69808 = CARTESIAN_POINT('Origin',(202.262277625405,568.962556589212,-40.5221601717608)) ;
#69809 = CARTESIAN_POINT('',(202.637277625405,569.982556589212,-40.5221601717608)) ;
#69810 = CARTESIAN_POINT('',(202.637277625405,586.170681589213,-40.5221601717608)) ;
#69811 = CARTESIAN_POINT('Origin',(202.262277625405,569.982556589212,-40.5221601717608)) ;
#69812 = CARTESIAN_POINT('Origin',(206.038527625412,559.972556589211,-40.3971601717609)) ;
#69813 = CARTESIAN_POINT('',(207.538527625412,559.972556589211,-40.397160171761)) ;
#69814 = CARTESIAN_POINT('Origin',(206.038527625412,559.972556589211,-40.3971601717609)) ;
#69815 = CARTESIAN_POINT('',(207.663527625412,559.972556589211,-40.522160171761)) ;
#69816 = CARTESIAN_POINT('Origin',(207.663527625412,559.972556589211,-40.397160171761)) ;
#69817 = CARTESIAN_POINT('Origin',(206.038527625412,559.972556589211,-40.5221601717609)) ;
#69818 = CARTESIAN_POINT('Origin',(206.038527625413,559.972556589211,-29.1521601717607)) ;
#69819 = CARTESIAN_POINT('',(207.538527625412,559.972556589211,-37.0052690928546)) ;
#69820 = CARTESIAN_POINT('Origin',(206.038527625412,559.972556589211,-37.0052690928546)) ;
#69821 = CARTESIAN_POINT('',(207.538527625413,559.972556589211,-29.1521601717608)) ;
#69822 = CARTESIAN_POINT('Origin',(205.838527625413,569.472556589214,-40.5221601717609)) ;
#69823 = CARTESIAN_POINT('',(199.088527625412,564.048005939932,-40.5221601717606)) ;
#69824 = CARTESIAN_POINT('',(199.088527625411,555.897107238502,-40.5221601717606)) ;
#69825 = CARTESIAN_POINT('',(199.088527625409,547.972556589214,-40.5221601717606)) ;
#69826 = CARTESIAN_POINT('',(212.588527625412,564.04800593993,-40.5221601717612)) ;
#69827 = CARTESIAN_POINT('',(202.463527625412,564.04800593993,-40.5221601717608)) ;
#69828 = CARTESIAN_POINT('',(212.588527625411,555.8971072385,-40.5221601717612)) ;
#69829 = CARTESIAN_POINT('',(212.588527625409,547.972556589211,-40.5221601717612)) ;
#69830 = CARTESIAN_POINT('',(209.213527625411,555.897107238496,-40.5221601717611)) ;
#69831 = CARTESIAN_POINT('',(202.262277625406,560.857556589212,-40.5221601717608)) ;
#69832 = CARTESIAN_POINT('',(201.559777625406,560.857556589212,-40.5221601717607)) ;
#69833 = CARTESIAN_POINT('',(212.018652625409,560.857556589212,-40.5221601717612)) ;
#69834 = CARTESIAN_POINT('',(201.184777625406,560.482556589212,-40.5221601717607)) ;
#69835 = CARTESIAN_POINT('Origin',(201.559777625406,560.482556589212,-40.5221601717607)) ;
#69836 = CARTESIAN_POINT('',(201.184777625406,559.462556589212,-40.5221601717607)) ;
#69837 = CARTESIAN_POINT('',(201.184777625406,576.670681589212,-40.5221601717607)) ;
#69838 = CARTESIAN_POINT('',(201.559777625406,559.087556589212,-40.5221601717607)) ;
#69839 = CARTESIAN_POINT('Origin',(201.559777625406,559.462556589212,-40.5221601717607)) ;
#69840 = CARTESIAN_POINT('',(202.262277625406,559.087556589212,-40.5221601717608)) ;
#69841 = CARTESIAN_POINT('',(212.844152625408,559.087556589212,-40.5221601717612)) ;
#69842 = CARTESIAN_POINT('',(202.637277625406,559.462556589212,-40.5221601717608)) ;
#69843 = CARTESIAN_POINT('Origin',(202.262277625406,559.462556589212,-40.5221601717608)) ;
#69844 = CARTESIAN_POINT('',(202.637277625406,560.482556589212,-40.5221601717608)) ;
#69845 = CARTESIAN_POINT('',(202.637277625406,576.670681589213,-40.5221601717608)) ;
#69846 = CARTESIAN_POINT('Origin',(202.262277625406,560.482556589212,-40.5221601717608)) ;
#69847 = CARTESIAN_POINT('Origin',(206.03852762541,550.472556589211,-40.3971601717609)) ;
#69848 = CARTESIAN_POINT('',(207.53852762541,550.47255658921,-40.397160171761)) ;
#69849 = CARTESIAN_POINT('Origin',(206.03852762541,550.472556589211,-40.3971601717609)) ;
#69850 = CARTESIAN_POINT('',(207.66352762541,550.47255658921,-40.522160171761)) ;
#69851 = CARTESIAN_POINT('Origin',(207.66352762541,550.472556589211,-40.397160171761)) ;
#69852 = CARTESIAN_POINT('Origin',(206.03852762541,550.472556589211,-40.5221601717609)) ;
#69853 = CARTESIAN_POINT('Origin',(206.038527625411,550.472556589211,-29.1521601717607)) ;
#69854 = CARTESIAN_POINT('',(207.53852762541,550.47255658921,-37.0052690928546)) ;
#69855 = CARTESIAN_POINT('Origin',(206.038527625411,550.472556589211,-37.0052690928546)) ;
#69856 = CARTESIAN_POINT('',(207.538527625411,550.472556589211,-29.1521601717608)) ;
#69857 = CARTESIAN_POINT('Origin',(205.838527625413,569.472556589214,-40.5221601717609)) ;
#69858 = CARTESIAN_POINT('',(199.088527625411,554.548005939932,-40.5221601717606)) ;
#69859 = CARTESIAN_POINT('',(199.088527625409,546.397107238502,-40.5221601717606)) ;
#69860 = CARTESIAN_POINT('',(199.088527625409,547.972556589214,-40.5221601717606)) ;
#69861 = CARTESIAN_POINT('',(212.588527625411,554.54800593993,-40.5221601717612)) ;
#69862 = CARTESIAN_POINT('',(202.463527625411,554.54800593993,-40.5221601717608)) ;
#69863 = CARTESIAN_POINT('',(212.588527625409,546.3971072385,-40.5221601717612)) ;
#69864 = CARTESIAN_POINT('',(212.588527625409,547.972556589211,-40.5221601717612)) ;
#69865 = CARTESIAN_POINT('',(209.213527625409,546.397107238496,-40.5221601717611)) ;
#69866 = CARTESIAN_POINT('',(202.262277625406,551.357556589212,-40.5221601717608)) ;
#69867 = CARTESIAN_POINT('',(201.559777625406,551.357556589212,-40.5221601717607)) ;
#69868 = CARTESIAN_POINT('',(212.018652625409,551.357556589212,-40.5221601717612)) ;
#69869 = CARTESIAN_POINT('',(201.184777625406,550.982556589212,-40.5221601717607)) ;
#69870 = CARTESIAN_POINT('Origin',(201.559777625406,550.982556589212,-40.5221601717607)) ;
#69871 = CARTESIAN_POINT('',(201.184777625406,549.962556589212,-40.5221601717607)) ;
#69872 = CARTESIAN_POINT('',(201.184777625406,567.170681589212,-40.5221601717607)) ;
#69873 = CARTESIAN_POINT('',(201.559777625407,549.587556589212,-40.5221601717607)) ;
#69874 = CARTESIAN_POINT('Origin',(201.559777625406,549.962556589212,-40.5221601717607)) ;
#69875 = CARTESIAN_POINT('',(202.262277625406,549.587556589212,-40.5221601717608)) ;
#69876 = CARTESIAN_POINT('',(212.844152625409,549.587556589212,-40.5221601717612)) ;
#69877 = CARTESIAN_POINT('',(202.637277625406,549.962556589212,-40.5221601717608)) ;
#69878 = CARTESIAN_POINT('Origin',(202.262277625406,549.962556589212,-40.5221601717608)) ;
#69879 = CARTESIAN_POINT('',(202.637277625406,550.982556589212,-40.5221601717608)) ;
#69880 = CARTESIAN_POINT('',(202.637277625406,567.170681589213,-40.5221601717608)) ;
#69881 = CARTESIAN_POINT('Origin',(202.262277625406,550.982556589212,-40.5221601717608)) ;
#69882 = CARTESIAN_POINT('Origin',(206.038527625409,540.972556589211,-40.3971601717609)) ;
#69883 = CARTESIAN_POINT('',(207.538527625409,540.97255658921,-40.397160171761)) ;
#69884 = CARTESIAN_POINT('Origin',(206.038527625409,540.972556589211,-40.3971601717609)) ;
#69885 = CARTESIAN_POINT('',(207.663527625409,540.97255658921,-40.522160171761)) ;
#69886 = CARTESIAN_POINT('Origin',(207.663527625409,540.972556589211,-40.397160171761)) ;
#69887 = CARTESIAN_POINT('Origin',(206.038527625409,540.972556589211,-40.5221601717609)) ;
#69888 = CARTESIAN_POINT('Origin',(206.038527625409,540.972556589211,-29.1521601717607)) ;
#69889 = CARTESIAN_POINT('',(207.538527625409,540.97255658921,-37.0052690928546)) ;
#69890 = CARTESIAN_POINT('Origin',(206.038527625409,540.972556589211,-37.0052690928546)) ;
#69891 = CARTESIAN_POINT('',(207.538527625409,540.972556589211,-29.1521601717608)) ;
#69892 = CARTESIAN_POINT('Origin',(205.838527625413,569.472556589214,-40.5221601717609)) ;
#69893 = CARTESIAN_POINT('',(199.088527625409,545.048005939932,-40.5221601717606)) ;
#69894 = CARTESIAN_POINT('',(199.088527625407,536.897107238502,-40.5221601717606)) ;
#69895 = CARTESIAN_POINT('',(199.088527625409,547.972556589214,-40.5221601717606)) ;
#69896 = CARTESIAN_POINT('',(212.588527625409,545.04800593993,-40.5221601717612)) ;
#69897 = CARTESIAN_POINT('',(202.463527625409,545.04800593993,-40.5221601717608)) ;
#69898 = CARTESIAN_POINT('',(212.588527625407,536.8971072385,-40.5221601717612)) ;
#69899 = CARTESIAN_POINT('',(212.588527625409,547.972556589211,-40.5221601717612)) ;
#69900 = CARTESIAN_POINT('',(209.213527625407,536.897107238496,-40.5221601717611)) ;
#69901 = CARTESIAN_POINT('',(202.262277625406,541.857556589212,-40.5221601717608)) ;
#69902 = CARTESIAN_POINT('',(201.559777625407,541.857556589212,-40.5221601717607)) ;
#69903 = CARTESIAN_POINT('',(212.018652625409,541.857556589212,-40.5221601717612)) ;
#69904 = CARTESIAN_POINT('',(201.184777625407,541.482556589212,-40.5221601717607)) ;
#69905 = CARTESIAN_POINT('Origin',(201.559777625407,541.482556589212,-40.5221601717607)) ;
#69906 = CARTESIAN_POINT('',(201.184777625407,540.462556589212,-40.5221601717607)) ;
#69907 = CARTESIAN_POINT('',(201.184777625407,557.670681589212,-40.5221601717607)) ;
#69908 = CARTESIAN_POINT('',(201.559777625407,540.087556589212,-40.5221601717607)) ;
#69909 = CARTESIAN_POINT('Origin',(201.559777625407,540.462556589212,-40.5221601717607)) ;
#69910 = CARTESIAN_POINT('',(202.262277625406,540.087556589212,-40.5221601717608)) ;
#69911 = CARTESIAN_POINT('',(212.844152625409,540.087556589212,-40.5221601717612)) ;
#69912 = CARTESIAN_POINT('',(202.637277625406,540.462556589212,-40.5221601717608)) ;
#69913 = CARTESIAN_POINT('Origin',(202.262277625406,540.462556589212,-40.5221601717608)) ;
#69914 = CARTESIAN_POINT('',(202.637277625406,541.482556589212,-40.5221601717608)) ;
#69915 = CARTESIAN_POINT('',(202.637277625406,557.670681589212,-40.5221601717608)) ;
#69916 = CARTESIAN_POINT('Origin',(202.262277625406,541.482556589212,-40.5221601717608)) ;
#69917 = CARTESIAN_POINT('Origin',(206.038527625407,531.472556589211,-40.3971601717609)) ;
#69918 = CARTESIAN_POINT('',(207.538527625407,531.47255658921,-40.397160171761)) ;
#69919 = CARTESIAN_POINT('Origin',(206.038527625407,531.472556589211,-40.3971601717609)) ;
#69920 = CARTESIAN_POINT('',(207.663527625407,531.47255658921,-40.522160171761)) ;
#69921 = CARTESIAN_POINT('Origin',(207.663527625407,531.472556589211,-40.397160171761)) ;
#69922 = CARTESIAN_POINT('Origin',(206.038527625407,531.472556589211,-40.5221601717609)) ;
#69923 = CARTESIAN_POINT('Origin',(205.838527625413,569.472556589214,-40.5221601717609)) ;
#69924 = CARTESIAN_POINT('',(199.088527625407,535.548005939932,-40.5221601717606)) ;
#69925 = CARTESIAN_POINT('',(199.088527625406,527.397107238502,-40.5221601717606)) ;
#69926 = CARTESIAN_POINT('',(199.088527625409,547.972556589214,-40.5221601717606)) ;
#69927 = CARTESIAN_POINT('',(212.588527625407,535.54800593993,-40.5221601717612)) ;
#69928 = CARTESIAN_POINT('',(202.463527625407,535.54800593993,-40.5221601717608)) ;
#69929 = CARTESIAN_POINT('',(212.588527625406,527.3971072385,-40.5221601717612)) ;
#69930 = CARTESIAN_POINT('',(212.588527625409,547.972556589211,-40.5221601717612)) ;
#69931 = CARTESIAN_POINT('',(209.213527625406,527.397107238496,-40.5221601717611)) ;
#69932 = CARTESIAN_POINT('',(201.559777625407,532.357556589212,-40.5221601717607)) ;
#69933 = CARTESIAN_POINT('',(202.262277625407,532.357556589212,-40.5221601717608)) ;
#69934 = CARTESIAN_POINT('',(212.01865262541,532.357556589212,-40.5221601717612)) ;
#69935 = CARTESIAN_POINT('',(201.184777625407,531.982556589212,-40.5221601717607)) ;
#69936 = CARTESIAN_POINT('Origin',(201.559777625407,531.982556589212,-40.5221601717607)) ;
#69937 = CARTESIAN_POINT('',(201.184777625407,530.962556589212,-40.5221601717607)) ;
#69938 = CARTESIAN_POINT('',(201.184777625407,548.170681589212,-40.5221601717607)) ;
#69939 = CARTESIAN_POINT('',(201.559777625407,530.587556589212,-40.5221601717607)) ;
#69940 = CARTESIAN_POINT('Origin',(201.559777625407,530.962556589212,-40.5221601717607)) ;
#69941 = CARTESIAN_POINT('',(202.262277625407,530.587556589212,-40.5221601717608)) ;
#69942 = CARTESIAN_POINT('',(212.844152625409,530.587556589212,-40.5221601717613)) ;
#69943 = CARTESIAN_POINT('',(202.637277625407,530.962556589212,-40.5221601717608)) ;
#69944 = CARTESIAN_POINT('Origin',(202.262277625407,530.962556589212,-40.5221601717608)) ;
#69945 = CARTESIAN_POINT('',(202.637277625407,531.982556589212,-40.5221601717608)) ;
#69946 = CARTESIAN_POINT('',(202.637277625407,548.170681589212,-40.5221601717608)) ;
#69947 = CARTESIAN_POINT('Origin',(202.262277625407,531.982556589212,-40.5221601717608)) ;
#69948 = CARTESIAN_POINT('Origin',(206.038527625407,531.472556589211,-29.1521601717607)) ;
#69949 = CARTESIAN_POINT('',(207.538527625407,531.47255658921,-37.0052690928546)) ;
#69950 = CARTESIAN_POINT('Origin',(206.038527625407,531.472556589211,-37.0052690928546)) ;
#69951 = CARTESIAN_POINT('',(207.538527625407,531.472556589211,-29.1521601717608)) ;
#69952 = CARTESIAN_POINT('Origin',(202.466652625407,535.044431589211,-37.0052690928544)) ;
#69953 = CARTESIAN_POINT('',(208.77102762542,607.472556589211,-37.0052690928544)) ;
#69954 = CARTESIAN_POINT('Origin',(206.03852762542,607.472556589211,-37.0052690928544)) ;
#69955 = CARTESIAN_POINT('Origin',(202.466652625407,535.044431589211,-37.0052690928544)) ;
#69956 = CARTESIAN_POINT('',(208.771027625418,597.972556589211,-37.0052690928544)) ;
#69957 = CARTESIAN_POINT('Origin',(206.038527625418,597.972556589211,-37.0052690928544)) ;
#69958 = CARTESIAN_POINT('Origin',(202.466652625407,535.044431589211,-37.0052690928544)) ;
#69959 = CARTESIAN_POINT('',(208.771027625417,588.472556589211,-37.0052690928544)) ;
#69960 = CARTESIAN_POINT('Origin',(206.038527625417,588.472556589211,-37.0052690928544)) ;
#69961 = CARTESIAN_POINT('Origin',(202.466652625407,535.044431589211,-37.0052690928544)) ;
#69962 = CARTESIAN_POINT('',(208.771027625415,578.972556589211,-37.0052690928544)) ;
#69963 = CARTESIAN_POINT('Origin',(206.038527625415,578.972556589211,-37.0052690928544)) ;
#69964 = CARTESIAN_POINT('Origin',(202.466652625407,535.044431589211,-37.0052690928544)) ;
#69965 = CARTESIAN_POINT('',(208.771027625413,569.472556589211,-37.0052690928544)) ;
#69966 = CARTESIAN_POINT('Origin',(206.038527625413,569.472556589211,-37.0052690928544)) ;
#69967 = CARTESIAN_POINT('Origin',(202.466652625407,535.044431589211,-37.0052690928544)) ;
#69968 = CARTESIAN_POINT('',(208.771027625412,559.972556589211,-37.0052690928544)) ;
#69969 = CARTESIAN_POINT('Origin',(206.038527625412,559.972556589211,-37.0052690928544)) ;
#69970 = CARTESIAN_POINT('Origin',(202.466652625407,535.044431589211,-37.0052690928544)) ;
#69971 = CARTESIAN_POINT('',(208.77102762541,550.472556589211,-37.0052690928544)) ;
#69972 = CARTESIAN_POINT('Origin',(206.03852762541,550.472556589211,-37.0052690928544)) ;
#69973 = CARTESIAN_POINT('Origin',(202.466652625407,535.044431589211,-37.0052690928544)) ;
#69974 = CARTESIAN_POINT('',(208.771027625408,540.972556589211,-37.0052690928544)) ;
#69975 = CARTESIAN_POINT('Origin',(206.038527625408,540.972556589211,-37.0052690928544)) ;
#69976 = CARTESIAN_POINT('Origin',(212.018652625407,608.357556589212,-40.2721601717612)) ;
#69977 = CARTESIAN_POINT('',(202.262277625404,608.107556589212,-40.2721601717608)) ;
#69978 = CARTESIAN_POINT('Origin',(202.262277625404,608.357556589212,-40.2721601717608)) ;
#69979 = CARTESIAN_POINT('',(201.559777625404,608.107556589212,-40.2721601717607)) ;
#69980 = CARTESIAN_POINT('',(212.018652625407,608.107556589212,-40.2721601717612)) ;
#69981 = CARTESIAN_POINT('Origin',(201.559777625404,608.357556589212,-40.2721601717607)) ;
#69982 = CARTESIAN_POINT('Origin',(201.559777625404,607.982556589212,-40.2721601717609)) ;
#69983 = CARTESIAN_POINT('',(201.434777625404,607.982556589212,-40.2721601717609)) ;
#69984 = CARTESIAN_POINT('Origin',(201.184777625404,607.982556589212,-40.2721601717609)) ;
#69985 = CARTESIAN_POINT('Origin',(201.559777625404,607.982556589212,-40.2721601717609)) ;
#69986 = CARTESIAN_POINT('Origin',(201.184777625405,624.170681589212,-40.2721601717607)) ;
#69987 = CARTESIAN_POINT('',(201.434777625404,606.962556589212,-40.2721601717607)) ;
#69988 = CARTESIAN_POINT('Origin',(201.184777625405,606.962556589212,-40.2721601717607)) ;
#69989 = CARTESIAN_POINT('',(201.43477762542,624.170681589212,-40.2721601717607)) ;
#69990 = CARTESIAN_POINT('Origin',(201.559777625404,606.962556589212,-40.2721601717609)) ;
#69991 = CARTESIAN_POINT('',(201.559777625405,606.837556589212,-40.2721601717609)) ;
#69992 = CARTESIAN_POINT('Origin',(201.559777625405,606.587556589212,-40.2721601717609)) ;
#69993 = CARTESIAN_POINT('Origin',(201.559777625404,606.962556589212,-40.2721601717609)) ;
#69994 = CARTESIAN_POINT('Origin',(212.844152625407,606.587556589212,-40.2721601717612)) ;
#69995 = CARTESIAN_POINT('',(202.262277625404,606.837556589212,-40.2721601717608)) ;
#69996 = CARTESIAN_POINT('Origin',(202.262277625404,606.587556589212,-40.2721601717608)) ;
#69997 = CARTESIAN_POINT('',(212.844152625407,606.837556589212,-40.2721601717612)) ;
#69998 = CARTESIAN_POINT('Origin',(202.262277625404,606.962556589212,-40.2721601717609)) ;
#69999 = CARTESIAN_POINT('',(202.387277625404,606.962556589212,-40.2721601717609)) ;
#70000 = CARTESIAN_POINT('Origin',(202.637277625404,606.962556589212,-40.2721601717609)) ;
#70001 = CARTESIAN_POINT('Origin',(202.262277625404,606.962556589212,-40.2721601717609)) ;
#70002 = CARTESIAN_POINT('Origin',(202.637277625404,624.170681589213,-40.2721601717608)) ;
#70003 = CARTESIAN_POINT('',(202.387277625404,607.982556589212,-40.2721601717608)) ;
#70004 = CARTESIAN_POINT('Origin',(202.637277625404,607.982556589212,-40.2721601717608)) ;
#70005 = CARTESIAN_POINT('',(202.38727762542,624.170681589213,-40.2721601717608)) ;
#70006 = CARTESIAN_POINT('Origin',(202.262277625404,607.982556589212,-40.2721601717609)) ;
#70007 = CARTESIAN_POINT('Origin',(202.262277625404,607.982556589212,-40.2721601717609)) ;
#70008 = CARTESIAN_POINT('Origin',(201.55977762542,606.962556589212,-42.3117150424525)) ;
#70009 = CARTESIAN_POINT('',(201.43477762542,606.962556589212,-39.4182700580611)) ;
#70010 = CARTESIAN_POINT('',(201.43477762542,606.962556589212,-42.3117150424525)) ;
#70011 = CARTESIAN_POINT('',(201.55977762542,606.837556589212,-39.4182700580611)) ;
#70012 = CARTESIAN_POINT('Origin',(201.55977762542,606.962556589212,-39.4182700580611)) ;
#70013 = CARTESIAN_POINT('',(201.55977762542,606.837556589212,-42.3117150424525)) ;
#70014 = CARTESIAN_POINT('Origin',(201.43477762542,602.868806589211,-43.1012690928543)) ;
#70015 = CARTESIAN_POINT('',(201.43477762542,607.982556589212,-39.4182700580611)) ;
#70016 = CARTESIAN_POINT('',(201.43477762542,607.982556589212,-44.5342150424525)) ;
#70017 = CARTESIAN_POINT('',(201.43477762542,608.171056589212,-39.2297700580612)) ;
#70018 = CARTESIAN_POINT('Origin',(201.43477762542,608.171056589212,-39.4182700580612)) ;
#70019 = CARTESIAN_POINT('',(201.43477762542,609.347556589211,-39.2297700580612)) ;
#70020 = CARTESIAN_POINT('',(201.43477762542,605.488181589211,-39.2297700580612)) ;
#70021 = CARTESIAN_POINT('',(201.434777625407,609.347556589211,-35.2721601717607)) ;
#70022 = CARTESIAN_POINT('',(201.43477762542,609.347556589211,-38.5610190928544)) ;
#70023 = CARTESIAN_POINT('',(201.434777625407,605.597556589211,-35.2721601717609)) ;
#70024 = CARTESIAN_POINT('',(201.43477762542,624.170681589221,-35.2721601717607)) ;
#70025 = CARTESIAN_POINT('',(201.43477762542,605.597556589211,-39.2297700580612)) ;
#70026 = CARTESIAN_POINT('',(201.43477762542,605.597556589211,-40.5297040214914)) ;
#70027 = CARTESIAN_POINT('',(201.43477762542,606.774056589212,-39.2297700580612)) ;
#70028 = CARTESIAN_POINT('',(201.43477762542,605.488181589211,-39.2297700580612)) ;
#70029 = CARTESIAN_POINT('Origin',(201.43477762542,606.774056589212,-39.4182700580611)) ;
#70030 = CARTESIAN_POINT('Origin',(201.55977762542,607.982556589212,-44.5342150424525)) ;
#70031 = CARTESIAN_POINT('',(201.55977762542,608.107556589212,-39.4182700580612)) ;
#70032 = CARTESIAN_POINT('',(201.55977762542,608.107556589212,-44.5342150424525)) ;
#70033 = CARTESIAN_POINT('Origin',(201.55977762542,607.982556589212,-39.4182700580611)) ;
#70034 = CARTESIAN_POINT('Origin',(218.198777625419,608.107556589212,-45.9671609920506)) ;
#70035 = CARTESIAN_POINT('',(202.26227762542,608.107556589212,-39.4182700580612)) ;
#70036 = CARTESIAN_POINT('',(202.26227762542,608.107556589212,-39.8669650424525)) ;
#70037 = CARTESIAN_POINT('',(218.198777625419,608.107556589212,-39.4182700580611)) ;
#70038 = CARTESIAN_POINT('Origin',(212.018652625407,598.857556589212,-40.2721601717612)) ;
#70039 = CARTESIAN_POINT('',(202.262277625404,598.607556589212,-40.2721601717608)) ;
#70040 = CARTESIAN_POINT('Origin',(202.262277625404,598.857556589212,-40.2721601717608)) ;
#70041 = CARTESIAN_POINT('',(201.559777625405,598.607556589212,-40.2721601717607)) ;
#70042 = CARTESIAN_POINT('',(212.018652625407,598.607556589212,-40.2721601717612)) ;
#70043 = CARTESIAN_POINT('Origin',(201.559777625405,598.857556589212,-40.2721601717607)) ;
#70044 = CARTESIAN_POINT('Origin',(201.559777625405,598.482556589212,-40.2721601717609)) ;
#70045 = CARTESIAN_POINT('',(201.434777625405,598.482556589212,-40.2721601717609)) ;
#70046 = CARTESIAN_POINT('Origin',(201.184777625405,598.482556589212,-40.2721601717609)) ;
#70047 = CARTESIAN_POINT('Origin',(201.559777625405,598.482556589212,-40.2721601717609)) ;
#70048 = CARTESIAN_POINT('Origin',(201.184777625405,614.670681589212,-40.2721601717607)) ;
#70049 = CARTESIAN_POINT('',(201.434777625405,597.462556589212,-40.2721601717607)) ;
#70050 = CARTESIAN_POINT('Origin',(201.184777625405,597.462556589212,-40.2721601717607)) ;
#70051 = CARTESIAN_POINT('',(201.434777625419,614.670681589212,-40.2721601717607)) ;
#70052 = CARTESIAN_POINT('Origin',(201.559777625405,597.462556589212,-40.2721601717609)) ;
#70053 = CARTESIAN_POINT('',(201.559777625405,597.337556589212,-40.2721601717609)) ;
#70054 = CARTESIAN_POINT('Origin',(201.559777625405,597.087556589212,-40.2721601717609)) ;
#70055 = CARTESIAN_POINT('Origin',(201.559777625405,597.462556589212,-40.2721601717609)) ;
#70056 = CARTESIAN_POINT('Origin',(212.844152625407,597.087556589212,-40.2721601717612)) ;
#70057 = CARTESIAN_POINT('',(202.262277625404,597.337556589212,-40.2721601717608)) ;
#70058 = CARTESIAN_POINT('Origin',(202.262277625404,597.087556589212,-40.2721601717608)) ;
#70059 = CARTESIAN_POINT('',(212.844152625407,597.337556589212,-40.2721601717612)) ;
#70060 = CARTESIAN_POINT('Origin',(202.262277625404,597.462556589212,-40.2721601717609)) ;
#70061 = CARTESIAN_POINT('',(202.387277625404,597.462556589212,-40.2721601717609)) ;
#70062 = CARTESIAN_POINT('Origin',(202.637277625404,597.462556589212,-40.2721601717609)) ;
#70063 = CARTESIAN_POINT('Origin',(202.262277625404,597.462556589212,-40.2721601717609)) ;
#70064 = CARTESIAN_POINT('Origin',(202.637277625404,614.670681589213,-40.2721601717608)) ;
#70065 = CARTESIAN_POINT('',(202.387277625404,598.482556589212,-40.2721601717608)) ;
#70066 = CARTESIAN_POINT('Origin',(202.637277625404,598.482556589212,-40.2721601717608)) ;
#70067 = CARTESIAN_POINT('',(202.387277625418,614.670681589213,-40.2721601717608)) ;
#70068 = CARTESIAN_POINT('Origin',(202.262277625404,598.482556589212,-40.2721601717609)) ;
#70069 = CARTESIAN_POINT('Origin',(202.262277625404,598.482556589212,-40.2721601717609)) ;
#70070 = CARTESIAN_POINT('Origin',(201.559777625419,597.462556589212,-42.3117150424525)) ;
#70071 = CARTESIAN_POINT('',(201.434777625419,597.462556589212,-39.4182700580611)) ;
#70072 = CARTESIAN_POINT('',(201.434777625419,597.462556589212,-42.3117150424525)) ;
#70073 = CARTESIAN_POINT('',(201.559777625419,597.337556589212,-39.4182700580611)) ;
#70074 = CARTESIAN_POINT('Origin',(201.559777625419,597.462556589212,-39.4182700580611)) ;
#70075 = CARTESIAN_POINT('',(201.559777625419,597.337556589212,-42.3117150424525)) ;
#70076 = CARTESIAN_POINT('Origin',(201.434777625419,593.368806589211,-43.1012690928543)) ;
#70077 = CARTESIAN_POINT('',(201.434777625419,598.482556589212,-39.4182700580611)) ;
#70078 = CARTESIAN_POINT('',(201.434777625419,598.482556589212,-44.5342150424525)) ;
#70079 = CARTESIAN_POINT('',(201.434777625419,598.671056589212,-39.2297700580612)) ;
#70080 = CARTESIAN_POINT('Origin',(201.434777625419,598.671056589212,-39.4182700580612)) ;
#70081 = CARTESIAN_POINT('',(201.434777625419,599.847556589211,-39.2297700580612)) ;
#70082 = CARTESIAN_POINT('',(201.434777625419,595.988181589211,-39.2297700580612)) ;
#70083 = CARTESIAN_POINT('',(201.434777625407,599.847556589211,-35.2721601717607)) ;
#70084 = CARTESIAN_POINT('',(201.434777625419,599.847556589211,-38.5610190928544)) ;
#70085 = CARTESIAN_POINT('',(201.434777625407,596.097556589211,-35.2721601717609)) ;
#70086 = CARTESIAN_POINT('',(201.434777625419,614.670681589221,-35.2721601717607)) ;
#70087 = CARTESIAN_POINT('',(201.434777625419,596.097556589211,-39.2297700580612)) ;
#70088 = CARTESIAN_POINT('',(201.434777625419,596.097556589211,-40.5297040214914)) ;
#70089 = CARTESIAN_POINT('',(201.434777625419,597.274056589212,-39.2297700580612)) ;
#70090 = CARTESIAN_POINT('',(201.434777625419,595.988181589211,-39.2297700580612)) ;
#70091 = CARTESIAN_POINT('Origin',(201.434777625419,597.274056589212,-39.4182700580611)) ;
#70092 = CARTESIAN_POINT('Origin',(201.559777625419,598.482556589212,-44.5342150424525)) ;
#70093 = CARTESIAN_POINT('',(201.559777625419,598.607556589212,-39.4182700580612)) ;
#70094 = CARTESIAN_POINT('',(201.559777625419,598.607556589212,-44.5342150424525)) ;
#70095 = CARTESIAN_POINT('Origin',(201.559777625419,598.482556589212,-39.4182700580611)) ;
#70096 = CARTESIAN_POINT('Origin',(218.198777625417,598.607556589212,-45.9671609920506)) ;
#70097 = CARTESIAN_POINT('',(202.262277625418,598.607556589212,-39.4182700580612)) ;
#70098 = CARTESIAN_POINT('',(202.262277625418,598.607556589212,-39.8669650424525)) ;
#70099 = CARTESIAN_POINT('',(218.198777625418,598.607556589212,-39.4182700580611)) ;
#70100 = CARTESIAN_POINT('Origin',(212.018652625408,589.357556589212,-40.2721601717612)) ;
#70101 = CARTESIAN_POINT('',(202.262277625405,589.107556589212,-40.2721601717608)) ;
#70102 = CARTESIAN_POINT('Origin',(202.262277625405,589.357556589212,-40.2721601717608)) ;
#70103 = CARTESIAN_POINT('',(201.559777625405,589.107556589212,-40.2721601717607)) ;
#70104 = CARTESIAN_POINT('',(212.018652625408,589.107556589212,-40.2721601717612)) ;
#70105 = CARTESIAN_POINT('Origin',(201.559777625405,589.357556589212,-40.2721601717607)) ;
#70106 = CARTESIAN_POINT('Origin',(201.559777625405,588.982556589212,-40.2721601717609)) ;
#70107 = CARTESIAN_POINT('',(201.434777625405,588.982556589212,-40.2721601717609)) ;
#70108 = CARTESIAN_POINT('Origin',(201.184777625405,588.982556589212,-40.2721601717609)) ;
#70109 = CARTESIAN_POINT('Origin',(201.559777625405,588.982556589212,-40.2721601717609)) ;
#70110 = CARTESIAN_POINT('Origin',(201.184777625405,605.170681589212,-40.2721601717607)) ;
#70111 = CARTESIAN_POINT('',(201.434777625405,587.962556589212,-40.2721601717607)) ;
#70112 = CARTESIAN_POINT('Origin',(201.184777625405,587.962556589212,-40.2721601717607)) ;
#70113 = CARTESIAN_POINT('',(201.434777625417,605.170681589212,-40.2721601717607)) ;
#70114 = CARTESIAN_POINT('Origin',(201.559777625405,587.962556589212,-40.2721601717609)) ;
#70115 = CARTESIAN_POINT('',(201.559777625405,587.837556589212,-40.2721601717609)) ;
#70116 = CARTESIAN_POINT('Origin',(201.559777625405,587.587556589212,-40.2721601717609)) ;
#70117 = CARTESIAN_POINT('Origin',(201.559777625405,587.962556589212,-40.2721601717609)) ;
#70118 = CARTESIAN_POINT('Origin',(212.844152625407,587.587556589212,-40.2721601717612)) ;
#70119 = CARTESIAN_POINT('',(202.262277625405,587.837556589212,-40.2721601717608)) ;
#70120 = CARTESIAN_POINT('Origin',(202.262277625405,587.587556589212,-40.2721601717608)) ;
#70121 = CARTESIAN_POINT('',(212.844152625408,587.837556589212,-40.2721601717612)) ;
#70122 = CARTESIAN_POINT('Origin',(202.262277625405,587.962556589212,-40.2721601717609)) ;
#70123 = CARTESIAN_POINT('',(202.387277625405,587.962556589212,-40.2721601717609)) ;
#70124 = CARTESIAN_POINT('Origin',(202.637277625405,587.962556589212,-40.2721601717609)) ;
#70125 = CARTESIAN_POINT('Origin',(202.262277625405,587.962556589212,-40.2721601717609)) ;
#70126 = CARTESIAN_POINT('Origin',(202.637277625405,605.170681589213,-40.2721601717608)) ;
#70127 = CARTESIAN_POINT('',(202.387277625405,588.982556589212,-40.2721601717608)) ;
#70128 = CARTESIAN_POINT('Origin',(202.637277625405,588.982556589212,-40.2721601717608)) ;
#70129 = CARTESIAN_POINT('',(202.387277625417,605.170681589213,-40.2721601717608)) ;
#70130 = CARTESIAN_POINT('Origin',(202.262277625405,588.982556589212,-40.2721601717609)) ;
#70131 = CARTESIAN_POINT('Origin',(202.262277625405,588.982556589212,-40.2721601717609)) ;
#70132 = CARTESIAN_POINT('Origin',(201.559777625417,587.962556589212,-42.3117150424525)) ;
#70133 = CARTESIAN_POINT('',(201.434777625417,587.962556589212,-39.4182700580611)) ;
#70134 = CARTESIAN_POINT('',(201.434777625417,587.962556589212,-42.3117150424525)) ;
#70135 = CARTESIAN_POINT('',(201.559777625417,587.837556589212,-39.4182700580611)) ;
#70136 = CARTESIAN_POINT('Origin',(201.559777625417,587.962556589212,-39.4182700580611)) ;
#70137 = CARTESIAN_POINT('',(201.559777625417,587.837556589212,-42.3117150424525)) ;
#70138 = CARTESIAN_POINT('Origin',(201.434777625417,583.868806589211,-43.1012690928543)) ;
#70139 = CARTESIAN_POINT('',(201.434777625417,588.982556589212,-39.4182700580611)) ;
#70140 = CARTESIAN_POINT('',(201.434777625417,588.982556589212,-44.5342150424525)) ;
#70141 = CARTESIAN_POINT('',(201.434777625417,589.171056589212,-39.2297700580612)) ;
#70142 = CARTESIAN_POINT('Origin',(201.434777625417,589.171056589212,-39.4182700580612)) ;
#70143 = CARTESIAN_POINT('',(201.434777625417,590.347556589211,-39.2297700580612)) ;
#70144 = CARTESIAN_POINT('',(201.434777625417,586.488181589211,-39.2297700580612)) ;
#70145 = CARTESIAN_POINT('',(201.434777625407,590.347556589211,-35.2721601717607)) ;
#70146 = CARTESIAN_POINT('',(201.434777625417,590.347556589211,-38.5610190928544)) ;
#70147 = CARTESIAN_POINT('',(201.434777625407,586.597556589211,-35.2721601717609)) ;
#70148 = CARTESIAN_POINT('',(201.434777625417,605.170681589221,-35.2721601717607)) ;
#70149 = CARTESIAN_POINT('',(201.434777625417,586.597556589211,-39.2297700580612)) ;
#70150 = CARTESIAN_POINT('',(201.434777625417,586.597556589211,-40.5297040214914)) ;
#70151 = CARTESIAN_POINT('',(201.434777625417,587.774056589212,-39.2297700580612)) ;
#70152 = CARTESIAN_POINT('',(201.434777625417,586.488181589211,-39.2297700580612)) ;
#70153 = CARTESIAN_POINT('Origin',(201.434777625417,587.774056589212,-39.4182700580611)) ;
#70154 = CARTESIAN_POINT('Origin',(201.559777625417,588.982556589212,-44.5342150424525)) ;
#70155 = CARTESIAN_POINT('',(201.559777625417,589.107556589212,-39.4182700580612)) ;
#70156 = CARTESIAN_POINT('',(201.559777625417,589.107556589212,-44.5342150424525)) ;
#70157 = CARTESIAN_POINT('Origin',(201.559777625417,588.982556589212,-39.4182700580611)) ;
#70158 = CARTESIAN_POINT('Origin',(218.198777625415,589.107556589212,-45.9671609920506)) ;
#70159 = CARTESIAN_POINT('',(202.262277625416,589.107556589212,-39.4182700580612)) ;
#70160 = CARTESIAN_POINT('',(202.262277625416,589.107556589212,-39.8669650424525)) ;
#70161 = CARTESIAN_POINT('',(218.198777625416,589.107556589212,-39.4182700580611)) ;
#70162 = CARTESIAN_POINT('Origin',(212.018652625408,579.857556589212,-40.2721601717612)) ;
#70163 = CARTESIAN_POINT('',(202.262277625405,579.607556589212,-40.2721601717608)) ;
#70164 = CARTESIAN_POINT('Origin',(202.262277625405,579.857556589212,-40.2721601717608)) ;
#70165 = CARTESIAN_POINT('',(201.559777625405,579.607556589212,-40.2721601717607)) ;
#70166 = CARTESIAN_POINT('',(212.018652625408,579.607556589212,-40.2721601717612)) ;
#70167 = CARTESIAN_POINT('Origin',(201.559777625405,579.857556589212,-40.2721601717607)) ;
#70168 = CARTESIAN_POINT('Origin',(201.559777625405,579.482556589212,-40.2721601717609)) ;
#70169 = CARTESIAN_POINT('',(201.434777625406,579.482556589212,-40.2721601717609)) ;
#70170 = CARTESIAN_POINT('Origin',(201.184777625405,579.482556589212,-40.2721601717609)) ;
#70171 = CARTESIAN_POINT('Origin',(201.559777625405,579.482556589212,-40.2721601717609)) ;
#70172 = CARTESIAN_POINT('Origin',(201.184777625406,595.670681589212,-40.2721601717607)) ;
#70173 = CARTESIAN_POINT('',(201.434777625406,578.462556589212,-40.2721601717607)) ;
#70174 = CARTESIAN_POINT('Origin',(201.184777625406,578.462556589212,-40.2721601717607)) ;
#70175 = CARTESIAN_POINT('',(201.434777625415,595.670681589212,-40.2721601717607)) ;
#70176 = CARTESIAN_POINT('Origin',(201.559777625405,578.462556589212,-40.2721601717609)) ;
#70177 = CARTESIAN_POINT('',(201.559777625406,578.337556589212,-40.2721601717609)) ;
#70178 = CARTESIAN_POINT('Origin',(201.559777625406,578.087556589212,-40.2721601717609)) ;
#70179 = CARTESIAN_POINT('Origin',(201.559777625405,578.462556589212,-40.2721601717609)) ;
#70180 = CARTESIAN_POINT('Origin',(212.844152625408,578.087556589212,-40.2721601717612)) ;
#70181 = CARTESIAN_POINT('',(202.262277625405,578.337556589212,-40.2721601717608)) ;
#70182 = CARTESIAN_POINT('Origin',(202.262277625405,578.087556589212,-40.2721601717608)) ;
#70183 = CARTESIAN_POINT('',(212.844152625408,578.337556589212,-40.2721601717612)) ;
#70184 = CARTESIAN_POINT('Origin',(202.262277625405,578.462556589212,-40.2721601717609)) ;
#70185 = CARTESIAN_POINT('',(202.387277625405,578.462556589212,-40.2721601717609)) ;
#70186 = CARTESIAN_POINT('Origin',(202.637277625405,578.462556589212,-40.2721601717609)) ;
#70187 = CARTESIAN_POINT('Origin',(202.262277625405,578.462556589212,-40.2721601717609)) ;
#70188 = CARTESIAN_POINT('Origin',(202.637277625405,595.670681589213,-40.2721601717608)) ;
#70189 = CARTESIAN_POINT('',(202.387277625405,579.482556589212,-40.2721601717608)) ;
#70190 = CARTESIAN_POINT('Origin',(202.637277625405,579.482556589212,-40.2721601717608)) ;
#70191 = CARTESIAN_POINT('',(202.387277625415,595.670681589213,-40.2721601717608)) ;
#70192 = CARTESIAN_POINT('Origin',(202.262277625405,579.482556589212,-40.2721601717609)) ;
#70193 = CARTESIAN_POINT('Origin',(202.262277625405,579.482556589212,-40.2721601717609)) ;
#70194 = CARTESIAN_POINT('Origin',(201.559777625415,578.462556589212,-42.3117150424525)) ;
#70195 = CARTESIAN_POINT('',(201.434777625415,578.462556589212,-39.4182700580611)) ;
#70196 = CARTESIAN_POINT('',(201.434777625415,578.462556589212,-42.3117150424525)) ;
#70197 = CARTESIAN_POINT('',(201.559777625416,578.337556589212,-39.4182700580611)) ;
#70198 = CARTESIAN_POINT('Origin',(201.559777625415,578.462556589212,-39.4182700580611)) ;
#70199 = CARTESIAN_POINT('',(201.559777625416,578.337556589212,-42.3117150424525)) ;
#70200 = CARTESIAN_POINT('Origin',(201.434777625415,574.368806589211,-43.1012690928543)) ;
#70201 = CARTESIAN_POINT('',(201.434777625415,579.482556589212,-39.4182700580611)) ;
#70202 = CARTESIAN_POINT('',(201.434777625415,579.482556589212,-44.5342150424525)) ;
#70203 = CARTESIAN_POINT('',(201.434777625415,579.671056589212,-39.2297700580612)) ;
#70204 = CARTESIAN_POINT('Origin',(201.434777625415,579.671056589212,-39.4182700580612)) ;
#70205 = CARTESIAN_POINT('',(201.434777625415,580.847556589211,-39.2297700580612)) ;
#70206 = CARTESIAN_POINT('',(201.434777625415,576.988181589211,-39.2297700580612)) ;
#70207 = CARTESIAN_POINT('',(201.434777625407,580.847556589211,-35.2721601717607)) ;
#70208 = CARTESIAN_POINT('',(201.434777625415,580.847556589211,-38.5610190928544)) ;
#70209 = CARTESIAN_POINT('',(201.434777625407,577.097556589211,-35.2721601717609)) ;
#70210 = CARTESIAN_POINT('',(201.434777625415,595.670681589221,-35.2721601717607)) ;
#70211 = CARTESIAN_POINT('',(201.434777625415,577.097556589211,-39.2297700580612)) ;
#70212 = CARTESIAN_POINT('',(201.434777625415,577.097556589211,-40.5297040214914)) ;
#70213 = CARTESIAN_POINT('',(201.434777625415,578.274056589212,-39.2297700580612)) ;
#70214 = CARTESIAN_POINT('',(201.434777625415,576.988181589211,-39.2297700580612)) ;
#70215 = CARTESIAN_POINT('Origin',(201.434777625415,578.274056589212,-39.4182700580611)) ;
#70216 = CARTESIAN_POINT('Origin',(201.559777625415,579.482556589212,-44.5342150424525)) ;
#70217 = CARTESIAN_POINT('',(201.559777625415,579.607556589212,-39.4182700580612)) ;
#70218 = CARTESIAN_POINT('',(201.559777625415,579.607556589212,-44.5342150424525)) ;
#70219 = CARTESIAN_POINT('Origin',(201.559777625415,579.482556589212,-39.4182700580611)) ;
#70220 = CARTESIAN_POINT('Origin',(218.198777625414,579.607556589212,-45.9671609920506)) ;
#70221 = CARTESIAN_POINT('',(202.262277625415,579.607556589212,-39.4182700580612)) ;
#70222 = CARTESIAN_POINT('',(202.262277625415,579.607556589212,-39.8669650424525)) ;
#70223 = CARTESIAN_POINT('',(218.198777625414,579.607556589212,-39.4182700580611)) ;
#70224 = CARTESIAN_POINT('Origin',(212.018652625408,570.357556589212,-40.2721601717612)) ;
#70225 = CARTESIAN_POINT('',(202.262277625405,570.107556589212,-40.2721601717608)) ;
#70226 = CARTESIAN_POINT('Origin',(202.262277625405,570.357556589212,-40.2721601717608)) ;
#70227 = CARTESIAN_POINT('',(201.559777625406,570.107556589212,-40.2721601717607)) ;
#70228 = CARTESIAN_POINT('',(212.018652625408,570.107556589212,-40.2721601717612)) ;
#70229 = CARTESIAN_POINT('Origin',(201.559777625406,570.357556589212,-40.2721601717607)) ;
#70230 = CARTESIAN_POINT('Origin',(201.559777625406,569.982556589212,-40.2721601717609)) ;
#70231 = CARTESIAN_POINT('',(201.434777625406,569.982556589212,-40.2721601717609)) ;
#70232 = CARTESIAN_POINT('Origin',(201.184777625406,569.982556589212,-40.2721601717609)) ;
#70233 = CARTESIAN_POINT('Origin',(201.559777625406,569.982556589212,-40.2721601717609)) ;
#70234 = CARTESIAN_POINT('Origin',(201.184777625406,586.170681589212,-40.2721601717607)) ;
#70235 = CARTESIAN_POINT('',(201.434777625406,568.962556589212,-40.2721601717607)) ;
#70236 = CARTESIAN_POINT('Origin',(201.184777625406,568.962556589212,-40.2721601717607)) ;
#70237 = CARTESIAN_POINT('',(201.434777625414,586.170681589212,-40.2721601717607)) ;
#70238 = CARTESIAN_POINT('Origin',(201.559777625406,568.962556589212,-40.2721601717609)) ;
#70239 = CARTESIAN_POINT('',(201.559777625406,568.837556589212,-40.2721601717609)) ;
#70240 = CARTESIAN_POINT('Origin',(201.559777625406,568.587556589212,-40.2721601717609)) ;
#70241 = CARTESIAN_POINT('Origin',(201.559777625406,568.962556589212,-40.2721601717609)) ;
#70242 = CARTESIAN_POINT('Origin',(212.844152625408,568.587556589212,-40.2721601717612)) ;
#70243 = CARTESIAN_POINT('',(202.262277625405,568.837556589212,-40.2721601717608)) ;
#70244 = CARTESIAN_POINT('Origin',(202.262277625405,568.587556589212,-40.2721601717608)) ;
#70245 = CARTESIAN_POINT('',(212.844152625408,568.837556589212,-40.2721601717612)) ;
#70246 = CARTESIAN_POINT('Origin',(202.262277625405,568.962556589212,-40.2721601717609)) ;
#70247 = CARTESIAN_POINT('',(202.387277625405,568.962556589212,-40.2721601717609)) ;
#70248 = CARTESIAN_POINT('Origin',(202.637277625405,568.962556589212,-40.2721601717609)) ;
#70249 = CARTESIAN_POINT('Origin',(202.262277625405,568.962556589212,-40.2721601717609)) ;
#70250 = CARTESIAN_POINT('Origin',(202.637277625405,586.170681589213,-40.2721601717608)) ;
#70251 = CARTESIAN_POINT('',(202.387277625405,569.982556589212,-40.2721601717608)) ;
#70252 = CARTESIAN_POINT('Origin',(202.637277625405,569.982556589212,-40.2721601717608)) ;
#70253 = CARTESIAN_POINT('',(202.387277625413,586.170681589213,-40.2721601717608)) ;
#70254 = CARTESIAN_POINT('Origin',(202.262277625405,569.982556589212,-40.2721601717609)) ;
#70255 = CARTESIAN_POINT('Origin',(202.262277625405,569.982556589212,-40.2721601717609)) ;
#70256 = CARTESIAN_POINT('Origin',(201.559777625414,568.962556589212,-42.3117150424525)) ;
#70257 = CARTESIAN_POINT('',(201.434777625414,568.962556589212,-39.4182700580611)) ;
#70258 = CARTESIAN_POINT('',(201.434777625414,568.962556589212,-42.3117150424525)) ;
#70259 = CARTESIAN_POINT('',(201.559777625414,568.837556589212,-39.4182700580611)) ;
#70260 = CARTESIAN_POINT('Origin',(201.559777625414,568.962556589212,-39.4182700580611)) ;
#70261 = CARTESIAN_POINT('',(201.559777625414,568.837556589212,-42.3117150424525)) ;
#70262 = CARTESIAN_POINT('Origin',(201.434777625414,564.868806589211,-43.1012690928543)) ;
#70263 = CARTESIAN_POINT('',(201.434777625414,569.982556589212,-39.4182700580611)) ;
#70264 = CARTESIAN_POINT('',(201.434777625414,569.982556589212,-44.5342150424525)) ;
#70265 = CARTESIAN_POINT('',(201.434777625414,570.171056589212,-39.2297700580612)) ;
#70266 = CARTESIAN_POINT('Origin',(201.434777625414,570.171056589212,-39.4182700580612)) ;
#70267 = CARTESIAN_POINT('',(201.434777625414,571.347556589211,-39.2297700580612)) ;
#70268 = CARTESIAN_POINT('',(201.434777625414,567.488181589211,-39.2297700580612)) ;
#70269 = CARTESIAN_POINT('',(201.434777625407,571.347556589211,-35.2721601717607)) ;
#70270 = CARTESIAN_POINT('',(201.434777625414,571.347556589211,-38.5610190928544)) ;
#70271 = CARTESIAN_POINT('',(201.434777625407,567.597556589211,-35.2721601717609)) ;
#70272 = CARTESIAN_POINT('',(201.434777625414,586.170681589221,-35.2721601717607)) ;
#70273 = CARTESIAN_POINT('',(201.434777625414,567.59755658921,-39.2297700580612)) ;
#70274 = CARTESIAN_POINT('',(201.434777625414,567.59755658921,-40.5297040214914)) ;
#70275 = CARTESIAN_POINT('',(201.434777625414,568.774056589212,-39.2297700580612)) ;
#70276 = CARTESIAN_POINT('',(201.434777625414,567.488181589211,-39.2297700580612)) ;
#70277 = CARTESIAN_POINT('Origin',(201.434777625414,568.774056589212,-39.4182700580611)) ;
#70278 = CARTESIAN_POINT('Origin',(201.559777625414,569.982556589212,-44.5342150424525)) ;
#70279 = CARTESIAN_POINT('',(201.559777625414,570.107556589212,-39.4182700580612)) ;
#70280 = CARTESIAN_POINT('',(201.559777625414,570.107556589212,-44.5342150424525)) ;
#70281 = CARTESIAN_POINT('Origin',(201.559777625414,569.982556589212,-39.4182700580611)) ;
#70282 = CARTESIAN_POINT('Origin',(218.198777625412,570.107556589212,-45.9671609920506)) ;
#70283 = CARTESIAN_POINT('',(202.262277625413,570.107556589212,-39.4182700580612)) ;
#70284 = CARTESIAN_POINT('',(202.262277625413,570.107556589212,-39.8669650424525)) ;
#70285 = CARTESIAN_POINT('',(218.198777625413,570.107556589212,-39.4182700580611)) ;
#70286 = CARTESIAN_POINT('Origin',(212.018652625409,560.857556589212,-40.2721601717612)) ;
#70287 = CARTESIAN_POINT('',(202.262277625406,560.607556589212,-40.2721601717608)) ;
#70288 = CARTESIAN_POINT('Origin',(202.262277625406,560.857556589212,-40.2721601717608)) ;
#70289 = CARTESIAN_POINT('',(201.559777625406,560.607556589212,-40.2721601717607)) ;
#70290 = CARTESIAN_POINT('',(212.018652625409,560.607556589212,-40.2721601717612)) ;
#70291 = CARTESIAN_POINT('Origin',(201.559777625406,560.857556589212,-40.2721601717607)) ;
#70292 = CARTESIAN_POINT('Origin',(201.559777625406,560.482556589212,-40.2721601717609)) ;
#70293 = CARTESIAN_POINT('',(201.434777625406,560.482556589212,-40.2721601717609)) ;
#70294 = CARTESIAN_POINT('Origin',(201.184777625406,560.482556589212,-40.2721601717609)) ;
#70295 = CARTESIAN_POINT('Origin',(201.559777625406,560.482556589212,-40.2721601717609)) ;
#70296 = CARTESIAN_POINT('Origin',(201.184777625406,576.670681589212,-40.2721601717607)) ;
#70297 = CARTESIAN_POINT('',(201.434777625406,559.462556589212,-40.2721601717607)) ;
#70298 = CARTESIAN_POINT('Origin',(201.184777625406,559.462556589212,-40.2721601717607)) ;
#70299 = CARTESIAN_POINT('',(201.434777625412,576.670681589212,-40.2721601717607)) ;
#70300 = CARTESIAN_POINT('Origin',(201.559777625406,559.462556589212,-40.2721601717609)) ;
#70301 = CARTESIAN_POINT('',(201.559777625406,559.337556589212,-40.2721601717609)) ;
#70302 = CARTESIAN_POINT('Origin',(201.559777625406,559.087556589212,-40.2721601717609)) ;
#70303 = CARTESIAN_POINT('Origin',(201.559777625406,559.462556589212,-40.2721601717609)) ;
#70304 = CARTESIAN_POINT('Origin',(212.844152625408,559.087556589212,-40.2721601717612)) ;
#70305 = CARTESIAN_POINT('',(202.262277625406,559.337556589212,-40.2721601717608)) ;
#70306 = CARTESIAN_POINT('Origin',(202.262277625406,559.087556589212,-40.2721601717608)) ;
#70307 = CARTESIAN_POINT('',(212.844152625408,559.337556589212,-40.2721601717612)) ;
#70308 = CARTESIAN_POINT('Origin',(202.262277625406,559.462556589212,-40.2721601717609)) ;
#70309 = CARTESIAN_POINT('',(202.387277625406,559.462556589212,-40.2721601717609)) ;
#70310 = CARTESIAN_POINT('Origin',(202.637277625406,559.462556589212,-40.2721601717609)) ;
#70311 = CARTESIAN_POINT('Origin',(202.262277625406,559.462556589212,-40.2721601717609)) ;
#70312 = CARTESIAN_POINT('Origin',(202.637277625406,576.670681589213,-40.2721601717608)) ;
#70313 = CARTESIAN_POINT('',(202.387277625406,560.482556589212,-40.2721601717608)) ;
#70314 = CARTESIAN_POINT('Origin',(202.637277625406,560.482556589212,-40.2721601717608)) ;
#70315 = CARTESIAN_POINT('',(202.387277625412,576.670681589213,-40.2721601717608)) ;
#70316 = CARTESIAN_POINT('Origin',(202.262277625406,560.482556589212,-40.2721601717609)) ;
#70317 = CARTESIAN_POINT('Origin',(202.262277625406,560.482556589212,-40.2721601717609)) ;
#70318 = CARTESIAN_POINT('Origin',(201.559777625412,559.462556589212,-42.3117150424525)) ;
#70319 = CARTESIAN_POINT('',(201.434777625412,559.462556589212,-39.4182700580611)) ;
#70320 = CARTESIAN_POINT('',(201.434777625412,559.462556589212,-42.3117150424525)) ;
#70321 = CARTESIAN_POINT('',(201.559777625412,559.337556589212,-39.4182700580611)) ;
#70322 = CARTESIAN_POINT('Origin',(201.559777625412,559.462556589212,-39.4182700580611)) ;
#70323 = CARTESIAN_POINT('',(201.559777625412,559.337556589212,-42.3117150424525)) ;
#70324 = CARTESIAN_POINT('Origin',(201.434777625412,555.368806589211,-43.1012690928543)) ;
#70325 = CARTESIAN_POINT('',(201.434777625412,560.482556589212,-39.4182700580611)) ;
#70326 = CARTESIAN_POINT('',(201.434777625412,560.482556589212,-44.5342150424525)) ;
#70327 = CARTESIAN_POINT('',(201.434777625412,560.671056589212,-39.2297700580612)) ;
#70328 = CARTESIAN_POINT('Origin',(201.434777625412,560.671056589212,-39.4182700580612)) ;
#70329 = CARTESIAN_POINT('',(201.434777625412,561.847556589211,-39.2297700580612)) ;
#70330 = CARTESIAN_POINT('',(201.434777625412,557.988181589211,-39.2297700580612)) ;
#70331 = CARTESIAN_POINT('',(201.434777625407,561.847556589211,-35.2721601717607)) ;
#70332 = CARTESIAN_POINT('',(201.434777625412,561.847556589211,-38.5610190928544)) ;
#70333 = CARTESIAN_POINT('',(201.434777625407,558.097556589211,-35.2721601717609)) ;
#70334 = CARTESIAN_POINT('',(201.434777625412,576.670681589221,-35.2721601717607)) ;
#70335 = CARTESIAN_POINT('',(201.434777625412,558.097556589211,-39.2297700580612)) ;
#70336 = CARTESIAN_POINT('',(201.434777625412,558.097556589211,-40.5297040214914)) ;
#70337 = CARTESIAN_POINT('',(201.434777625412,559.274056589212,-39.2297700580612)) ;
#70338 = CARTESIAN_POINT('',(201.434777625412,557.988181589211,-39.2297700580612)) ;
#70339 = CARTESIAN_POINT('Origin',(201.434777625412,559.274056589212,-39.4182700580611)) ;
#70340 = CARTESIAN_POINT('Origin',(201.559777625412,560.482556589212,-44.5342150424525)) ;
#70341 = CARTESIAN_POINT('',(201.559777625412,560.607556589212,-39.4182700580612)) ;
#70342 = CARTESIAN_POINT('',(201.559777625412,560.607556589212,-44.5342150424525)) ;
#70343 = CARTESIAN_POINT('Origin',(201.559777625412,560.482556589212,-39.4182700580611)) ;
#70344 = CARTESIAN_POINT('Origin',(218.198777625411,560.607556589212,-45.9671609920506)) ;
#70345 = CARTESIAN_POINT('',(202.262277625412,560.607556589212,-39.4182700580612)) ;
#70346 = CARTESIAN_POINT('',(202.262277625412,560.607556589212,-39.8669650424525)) ;
#70347 = CARTESIAN_POINT('',(218.198777625411,560.607556589212,-39.4182700580611)) ;
#70348 = CARTESIAN_POINT('Origin',(212.018652625409,551.357556589212,-40.2721601717612)) ;
#70349 = CARTESIAN_POINT('',(202.262277625406,551.107556589212,-40.2721601717608)) ;
#70350 = CARTESIAN_POINT('Origin',(202.262277625406,551.357556589212,-40.2721601717608)) ;
#70351 = CARTESIAN_POINT('',(201.559777625406,551.107556589212,-40.2721601717607)) ;
#70352 = CARTESIAN_POINT('',(212.018652625409,551.107556589212,-40.2721601717612)) ;
#70353 = CARTESIAN_POINT('Origin',(201.559777625406,551.357556589212,-40.2721601717607)) ;
#70354 = CARTESIAN_POINT('Origin',(201.559777625406,550.982556589212,-40.2721601717609)) ;
#70355 = CARTESIAN_POINT('',(201.434777625406,550.982556589212,-40.2721601717609)) ;
#70356 = CARTESIAN_POINT('Origin',(201.184777625406,550.982556589212,-40.2721601717609)) ;
#70357 = CARTESIAN_POINT('Origin',(201.559777625406,550.982556589212,-40.2721601717609)) ;
#70358 = CARTESIAN_POINT('Origin',(201.184777625406,567.170681589212,-40.2721601717607)) ;
#70359 = CARTESIAN_POINT('',(201.434777625406,549.962556589212,-40.2721601717607)) ;
#70360 = CARTESIAN_POINT('Origin',(201.184777625406,549.962556589212,-40.2721601717607)) ;
#70361 = CARTESIAN_POINT('',(201.43477762541,567.170681589212,-40.2721601717607)) ;
#70362 = CARTESIAN_POINT('Origin',(201.559777625406,549.962556589212,-40.2721601717609)) ;
#70363 = CARTESIAN_POINT('',(201.559777625407,549.837556589212,-40.2721601717609)) ;
#70364 = CARTESIAN_POINT('Origin',(201.559777625407,549.587556589212,-40.2721601717609)) ;
#70365 = CARTESIAN_POINT('Origin',(201.559777625406,549.962556589212,-40.2721601717609)) ;
#70366 = CARTESIAN_POINT('Origin',(212.844152625409,549.587556589212,-40.2721601717612)) ;
#70367 = CARTESIAN_POINT('',(202.262277625406,549.837556589212,-40.2721601717608)) ;
#70368 = CARTESIAN_POINT('Origin',(202.262277625406,549.587556589212,-40.2721601717608)) ;
#70369 = CARTESIAN_POINT('',(212.844152625409,549.837556589212,-40.2721601717612)) ;
#70370 = CARTESIAN_POINT('Origin',(202.262277625406,549.962556589212,-40.2721601717609)) ;
#70371 = CARTESIAN_POINT('',(202.387277625406,549.962556589212,-40.2721601717609)) ;
#70372 = CARTESIAN_POINT('Origin',(202.637277625406,549.962556589212,-40.2721601717609)) ;
#70373 = CARTESIAN_POINT('Origin',(202.262277625406,549.962556589212,-40.2721601717609)) ;
#70374 = CARTESIAN_POINT('Origin',(202.637277625406,567.170681589213,-40.2721601717608)) ;
#70375 = CARTESIAN_POINT('',(202.387277625406,550.982556589212,-40.2721601717608)) ;
#70376 = CARTESIAN_POINT('Origin',(202.637277625406,550.982556589212,-40.2721601717608)) ;
#70377 = CARTESIAN_POINT('',(202.38727762541,567.170681589213,-40.2721601717608)) ;
#70378 = CARTESIAN_POINT('Origin',(202.262277625406,550.982556589212,-40.2721601717609)) ;
#70379 = CARTESIAN_POINT('Origin',(202.262277625406,550.982556589212,-40.2721601717609)) ;
#70380 = CARTESIAN_POINT('Origin',(201.55977762541,549.962556589212,-42.3117150424525)) ;
#70381 = CARTESIAN_POINT('',(201.43477762541,549.962556589212,-39.4182700580611)) ;
#70382 = CARTESIAN_POINT('',(201.43477762541,549.962556589212,-42.3117150424525)) ;
#70383 = CARTESIAN_POINT('',(201.55977762541,549.837556589212,-39.4182700580611)) ;
#70384 = CARTESIAN_POINT('Origin',(201.55977762541,549.962556589212,-39.4182700580611)) ;
#70385 = CARTESIAN_POINT('',(201.55977762541,549.837556589212,-42.3117150424525)) ;
#70386 = CARTESIAN_POINT('Origin',(201.43477762541,545.868806589211,-43.1012690928543)) ;
#70387 = CARTESIAN_POINT('',(201.43477762541,550.982556589212,-39.4182700580611)) ;
#70388 = CARTESIAN_POINT('',(201.43477762541,550.982556589212,-44.5342150424525)) ;
#70389 = CARTESIAN_POINT('',(201.43477762541,551.171056589212,-39.2297700580612)) ;
#70390 = CARTESIAN_POINT('Origin',(201.43477762541,551.171056589212,-39.4182700580612)) ;
#70391 = CARTESIAN_POINT('',(201.43477762541,552.347556589211,-39.2297700580612)) ;
#70392 = CARTESIAN_POINT('',(201.43477762541,548.488181589211,-39.2297700580612)) ;
#70393 = CARTESIAN_POINT('',(201.434777625407,552.347556589211,-35.2721601717607)) ;
#70394 = CARTESIAN_POINT('',(201.43477762541,552.347556589211,-38.5610190928544)) ;
#70395 = CARTESIAN_POINT('',(201.434777625407,548.59755658921,-35.2721601717609)) ;
#70396 = CARTESIAN_POINT('',(201.43477762541,567.170681589221,-35.2721601717607)) ;
#70397 = CARTESIAN_POINT('',(201.43477762541,548.59755658921,-39.2297700580612)) ;
#70398 = CARTESIAN_POINT('',(201.43477762541,548.59755658921,-40.5297040214914)) ;
#70399 = CARTESIAN_POINT('',(201.43477762541,549.774056589212,-39.2297700580612)) ;
#70400 = CARTESIAN_POINT('',(201.43477762541,548.488181589211,-39.2297700580612)) ;
#70401 = CARTESIAN_POINT('Origin',(201.43477762541,549.774056589212,-39.4182700580611)) ;
#70402 = CARTESIAN_POINT('Origin',(201.55977762541,550.982556589212,-44.5342150424525)) ;
#70403 = CARTESIAN_POINT('',(201.55977762541,551.107556589212,-39.4182700580612)) ;
#70404 = CARTESIAN_POINT('',(201.55977762541,551.107556589212,-44.5342150424525)) ;
#70405 = CARTESIAN_POINT('Origin',(201.55977762541,550.982556589212,-39.4182700580611)) ;
#70406 = CARTESIAN_POINT('Origin',(218.198777625409,551.107556589212,-45.9671609920506)) ;
#70407 = CARTESIAN_POINT('',(202.26227762541,551.107556589212,-39.4182700580612)) ;
#70408 = CARTESIAN_POINT('',(202.26227762541,551.107556589212,-39.8669650424525)) ;
#70409 = CARTESIAN_POINT('',(218.198777625409,551.107556589212,-39.4182700580611)) ;
#70410 = CARTESIAN_POINT('Origin',(212.018652625409,541.857556589212,-40.2721601717612)) ;
#70411 = CARTESIAN_POINT('',(202.262277625406,541.607556589212,-40.2721601717608)) ;
#70412 = CARTESIAN_POINT('Origin',(202.262277625406,541.857556589212,-40.2721601717608)) ;
#70413 = CARTESIAN_POINT('',(201.559777625407,541.607556589212,-40.2721601717607)) ;
#70414 = CARTESIAN_POINT('',(212.018652625409,541.607556589212,-40.2721601717612)) ;
#70415 = CARTESIAN_POINT('Origin',(201.559777625407,541.857556589212,-40.2721601717607)) ;
#70416 = CARTESIAN_POINT('Origin',(201.559777625407,541.482556589212,-40.2721601717609)) ;
#70417 = CARTESIAN_POINT('',(201.434777625407,541.482556589212,-40.2721601717609)) ;
#70418 = CARTESIAN_POINT('Origin',(201.184777625407,541.482556589212,-40.2721601717609)) ;
#70419 = CARTESIAN_POINT('Origin',(201.559777625407,541.482556589212,-40.2721601717609)) ;
#70420 = CARTESIAN_POINT('Origin',(201.184777625407,557.670681589212,-40.2721601717607)) ;
#70421 = CARTESIAN_POINT('',(201.434777625407,540.462556589212,-40.2721601717607)) ;
#70422 = CARTESIAN_POINT('Origin',(201.184777625407,540.462556589212,-40.2721601717607)) ;
#70423 = CARTESIAN_POINT('',(201.434777625409,557.670681589212,-40.2721601717607)) ;
#70424 = CARTESIAN_POINT('Origin',(201.559777625407,540.462556589212,-40.2721601717609)) ;
#70425 = CARTESIAN_POINT('',(201.559777625407,540.337556589212,-40.2721601717609)) ;
#70426 = CARTESIAN_POINT('Origin',(201.559777625407,540.087556589212,-40.2721601717609)) ;
#70427 = CARTESIAN_POINT('Origin',(201.559777625407,540.462556589212,-40.2721601717609)) ;
#70428 = CARTESIAN_POINT('Origin',(212.844152625409,540.087556589212,-40.2721601717612)) ;
#70429 = CARTESIAN_POINT('',(202.262277625406,540.337556589212,-40.2721601717608)) ;
#70430 = CARTESIAN_POINT('Origin',(202.262277625406,540.087556589212,-40.2721601717608)) ;
#70431 = CARTESIAN_POINT('',(212.844152625409,540.337556589212,-40.2721601717612)) ;
#70432 = CARTESIAN_POINT('Origin',(202.262277625406,540.462556589212,-40.2721601717609)) ;
#70433 = CARTESIAN_POINT('',(202.387277625406,540.462556589212,-40.2721601717609)) ;
#70434 = CARTESIAN_POINT('Origin',(202.637277625406,540.462556589212,-40.2721601717609)) ;
#70435 = CARTESIAN_POINT('Origin',(202.262277625406,540.462556589212,-40.2721601717609)) ;
#70436 = CARTESIAN_POINT('Origin',(202.637277625406,557.670681589212,-40.2721601717608)) ;
#70437 = CARTESIAN_POINT('',(202.387277625406,541.482556589212,-40.2721601717608)) ;
#70438 = CARTESIAN_POINT('Origin',(202.637277625406,541.482556589212,-40.2721601717608)) ;
#70439 = CARTESIAN_POINT('',(202.387277625408,557.670681589212,-40.2721601717608)) ;
#70440 = CARTESIAN_POINT('Origin',(202.262277625406,541.482556589212,-40.2721601717609)) ;
#70441 = CARTESIAN_POINT('Origin',(202.262277625406,541.482556589212,-40.2721601717609)) ;
#70442 = CARTESIAN_POINT('Origin',(201.559777625409,540.462556589212,-42.3117150424525)) ;
#70443 = CARTESIAN_POINT('',(201.434777625409,540.462556589212,-39.4182700580611)) ;
#70444 = CARTESIAN_POINT('',(201.434777625409,540.462556589212,-42.3117150424525)) ;
#70445 = CARTESIAN_POINT('',(201.559777625409,540.337556589212,-39.4182700580611)) ;
#70446 = CARTESIAN_POINT('Origin',(201.559777625409,540.462556589212,-39.4182700580611)) ;
#70447 = CARTESIAN_POINT('',(201.559777625409,540.337556589212,-42.3117150424525)) ;
#70448 = CARTESIAN_POINT('Origin',(201.434777625409,536.368806589211,-43.1012690928543)) ;
#70449 = CARTESIAN_POINT('',(201.434777625409,541.482556589212,-39.4182700580611)) ;
#70450 = CARTESIAN_POINT('',(201.434777625409,541.482556589212,-44.5342150424525)) ;
#70451 = CARTESIAN_POINT('',(201.434777625409,541.671056589212,-39.2297700580612)) ;
#70452 = CARTESIAN_POINT('Origin',(201.434777625409,541.671056589212,-39.4182700580612)) ;
#70453 = CARTESIAN_POINT('',(201.434777625409,542.847556589211,-39.2297700580612)) ;
#70454 = CARTESIAN_POINT('',(201.434777625409,538.988181589211,-39.2297700580612)) ;
#70455 = CARTESIAN_POINT('',(201.434777625407,542.847556589211,-35.2721601717607)) ;
#70456 = CARTESIAN_POINT('',(201.434777625409,542.847556589211,-38.5610190928544)) ;
#70457 = CARTESIAN_POINT('',(201.434777625407,539.09755658921,-35.2721601717609)) ;
#70458 = CARTESIAN_POINT('',(201.434777625409,557.670681589221,-35.2721601717607)) ;
#70459 = CARTESIAN_POINT('',(201.434777625409,539.09755658921,-39.2297700580612)) ;
#70460 = CARTESIAN_POINT('',(201.434777625409,539.09755658921,-40.5297040214914)) ;
#70461 = CARTESIAN_POINT('',(201.434777625409,540.274056589212,-39.2297700580612)) ;
#70462 = CARTESIAN_POINT('',(201.434777625409,538.988181589211,-39.2297700580612)) ;
#70463 = CARTESIAN_POINT('Origin',(201.434777625409,540.274056589212,-39.4182700580611)) ;
#70464 = CARTESIAN_POINT('Origin',(201.559777625409,541.482556589212,-44.5342150424525)) ;
#70465 = CARTESIAN_POINT('',(201.559777625409,541.607556589212,-39.4182700580612)) ;
#70466 = CARTESIAN_POINT('',(201.559777625409,541.607556589212,-44.5342150424525)) ;
#70467 = CARTESIAN_POINT('Origin',(201.559777625409,541.482556589212,-39.4182700580611)) ;
#70468 = CARTESIAN_POINT('Origin',(218.198777625407,541.607556589212,-45.9671609920506)) ;
#70469 = CARTESIAN_POINT('',(202.262277625408,541.607556589212,-39.4182700580612)) ;
#70470 = CARTESIAN_POINT('',(202.262277625408,541.607556589212,-39.8669650424525)) ;
#70471 = CARTESIAN_POINT('',(218.198777625408,541.607556589212,-39.4182700580611)) ;
#70472 = CARTESIAN_POINT('Origin',(212.01865262541,532.357556589212,-40.2721601717612)) ;
#70473 = CARTESIAN_POINT('',(202.262277625407,532.107556589212,-40.2721601717608)) ;
#70474 = CARTESIAN_POINT('Origin',(202.262277625407,532.357556589212,-40.2721601717608)) ;
#70475 = CARTESIAN_POINT('',(201.559777625407,532.107556589212,-40.2721601717607)) ;
#70476 = CARTESIAN_POINT('',(212.01865262541,532.107556589212,-40.2721601717612)) ;
#70477 = CARTESIAN_POINT('Origin',(201.559777625407,532.357556589212,-40.2721601717607)) ;
#70478 = CARTESIAN_POINT('Origin',(201.559777625407,531.982556589212,-40.2721601717609)) ;
#70479 = CARTESIAN_POINT('',(201.434777625407,531.982556589212,-40.2721601717609)) ;
#70480 = CARTESIAN_POINT('Origin',(201.184777625407,531.982556589212,-40.2721601717609)) ;
#70481 = CARTESIAN_POINT('Origin',(201.559777625407,531.982556589212,-40.2721601717609)) ;
#70482 = CARTESIAN_POINT('Origin',(201.184777625407,548.170681589212,-40.2721601717607)) ;
#70483 = CARTESIAN_POINT('',(201.434777625407,530.962556589212,-40.2721601717607)) ;
#70484 = CARTESIAN_POINT('Origin',(201.184777625407,530.962556589212,-40.2721601717607)) ;
#70485 = CARTESIAN_POINT('',(201.434777625407,548.170681589212,-40.2721601717607)) ;
#70486 = CARTESIAN_POINT('Origin',(201.559777625407,530.962556589212,-40.2721601717609)) ;
#70487 = CARTESIAN_POINT('',(201.559777625407,530.837556589212,-40.2721601717609)) ;
#70488 = CARTESIAN_POINT('Origin',(201.559777625407,530.587556589212,-40.2721601717609)) ;
#70489 = CARTESIAN_POINT('Origin',(201.559777625407,530.962556589212,-40.2721601717609)) ;
#70490 = CARTESIAN_POINT('Origin',(212.844152625409,530.587556589212,-40.2721601717612)) ;
#70491 = CARTESIAN_POINT('',(202.262277625407,530.837556589212,-40.2721601717608)) ;
#70492 = CARTESIAN_POINT('Origin',(202.262277625407,530.587556589212,-40.2721601717608)) ;
#70493 = CARTESIAN_POINT('',(212.844152625409,530.837556589212,-40.2721601717612)) ;
#70494 = CARTESIAN_POINT('Origin',(202.262277625407,530.962556589212,-40.2721601717609)) ;
#70495 = CARTESIAN_POINT('',(202.387277625407,530.962556589212,-40.2721601717609)) ;
#70496 = CARTESIAN_POINT('Origin',(202.637277625407,530.962556589212,-40.2721601717609)) ;
#70497 = CARTESIAN_POINT('Origin',(202.262277625407,530.962556589212,-40.2721601717609)) ;
#70498 = CARTESIAN_POINT('Origin',(202.637277625407,548.170681589212,-40.2721601717608)) ;
#70499 = CARTESIAN_POINT('',(202.387277625407,531.982556589212,-40.2721601717608)) ;
#70500 = CARTESIAN_POINT('Origin',(202.637277625407,531.982556589212,-40.2721601717608)) ;
#70501 = CARTESIAN_POINT('',(202.387277625407,548.170681589212,-40.2721601717608)) ;
#70502 = CARTESIAN_POINT('Origin',(202.262277625407,531.982556589212,-40.2721601717609)) ;
#70503 = CARTESIAN_POINT('Origin',(202.262277625407,531.982556589212,-40.2721601717609)) ;
#70504 = CARTESIAN_POINT('Origin',(201.559777625407,530.962556589212,-42.3117150424525)) ;
#70505 = CARTESIAN_POINT('',(201.434777625407,530.962556589212,-39.4182700580611)) ;
#70506 = CARTESIAN_POINT('',(201.434777625407,530.962556589212,-42.3117150424525)) ;
#70507 = CARTESIAN_POINT('',(201.559777625407,530.837556589212,-39.4182700580611)) ;
#70508 = CARTESIAN_POINT('Origin',(201.559777625407,530.962556589212,-39.4182700580611)) ;
#70509 = CARTESIAN_POINT('',(201.559777625407,530.837556589212,-42.3117150424525)) ;
#70510 = CARTESIAN_POINT('Origin',(201.434777625407,526.868806589211,-43.1012690928543)) ;
#70511 = CARTESIAN_POINT('',(201.434777625407,529.59755658921,-35.2721601717609)) ;
#70512 = CARTESIAN_POINT('',(201.434777625407,533.347556589211,-35.2721601717607)) ;
#70513 = CARTESIAN_POINT('',(201.434777625407,548.170681589221,-35.2721601717607)) ;
#70514 = CARTESIAN_POINT('',(201.434777625407,529.59755658921,-39.2297700580612)) ;
#70515 = CARTESIAN_POINT('',(201.434777625407,529.59755658921,-40.5297040214914)) ;
#70516 = CARTESIAN_POINT('',(201.434777625407,530.774056589212,-39.2297700580612)) ;
#70517 = CARTESIAN_POINT('',(201.434777625407,529.488181589211,-39.2297700580612)) ;
#70518 = CARTESIAN_POINT('Origin',(201.434777625407,530.774056589212,-39.4182700580611)) ;
#70519 = CARTESIAN_POINT('',(201.434777625407,531.982556589212,-39.4182700580611)) ;
#70520 = CARTESIAN_POINT('',(201.434777625407,531.982556589212,-44.5342150424525)) ;
#70521 = CARTESIAN_POINT('',(201.434777625407,532.171056589212,-39.2297700580612)) ;
#70522 = CARTESIAN_POINT('Origin',(201.434777625407,532.171056589212,-39.4182700580612)) ;
#70523 = CARTESIAN_POINT('',(201.434777625407,533.347556589211,-39.2297700580612)) ;
#70524 = CARTESIAN_POINT('',(201.434777625407,529.488181589211,-39.2297700580612)) ;
#70525 = CARTESIAN_POINT('',(201.434777625407,533.347556589211,-38.5610190928544)) ;
#70526 = CARTESIAN_POINT('Origin',(201.559777625407,531.982556589212,-44.5342150424525)) ;
#70527 = CARTESIAN_POINT('',(201.559777625407,532.107556589212,-39.4182700580612)) ;
#70528 = CARTESIAN_POINT('',(201.559777625407,532.107556589212,-44.5342150424525)) ;
#70529 = CARTESIAN_POINT('Origin',(201.559777625407,531.982556589212,-39.4182700580611)) ;
#70530 = CARTESIAN_POINT('Origin',(218.198777625406,532.107556589212,-45.9671609920506)) ;
#70531 = CARTESIAN_POINT('',(202.262277625407,532.107556589212,-39.4182700580612)) ;
#70532 = CARTESIAN_POINT('',(202.262277625407,532.107556589212,-39.8669650424525)) ;
#70533 = CARTESIAN_POINT('',(218.198777625406,532.107556589212,-39.4182700580611)) ;
#70534 = CARTESIAN_POINT('Origin',(201.57290262541,609.722556589211,-35.2721601717607)) ;
#70535 = CARTESIAN_POINT('',(209.814777625407,609.722556589211,-35.0221601717611)) ;
#70536 = CARTESIAN_POINT('',(209.814777625407,609.472556589211,-35.2721601717611)) ;
#70537 = CARTESIAN_POINT('Origin',(209.814777625407,609.722556589211,-35.2721601717611)) ;
#70538 = CARTESIAN_POINT('',(210.517277625407,609.472556589211,-35.2721601717611)) ;
#70539 = CARTESIAN_POINT('',(201.57290262541,609.472556589211,-35.2721601717607)) ;
#70540 = CARTESIAN_POINT('',(210.517277625407,609.722556589211,-35.0221601717611)) ;
#70541 = CARTESIAN_POINT('Origin',(210.517277625407,609.722556589211,-35.2721601717611)) ;
#70542 = CARTESIAN_POINT('',(201.57290262541,609.722556589211,-35.0221601717607)) ;
#70543 = CARTESIAN_POINT('Origin',(210.517277625407,609.347556589211,-35.2721601717609)) ;
#70544 = CARTESIAN_POINT('',(210.642277625407,609.347556589211,-35.2721601717609)) ;
#70545 = CARTESIAN_POINT('',(210.892277625407,609.347556589211,-35.0221601717612)) ;
#70546 = CARTESIAN_POINT('Origin',(210.892277625407,609.347556589211,-35.2721601717609)) ;
#70547 = CARTESIAN_POINT('Origin',(210.517277625407,609.347556589211,-35.0221601717611)) ;
#70548 = CARTESIAN_POINT('Origin',(210.517277625407,609.347556589211,-35.2721601717609)) ;
#70549 = CARTESIAN_POINT('Origin',(210.892277625407,624.170681589221,-35.2721601717611)) ;
#70550 = CARTESIAN_POINT('',(210.642277625407,605.597556589211,-35.2721601717612)) ;
#70551 = CARTESIAN_POINT('',(210.892277625407,605.597556589211,-35.0221601717612)) ;
#70552 = CARTESIAN_POINT('Origin',(210.892277625407,605.597556589211,-35.2721601717612)) ;
#70553 = CARTESIAN_POINT('',(210.892277625407,624.170681589221,-35.0221601717611)) ;
#70554 = CARTESIAN_POINT('',(210.64227762542,624.170681589221,-35.2721601717611)) ;
#70555 = CARTESIAN_POINT('Origin',(210.517277625407,605.597556589211,-35.2721601717609)) ;
#70556 = CARTESIAN_POINT('',(210.517277625407,605.472556589211,-35.2721601717609)) ;
#70557 = CARTESIAN_POINT('',(210.517277625407,605.222556589211,-35.0221601717611)) ;
#70558 = CARTESIAN_POINT('Origin',(210.517277625407,605.222556589211,-35.2721601717609)) ;
#70559 = CARTESIAN_POINT('Origin',(210.517277625407,605.597556589211,-35.0221601717611)) ;
#70560 = CARTESIAN_POINT('Origin',(210.517277625407,605.597556589211,-35.2721601717609)) ;
#70561 = CARTESIAN_POINT('Origin',(205.938476772278,605.222556589211,-35.2721601717609)) ;
#70562 = CARTESIAN_POINT('',(209.814777625407,605.472556589211,-35.2721601717611)) ;
#70563 = CARTESIAN_POINT('',(209.814777625407,605.222556589211,-35.0221601717611)) ;
#70564 = CARTESIAN_POINT('Origin',(209.814777625407,605.222556589211,-35.2721601717611)) ;
#70565 = CARTESIAN_POINT('',(205.938476772278,605.222556589211,-35.0221601717609)) ;
#70566 = CARTESIAN_POINT('',(205.938476772278,605.472556589211,-35.2721601717609)) ;
#70567 = CARTESIAN_POINT('Origin',(209.814777625407,605.597556589211,-35.2721601717609)) ;
#70568 = CARTESIAN_POINT('',(209.689777625407,605.597556589211,-35.2721601717609)) ;
#70569 = CARTESIAN_POINT('',(209.439777625407,605.597556589211,-35.0221601717611)) ;
#70570 = CARTESIAN_POINT('Origin',(209.439777625407,605.597556589211,-35.2721601717609)) ;
#70571 = CARTESIAN_POINT('Origin',(209.814777625407,605.597556589211,-35.0221601717611)) ;
#70572 = CARTESIAN_POINT('Origin',(209.814777625407,605.597556589211,-35.2721601717609)) ;
#70573 = CARTESIAN_POINT('Origin',(209.439777625407,624.170681589221,-35.2721601717611)) ;
#70574 = CARTESIAN_POINT('',(209.689777625407,609.347556589211,-35.2721601717611)) ;
#70575 = CARTESIAN_POINT('',(209.439777625407,609.347556589211,-35.0221601717611)) ;
#70576 = CARTESIAN_POINT('Origin',(209.439777625407,609.347556589211,-35.2721601717611)) ;
#70577 = CARTESIAN_POINT('',(209.439777625407,624.170681589221,-35.0221601717611)) ;
#70578 = CARTESIAN_POINT('',(209.68977762542,624.170681589221,-35.2721601717611)) ;
#70579 = CARTESIAN_POINT('Origin',(209.814777625407,609.347556589211,-35.2721601717609)) ;
#70580 = CARTESIAN_POINT('Origin',(209.814777625407,609.347556589211,-35.0221601717611)) ;
#70581 = CARTESIAN_POINT('Origin',(209.814777625407,609.347556589211,-35.2721601717609)) ;
#70582 = CARTESIAN_POINT('Origin',(210.51727762542,605.597556589211,-35.7037040214914)) ;
#70583 = CARTESIAN_POINT('',(210.64227762542,605.597556589211,-39.2297690928544)) ;
#70584 = CARTESIAN_POINT('',(210.64227762542,605.597556589211,-35.7037040214914)) ;
#70585 = CARTESIAN_POINT('',(210.51727762542,605.472556589211,-39.2297690928544)) ;
#70586 = CARTESIAN_POINT('Origin',(210.51727762542,605.597556589211,-39.2297690928544)) ;
#70587 = CARTESIAN_POINT('',(210.51727762542,605.472556589211,-35.7037040214914)) ;
#70588 = CARTESIAN_POINT('Origin',(210.64227762542,602.868806589211,-33.4492690928543)) ;
#70589 = CARTESIAN_POINT('',(210.64227762542,609.347556589211,-39.2297690928544)) ;
#70590 = CARTESIAN_POINT('',(210.64227762542,609.347556589211,-33.7350190928543)) ;
#70591 = CARTESIAN_POINT('',(210.64227762542,605.488181589211,-39.2297690928544)) ;
#70592 = CARTESIAN_POINT('Origin',(210.51727762542,609.347556589211,-33.7350190928543)) ;
#70593 = CARTESIAN_POINT('',(210.51727762542,609.472556589211,-39.2297690928544)) ;
#70594 = CARTESIAN_POINT('',(210.51727762542,609.472556589211,-33.7350190928543)) ;
#70595 = CARTESIAN_POINT('Origin',(210.51727762542,609.347556589211,-39.2297690928544)) ;
#70596 = CARTESIAN_POINT('Origin',(197.30727762542,609.472556589211,-34.0207690928544)) ;
#70597 = CARTESIAN_POINT('',(209.81477762542,609.472556589211,-39.2297690928544)) ;
#70598 = CARTESIAN_POINT('',(209.81477762542,609.472556589211,-38.5610190928544)) ;
#70599 = CARTESIAN_POINT('',(207.75302762542,609.472556589211,-39.2297690928544)) ;
#70600 = CARTESIAN_POINT('Origin',(201.57290262541,600.222556589211,-35.2721601717607)) ;
#70601 = CARTESIAN_POINT('',(209.814777625407,600.222556589211,-35.0221601717611)) ;
#70602 = CARTESIAN_POINT('',(209.814777625407,599.972556589211,-35.2721601717611)) ;
#70603 = CARTESIAN_POINT('Origin',(209.814777625407,600.222556589211,-35.2721601717611)) ;
#70604 = CARTESIAN_POINT('',(210.517277625407,599.972556589211,-35.2721601717611)) ;
#70605 = CARTESIAN_POINT('',(201.57290262541,599.972556589211,-35.2721601717607)) ;
#70606 = CARTESIAN_POINT('',(210.517277625407,600.222556589211,-35.0221601717611)) ;
#70607 = CARTESIAN_POINT('Origin',(210.517277625407,600.222556589211,-35.2721601717611)) ;
#70608 = CARTESIAN_POINT('',(201.57290262541,600.222556589211,-35.0221601717607)) ;
#70609 = CARTESIAN_POINT('Origin',(210.517277625407,599.847556589211,-35.2721601717609)) ;
#70610 = CARTESIAN_POINT('',(210.642277625407,599.847556589211,-35.2721601717609)) ;
#70611 = CARTESIAN_POINT('',(210.892277625407,599.847556589211,-35.0221601717612)) ;
#70612 = CARTESIAN_POINT('Origin',(210.892277625407,599.847556589211,-35.2721601717609)) ;
#70613 = CARTESIAN_POINT('Origin',(210.517277625407,599.847556589211,-35.0221601717611)) ;
#70614 = CARTESIAN_POINT('Origin',(210.517277625407,599.847556589211,-35.2721601717609)) ;
#70615 = CARTESIAN_POINT('Origin',(210.892277625407,614.670681589221,-35.2721601717611)) ;
#70616 = CARTESIAN_POINT('',(210.642277625407,596.097556589211,-35.2721601717612)) ;
#70617 = CARTESIAN_POINT('',(210.892277625407,596.097556589211,-35.0221601717612)) ;
#70618 = CARTESIAN_POINT('Origin',(210.892277625407,596.097556589211,-35.2721601717612)) ;
#70619 = CARTESIAN_POINT('',(210.892277625407,614.670681589221,-35.0221601717611)) ;
#70620 = CARTESIAN_POINT('',(210.642277625419,614.670681589221,-35.2721601717611)) ;
#70621 = CARTESIAN_POINT('Origin',(210.517277625407,596.097556589211,-35.2721601717609)) ;
#70622 = CARTESIAN_POINT('',(210.517277625407,595.972556589211,-35.2721601717609)) ;
#70623 = CARTESIAN_POINT('',(210.517277625407,595.722556589211,-35.0221601717611)) ;
#70624 = CARTESIAN_POINT('Origin',(210.517277625407,595.722556589211,-35.2721601717609)) ;
#70625 = CARTESIAN_POINT('Origin',(210.517277625407,596.097556589211,-35.0221601717611)) ;
#70626 = CARTESIAN_POINT('Origin',(210.517277625407,596.097556589211,-35.2721601717609)) ;
#70627 = CARTESIAN_POINT('Origin',(205.938476772278,595.722556589211,-35.2721601717609)) ;
#70628 = CARTESIAN_POINT('',(209.814777625407,595.972556589211,-35.2721601717611)) ;
#70629 = CARTESIAN_POINT('',(209.814777625407,595.722556589211,-35.0221601717611)) ;
#70630 = CARTESIAN_POINT('Origin',(209.814777625407,595.722556589211,-35.2721601717611)) ;
#70631 = CARTESIAN_POINT('',(205.938476772278,595.722556589211,-35.0221601717609)) ;
#70632 = CARTESIAN_POINT('',(205.938476772278,595.972556589211,-35.2721601717609)) ;
#70633 = CARTESIAN_POINT('Origin',(209.814777625407,596.097556589211,-35.2721601717609)) ;
#70634 = CARTESIAN_POINT('',(209.689777625407,596.097556589211,-35.2721601717609)) ;
#70635 = CARTESIAN_POINT('',(209.439777625407,596.097556589211,-35.0221601717611)) ;
#70636 = CARTESIAN_POINT('Origin',(209.439777625407,596.097556589211,-35.2721601717609)) ;
#70637 = CARTESIAN_POINT('Origin',(209.814777625407,596.097556589211,-35.0221601717611)) ;
#70638 = CARTESIAN_POINT('Origin',(209.814777625407,596.097556589211,-35.2721601717609)) ;
#70639 = CARTESIAN_POINT('Origin',(209.439777625407,614.670681589221,-35.2721601717611)) ;
#70640 = CARTESIAN_POINT('',(209.689777625407,599.847556589211,-35.2721601717611)) ;
#70641 = CARTESIAN_POINT('',(209.439777625407,599.847556589211,-35.0221601717611)) ;
#70642 = CARTESIAN_POINT('Origin',(209.439777625407,599.847556589211,-35.2721601717611)) ;
#70643 = CARTESIAN_POINT('',(209.439777625407,614.670681589221,-35.0221601717611)) ;
#70644 = CARTESIAN_POINT('',(209.689777625418,614.670681589221,-35.2721601717611)) ;
#70645 = CARTESIAN_POINT('Origin',(209.814777625407,599.847556589211,-35.2721601717609)) ;
#70646 = CARTESIAN_POINT('Origin',(209.814777625407,599.847556589211,-35.0221601717611)) ;
#70647 = CARTESIAN_POINT('Origin',(209.814777625407,599.847556589211,-35.2721601717609)) ;
#70648 = CARTESIAN_POINT('Origin',(210.517277625419,596.097556589211,-35.7037040214914)) ;
#70649 = CARTESIAN_POINT('',(210.642277625419,596.097556589211,-39.2297690928544)) ;
#70650 = CARTESIAN_POINT('',(210.642277625419,596.097556589211,-35.7037040214914)) ;
#70651 = CARTESIAN_POINT('',(210.517277625419,595.972556589211,-39.2297690928544)) ;
#70652 = CARTESIAN_POINT('Origin',(210.517277625419,596.097556589211,-39.2297690928544)) ;
#70653 = CARTESIAN_POINT('',(210.517277625419,595.972556589211,-35.7037040214914)) ;
#70654 = CARTESIAN_POINT('Origin',(210.642277625419,593.368806589211,-33.4492690928543)) ;
#70655 = CARTESIAN_POINT('',(210.642277625419,599.847556589211,-39.2297690928544)) ;
#70656 = CARTESIAN_POINT('',(210.642277625419,599.847556589211,-33.7350190928543)) ;
#70657 = CARTESIAN_POINT('',(210.642277625419,595.988181589211,-39.2297690928544)) ;
#70658 = CARTESIAN_POINT('Origin',(210.517277625419,599.847556589211,-33.7350190928543)) ;
#70659 = CARTESIAN_POINT('',(210.517277625419,599.972556589211,-39.2297690928544)) ;
#70660 = CARTESIAN_POINT('',(210.517277625419,599.972556589211,-33.7350190928543)) ;
#70661 = CARTESIAN_POINT('Origin',(210.517277625419,599.847556589211,-39.2297690928544)) ;
#70662 = CARTESIAN_POINT('Origin',(197.307277625418,599.972556589211,-34.0207690928544)) ;
#70663 = CARTESIAN_POINT('',(209.814777625418,599.972556589211,-39.2297690928544)) ;
#70664 = CARTESIAN_POINT('',(209.814777625418,599.972556589211,-38.5610190928544)) ;
#70665 = CARTESIAN_POINT('',(207.753027625418,599.972556589211,-39.2297690928544)) ;
#70666 = CARTESIAN_POINT('Origin',(201.57290262541,590.722556589211,-35.2721601717607)) ;
#70667 = CARTESIAN_POINT('',(209.814777625407,590.722556589211,-35.0221601717611)) ;
#70668 = CARTESIAN_POINT('',(209.814777625407,590.472556589211,-35.2721601717611)) ;
#70669 = CARTESIAN_POINT('Origin',(209.814777625407,590.722556589211,-35.2721601717611)) ;
#70670 = CARTESIAN_POINT('',(210.517277625407,590.472556589211,-35.2721601717611)) ;
#70671 = CARTESIAN_POINT('',(201.57290262541,590.472556589211,-35.2721601717607)) ;
#70672 = CARTESIAN_POINT('',(210.517277625407,590.722556589211,-35.0221601717611)) ;
#70673 = CARTESIAN_POINT('Origin',(210.517277625407,590.722556589211,-35.2721601717611)) ;
#70674 = CARTESIAN_POINT('',(201.57290262541,590.722556589211,-35.0221601717607)) ;
#70675 = CARTESIAN_POINT('Origin',(210.517277625407,590.347556589211,-35.2721601717609)) ;
#70676 = CARTESIAN_POINT('',(210.642277625407,590.347556589211,-35.2721601717609)) ;
#70677 = CARTESIAN_POINT('',(210.892277625407,590.347556589211,-35.0221601717612)) ;
#70678 = CARTESIAN_POINT('Origin',(210.892277625407,590.347556589211,-35.2721601717609)) ;
#70679 = CARTESIAN_POINT('Origin',(210.517277625407,590.347556589211,-35.0221601717611)) ;
#70680 = CARTESIAN_POINT('Origin',(210.517277625407,590.347556589211,-35.2721601717609)) ;
#70681 = CARTESIAN_POINT('Origin',(210.892277625407,605.170681589221,-35.2721601717611)) ;
#70682 = CARTESIAN_POINT('',(210.642277625407,586.597556589211,-35.2721601717612)) ;
#70683 = CARTESIAN_POINT('',(210.892277625407,586.597556589211,-35.0221601717612)) ;
#70684 = CARTESIAN_POINT('Origin',(210.892277625407,586.597556589211,-35.2721601717612)) ;
#70685 = CARTESIAN_POINT('',(210.892277625407,605.170681589221,-35.0221601717611)) ;
#70686 = CARTESIAN_POINT('',(210.642277625417,605.170681589221,-35.2721601717611)) ;
#70687 = CARTESIAN_POINT('Origin',(210.517277625407,586.597556589211,-35.2721601717609)) ;
#70688 = CARTESIAN_POINT('',(210.517277625407,586.472556589211,-35.2721601717609)) ;
#70689 = CARTESIAN_POINT('',(210.517277625407,586.222556589211,-35.0221601717611)) ;
#70690 = CARTESIAN_POINT('Origin',(210.517277625407,586.222556589211,-35.2721601717609)) ;
#70691 = CARTESIAN_POINT('Origin',(210.517277625407,586.597556589211,-35.0221601717611)) ;
#70692 = CARTESIAN_POINT('Origin',(210.517277625407,586.597556589211,-35.2721601717609)) ;
#70693 = CARTESIAN_POINT('Origin',(205.938476772278,586.222556589211,-35.2721601717609)) ;
#70694 = CARTESIAN_POINT('',(209.814777625407,586.472556589211,-35.2721601717611)) ;
#70695 = CARTESIAN_POINT('',(209.814777625407,586.222556589211,-35.0221601717611)) ;
#70696 = CARTESIAN_POINT('Origin',(209.814777625407,586.222556589211,-35.2721601717611)) ;
#70697 = CARTESIAN_POINT('',(205.938476772278,586.222556589211,-35.0221601717609)) ;
#70698 = CARTESIAN_POINT('',(205.938476772278,586.472556589211,-35.2721601717609)) ;
#70699 = CARTESIAN_POINT('Origin',(209.814777625407,586.597556589211,-35.2721601717609)) ;
#70700 = CARTESIAN_POINT('',(209.689777625407,586.597556589211,-35.2721601717609)) ;
#70701 = CARTESIAN_POINT('',(209.439777625407,586.597556589211,-35.0221601717611)) ;
#70702 = CARTESIAN_POINT('Origin',(209.439777625407,586.597556589211,-35.2721601717609)) ;
#70703 = CARTESIAN_POINT('Origin',(209.814777625407,586.597556589211,-35.0221601717611)) ;
#70704 = CARTESIAN_POINT('Origin',(209.814777625407,586.597556589211,-35.2721601717609)) ;
#70705 = CARTESIAN_POINT('Origin',(209.439777625407,605.170681589221,-35.2721601717611)) ;
#70706 = CARTESIAN_POINT('',(209.689777625407,590.347556589211,-35.2721601717611)) ;
#70707 = CARTESIAN_POINT('',(209.439777625407,590.347556589211,-35.0221601717611)) ;
#70708 = CARTESIAN_POINT('Origin',(209.439777625407,590.347556589211,-35.2721601717611)) ;
#70709 = CARTESIAN_POINT('',(209.439777625407,605.170681589221,-35.0221601717611)) ;
#70710 = CARTESIAN_POINT('',(209.689777625417,605.170681589221,-35.2721601717611)) ;
#70711 = CARTESIAN_POINT('Origin',(209.814777625407,590.347556589211,-35.2721601717609)) ;
#70712 = CARTESIAN_POINT('Origin',(209.814777625407,590.347556589211,-35.0221601717611)) ;
#70713 = CARTESIAN_POINT('Origin',(209.814777625407,590.347556589211,-35.2721601717609)) ;
#70714 = CARTESIAN_POINT('Origin',(210.517277625417,586.597556589211,-35.7037040214914)) ;
#70715 = CARTESIAN_POINT('',(210.642277625417,586.597556589211,-39.2297690928544)) ;
#70716 = CARTESIAN_POINT('',(210.642277625417,586.597556589211,-35.7037040214914)) ;
#70717 = CARTESIAN_POINT('',(210.517277625417,586.472556589211,-39.2297690928544)) ;
#70718 = CARTESIAN_POINT('Origin',(210.517277625417,586.597556589211,-39.2297690928544)) ;
#70719 = CARTESIAN_POINT('',(210.517277625417,586.472556589211,-35.7037040214914)) ;
#70720 = CARTESIAN_POINT('Origin',(210.642277625417,583.868806589211,-33.4492690928543)) ;
#70721 = CARTESIAN_POINT('',(210.642277625417,590.347556589211,-39.2297690928544)) ;
#70722 = CARTESIAN_POINT('',(210.642277625417,590.347556589211,-33.7350190928543)) ;
#70723 = CARTESIAN_POINT('',(210.642277625417,586.488181589211,-39.2297690928544)) ;
#70724 = CARTESIAN_POINT('Origin',(210.517277625417,590.347556589211,-33.7350190928543)) ;
#70725 = CARTESIAN_POINT('',(210.517277625417,590.472556589211,-39.2297690928544)) ;
#70726 = CARTESIAN_POINT('',(210.517277625417,590.472556589211,-33.7350190928543)) ;
#70727 = CARTESIAN_POINT('Origin',(210.517277625417,590.347556589211,-39.2297690928544)) ;
#70728 = CARTESIAN_POINT('Origin',(197.307277625417,590.472556589211,-34.0207690928544)) ;
#70729 = CARTESIAN_POINT('',(209.814777625417,590.472556589211,-39.2297690928544)) ;
#70730 = CARTESIAN_POINT('',(209.814777625417,590.472556589211,-38.5610190928544)) ;
#70731 = CARTESIAN_POINT('',(207.753027625417,590.472556589211,-39.2297690928544)) ;
#70732 = CARTESIAN_POINT('Origin',(201.57290262541,581.222556589211,-35.2721601717607)) ;
#70733 = CARTESIAN_POINT('',(209.814777625407,581.222556589211,-35.0221601717611)) ;
#70734 = CARTESIAN_POINT('',(209.814777625407,580.972556589211,-35.2721601717611)) ;
#70735 = CARTESIAN_POINT('Origin',(209.814777625407,581.222556589211,-35.2721601717611)) ;
#70736 = CARTESIAN_POINT('',(210.517277625407,580.972556589211,-35.2721601717611)) ;
#70737 = CARTESIAN_POINT('',(201.57290262541,580.972556589211,-35.2721601717607)) ;
#70738 = CARTESIAN_POINT('',(210.517277625407,581.222556589211,-35.0221601717611)) ;
#70739 = CARTESIAN_POINT('Origin',(210.517277625407,581.222556589211,-35.2721601717611)) ;
#70740 = CARTESIAN_POINT('',(201.57290262541,581.222556589211,-35.0221601717607)) ;
#70741 = CARTESIAN_POINT('Origin',(210.517277625407,580.847556589211,-35.2721601717609)) ;
#70742 = CARTESIAN_POINT('',(210.642277625407,580.847556589211,-35.2721601717609)) ;
#70743 = CARTESIAN_POINT('',(210.892277625407,580.847556589211,-35.0221601717612)) ;
#70744 = CARTESIAN_POINT('Origin',(210.892277625407,580.847556589211,-35.2721601717609)) ;
#70745 = CARTESIAN_POINT('Origin',(210.517277625407,580.847556589211,-35.0221601717611)) ;
#70746 = CARTESIAN_POINT('Origin',(210.517277625407,580.847556589211,-35.2721601717609)) ;
#70747 = CARTESIAN_POINT('Origin',(210.892277625407,595.670681589221,-35.2721601717611)) ;
#70748 = CARTESIAN_POINT('',(210.642277625407,577.097556589211,-35.2721601717612)) ;
#70749 = CARTESIAN_POINT('',(210.892277625407,577.097556589211,-35.0221601717612)) ;
#70750 = CARTESIAN_POINT('Origin',(210.892277625407,577.097556589211,-35.2721601717612)) ;
#70751 = CARTESIAN_POINT('',(210.892277625407,595.670681589221,-35.0221601717611)) ;
#70752 = CARTESIAN_POINT('',(210.642277625415,595.670681589221,-35.2721601717611)) ;
#70753 = CARTESIAN_POINT('Origin',(210.517277625407,577.097556589211,-35.2721601717609)) ;
#70754 = CARTESIAN_POINT('',(210.517277625407,576.972556589211,-35.2721601717609)) ;
#70755 = CARTESIAN_POINT('',(210.517277625407,576.722556589211,-35.0221601717611)) ;
#70756 = CARTESIAN_POINT('Origin',(210.517277625407,576.722556589211,-35.2721601717609)) ;
#70757 = CARTESIAN_POINT('Origin',(210.517277625407,577.097556589211,-35.0221601717611)) ;
#70758 = CARTESIAN_POINT('Origin',(210.517277625407,577.097556589211,-35.2721601717609)) ;
#70759 = CARTESIAN_POINT('Origin',(205.938476772278,576.722556589211,-35.2721601717609)) ;
#70760 = CARTESIAN_POINT('',(209.814777625407,576.972556589211,-35.2721601717611)) ;
#70761 = CARTESIAN_POINT('',(209.814777625407,576.722556589211,-35.0221601717611)) ;
#70762 = CARTESIAN_POINT('Origin',(209.814777625407,576.722556589211,-35.2721601717611)) ;
#70763 = CARTESIAN_POINT('',(205.938476772278,576.722556589211,-35.0221601717609)) ;
#70764 = CARTESIAN_POINT('',(205.938476772278,576.972556589211,-35.2721601717609)) ;
#70765 = CARTESIAN_POINT('Origin',(209.814777625407,577.097556589211,-35.2721601717609)) ;
#70766 = CARTESIAN_POINT('',(209.689777625407,577.097556589211,-35.2721601717609)) ;
#70767 = CARTESIAN_POINT('',(209.439777625407,577.097556589211,-35.0221601717611)) ;
#70768 = CARTESIAN_POINT('Origin',(209.439777625407,577.097556589211,-35.2721601717609)) ;
#70769 = CARTESIAN_POINT('Origin',(209.814777625407,577.097556589211,-35.0221601717611)) ;
#70770 = CARTESIAN_POINT('Origin',(209.814777625407,577.097556589211,-35.2721601717609)) ;
#70771 = CARTESIAN_POINT('Origin',(209.439777625407,595.670681589221,-35.2721601717611)) ;
#70772 = CARTESIAN_POINT('',(209.689777625407,580.847556589211,-35.2721601717611)) ;
#70773 = CARTESIAN_POINT('',(209.439777625407,580.847556589211,-35.0221601717611)) ;
#70774 = CARTESIAN_POINT('Origin',(209.439777625407,580.847556589211,-35.2721601717611)) ;
#70775 = CARTESIAN_POINT('',(209.439777625407,595.670681589221,-35.0221601717611)) ;
#70776 = CARTESIAN_POINT('',(209.689777625415,595.670681589221,-35.2721601717611)) ;
#70777 = CARTESIAN_POINT('Origin',(209.814777625407,580.847556589211,-35.2721601717609)) ;
#70778 = CARTESIAN_POINT('Origin',(209.814777625407,580.847556589211,-35.0221601717611)) ;
#70779 = CARTESIAN_POINT('Origin',(209.814777625407,580.847556589211,-35.2721601717609)) ;
#70780 = CARTESIAN_POINT('Origin',(210.517277625416,577.097556589211,-35.7037040214914)) ;
#70781 = CARTESIAN_POINT('',(210.642277625416,577.097556589211,-39.2297690928544)) ;
#70782 = CARTESIAN_POINT('',(210.642277625416,577.097556589211,-35.7037040214914)) ;
#70783 = CARTESIAN_POINT('',(210.517277625416,576.972556589211,-39.2297690928544)) ;
#70784 = CARTESIAN_POINT('Origin',(210.517277625416,577.097556589211,-39.2297690928544)) ;
#70785 = CARTESIAN_POINT('',(210.517277625416,576.972556589211,-35.7037040214914)) ;
#70786 = CARTESIAN_POINT('Origin',(210.642277625415,574.368806589211,-33.4492690928543)) ;
#70787 = CARTESIAN_POINT('',(210.642277625416,580.847556589211,-39.2297690928544)) ;
#70788 = CARTESIAN_POINT('',(210.642277625415,580.847556589211,-33.7350190928543)) ;
#70789 = CARTESIAN_POINT('',(210.642277625416,576.988181589211,-39.2297690928544)) ;
#70790 = CARTESIAN_POINT('Origin',(210.517277625415,580.847556589211,-33.7350190928543)) ;
#70791 = CARTESIAN_POINT('',(210.517277625416,580.972556589211,-39.2297690928544)) ;
#70792 = CARTESIAN_POINT('',(210.517277625415,580.972556589211,-33.7350190928543)) ;
#70793 = CARTESIAN_POINT('Origin',(210.517277625416,580.847556589211,-39.2297690928544)) ;
#70794 = CARTESIAN_POINT('Origin',(197.307277625415,580.972556589211,-34.0207690928544)) ;
#70795 = CARTESIAN_POINT('',(209.814777625415,580.972556589211,-39.2297690928544)) ;
#70796 = CARTESIAN_POINT('',(209.814777625415,580.972556589211,-38.5610190928544)) ;
#70797 = CARTESIAN_POINT('',(207.753027625415,580.972556589211,-39.2297690928544)) ;
#70798 = CARTESIAN_POINT('Origin',(201.57290262541,571.722556589211,-35.2721601717607)) ;
#70799 = CARTESIAN_POINT('',(209.814777625407,571.722556589211,-35.0221601717611)) ;
#70800 = CARTESIAN_POINT('',(209.814777625407,571.472556589211,-35.2721601717611)) ;
#70801 = CARTESIAN_POINT('Origin',(209.814777625407,571.722556589211,-35.2721601717611)) ;
#70802 = CARTESIAN_POINT('',(210.517277625407,571.472556589211,-35.2721601717611)) ;
#70803 = CARTESIAN_POINT('',(201.57290262541,571.472556589211,-35.2721601717607)) ;
#70804 = CARTESIAN_POINT('',(210.517277625407,571.722556589211,-35.0221601717611)) ;
#70805 = CARTESIAN_POINT('Origin',(210.517277625407,571.722556589211,-35.2721601717611)) ;
#70806 = CARTESIAN_POINT('',(201.57290262541,571.722556589211,-35.0221601717607)) ;
#70807 = CARTESIAN_POINT('Origin',(210.517277625407,571.347556589211,-35.2721601717609)) ;
#70808 = CARTESIAN_POINT('',(210.642277625407,571.347556589211,-35.2721601717609)) ;
#70809 = CARTESIAN_POINT('',(210.892277625407,571.347556589211,-35.0221601717612)) ;
#70810 = CARTESIAN_POINT('Origin',(210.892277625407,571.347556589211,-35.2721601717609)) ;
#70811 = CARTESIAN_POINT('Origin',(210.517277625407,571.347556589211,-35.0221601717611)) ;
#70812 = CARTESIAN_POINT('Origin',(210.517277625407,571.347556589211,-35.2721601717609)) ;
#70813 = CARTESIAN_POINT('Origin',(210.892277625407,586.170681589221,-35.2721601717611)) ;
#70814 = CARTESIAN_POINT('',(210.642277625407,567.59755658921,-35.2721601717612)) ;
#70815 = CARTESIAN_POINT('',(210.892277625407,567.59755658921,-35.0221601717612)) ;
#70816 = CARTESIAN_POINT('Origin',(210.892277625407,567.59755658921,-35.2721601717612)) ;
#70817 = CARTESIAN_POINT('',(210.892277625407,586.170681589221,-35.0221601717611)) ;
#70818 = CARTESIAN_POINT('',(210.642277625414,586.170681589221,-35.2721601717611)) ;
#70819 = CARTESIAN_POINT('Origin',(210.517277625407,567.59755658921,-35.2721601717609)) ;
#70820 = CARTESIAN_POINT('',(210.517277625407,567.472556589211,-35.2721601717609)) ;
#70821 = CARTESIAN_POINT('',(210.517277625407,567.222556589211,-35.0221601717611)) ;
#70822 = CARTESIAN_POINT('Origin',(210.517277625407,567.222556589211,-35.2721601717609)) ;
#70823 = CARTESIAN_POINT('Origin',(210.517277625407,567.59755658921,-35.0221601717611)) ;
#70824 = CARTESIAN_POINT('Origin',(210.517277625407,567.59755658921,-35.2721601717609)) ;
#70825 = CARTESIAN_POINT('Origin',(205.938476772278,567.222556589211,-35.2721601717609)) ;
#70826 = CARTESIAN_POINT('',(209.814777625407,567.472556589211,-35.2721601717611)) ;
#70827 = CARTESIAN_POINT('',(209.814777625407,567.222556589211,-35.0221601717611)) ;
#70828 = CARTESIAN_POINT('Origin',(209.814777625407,567.222556589211,-35.2721601717611)) ;
#70829 = CARTESIAN_POINT('',(205.938476772278,567.222556589211,-35.0221601717609)) ;
#70830 = CARTESIAN_POINT('',(205.938476772278,567.47255658921,-35.2721601717609)) ;
#70831 = CARTESIAN_POINT('Origin',(209.814777625407,567.597556589211,-35.2721601717609)) ;
#70832 = CARTESIAN_POINT('',(209.689777625407,567.597556589211,-35.2721601717609)) ;
#70833 = CARTESIAN_POINT('',(209.439777625407,567.597556589211,-35.0221601717611)) ;
#70834 = CARTESIAN_POINT('Origin',(209.439777625407,567.597556589211,-35.2721601717609)) ;
#70835 = CARTESIAN_POINT('Origin',(209.814777625407,567.597556589211,-35.0221601717611)) ;
#70836 = CARTESIAN_POINT('Origin',(209.814777625407,567.597556589211,-35.2721601717609)) ;
#70837 = CARTESIAN_POINT('Origin',(209.439777625407,586.170681589221,-35.2721601717611)) ;
#70838 = CARTESIAN_POINT('',(209.689777625407,571.347556589211,-35.2721601717611)) ;
#70839 = CARTESIAN_POINT('',(209.439777625407,571.347556589211,-35.0221601717611)) ;
#70840 = CARTESIAN_POINT('Origin',(209.439777625407,571.347556589211,-35.2721601717611)) ;
#70841 = CARTESIAN_POINT('',(209.439777625407,586.170681589221,-35.0221601717611)) ;
#70842 = CARTESIAN_POINT('',(209.689777625413,586.170681589221,-35.2721601717611)) ;
#70843 = CARTESIAN_POINT('Origin',(209.814777625407,571.347556589211,-35.2721601717609)) ;
#70844 = CARTESIAN_POINT('Origin',(209.814777625407,571.347556589211,-35.0221601717611)) ;
#70845 = CARTESIAN_POINT('Origin',(209.814777625407,571.347556589211,-35.2721601717609)) ;
#70846 = CARTESIAN_POINT('Origin',(210.517277625414,567.59755658921,-35.7037040214914)) ;
#70847 = CARTESIAN_POINT('',(210.642277625414,567.59755658921,-39.2297690928544)) ;
#70848 = CARTESIAN_POINT('',(210.642277625414,567.59755658921,-35.7037040214914)) ;
#70849 = CARTESIAN_POINT('',(210.517277625414,567.47255658921,-39.2297690928544)) ;
#70850 = CARTESIAN_POINT('Origin',(210.517277625414,567.59755658921,-39.2297690928544)) ;
#70851 = CARTESIAN_POINT('',(210.517277625414,567.47255658921,-35.7037040214914)) ;
#70852 = CARTESIAN_POINT('Origin',(210.642277625414,564.868806589211,-33.4492690928543)) ;
#70853 = CARTESIAN_POINT('',(210.642277625414,571.347556589211,-39.2297690928544)) ;
#70854 = CARTESIAN_POINT('',(210.642277625414,571.347556589211,-33.7350190928543)) ;
#70855 = CARTESIAN_POINT('',(210.642277625414,567.488181589211,-39.2297690928544)) ;
#70856 = CARTESIAN_POINT('Origin',(210.517277625414,571.347556589211,-33.7350190928543)) ;
#70857 = CARTESIAN_POINT('',(210.517277625414,571.472556589211,-39.2297690928544)) ;
#70858 = CARTESIAN_POINT('',(210.517277625414,571.472556589211,-33.7350190928543)) ;
#70859 = CARTESIAN_POINT('Origin',(210.517277625414,571.347556589211,-39.2297690928544)) ;
#70860 = CARTESIAN_POINT('Origin',(197.307277625413,571.472556589211,-34.0207690928544)) ;
#70861 = CARTESIAN_POINT('',(209.814777625413,571.472556589211,-39.2297690928544)) ;
#70862 = CARTESIAN_POINT('',(209.814777625413,571.472556589211,-38.5610190928544)) ;
#70863 = CARTESIAN_POINT('',(207.753027625413,571.472556589211,-39.2297690928544)) ;
#70864 = CARTESIAN_POINT('Origin',(201.57290262541,562.222556589211,-35.2721601717607)) ;
#70865 = CARTESIAN_POINT('',(209.814777625407,562.222556589211,-35.0221601717611)) ;
#70866 = CARTESIAN_POINT('',(209.814777625407,561.972556589211,-35.2721601717611)) ;
#70867 = CARTESIAN_POINT('Origin',(209.814777625407,562.222556589211,-35.2721601717611)) ;
#70868 = CARTESIAN_POINT('',(210.517277625407,561.972556589211,-35.2721601717611)) ;
#70869 = CARTESIAN_POINT('',(201.57290262541,561.972556589211,-35.2721601717607)) ;
#70870 = CARTESIAN_POINT('',(210.517277625407,562.222556589211,-35.0221601717611)) ;
#70871 = CARTESIAN_POINT('Origin',(210.517277625407,562.222556589211,-35.2721601717611)) ;
#70872 = CARTESIAN_POINT('',(201.57290262541,562.222556589211,-35.0221601717607)) ;
#70873 = CARTESIAN_POINT('Origin',(210.517277625407,561.847556589211,-35.2721601717609)) ;
#70874 = CARTESIAN_POINT('',(210.642277625407,561.847556589211,-35.2721601717609)) ;
#70875 = CARTESIAN_POINT('',(210.892277625407,561.847556589211,-35.0221601717612)) ;
#70876 = CARTESIAN_POINT('Origin',(210.892277625407,561.847556589211,-35.2721601717609)) ;
#70877 = CARTESIAN_POINT('Origin',(210.517277625407,561.847556589211,-35.0221601717611)) ;
#70878 = CARTESIAN_POINT('Origin',(210.517277625407,561.847556589211,-35.2721601717609)) ;
#70879 = CARTESIAN_POINT('Origin',(210.892277625407,576.670681589221,-35.2721601717611)) ;
#70880 = CARTESIAN_POINT('',(210.642277625407,558.09755658921,-35.2721601717612)) ;
#70881 = CARTESIAN_POINT('',(210.892277625407,558.09755658921,-35.0221601717612)) ;
#70882 = CARTESIAN_POINT('Origin',(210.892277625407,558.09755658921,-35.2721601717612)) ;
#70883 = CARTESIAN_POINT('',(210.892277625407,576.670681589221,-35.0221601717611)) ;
#70884 = CARTESIAN_POINT('',(210.642277625412,576.670681589221,-35.2721601717611)) ;
#70885 = CARTESIAN_POINT('Origin',(210.517277625407,558.09755658921,-35.2721601717609)) ;
#70886 = CARTESIAN_POINT('',(210.517277625407,557.97255658921,-35.2721601717609)) ;
#70887 = CARTESIAN_POINT('',(210.517277625407,557.722556589211,-35.0221601717611)) ;
#70888 = CARTESIAN_POINT('Origin',(210.517277625407,557.722556589211,-35.2721601717609)) ;
#70889 = CARTESIAN_POINT('Origin',(210.517277625407,558.09755658921,-35.0221601717611)) ;
#70890 = CARTESIAN_POINT('Origin',(210.517277625407,558.09755658921,-35.2721601717609)) ;
#70891 = CARTESIAN_POINT('Origin',(205.938476772278,557.722556589211,-35.2721601717609)) ;
#70892 = CARTESIAN_POINT('',(209.814777625407,557.97255658921,-35.2721601717611)) ;
#70893 = CARTESIAN_POINT('',(209.814777625407,557.722556589211,-35.0221601717611)) ;
#70894 = CARTESIAN_POINT('Origin',(209.814777625407,557.722556589211,-35.2721601717611)) ;
#70895 = CARTESIAN_POINT('',(205.938476772278,557.722556589211,-35.0221601717609)) ;
#70896 = CARTESIAN_POINT('',(205.938476772278,557.97255658921,-35.2721601717609)) ;
#70897 = CARTESIAN_POINT('Origin',(209.814777625407,558.097556589211,-35.2721601717609)) ;
#70898 = CARTESIAN_POINT('',(209.689777625407,558.097556589211,-35.2721601717609)) ;
#70899 = CARTESIAN_POINT('',(209.439777625407,558.097556589211,-35.0221601717611)) ;
#70900 = CARTESIAN_POINT('Origin',(209.439777625407,558.097556589211,-35.2721601717609)) ;
#70901 = CARTESIAN_POINT('Origin',(209.814777625407,558.097556589211,-35.0221601717611)) ;
#70902 = CARTESIAN_POINT('Origin',(209.814777625407,558.097556589211,-35.2721601717609)) ;
#70903 = CARTESIAN_POINT('Origin',(209.439777625407,576.670681589221,-35.2721601717611)) ;
#70904 = CARTESIAN_POINT('',(209.689777625407,561.847556589211,-35.2721601717611)) ;
#70905 = CARTESIAN_POINT('',(209.439777625407,561.847556589211,-35.0221601717611)) ;
#70906 = CARTESIAN_POINT('Origin',(209.439777625407,561.847556589211,-35.2721601717611)) ;
#70907 = CARTESIAN_POINT('',(209.439777625407,576.670681589221,-35.0221601717611)) ;
#70908 = CARTESIAN_POINT('',(209.689777625412,576.670681589221,-35.2721601717611)) ;
#70909 = CARTESIAN_POINT('Origin',(209.814777625407,561.847556589211,-35.2721601717609)) ;
#70910 = CARTESIAN_POINT('Origin',(209.814777625407,561.847556589211,-35.0221601717611)) ;
#70911 = CARTESIAN_POINT('Origin',(209.814777625407,561.847556589211,-35.2721601717609)) ;
#70912 = CARTESIAN_POINT('Origin',(210.517277625412,558.09755658921,-35.7037040214914)) ;
#70913 = CARTESIAN_POINT('',(210.642277625412,558.097556589211,-39.2297690928544)) ;
#70914 = CARTESIAN_POINT('',(210.642277625412,558.09755658921,-35.7037040214914)) ;
#70915 = CARTESIAN_POINT('',(210.517277625412,557.97255658921,-39.2297690928544)) ;
#70916 = CARTESIAN_POINT('Origin',(210.517277625412,558.097556589211,-39.2297690928544)) ;
#70917 = CARTESIAN_POINT('',(210.517277625412,557.97255658921,-35.7037040214914)) ;
#70918 = CARTESIAN_POINT('Origin',(210.642277625412,555.368806589211,-33.4492690928543)) ;
#70919 = CARTESIAN_POINT('',(210.642277625412,561.847556589211,-39.2297690928544)) ;
#70920 = CARTESIAN_POINT('',(210.642277625412,561.847556589211,-33.7350190928543)) ;
#70921 = CARTESIAN_POINT('',(210.642277625412,557.988181589211,-39.2297690928544)) ;
#70922 = CARTESIAN_POINT('Origin',(210.517277625412,561.847556589211,-33.7350190928543)) ;
#70923 = CARTESIAN_POINT('',(210.517277625412,561.972556589211,-39.2297690928544)) ;
#70924 = CARTESIAN_POINT('',(210.517277625412,561.972556589211,-33.7350190928543)) ;
#70925 = CARTESIAN_POINT('Origin',(210.517277625412,561.847556589211,-39.2297690928544)) ;
#70926 = CARTESIAN_POINT('Origin',(197.307277625412,561.972556589211,-34.0207690928544)) ;
#70927 = CARTESIAN_POINT('',(209.814777625412,561.972556589211,-39.2297690928544)) ;
#70928 = CARTESIAN_POINT('',(209.814777625412,561.972556589211,-38.5610190928544)) ;
#70929 = CARTESIAN_POINT('',(207.753027625412,561.972556589211,-39.2297690928544)) ;
#70930 = CARTESIAN_POINT('Origin',(201.57290262541,552.722556589211,-35.2721601717607)) ;
#70931 = CARTESIAN_POINT('',(209.814777625407,552.722556589211,-35.0221601717611)) ;
#70932 = CARTESIAN_POINT('',(209.814777625407,552.472556589211,-35.2721601717611)) ;
#70933 = CARTESIAN_POINT('Origin',(209.814777625407,552.722556589211,-35.2721601717611)) ;
#70934 = CARTESIAN_POINT('',(210.517277625407,552.472556589211,-35.2721601717611)) ;
#70935 = CARTESIAN_POINT('',(201.57290262541,552.472556589211,-35.2721601717607)) ;
#70936 = CARTESIAN_POINT('',(210.517277625407,552.722556589211,-35.0221601717611)) ;
#70937 = CARTESIAN_POINT('Origin',(210.517277625407,552.722556589211,-35.2721601717611)) ;
#70938 = CARTESIAN_POINT('',(201.57290262541,552.722556589211,-35.0221601717607)) ;
#70939 = CARTESIAN_POINT('Origin',(210.517277625407,552.347556589211,-35.2721601717609)) ;
#70940 = CARTESIAN_POINT('',(210.642277625407,552.347556589211,-35.2721601717609)) ;
#70941 = CARTESIAN_POINT('',(210.892277625407,552.347556589211,-35.0221601717612)) ;
#70942 = CARTESIAN_POINT('Origin',(210.892277625407,552.347556589211,-35.2721601717609)) ;
#70943 = CARTESIAN_POINT('Origin',(210.517277625407,552.347556589211,-35.0221601717611)) ;
#70944 = CARTESIAN_POINT('Origin',(210.517277625407,552.347556589211,-35.2721601717609)) ;
#70945 = CARTESIAN_POINT('Origin',(210.892277625407,567.170681589221,-35.2721601717611)) ;
#70946 = CARTESIAN_POINT('',(210.642277625407,548.59755658921,-35.2721601717612)) ;
#70947 = CARTESIAN_POINT('',(210.892277625407,548.59755658921,-35.0221601717612)) ;
#70948 = CARTESIAN_POINT('Origin',(210.892277625407,548.59755658921,-35.2721601717612)) ;
#70949 = CARTESIAN_POINT('',(210.892277625407,567.170681589221,-35.0221601717611)) ;
#70950 = CARTESIAN_POINT('',(210.64227762541,567.170681589221,-35.2721601717611)) ;
#70951 = CARTESIAN_POINT('Origin',(210.517277625407,548.59755658921,-35.2721601717609)) ;
#70952 = CARTESIAN_POINT('',(210.517277625407,548.47255658921,-35.2721601717609)) ;
#70953 = CARTESIAN_POINT('',(210.517277625407,548.22255658921,-35.0221601717611)) ;
#70954 = CARTESIAN_POINT('Origin',(210.517277625407,548.22255658921,-35.2721601717609)) ;
#70955 = CARTESIAN_POINT('Origin',(210.517277625407,548.59755658921,-35.0221601717611)) ;
#70956 = CARTESIAN_POINT('Origin',(210.517277625407,548.59755658921,-35.2721601717609)) ;
#70957 = CARTESIAN_POINT('Origin',(205.938476772278,548.22255658921,-35.2721601717609)) ;
#70958 = CARTESIAN_POINT('',(209.814777625407,548.47255658921,-35.2721601717611)) ;
#70959 = CARTESIAN_POINT('',(209.814777625407,548.22255658921,-35.0221601717611)) ;
#70960 = CARTESIAN_POINT('Origin',(209.814777625407,548.22255658921,-35.2721601717611)) ;
#70961 = CARTESIAN_POINT('',(205.938476772278,548.22255658921,-35.0221601717609)) ;
#70962 = CARTESIAN_POINT('',(205.938476772278,548.47255658921,-35.2721601717609)) ;
#70963 = CARTESIAN_POINT('Origin',(209.814777625407,548.59755658921,-35.2721601717609)) ;
#70964 = CARTESIAN_POINT('',(209.689777625407,548.59755658921,-35.2721601717609)) ;
#70965 = CARTESIAN_POINT('',(209.439777625407,548.59755658921,-35.0221601717611)) ;
#70966 = CARTESIAN_POINT('Origin',(209.439777625407,548.59755658921,-35.2721601717609)) ;
#70967 = CARTESIAN_POINT('Origin',(209.814777625407,548.59755658921,-35.0221601717611)) ;
#70968 = CARTESIAN_POINT('Origin',(209.814777625407,548.59755658921,-35.2721601717609)) ;
#70969 = CARTESIAN_POINT('Origin',(209.439777625407,567.170681589221,-35.2721601717611)) ;
#70970 = CARTESIAN_POINT('',(209.689777625407,552.347556589211,-35.2721601717611)) ;
#70971 = CARTESIAN_POINT('',(209.439777625407,552.347556589211,-35.0221601717611)) ;
#70972 = CARTESIAN_POINT('Origin',(209.439777625407,552.347556589211,-35.2721601717611)) ;
#70973 = CARTESIAN_POINT('',(209.439777625407,567.170681589221,-35.0221601717611)) ;
#70974 = CARTESIAN_POINT('',(209.68977762541,567.170681589221,-35.2721601717611)) ;
#70975 = CARTESIAN_POINT('Origin',(209.814777625407,552.347556589211,-35.2721601717609)) ;
#70976 = CARTESIAN_POINT('Origin',(209.814777625407,552.347556589211,-35.0221601717611)) ;
#70977 = CARTESIAN_POINT('Origin',(209.814777625407,552.347556589211,-35.2721601717609)) ;
#70978 = CARTESIAN_POINT('Origin',(210.51727762541,548.59755658921,-35.7037040214914)) ;
#70979 = CARTESIAN_POINT('',(210.64227762541,548.59755658921,-39.2297690928544)) ;
#70980 = CARTESIAN_POINT('',(210.64227762541,548.59755658921,-35.7037040214914)) ;
#70981 = CARTESIAN_POINT('',(210.517277625411,548.47255658921,-39.2297690928544)) ;
#70982 = CARTESIAN_POINT('Origin',(210.51727762541,548.59755658921,-39.2297690928544)) ;
#70983 = CARTESIAN_POINT('',(210.517277625411,548.47255658921,-35.7037040214914)) ;
#70984 = CARTESIAN_POINT('Origin',(210.64227762541,545.86880658921,-33.4492690928543)) ;
#70985 = CARTESIAN_POINT('',(210.64227762541,552.347556589211,-39.2297690928544)) ;
#70986 = CARTESIAN_POINT('',(210.64227762541,552.347556589211,-33.7350190928543)) ;
#70987 = CARTESIAN_POINT('',(210.64227762541,548.488181589211,-39.2297690928544)) ;
#70988 = CARTESIAN_POINT('Origin',(210.51727762541,552.347556589211,-33.7350190928543)) ;
#70989 = CARTESIAN_POINT('',(210.51727762541,552.472556589211,-39.2297690928544)) ;
#70990 = CARTESIAN_POINT('',(210.51727762541,552.472556589211,-33.7350190928543)) ;
#70991 = CARTESIAN_POINT('Origin',(210.51727762541,552.347556589211,-39.2297690928544)) ;
#70992 = CARTESIAN_POINT('Origin',(197.30727762541,552.472556589211,-34.0207690928544)) ;
#70993 = CARTESIAN_POINT('',(209.81477762541,552.472556589211,-39.2297690928544)) ;
#70994 = CARTESIAN_POINT('',(209.81477762541,552.472556589211,-38.5610190928544)) ;
#70995 = CARTESIAN_POINT('',(207.75302762541,552.472556589211,-39.2297690928544)) ;
#70996 = CARTESIAN_POINT('Origin',(201.57290262541,543.222556589211,-35.2721601717607)) ;
#70997 = CARTESIAN_POINT('',(209.814777625407,543.222556589211,-35.0221601717611)) ;
#70998 = CARTESIAN_POINT('',(209.814777625407,542.972556589211,-35.2721601717611)) ;
#70999 = CARTESIAN_POINT('Origin',(209.814777625407,543.222556589211,-35.2721601717611)) ;
#71000 = CARTESIAN_POINT('',(210.517277625407,542.972556589211,-35.2721601717611)) ;
#71001 = CARTESIAN_POINT('',(201.57290262541,542.972556589211,-35.2721601717607)) ;
#71002 = CARTESIAN_POINT('',(210.517277625407,543.222556589211,-35.0221601717611)) ;
#71003 = CARTESIAN_POINT('Origin',(210.517277625407,543.222556589211,-35.2721601717611)) ;
#71004 = CARTESIAN_POINT('',(201.57290262541,543.222556589211,-35.0221601717607)) ;
#71005 = CARTESIAN_POINT('Origin',(210.517277625407,542.847556589211,-35.2721601717609)) ;
#71006 = CARTESIAN_POINT('',(210.642277625407,542.847556589211,-35.2721601717609)) ;
#71007 = CARTESIAN_POINT('',(210.892277625407,542.847556589211,-35.0221601717612)) ;
#71008 = CARTESIAN_POINT('Origin',(210.892277625407,542.847556589211,-35.2721601717609)) ;
#71009 = CARTESIAN_POINT('Origin',(210.517277625407,542.847556589211,-35.0221601717611)) ;
#71010 = CARTESIAN_POINT('Origin',(210.517277625407,542.847556589211,-35.2721601717609)) ;
#71011 = CARTESIAN_POINT('Origin',(210.892277625407,557.670681589221,-35.2721601717611)) ;
#71012 = CARTESIAN_POINT('',(210.642277625407,539.09755658921,-35.2721601717612)) ;
#71013 = CARTESIAN_POINT('',(210.892277625407,539.09755658921,-35.0221601717612)) ;
#71014 = CARTESIAN_POINT('Origin',(210.892277625407,539.09755658921,-35.2721601717612)) ;
#71015 = CARTESIAN_POINT('',(210.892277625407,557.670681589221,-35.0221601717611)) ;
#71016 = CARTESIAN_POINT('',(210.642277625409,557.670681589221,-35.2721601717611)) ;
#71017 = CARTESIAN_POINT('Origin',(210.517277625407,539.09755658921,-35.2721601717609)) ;
#71018 = CARTESIAN_POINT('',(210.517277625407,538.97255658921,-35.2721601717609)) ;
#71019 = CARTESIAN_POINT('',(210.517277625407,538.72255658921,-35.0221601717611)) ;
#71020 = CARTESIAN_POINT('Origin',(210.517277625407,538.72255658921,-35.2721601717609)) ;
#71021 = CARTESIAN_POINT('Origin',(210.517277625407,539.09755658921,-35.0221601717611)) ;
#71022 = CARTESIAN_POINT('Origin',(210.517277625407,539.09755658921,-35.2721601717609)) ;
#71023 = CARTESIAN_POINT('Origin',(205.938476772278,538.72255658921,-35.2721601717609)) ;
#71024 = CARTESIAN_POINT('',(209.814777625407,538.97255658921,-35.2721601717611)) ;
#71025 = CARTESIAN_POINT('',(209.814777625407,538.72255658921,-35.0221601717611)) ;
#71026 = CARTESIAN_POINT('Origin',(209.814777625407,538.72255658921,-35.2721601717611)) ;
#71027 = CARTESIAN_POINT('',(205.938476772278,538.72255658921,-35.0221601717609)) ;
#71028 = CARTESIAN_POINT('',(205.938476772278,538.97255658921,-35.2721601717609)) ;
#71029 = CARTESIAN_POINT('Origin',(209.814777625407,539.09755658921,-35.2721601717609)) ;
#71030 = CARTESIAN_POINT('',(209.689777625407,539.09755658921,-35.2721601717609)) ;
#71031 = CARTESIAN_POINT('',(209.439777625407,539.09755658921,-35.0221601717611)) ;
#71032 = CARTESIAN_POINT('Origin',(209.439777625407,539.09755658921,-35.2721601717609)) ;
#71033 = CARTESIAN_POINT('Origin',(209.814777625407,539.09755658921,-35.0221601717611)) ;
#71034 = CARTESIAN_POINT('Origin',(209.814777625407,539.09755658921,-35.2721601717609)) ;
#71035 = CARTESIAN_POINT('Origin',(209.439777625407,557.670681589221,-35.2721601717611)) ;
#71036 = CARTESIAN_POINT('',(209.689777625407,542.847556589211,-35.2721601717611)) ;
#71037 = CARTESIAN_POINT('',(209.439777625407,542.847556589211,-35.0221601717611)) ;
#71038 = CARTESIAN_POINT('Origin',(209.439777625407,542.847556589211,-35.2721601717611)) ;
#71039 = CARTESIAN_POINT('',(209.439777625407,557.670681589221,-35.0221601717611)) ;
#71040 = CARTESIAN_POINT('',(209.689777625408,557.670681589221,-35.2721601717611)) ;
#71041 = CARTESIAN_POINT('Origin',(209.814777625407,542.847556589211,-35.2721601717609)) ;
#71042 = CARTESIAN_POINT('Origin',(209.814777625407,542.847556589211,-35.0221601717611)) ;
#71043 = CARTESIAN_POINT('Origin',(209.814777625407,542.847556589211,-35.2721601717609)) ;
#71044 = CARTESIAN_POINT('Origin',(210.517277625409,539.09755658921,-35.7037040214914)) ;
#71045 = CARTESIAN_POINT('',(210.642277625409,539.09755658921,-39.2297690928544)) ;
#71046 = CARTESIAN_POINT('',(210.642277625409,539.09755658921,-35.7037040214914)) ;
#71047 = CARTESIAN_POINT('',(210.517277625409,538.97255658921,-39.2297690928544)) ;
#71048 = CARTESIAN_POINT('Origin',(210.517277625409,539.09755658921,-39.2297690928544)) ;
#71049 = CARTESIAN_POINT('',(210.517277625409,538.97255658921,-35.7037040214914)) ;
#71050 = CARTESIAN_POINT('Origin',(210.642277625409,536.36880658921,-33.4492690928543)) ;
#71051 = CARTESIAN_POINT('',(210.642277625409,542.847556589211,-39.2297690928544)) ;
#71052 = CARTESIAN_POINT('',(210.642277625409,542.847556589211,-33.7350190928543)) ;
#71053 = CARTESIAN_POINT('',(210.642277625409,538.988181589211,-39.2297690928544)) ;
#71054 = CARTESIAN_POINT('Origin',(210.517277625409,542.847556589211,-33.7350190928543)) ;
#71055 = CARTESIAN_POINT('',(210.517277625409,542.972556589211,-39.2297690928544)) ;
#71056 = CARTESIAN_POINT('',(210.517277625409,542.972556589211,-33.7350190928543)) ;
#71057 = CARTESIAN_POINT('Origin',(210.517277625409,542.847556589211,-39.2297690928544)) ;
#71058 = CARTESIAN_POINT('Origin',(197.307277625408,542.972556589211,-34.0207690928544)) ;
#71059 = CARTESIAN_POINT('',(209.814777625408,542.972556589211,-39.2297690928544)) ;
#71060 = CARTESIAN_POINT('',(209.814777625408,542.972556589211,-38.5610190928544)) ;
#71061 = CARTESIAN_POINT('',(207.753027625408,542.972556589211,-39.2297690928544)) ;
#71062 = CARTESIAN_POINT('Origin',(201.57290262541,609.722556589211,-35.2721601717607)) ;
#71063 = CARTESIAN_POINT('',(201.559777625407,609.722556589211,-35.0221601717607)) ;
#71064 = CARTESIAN_POINT('',(201.559777625407,609.472556589211,-35.2721601717607)) ;
#71065 = CARTESIAN_POINT('Origin',(201.559777625407,609.722556589211,-35.2721601717607)) ;
#71066 = CARTESIAN_POINT('',(202.262277625407,609.472556589211,-35.2721601717608)) ;
#71067 = CARTESIAN_POINT('',(201.57290262541,609.472556589211,-35.2721601717607)) ;
#71068 = CARTESIAN_POINT('',(202.262277625407,609.722556589211,-35.0221601717608)) ;
#71069 = CARTESIAN_POINT('Origin',(202.262277625407,609.722556589211,-35.2721601717608)) ;
#71070 = CARTESIAN_POINT('',(201.57290262541,609.722556589211,-35.0221601717607)) ;
#71071 = CARTESIAN_POINT('Origin',(202.262277625407,609.347556589211,-35.2721601717609)) ;
#71072 = CARTESIAN_POINT('',(202.387277625407,609.347556589211,-35.2721601717609)) ;
#71073 = CARTESIAN_POINT('',(202.637277625407,609.347556589211,-35.0221601717608)) ;
#71074 = CARTESIAN_POINT('Origin',(202.637277625407,609.347556589211,-35.2721601717609)) ;
#71075 = CARTESIAN_POINT('Origin',(202.262277625407,609.347556589211,-35.0221601717607)) ;
#71076 = CARTESIAN_POINT('Origin',(202.262277625407,609.347556589211,-35.2721601717609)) ;
#71077 = CARTESIAN_POINT('Origin',(202.637277625407,624.170681589221,-35.2721601717608)) ;
#71078 = CARTESIAN_POINT('',(202.387277625407,605.597556589211,-35.2721601717608)) ;
#71079 = CARTESIAN_POINT('',(202.637277625407,605.597556589211,-35.0221601717608)) ;
#71080 = CARTESIAN_POINT('Origin',(202.637277625407,605.597556589211,-35.2721601717608)) ;
#71081 = CARTESIAN_POINT('',(202.637277625407,624.170681589221,-35.0221601717608)) ;
#71082 = CARTESIAN_POINT('',(202.38727762542,624.170681589221,-35.2721601717608)) ;
#71083 = CARTESIAN_POINT('Origin',(202.262277625407,605.597556589211,-35.2721601717609)) ;
#71084 = CARTESIAN_POINT('',(202.262277625407,605.472556589211,-35.2721601717609)) ;
#71085 = CARTESIAN_POINT('',(202.262277625407,605.222556589211,-35.0221601717608)) ;
#71086 = CARTESIAN_POINT('Origin',(202.262277625407,605.222556589211,-35.2721601717609)) ;
#71087 = CARTESIAN_POINT('Origin',(202.262277625407,605.597556589211,-35.0221601717607)) ;
#71088 = CARTESIAN_POINT('Origin',(202.262277625407,605.597556589211,-35.2721601717609)) ;
#71089 = CARTESIAN_POINT('Origin',(205.938476772278,605.222556589211,-35.2721601717609)) ;
#71090 = CARTESIAN_POINT('',(201.559777625407,605.472556589211,-35.2721601717607)) ;
#71091 = CARTESIAN_POINT('',(201.559777625407,605.222556589211,-35.0221601717607)) ;
#71092 = CARTESIAN_POINT('Origin',(201.559777625407,605.222556589211,-35.2721601717607)) ;
#71093 = CARTESIAN_POINT('',(205.938476772278,605.222556589211,-35.0221601717609)) ;
#71094 = CARTESIAN_POINT('',(205.938476772278,605.472556589211,-35.2721601717609)) ;
#71095 = CARTESIAN_POINT('Origin',(201.559777625407,605.597556589211,-35.2721601717609)) ;
#71096 = CARTESIAN_POINT('',(201.184777625407,605.597556589211,-35.0221601717607)) ;
#71097 = CARTESIAN_POINT('Origin',(201.184777625407,605.597556589211,-35.2721601717609)) ;
#71098 = CARTESIAN_POINT('Origin',(201.559777625407,605.597556589211,-35.0221601717607)) ;
#71099 = CARTESIAN_POINT('Origin',(201.559777625407,605.597556589211,-35.2721601717609)) ;
#71100 = CARTESIAN_POINT('Origin',(201.184777625407,624.170681589221,-35.2721601717607)) ;
#71101 = CARTESIAN_POINT('',(201.184777625407,609.347556589211,-35.0221601717607)) ;
#71102 = CARTESIAN_POINT('Origin',(201.184777625407,609.347556589211,-35.2721601717607)) ;
#71103 = CARTESIAN_POINT('',(201.184777625407,624.170681589221,-35.0221601717607)) ;
#71104 = CARTESIAN_POINT('Origin',(201.559777625407,609.347556589211,-35.2721601717609)) ;
#71105 = CARTESIAN_POINT('Origin',(201.559777625407,609.347556589211,-35.0221601717607)) ;
#71106 = CARTESIAN_POINT('Origin',(201.559777625407,609.347556589211,-35.2721601717609)) ;
#71107 = CARTESIAN_POINT('Origin',(202.26227762542,605.597556589211,-35.8624540214915)) ;
#71108 = CARTESIAN_POINT('',(202.38727762542,605.597556589211,-39.2297700580612)) ;
#71109 = CARTESIAN_POINT('',(202.38727762542,605.597556589211,-35.8624540214915)) ;
#71110 = CARTESIAN_POINT('',(202.26227762542,605.472556589211,-39.2297700580612)) ;
#71111 = CARTESIAN_POINT('Origin',(202.26227762542,605.597556589211,-39.2297700580612)) ;
#71112 = CARTESIAN_POINT('',(202.26227762542,605.472556589211,-35.8624540214915)) ;
#71113 = CARTESIAN_POINT('Origin',(202.38727762542,602.868806589211,-33.7667690928544)) ;
#71114 = CARTESIAN_POINT('',(202.38727762542,606.962556589212,-39.4182700580611)) ;
#71115 = CARTESIAN_POINT('',(202.38727762542,606.962556589212,-37.6444650424525)) ;
#71116 = CARTESIAN_POINT('',(202.38727762542,606.774056589212,-39.2297700580612)) ;
#71117 = CARTESIAN_POINT('Origin',(202.38727762542,606.774056589212,-39.4182700580611)) ;
#71118 = CARTESIAN_POINT('',(202.38727762542,605.488181589211,-39.2297700580612)) ;
#71119 = CARTESIAN_POINT('',(202.38727762542,609.347556589211,-39.2297700580612)) ;
#71120 = CARTESIAN_POINT('',(202.38727762542,609.347556589211,-33.8937690928544)) ;
#71121 = CARTESIAN_POINT('',(202.38727762542,608.171056589212,-39.2297700580612)) ;
#71122 = CARTESIAN_POINT('',(202.38727762542,605.488181589211,-39.2297700580612)) ;
#71123 = CARTESIAN_POINT('',(202.38727762542,607.982556589212,-39.4182700580611)) ;
#71124 = CARTESIAN_POINT('Origin',(202.38727762542,608.171056589212,-39.4182700580612)) ;
#71125 = CARTESIAN_POINT('',(202.38727762542,607.982556589212,-39.8669650424525)) ;
#71126 = CARTESIAN_POINT('Origin',(202.26227762542,609.347556589211,-33.8937690928544)) ;
#71127 = CARTESIAN_POINT('',(202.26227762542,609.472556589211,-39.2297700580612)) ;
#71128 = CARTESIAN_POINT('',(202.26227762542,609.472556589211,-33.8937690928544)) ;
#71129 = CARTESIAN_POINT('Origin',(202.26227762542,609.347556589211,-39.2297700580612)) ;
#71130 = CARTESIAN_POINT('Origin',(197.30727762542,609.472556589211,-34.0207690928544)) ;
#71131 = CARTESIAN_POINT('',(201.55977762542,609.472556589211,-39.2297700580612)) ;
#71132 = CARTESIAN_POINT('',(201.55977762542,609.472556589211,-38.5610190928544)) ;
#71133 = CARTESIAN_POINT('',(207.75302762542,609.472556589211,-39.2297700580612)) ;
#71134 = CARTESIAN_POINT('Origin',(201.57290262541,600.222556589211,-35.2721601717607)) ;
#71135 = CARTESIAN_POINT('',(201.559777625407,600.222556589211,-35.0221601717607)) ;
#71136 = CARTESIAN_POINT('',(201.559777625407,599.972556589211,-35.2721601717607)) ;
#71137 = CARTESIAN_POINT('Origin',(201.559777625407,600.222556589211,-35.2721601717607)) ;
#71138 = CARTESIAN_POINT('',(202.262277625407,599.972556589211,-35.2721601717608)) ;
#71139 = CARTESIAN_POINT('',(201.57290262541,599.972556589211,-35.2721601717607)) ;
#71140 = CARTESIAN_POINT('',(202.262277625407,600.222556589211,-35.0221601717608)) ;
#71141 = CARTESIAN_POINT('Origin',(202.262277625407,600.222556589211,-35.2721601717608)) ;
#71142 = CARTESIAN_POINT('',(201.57290262541,600.222556589211,-35.0221601717607)) ;
#71143 = CARTESIAN_POINT('Origin',(202.262277625407,599.847556589211,-35.2721601717609)) ;
#71144 = CARTESIAN_POINT('',(202.387277625407,599.847556589211,-35.2721601717609)) ;
#71145 = CARTESIAN_POINT('',(202.637277625407,599.847556589211,-35.0221601717608)) ;
#71146 = CARTESIAN_POINT('Origin',(202.637277625407,599.847556589211,-35.2721601717609)) ;
#71147 = CARTESIAN_POINT('Origin',(202.262277625407,599.847556589211,-35.0221601717607)) ;
#71148 = CARTESIAN_POINT('Origin',(202.262277625407,599.847556589211,-35.2721601717609)) ;
#71149 = CARTESIAN_POINT('Origin',(202.637277625407,614.670681589221,-35.2721601717608)) ;
#71150 = CARTESIAN_POINT('',(202.387277625407,596.097556589211,-35.2721601717608)) ;
#71151 = CARTESIAN_POINT('',(202.637277625407,596.097556589211,-35.0221601717608)) ;
#71152 = CARTESIAN_POINT('Origin',(202.637277625407,596.097556589211,-35.2721601717608)) ;
#71153 = CARTESIAN_POINT('',(202.637277625407,614.670681589221,-35.0221601717608)) ;
#71154 = CARTESIAN_POINT('',(202.387277625418,614.670681589221,-35.2721601717608)) ;
#71155 = CARTESIAN_POINT('Origin',(202.262277625407,596.097556589211,-35.2721601717609)) ;
#71156 = CARTESIAN_POINT('',(202.262277625407,595.972556589211,-35.2721601717609)) ;
#71157 = CARTESIAN_POINT('',(202.262277625407,595.722556589211,-35.0221601717608)) ;
#71158 = CARTESIAN_POINT('Origin',(202.262277625407,595.722556589211,-35.2721601717609)) ;
#71159 = CARTESIAN_POINT('Origin',(202.262277625407,596.097556589211,-35.0221601717607)) ;
#71160 = CARTESIAN_POINT('Origin',(202.262277625407,596.097556589211,-35.2721601717609)) ;
#71161 = CARTESIAN_POINT('Origin',(205.938476772278,595.722556589211,-35.2721601717609)) ;
#71162 = CARTESIAN_POINT('',(201.559777625407,595.972556589211,-35.2721601717607)) ;
#71163 = CARTESIAN_POINT('',(201.559777625407,595.722556589211,-35.0221601717607)) ;
#71164 = CARTESIAN_POINT('Origin',(201.559777625407,595.722556589211,-35.2721601717607)) ;
#71165 = CARTESIAN_POINT('',(205.938476772278,595.722556589211,-35.0221601717609)) ;
#71166 = CARTESIAN_POINT('',(205.938476772278,595.972556589211,-35.2721601717609)) ;
#71167 = CARTESIAN_POINT('Origin',(201.559777625407,596.097556589211,-35.2721601717609)) ;
#71168 = CARTESIAN_POINT('',(201.184777625407,596.097556589211,-35.0221601717607)) ;
#71169 = CARTESIAN_POINT('Origin',(201.184777625407,596.097556589211,-35.2721601717609)) ;
#71170 = CARTESIAN_POINT('Origin',(201.559777625407,596.097556589211,-35.0221601717607)) ;
#71171 = CARTESIAN_POINT('Origin',(201.559777625407,596.097556589211,-35.2721601717609)) ;
#71172 = CARTESIAN_POINT('Origin',(201.184777625407,614.670681589221,-35.2721601717607)) ;
#71173 = CARTESIAN_POINT('',(201.184777625407,599.847556589211,-35.0221601717607)) ;
#71174 = CARTESIAN_POINT('Origin',(201.184777625407,599.847556589211,-35.2721601717607)) ;
#71175 = CARTESIAN_POINT('',(201.184777625407,614.670681589221,-35.0221601717607)) ;
#71176 = CARTESIAN_POINT('Origin',(201.559777625407,599.847556589211,-35.2721601717609)) ;
#71177 = CARTESIAN_POINT('Origin',(201.559777625407,599.847556589211,-35.0221601717607)) ;
#71178 = CARTESIAN_POINT('Origin',(201.559777625407,599.847556589211,-35.2721601717609)) ;
#71179 = CARTESIAN_POINT('Origin',(202.262277625418,596.097556589211,-35.8624540214915)) ;
#71180 = CARTESIAN_POINT('',(202.387277625418,596.097556589211,-39.2297700580612)) ;
#71181 = CARTESIAN_POINT('',(202.387277625418,596.097556589211,-35.8624540214915)) ;
#71182 = CARTESIAN_POINT('',(202.262277625418,595.972556589211,-39.2297700580612)) ;
#71183 = CARTESIAN_POINT('Origin',(202.262277625418,596.097556589211,-39.2297700580612)) ;
#71184 = CARTESIAN_POINT('',(202.262277625418,595.972556589211,-35.8624540214915)) ;
#71185 = CARTESIAN_POINT('Origin',(202.387277625418,593.368806589211,-33.7667690928544)) ;
#71186 = CARTESIAN_POINT('',(202.387277625418,597.462556589212,-39.4182700580611)) ;
#71187 = CARTESIAN_POINT('',(202.387277625418,597.462556589212,-37.6444650424525)) ;
#71188 = CARTESIAN_POINT('',(202.387277625418,597.274056589212,-39.2297700580612)) ;
#71189 = CARTESIAN_POINT('Origin',(202.387277625418,597.274056589212,-39.4182700580611)) ;
#71190 = CARTESIAN_POINT('',(202.387277625418,595.988181589211,-39.2297700580612)) ;
#71191 = CARTESIAN_POINT('',(202.387277625418,599.847556589211,-39.2297700580612)) ;
#71192 = CARTESIAN_POINT('',(202.387277625418,599.847556589211,-33.8937690928544)) ;
#71193 = CARTESIAN_POINT('',(202.387277625418,598.671056589212,-39.2297700580612)) ;
#71194 = CARTESIAN_POINT('',(202.387277625418,595.988181589211,-39.2297700580612)) ;
#71195 = CARTESIAN_POINT('',(202.387277625418,598.482556589212,-39.4182700580611)) ;
#71196 = CARTESIAN_POINT('Origin',(202.387277625418,598.671056589212,-39.4182700580612)) ;
#71197 = CARTESIAN_POINT('',(202.387277625418,598.482556589212,-39.8669650424525)) ;
#71198 = CARTESIAN_POINT('Origin',(202.262277625418,599.847556589211,-33.8937690928544)) ;
#71199 = CARTESIAN_POINT('',(202.262277625418,599.972556589211,-39.2297700580612)) ;
#71200 = CARTESIAN_POINT('',(202.262277625418,599.972556589211,-33.8937690928544)) ;
#71201 = CARTESIAN_POINT('Origin',(202.262277625418,599.847556589211,-39.2297700580612)) ;
#71202 = CARTESIAN_POINT('Origin',(197.307277625418,599.972556589211,-34.0207690928544)) ;
#71203 = CARTESIAN_POINT('',(201.559777625419,599.972556589211,-39.2297700580612)) ;
#71204 = CARTESIAN_POINT('',(201.559777625419,599.972556589211,-38.5610190928544)) ;
#71205 = CARTESIAN_POINT('',(207.753027625418,599.972556589211,-39.2297700580612)) ;
#71206 = CARTESIAN_POINT('Origin',(201.57290262541,590.722556589211,-35.2721601717607)) ;
#71207 = CARTESIAN_POINT('',(201.559777625407,590.722556589211,-35.0221601717607)) ;
#71208 = CARTESIAN_POINT('',(201.559777625407,590.472556589211,-35.2721601717607)) ;
#71209 = CARTESIAN_POINT('Origin',(201.559777625407,590.722556589211,-35.2721601717607)) ;
#71210 = CARTESIAN_POINT('',(202.262277625407,590.472556589211,-35.2721601717608)) ;
#71211 = CARTESIAN_POINT('',(201.57290262541,590.472556589211,-35.2721601717607)) ;
#71212 = CARTESIAN_POINT('',(202.262277625407,590.722556589211,-35.0221601717608)) ;
#71213 = CARTESIAN_POINT('Origin',(202.262277625407,590.722556589211,-35.2721601717608)) ;
#71214 = CARTESIAN_POINT('',(201.57290262541,590.722556589211,-35.0221601717607)) ;
#71215 = CARTESIAN_POINT('Origin',(202.262277625407,590.347556589211,-35.2721601717609)) ;
#71216 = CARTESIAN_POINT('',(202.387277625407,590.347556589211,-35.2721601717609)) ;
#71217 = CARTESIAN_POINT('',(202.637277625407,590.347556589211,-35.0221601717608)) ;
#71218 = CARTESIAN_POINT('Origin',(202.637277625407,590.347556589211,-35.2721601717609)) ;
#71219 = CARTESIAN_POINT('Origin',(202.262277625407,590.347556589211,-35.0221601717608)) ;
#71220 = CARTESIAN_POINT('Origin',(202.262277625407,590.347556589211,-35.2721601717609)) ;
#71221 = CARTESIAN_POINT('Origin',(202.637277625407,605.170681589221,-35.2721601717608)) ;
#71222 = CARTESIAN_POINT('',(202.387277625407,586.597556589211,-35.2721601717608)) ;
#71223 = CARTESIAN_POINT('',(202.637277625407,586.597556589211,-35.0221601717608)) ;
#71224 = CARTESIAN_POINT('Origin',(202.637277625407,586.597556589211,-35.2721601717608)) ;
#71225 = CARTESIAN_POINT('',(202.637277625407,605.170681589221,-35.0221601717608)) ;
#71226 = CARTESIAN_POINT('',(202.387277625417,605.170681589221,-35.2721601717608)) ;
#71227 = CARTESIAN_POINT('Origin',(202.262277625407,586.597556589211,-35.2721601717609)) ;
#71228 = CARTESIAN_POINT('',(202.262277625407,586.472556589211,-35.2721601717609)) ;
#71229 = CARTESIAN_POINT('',(202.262277625407,586.222556589211,-35.0221601717608)) ;
#71230 = CARTESIAN_POINT('Origin',(202.262277625407,586.222556589211,-35.2721601717609)) ;
#71231 = CARTESIAN_POINT('Origin',(202.262277625407,586.597556589211,-35.0221601717608)) ;
#71232 = CARTESIAN_POINT('Origin',(202.262277625407,586.597556589211,-35.2721601717609)) ;
#71233 = CARTESIAN_POINT('Origin',(205.938476772278,586.222556589211,-35.2721601717609)) ;
#71234 = CARTESIAN_POINT('',(201.559777625407,586.472556589211,-35.2721601717607)) ;
#71235 = CARTESIAN_POINT('',(201.559777625407,586.222556589211,-35.0221601717607)) ;
#71236 = CARTESIAN_POINT('Origin',(201.559777625407,586.222556589211,-35.2721601717607)) ;
#71237 = CARTESIAN_POINT('',(205.938476772278,586.222556589211,-35.0221601717609)) ;
#71238 = CARTESIAN_POINT('',(205.938476772278,586.472556589211,-35.2721601717609)) ;
#71239 = CARTESIAN_POINT('Origin',(201.559777625407,586.597556589211,-35.2721601717609)) ;
#71240 = CARTESIAN_POINT('',(201.184777625407,586.597556589211,-35.0221601717607)) ;
#71241 = CARTESIAN_POINT('Origin',(201.184777625407,586.597556589211,-35.2721601717609)) ;
#71242 = CARTESIAN_POINT('Origin',(201.559777625407,586.597556589211,-35.0221601717607)) ;
#71243 = CARTESIAN_POINT('Origin',(201.559777625407,586.597556589211,-35.2721601717609)) ;
#71244 = CARTESIAN_POINT('Origin',(201.184777625407,605.170681589221,-35.2721601717607)) ;
#71245 = CARTESIAN_POINT('',(201.184777625407,590.347556589211,-35.0221601717607)) ;
#71246 = CARTESIAN_POINT('Origin',(201.184777625407,590.347556589211,-35.2721601717607)) ;
#71247 = CARTESIAN_POINT('',(201.184777625407,605.170681589221,-35.0221601717607)) ;
#71248 = CARTESIAN_POINT('Origin',(201.559777625407,590.347556589211,-35.2721601717609)) ;
#71249 = CARTESIAN_POINT('Origin',(201.559777625407,590.347556589211,-35.0221601717607)) ;
#71250 = CARTESIAN_POINT('Origin',(201.559777625407,590.347556589211,-35.2721601717609)) ;
#71251 = CARTESIAN_POINT('Origin',(202.262277625417,586.597556589211,-35.8624540214915)) ;
#71252 = CARTESIAN_POINT('',(202.387277625417,586.597556589211,-39.2297700580612)) ;
#71253 = CARTESIAN_POINT('',(202.387277625417,586.597556589211,-35.8624540214915)) ;
#71254 = CARTESIAN_POINT('',(202.262277625417,586.472556589211,-39.2297700580612)) ;
#71255 = CARTESIAN_POINT('Origin',(202.262277625417,586.597556589211,-39.2297700580612)) ;
#71256 = CARTESIAN_POINT('',(202.262277625417,586.472556589211,-35.8624540214915)) ;
#71257 = CARTESIAN_POINT('Origin',(202.387277625417,583.868806589211,-33.7667690928544)) ;
#71258 = CARTESIAN_POINT('',(202.387277625417,587.962556589212,-39.4182700580611)) ;
#71259 = CARTESIAN_POINT('',(202.387277625417,587.962556589212,-37.6444650424525)) ;
#71260 = CARTESIAN_POINT('',(202.387277625417,587.774056589212,-39.2297700580612)) ;
#71261 = CARTESIAN_POINT('Origin',(202.387277625417,587.774056589212,-39.4182700580611)) ;
#71262 = CARTESIAN_POINT('',(202.387277625417,586.488181589211,-39.2297700580612)) ;
#71263 = CARTESIAN_POINT('',(202.387277625417,590.347556589211,-39.2297700580612)) ;
#71264 = CARTESIAN_POINT('',(202.387277625417,590.347556589211,-33.8937690928544)) ;
#71265 = CARTESIAN_POINT('',(202.387277625417,589.171056589212,-39.2297700580612)) ;
#71266 = CARTESIAN_POINT('',(202.387277625417,586.488181589211,-39.2297700580612)) ;
#71267 = CARTESIAN_POINT('',(202.387277625417,588.982556589212,-39.4182700580611)) ;
#71268 = CARTESIAN_POINT('Origin',(202.387277625417,589.171056589212,-39.4182700580612)) ;
#71269 = CARTESIAN_POINT('',(202.387277625417,588.982556589212,-39.8669650424525)) ;
#71270 = CARTESIAN_POINT('Origin',(202.262277625417,590.347556589211,-33.8937690928544)) ;
#71271 = CARTESIAN_POINT('',(202.262277625417,590.472556589211,-39.2297700580612)) ;
#71272 = CARTESIAN_POINT('',(202.262277625417,590.472556589211,-33.8937690928544)) ;
#71273 = CARTESIAN_POINT('Origin',(202.262277625417,590.347556589211,-39.2297700580612)) ;
#71274 = CARTESIAN_POINT('Origin',(197.307277625417,590.472556589211,-34.0207690928544)) ;
#71275 = CARTESIAN_POINT('',(201.559777625417,590.472556589211,-39.2297700580612)) ;
#71276 = CARTESIAN_POINT('',(201.559777625417,590.472556589211,-38.5610190928544)) ;
#71277 = CARTESIAN_POINT('',(207.753027625417,590.472556589211,-39.2297700580612)) ;
#71278 = CARTESIAN_POINT('Origin',(201.57290262541,581.222556589211,-35.2721601717607)) ;
#71279 = CARTESIAN_POINT('',(201.559777625407,581.222556589211,-35.0221601717607)) ;
#71280 = CARTESIAN_POINT('',(201.559777625407,580.972556589211,-35.2721601717607)) ;
#71281 = CARTESIAN_POINT('Origin',(201.559777625407,581.222556589211,-35.2721601717607)) ;
#71282 = CARTESIAN_POINT('',(202.262277625407,580.972556589211,-35.2721601717608)) ;
#71283 = CARTESIAN_POINT('',(201.57290262541,580.972556589211,-35.2721601717607)) ;
#71284 = CARTESIAN_POINT('',(202.262277625407,581.222556589211,-35.0221601717608)) ;
#71285 = CARTESIAN_POINT('Origin',(202.262277625407,581.222556589211,-35.2721601717608)) ;
#71286 = CARTESIAN_POINT('',(201.57290262541,581.222556589211,-35.0221601717607)) ;
#71287 = CARTESIAN_POINT('Origin',(202.262277625407,580.847556589211,-35.2721601717609)) ;
#71288 = CARTESIAN_POINT('',(202.387277625407,580.847556589211,-35.2721601717609)) ;
#71289 = CARTESIAN_POINT('',(202.637277625407,580.847556589211,-35.0221601717608)) ;
#71290 = CARTESIAN_POINT('Origin',(202.637277625407,580.847556589211,-35.2721601717609)) ;
#71291 = CARTESIAN_POINT('Origin',(202.262277625407,580.847556589211,-35.0221601717608)) ;
#71292 = CARTESIAN_POINT('Origin',(202.262277625407,580.847556589211,-35.2721601717609)) ;
#71293 = CARTESIAN_POINT('Origin',(202.637277625407,595.670681589221,-35.2721601717608)) ;
#71294 = CARTESIAN_POINT('',(202.387277625407,577.097556589211,-35.2721601717608)) ;
#71295 = CARTESIAN_POINT('',(202.637277625407,577.097556589211,-35.0221601717608)) ;
#71296 = CARTESIAN_POINT('Origin',(202.637277625407,577.097556589211,-35.2721601717608)) ;
#71297 = CARTESIAN_POINT('',(202.637277625407,595.670681589221,-35.0221601717608)) ;
#71298 = CARTESIAN_POINT('',(202.387277625415,595.670681589221,-35.2721601717608)) ;
#71299 = CARTESIAN_POINT('Origin',(202.262277625407,577.097556589211,-35.2721601717609)) ;
#71300 = CARTESIAN_POINT('',(202.262277625407,576.972556589211,-35.2721601717609)) ;
#71301 = CARTESIAN_POINT('',(202.262277625407,576.722556589211,-35.0221601717608)) ;
#71302 = CARTESIAN_POINT('Origin',(202.262277625407,576.722556589211,-35.2721601717609)) ;
#71303 = CARTESIAN_POINT('Origin',(202.262277625407,577.097556589211,-35.0221601717608)) ;
#71304 = CARTESIAN_POINT('Origin',(202.262277625407,577.097556589211,-35.2721601717609)) ;
#71305 = CARTESIAN_POINT('Origin',(205.938476772278,576.722556589211,-35.2721601717609)) ;
#71306 = CARTESIAN_POINT('',(201.559777625407,576.972556589211,-35.2721601717607)) ;
#71307 = CARTESIAN_POINT('',(201.559777625407,576.722556589211,-35.0221601717607)) ;
#71308 = CARTESIAN_POINT('Origin',(201.559777625407,576.722556589211,-35.2721601717607)) ;
#71309 = CARTESIAN_POINT('',(205.938476772278,576.722556589211,-35.0221601717609)) ;
#71310 = CARTESIAN_POINT('',(205.938476772278,576.972556589211,-35.2721601717609)) ;
#71311 = CARTESIAN_POINT('Origin',(201.559777625407,577.097556589211,-35.2721601717609)) ;
#71312 = CARTESIAN_POINT('',(201.184777625407,577.097556589211,-35.0221601717607)) ;
#71313 = CARTESIAN_POINT('Origin',(201.184777625407,577.097556589211,-35.2721601717609)) ;
#71314 = CARTESIAN_POINT('Origin',(201.559777625407,577.097556589211,-35.0221601717607)) ;
#71315 = CARTESIAN_POINT('Origin',(201.559777625407,577.097556589211,-35.2721601717609)) ;
#71316 = CARTESIAN_POINT('Origin',(201.184777625407,595.670681589221,-35.2721601717607)) ;
#71317 = CARTESIAN_POINT('',(201.184777625407,580.847556589211,-35.0221601717607)) ;
#71318 = CARTESIAN_POINT('Origin',(201.184777625407,580.847556589211,-35.2721601717607)) ;
#71319 = CARTESIAN_POINT('',(201.184777625407,595.670681589221,-35.0221601717607)) ;
#71320 = CARTESIAN_POINT('Origin',(201.559777625407,580.847556589211,-35.2721601717609)) ;
#71321 = CARTESIAN_POINT('Origin',(201.559777625407,580.847556589211,-35.0221601717607)) ;
#71322 = CARTESIAN_POINT('Origin',(201.559777625407,580.847556589211,-35.2721601717609)) ;
#71323 = CARTESIAN_POINT('Origin',(202.262277625415,577.097556589211,-35.8624540214915)) ;
#71324 = CARTESIAN_POINT('',(202.387277625415,577.097556589211,-39.2297700580612)) ;
#71325 = CARTESIAN_POINT('',(202.387277625415,577.097556589211,-35.8624540214915)) ;
#71326 = CARTESIAN_POINT('',(202.262277625415,576.972556589211,-39.2297700580612)) ;
#71327 = CARTESIAN_POINT('Origin',(202.262277625415,577.097556589211,-39.2297700580612)) ;
#71328 = CARTESIAN_POINT('',(202.262277625415,576.972556589211,-35.8624540214915)) ;
#71329 = CARTESIAN_POINT('Origin',(202.387277625415,574.368806589211,-33.7667690928544)) ;
#71330 = CARTESIAN_POINT('',(202.387277625415,578.462556589212,-39.4182700580611)) ;
#71331 = CARTESIAN_POINT('',(202.387277625415,578.462556589212,-37.6444650424525)) ;
#71332 = CARTESIAN_POINT('',(202.387277625415,578.274056589212,-39.2297700580612)) ;
#71333 = CARTESIAN_POINT('Origin',(202.387277625415,578.274056589212,-39.4182700580611)) ;
#71334 = CARTESIAN_POINT('',(202.387277625415,576.988181589211,-39.2297700580612)) ;
#71335 = CARTESIAN_POINT('',(202.387277625415,580.847556589211,-39.2297700580612)) ;
#71336 = CARTESIAN_POINT('',(202.387277625415,580.847556589211,-33.8937690928544)) ;
#71337 = CARTESIAN_POINT('',(202.387277625415,579.671056589212,-39.2297700580612)) ;
#71338 = CARTESIAN_POINT('',(202.387277625415,576.988181589211,-39.2297700580612)) ;
#71339 = CARTESIAN_POINT('',(202.387277625415,579.482556589212,-39.4182700580611)) ;
#71340 = CARTESIAN_POINT('Origin',(202.387277625415,579.671056589212,-39.4182700580612)) ;
#71341 = CARTESIAN_POINT('',(202.387277625415,579.482556589212,-39.8669650424525)) ;
#71342 = CARTESIAN_POINT('Origin',(202.262277625415,580.847556589211,-33.8937690928544)) ;
#71343 = CARTESIAN_POINT('',(202.262277625415,580.972556589211,-39.2297700580612)) ;
#71344 = CARTESIAN_POINT('',(202.262277625415,580.972556589211,-33.8937690928544)) ;
#71345 = CARTESIAN_POINT('Origin',(202.262277625415,580.847556589211,-39.2297700580612)) ;
#71346 = CARTESIAN_POINT('Origin',(197.307277625415,580.972556589211,-34.0207690928544)) ;
#71347 = CARTESIAN_POINT('',(201.559777625415,580.972556589211,-39.2297700580612)) ;
#71348 = CARTESIAN_POINT('',(201.559777625415,580.972556589211,-38.5610190928544)) ;
#71349 = CARTESIAN_POINT('',(207.753027625415,580.972556589211,-39.2297700580612)) ;
#71350 = CARTESIAN_POINT('Origin',(201.57290262541,571.722556589211,-35.2721601717607)) ;
#71351 = CARTESIAN_POINT('',(201.559777625407,571.722556589211,-35.0221601717607)) ;
#71352 = CARTESIAN_POINT('',(201.559777625407,571.472556589211,-35.2721601717607)) ;
#71353 = CARTESIAN_POINT('Origin',(201.559777625407,571.722556589211,-35.2721601717607)) ;
#71354 = CARTESIAN_POINT('',(202.262277625407,571.472556589211,-35.2721601717608)) ;
#71355 = CARTESIAN_POINT('',(201.57290262541,571.472556589211,-35.2721601717607)) ;
#71356 = CARTESIAN_POINT('',(202.262277625407,571.722556589211,-35.0221601717608)) ;
#71357 = CARTESIAN_POINT('Origin',(202.262277625407,571.722556589211,-35.2721601717608)) ;
#71358 = CARTESIAN_POINT('',(201.57290262541,571.722556589211,-35.0221601717607)) ;
#71359 = CARTESIAN_POINT('Origin',(202.262277625407,571.347556589211,-35.2721601717609)) ;
#71360 = CARTESIAN_POINT('',(202.387277625407,571.347556589211,-35.2721601717609)) ;
#71361 = CARTESIAN_POINT('',(202.637277625407,571.347556589211,-35.0221601717608)) ;
#71362 = CARTESIAN_POINT('Origin',(202.637277625407,571.347556589211,-35.2721601717609)) ;
#71363 = CARTESIAN_POINT('Origin',(202.262277625407,571.347556589211,-35.0221601717608)) ;
#71364 = CARTESIAN_POINT('Origin',(202.262277625407,571.347556589211,-35.2721601717609)) ;
#71365 = CARTESIAN_POINT('Origin',(202.637277625407,586.170681589221,-35.2721601717608)) ;
#71366 = CARTESIAN_POINT('',(202.387277625407,567.59755658921,-35.2721601717608)) ;
#71367 = CARTESIAN_POINT('',(202.637277625407,567.59755658921,-35.0221601717608)) ;
#71368 = CARTESIAN_POINT('Origin',(202.637277625407,567.59755658921,-35.2721601717608)) ;
#71369 = CARTESIAN_POINT('',(202.637277625407,586.170681589221,-35.0221601717608)) ;
#71370 = CARTESIAN_POINT('',(202.387277625413,586.170681589221,-35.2721601717608)) ;
#71371 = CARTESIAN_POINT('Origin',(202.262277625407,567.59755658921,-35.2721601717609)) ;
#71372 = CARTESIAN_POINT('',(202.262277625407,567.472556589211,-35.2721601717609)) ;
#71373 = CARTESIAN_POINT('',(202.262277625407,567.222556589211,-35.0221601717608)) ;
#71374 = CARTESIAN_POINT('Origin',(202.262277625407,567.222556589211,-35.2721601717609)) ;
#71375 = CARTESIAN_POINT('Origin',(202.262277625407,567.59755658921,-35.0221601717608)) ;
#71376 = CARTESIAN_POINT('Origin',(202.262277625407,567.59755658921,-35.2721601717609)) ;
#71377 = CARTESIAN_POINT('Origin',(205.938476772278,567.222556589211,-35.2721601717609)) ;
#71378 = CARTESIAN_POINT('',(201.559777625407,567.472556589211,-35.2721601717607)) ;
#71379 = CARTESIAN_POINT('',(201.559777625407,567.222556589211,-35.0221601717607)) ;
#71380 = CARTESIAN_POINT('Origin',(201.559777625407,567.222556589211,-35.2721601717607)) ;
#71381 = CARTESIAN_POINT('',(205.938476772278,567.222556589211,-35.0221601717609)) ;
#71382 = CARTESIAN_POINT('',(205.938476772278,567.47255658921,-35.2721601717609)) ;
#71383 = CARTESIAN_POINT('Origin',(201.559777625407,567.597556589211,-35.2721601717609)) ;
#71384 = CARTESIAN_POINT('',(201.184777625407,567.597556589211,-35.0221601717607)) ;
#71385 = CARTESIAN_POINT('Origin',(201.184777625407,567.597556589211,-35.2721601717609)) ;
#71386 = CARTESIAN_POINT('Origin',(201.559777625407,567.597556589211,-35.0221601717607)) ;
#71387 = CARTESIAN_POINT('Origin',(201.559777625407,567.597556589211,-35.2721601717609)) ;
#71388 = CARTESIAN_POINT('Origin',(201.184777625407,586.170681589221,-35.2721601717607)) ;
#71389 = CARTESIAN_POINT('',(201.184777625407,571.347556589211,-35.0221601717607)) ;
#71390 = CARTESIAN_POINT('Origin',(201.184777625407,571.347556589211,-35.2721601717607)) ;
#71391 = CARTESIAN_POINT('',(201.184777625407,586.170681589221,-35.0221601717607)) ;
#71392 = CARTESIAN_POINT('Origin',(201.559777625407,571.347556589211,-35.2721601717609)) ;
#71393 = CARTESIAN_POINT('Origin',(201.559777625407,571.347556589211,-35.0221601717607)) ;
#71394 = CARTESIAN_POINT('Origin',(201.559777625407,571.347556589211,-35.2721601717609)) ;
#71395 = CARTESIAN_POINT('Origin',(202.262277625413,567.59755658921,-35.8624540214915)) ;
#71396 = CARTESIAN_POINT('',(202.387277625413,567.59755658921,-39.2297700580612)) ;
#71397 = CARTESIAN_POINT('',(202.387277625413,567.59755658921,-35.8624540214915)) ;
#71398 = CARTESIAN_POINT('',(202.262277625413,567.47255658921,-39.2297700580612)) ;
#71399 = CARTESIAN_POINT('Origin',(202.262277625413,567.59755658921,-39.2297700580612)) ;
#71400 = CARTESIAN_POINT('',(202.262277625413,567.47255658921,-35.8624540214915)) ;
#71401 = CARTESIAN_POINT('Origin',(202.387277625413,564.868806589211,-33.7667690928544)) ;
#71402 = CARTESIAN_POINT('',(202.387277625413,568.962556589212,-39.4182700580611)) ;
#71403 = CARTESIAN_POINT('',(202.387277625413,568.962556589212,-37.6444650424525)) ;
#71404 = CARTESIAN_POINT('',(202.387277625413,568.774056589212,-39.2297700580612)) ;
#71405 = CARTESIAN_POINT('Origin',(202.387277625413,568.774056589212,-39.4182700580611)) ;
#71406 = CARTESIAN_POINT('',(202.387277625413,567.488181589211,-39.2297700580612)) ;
#71407 = CARTESIAN_POINT('',(202.387277625413,571.347556589211,-39.2297700580612)) ;
#71408 = CARTESIAN_POINT('',(202.387277625413,571.347556589211,-33.8937690928544)) ;
#71409 = CARTESIAN_POINT('',(202.387277625413,570.171056589212,-39.2297700580612)) ;
#71410 = CARTESIAN_POINT('',(202.387277625413,567.488181589211,-39.2297700580612)) ;
#71411 = CARTESIAN_POINT('',(202.387277625413,569.982556589212,-39.4182700580611)) ;
#71412 = CARTESIAN_POINT('Origin',(202.387277625413,570.171056589212,-39.4182700580612)) ;
#71413 = CARTESIAN_POINT('',(202.387277625413,569.982556589212,-39.8669650424525)) ;
#71414 = CARTESIAN_POINT('Origin',(202.262277625413,571.347556589211,-33.8937690928544)) ;
#71415 = CARTESIAN_POINT('',(202.262277625413,571.472556589211,-39.2297700580612)) ;
#71416 = CARTESIAN_POINT('',(202.262277625413,571.472556589211,-33.8937690928544)) ;
#71417 = CARTESIAN_POINT('Origin',(202.262277625413,571.347556589211,-39.2297700580612)) ;
#71418 = CARTESIAN_POINT('Origin',(197.307277625413,571.472556589211,-34.0207690928544)) ;
#71419 = CARTESIAN_POINT('',(201.559777625414,571.472556589211,-39.2297700580612)) ;
#71420 = CARTESIAN_POINT('',(201.559777625414,571.472556589211,-38.5610190928544)) ;
#71421 = CARTESIAN_POINT('',(207.753027625413,571.472556589211,-39.2297700580612)) ;
#71422 = CARTESIAN_POINT('Origin',(201.57290262541,562.222556589211,-35.2721601717607)) ;
#71423 = CARTESIAN_POINT('',(201.559777625407,562.222556589211,-35.0221601717607)) ;
#71424 = CARTESIAN_POINT('',(201.559777625407,561.972556589211,-35.2721601717607)) ;
#71425 = CARTESIAN_POINT('Origin',(201.559777625407,562.222556589211,-35.2721601717607)) ;
#71426 = CARTESIAN_POINT('',(202.262277625407,561.972556589211,-35.2721601717608)) ;
#71427 = CARTESIAN_POINT('',(201.57290262541,561.972556589211,-35.2721601717607)) ;
#71428 = CARTESIAN_POINT('',(202.262277625407,562.222556589211,-35.0221601717608)) ;
#71429 = CARTESIAN_POINT('Origin',(202.262277625407,562.222556589211,-35.2721601717608)) ;
#71430 = CARTESIAN_POINT('',(201.57290262541,562.222556589211,-35.0221601717607)) ;
#71431 = CARTESIAN_POINT('Origin',(202.262277625407,561.847556589211,-35.2721601717609)) ;
#71432 = CARTESIAN_POINT('',(202.387277625407,561.847556589211,-35.2721601717609)) ;
#71433 = CARTESIAN_POINT('',(202.637277625407,561.847556589211,-35.0221601717608)) ;
#71434 = CARTESIAN_POINT('Origin',(202.637277625407,561.847556589211,-35.2721601717609)) ;
#71435 = CARTESIAN_POINT('Origin',(202.262277625407,561.847556589211,-35.0221601717608)) ;
#71436 = CARTESIAN_POINT('Origin',(202.262277625407,561.847556589211,-35.2721601717609)) ;
#71437 = CARTESIAN_POINT('Origin',(202.637277625407,576.670681589221,-35.2721601717608)) ;
#71438 = CARTESIAN_POINT('',(202.387277625407,558.09755658921,-35.2721601717608)) ;
#71439 = CARTESIAN_POINT('',(202.637277625407,558.09755658921,-35.0221601717608)) ;
#71440 = CARTESIAN_POINT('Origin',(202.637277625407,558.09755658921,-35.2721601717608)) ;
#71441 = CARTESIAN_POINT('',(202.637277625407,576.670681589221,-35.0221601717608)) ;
#71442 = CARTESIAN_POINT('',(202.387277625412,576.670681589221,-35.2721601717608)) ;
#71443 = CARTESIAN_POINT('Origin',(202.262277625407,558.09755658921,-35.2721601717609)) ;
#71444 = CARTESIAN_POINT('',(202.262277625407,557.97255658921,-35.2721601717609)) ;
#71445 = CARTESIAN_POINT('',(202.262277625407,557.722556589211,-35.0221601717608)) ;
#71446 = CARTESIAN_POINT('Origin',(202.262277625407,557.722556589211,-35.2721601717609)) ;
#71447 = CARTESIAN_POINT('Origin',(202.262277625407,558.09755658921,-35.0221601717608)) ;
#71448 = CARTESIAN_POINT('Origin',(202.262277625407,558.09755658921,-35.2721601717609)) ;
#71449 = CARTESIAN_POINT('Origin',(205.938476772278,557.722556589211,-35.2721601717609)) ;
#71450 = CARTESIAN_POINT('',(201.559777625407,557.97255658921,-35.2721601717607)) ;
#71451 = CARTESIAN_POINT('',(201.559777625407,557.722556589211,-35.0221601717607)) ;
#71452 = CARTESIAN_POINT('Origin',(201.559777625407,557.722556589211,-35.2721601717607)) ;
#71453 = CARTESIAN_POINT('',(205.938476772278,557.722556589211,-35.0221601717609)) ;
#71454 = CARTESIAN_POINT('',(205.938476772278,557.97255658921,-35.2721601717609)) ;
#71455 = CARTESIAN_POINT('Origin',(201.559777625407,558.097556589211,-35.2721601717609)) ;
#71456 = CARTESIAN_POINT('',(201.184777625407,558.097556589211,-35.0221601717607)) ;
#71457 = CARTESIAN_POINT('Origin',(201.184777625407,558.097556589211,-35.2721601717609)) ;
#71458 = CARTESIAN_POINT('Origin',(201.559777625407,558.097556589211,-35.0221601717607)) ;
#71459 = CARTESIAN_POINT('Origin',(201.559777625407,558.097556589211,-35.2721601717609)) ;
#71460 = CARTESIAN_POINT('Origin',(201.184777625407,576.670681589221,-35.2721601717607)) ;
#71461 = CARTESIAN_POINT('',(201.184777625407,561.847556589211,-35.0221601717607)) ;
#71462 = CARTESIAN_POINT('Origin',(201.184777625407,561.847556589211,-35.2721601717607)) ;
#71463 = CARTESIAN_POINT('',(201.184777625407,576.670681589221,-35.0221601717607)) ;
#71464 = CARTESIAN_POINT('Origin',(201.559777625407,561.847556589211,-35.2721601717609)) ;
#71465 = CARTESIAN_POINT('Origin',(201.559777625407,561.847556589211,-35.0221601717607)) ;
#71466 = CARTESIAN_POINT('Origin',(201.559777625407,561.847556589211,-35.2721601717609)) ;
#71467 = CARTESIAN_POINT('Origin',(202.262277625412,558.09755658921,-35.8624540214915)) ;
#71468 = CARTESIAN_POINT('',(202.387277625412,558.09755658921,-39.2297700580612)) ;
#71469 = CARTESIAN_POINT('',(202.387277625412,558.09755658921,-35.8624540214915)) ;
#71470 = CARTESIAN_POINT('',(202.262277625412,557.97255658921,-39.2297700580612)) ;
#71471 = CARTESIAN_POINT('Origin',(202.262277625412,558.09755658921,-39.2297700580612)) ;
#71472 = CARTESIAN_POINT('',(202.262277625412,557.97255658921,-35.8624540214915)) ;
#71473 = CARTESIAN_POINT('Origin',(202.387277625412,555.368806589211,-33.7667690928544)) ;
#71474 = CARTESIAN_POINT('',(202.387277625412,559.462556589212,-39.4182700580611)) ;
#71475 = CARTESIAN_POINT('',(202.387277625412,559.462556589212,-37.6444650424525)) ;
#71476 = CARTESIAN_POINT('',(202.387277625412,559.274056589212,-39.2297700580612)) ;
#71477 = CARTESIAN_POINT('Origin',(202.387277625412,559.274056589212,-39.4182700580611)) ;
#71478 = CARTESIAN_POINT('',(202.387277625412,557.988181589211,-39.2297700580612)) ;
#71479 = CARTESIAN_POINT('',(202.387277625412,561.847556589211,-39.2297700580612)) ;
#71480 = CARTESIAN_POINT('',(202.387277625412,561.847556589211,-33.8937690928544)) ;
#71481 = CARTESIAN_POINT('',(202.387277625412,560.671056589212,-39.2297700580612)) ;
#71482 = CARTESIAN_POINT('',(202.387277625412,557.988181589211,-39.2297700580612)) ;
#71483 = CARTESIAN_POINT('',(202.387277625412,560.482556589212,-39.4182700580611)) ;
#71484 = CARTESIAN_POINT('Origin',(202.387277625412,560.671056589212,-39.4182700580612)) ;
#71485 = CARTESIAN_POINT('',(202.387277625412,560.482556589212,-39.8669650424525)) ;
#71486 = CARTESIAN_POINT('Origin',(202.262277625412,561.847556589211,-33.8937690928544)) ;
#71487 = CARTESIAN_POINT('',(202.262277625412,561.972556589211,-39.2297700580612)) ;
#71488 = CARTESIAN_POINT('',(202.262277625412,561.972556589211,-33.8937690928544)) ;
#71489 = CARTESIAN_POINT('Origin',(202.262277625412,561.847556589211,-39.2297700580612)) ;
#71490 = CARTESIAN_POINT('Origin',(197.307277625412,561.972556589211,-34.0207690928544)) ;
#71491 = CARTESIAN_POINT('',(201.559777625412,561.972556589211,-39.2297700580612)) ;
#71492 = CARTESIAN_POINT('',(201.559777625412,561.972556589211,-38.5610190928544)) ;
#71493 = CARTESIAN_POINT('',(207.753027625412,561.972556589211,-39.2297700580612)) ;
#71494 = CARTESIAN_POINT('Origin',(201.57290262541,552.722556589211,-35.2721601717607)) ;
#71495 = CARTESIAN_POINT('',(201.559777625407,552.722556589211,-35.0221601717607)) ;
#71496 = CARTESIAN_POINT('',(201.559777625407,552.472556589211,-35.2721601717607)) ;
#71497 = CARTESIAN_POINT('Origin',(201.559777625407,552.722556589211,-35.2721601717607)) ;
#71498 = CARTESIAN_POINT('',(202.262277625407,552.472556589211,-35.2721601717608)) ;
#71499 = CARTESIAN_POINT('',(201.57290262541,552.472556589211,-35.2721601717607)) ;
#71500 = CARTESIAN_POINT('',(202.262277625407,552.722556589211,-35.0221601717608)) ;
#71501 = CARTESIAN_POINT('Origin',(202.262277625407,552.722556589211,-35.2721601717608)) ;
#71502 = CARTESIAN_POINT('',(201.57290262541,552.722556589211,-35.0221601717607)) ;
#71503 = CARTESIAN_POINT('Origin',(202.262277625407,552.347556589211,-35.2721601717609)) ;
#71504 = CARTESIAN_POINT('',(202.387277625407,552.347556589211,-35.2721601717609)) ;
#71505 = CARTESIAN_POINT('',(202.637277625407,552.347556589211,-35.0221601717608)) ;
#71506 = CARTESIAN_POINT('Origin',(202.637277625407,552.347556589211,-35.2721601717609)) ;
#71507 = CARTESIAN_POINT('Origin',(202.262277625407,552.347556589211,-35.0221601717608)) ;
#71508 = CARTESIAN_POINT('Origin',(202.262277625407,552.347556589211,-35.2721601717609)) ;
#71509 = CARTESIAN_POINT('Origin',(202.637277625407,567.170681589221,-35.2721601717608)) ;
#71510 = CARTESIAN_POINT('',(202.387277625407,548.59755658921,-35.2721601717608)) ;
#71511 = CARTESIAN_POINT('',(202.637277625407,548.59755658921,-35.0221601717608)) ;
#71512 = CARTESIAN_POINT('Origin',(202.637277625407,548.59755658921,-35.2721601717608)) ;
#71513 = CARTESIAN_POINT('',(202.637277625407,567.170681589221,-35.0221601717608)) ;
#71514 = CARTESIAN_POINT('',(202.38727762541,567.170681589221,-35.2721601717608)) ;
#71515 = CARTESIAN_POINT('Origin',(202.262277625407,548.59755658921,-35.2721601717609)) ;
#71516 = CARTESIAN_POINT('',(202.262277625407,548.47255658921,-35.2721601717609)) ;
#71517 = CARTESIAN_POINT('',(202.262277625407,548.22255658921,-35.0221601717608)) ;
#71518 = CARTESIAN_POINT('Origin',(202.262277625407,548.22255658921,-35.2721601717609)) ;
#71519 = CARTESIAN_POINT('Origin',(202.262277625407,548.59755658921,-35.0221601717608)) ;
#71520 = CARTESIAN_POINT('Origin',(202.262277625407,548.59755658921,-35.2721601717609)) ;
#71521 = CARTESIAN_POINT('Origin',(205.938476772278,548.22255658921,-35.2721601717609)) ;
#71522 = CARTESIAN_POINT('',(201.559777625407,548.47255658921,-35.2721601717607)) ;
#71523 = CARTESIAN_POINT('',(201.559777625407,548.22255658921,-35.0221601717607)) ;
#71524 = CARTESIAN_POINT('Origin',(201.559777625407,548.22255658921,-35.2721601717607)) ;
#71525 = CARTESIAN_POINT('',(205.938476772278,548.22255658921,-35.0221601717609)) ;
#71526 = CARTESIAN_POINT('',(205.938476772278,548.47255658921,-35.2721601717609)) ;
#71527 = CARTESIAN_POINT('Origin',(201.559777625407,548.59755658921,-35.2721601717609)) ;
#71528 = CARTESIAN_POINT('',(201.184777625407,548.59755658921,-35.0221601717607)) ;
#71529 = CARTESIAN_POINT('Origin',(201.184777625407,548.59755658921,-35.2721601717609)) ;
#71530 = CARTESIAN_POINT('Origin',(201.559777625407,548.59755658921,-35.0221601717607)) ;
#71531 = CARTESIAN_POINT('Origin',(201.559777625407,548.59755658921,-35.2721601717609)) ;
#71532 = CARTESIAN_POINT('Origin',(201.184777625407,567.170681589221,-35.2721601717607)) ;
#71533 = CARTESIAN_POINT('',(201.184777625407,552.347556589211,-35.0221601717607)) ;
#71534 = CARTESIAN_POINT('Origin',(201.184777625407,552.347556589211,-35.2721601717607)) ;
#71535 = CARTESIAN_POINT('',(201.184777625407,567.170681589221,-35.0221601717607)) ;
#71536 = CARTESIAN_POINT('Origin',(201.559777625407,552.347556589211,-35.2721601717609)) ;
#71537 = CARTESIAN_POINT('Origin',(201.559777625407,552.347556589211,-35.0221601717607)) ;
#71538 = CARTESIAN_POINT('Origin',(201.559777625407,552.347556589211,-35.2721601717609)) ;
#71539 = CARTESIAN_POINT('Origin',(202.26227762541,548.59755658921,-35.8624540214915)) ;
#71540 = CARTESIAN_POINT('',(202.38727762541,548.59755658921,-39.2297700580612)) ;
#71541 = CARTESIAN_POINT('',(202.38727762541,548.59755658921,-35.8624540214915)) ;
#71542 = CARTESIAN_POINT('',(202.26227762541,548.47255658921,-39.2297700580612)) ;
#71543 = CARTESIAN_POINT('Origin',(202.26227762541,548.59755658921,-39.2297700580612)) ;
#71544 = CARTESIAN_POINT('',(202.26227762541,548.47255658921,-35.8624540214915)) ;
#71545 = CARTESIAN_POINT('Origin',(202.38727762541,545.868806589211,-33.7667690928544)) ;
#71546 = CARTESIAN_POINT('',(202.38727762541,549.962556589212,-39.4182700580611)) ;
#71547 = CARTESIAN_POINT('',(202.38727762541,549.962556589212,-37.6444650424525)) ;
#71548 = CARTESIAN_POINT('',(202.38727762541,549.774056589212,-39.2297700580612)) ;
#71549 = CARTESIAN_POINT('Origin',(202.38727762541,549.774056589212,-39.4182700580611)) ;
#71550 = CARTESIAN_POINT('',(202.38727762541,548.488181589211,-39.2297700580612)) ;
#71551 = CARTESIAN_POINT('',(202.38727762541,552.347556589211,-39.2297700580612)) ;
#71552 = CARTESIAN_POINT('',(202.38727762541,552.347556589211,-33.8937690928544)) ;
#71553 = CARTESIAN_POINT('',(202.38727762541,551.171056589212,-39.2297700580612)) ;
#71554 = CARTESIAN_POINT('',(202.38727762541,548.488181589211,-39.2297700580612)) ;
#71555 = CARTESIAN_POINT('',(202.38727762541,550.982556589212,-39.4182700580611)) ;
#71556 = CARTESIAN_POINT('Origin',(202.38727762541,551.171056589212,-39.4182700580612)) ;
#71557 = CARTESIAN_POINT('',(202.38727762541,550.982556589212,-39.8669650424525)) ;
#71558 = CARTESIAN_POINT('Origin',(202.26227762541,552.347556589211,-33.8937690928544)) ;
#71559 = CARTESIAN_POINT('',(202.26227762541,552.472556589211,-39.2297700580612)) ;
#71560 = CARTESIAN_POINT('',(202.26227762541,552.472556589211,-33.8937690928544)) ;
#71561 = CARTESIAN_POINT('Origin',(202.26227762541,552.347556589211,-39.2297700580612)) ;
#71562 = CARTESIAN_POINT('Origin',(197.30727762541,552.472556589211,-34.0207690928544)) ;
#71563 = CARTESIAN_POINT('',(201.55977762541,552.472556589211,-39.2297700580612)) ;
#71564 = CARTESIAN_POINT('',(201.55977762541,552.472556589211,-38.5610190928544)) ;
#71565 = CARTESIAN_POINT('',(207.75302762541,552.472556589211,-39.2297700580612)) ;
#71566 = CARTESIAN_POINT('Origin',(201.57290262541,543.222556589211,-35.2721601717607)) ;
#71567 = CARTESIAN_POINT('',(201.559777625407,543.222556589211,-35.0221601717607)) ;
#71568 = CARTESIAN_POINT('',(201.559777625407,542.972556589211,-35.2721601717607)) ;
#71569 = CARTESIAN_POINT('Origin',(201.559777625407,543.222556589211,-35.2721601717607)) ;
#71570 = CARTESIAN_POINT('',(202.262277625407,542.972556589211,-35.2721601717608)) ;
#71571 = CARTESIAN_POINT('',(201.57290262541,542.972556589211,-35.2721601717607)) ;
#71572 = CARTESIAN_POINT('',(202.262277625407,543.222556589211,-35.0221601717608)) ;
#71573 = CARTESIAN_POINT('Origin',(202.262277625407,543.222556589211,-35.2721601717608)) ;
#71574 = CARTESIAN_POINT('',(201.57290262541,543.222556589211,-35.0221601717607)) ;
#71575 = CARTESIAN_POINT('Origin',(202.262277625407,542.847556589211,-35.2721601717609)) ;
#71576 = CARTESIAN_POINT('',(202.387277625407,542.847556589211,-35.2721601717609)) ;
#71577 = CARTESIAN_POINT('',(202.637277625407,542.847556589211,-35.0221601717608)) ;
#71578 = CARTESIAN_POINT('Origin',(202.637277625407,542.847556589211,-35.2721601717609)) ;
#71579 = CARTESIAN_POINT('Origin',(202.262277625407,542.847556589211,-35.0221601717608)) ;
#71580 = CARTESIAN_POINT('Origin',(202.262277625407,542.847556589211,-35.2721601717609)) ;
#71581 = CARTESIAN_POINT('Origin',(202.637277625407,557.670681589221,-35.2721601717608)) ;
#71582 = CARTESIAN_POINT('',(202.387277625407,539.09755658921,-35.2721601717608)) ;
#71583 = CARTESIAN_POINT('',(202.637277625407,539.09755658921,-35.0221601717608)) ;
#71584 = CARTESIAN_POINT('Origin',(202.637277625407,539.09755658921,-35.2721601717608)) ;
#71585 = CARTESIAN_POINT('',(202.637277625407,557.670681589221,-35.0221601717608)) ;
#71586 = CARTESIAN_POINT('',(202.387277625408,557.670681589221,-35.2721601717608)) ;
#71587 = CARTESIAN_POINT('Origin',(202.262277625407,539.09755658921,-35.2721601717609)) ;
#71588 = CARTESIAN_POINT('',(202.262277625407,538.97255658921,-35.2721601717609)) ;
#71589 = CARTESIAN_POINT('',(202.262277625407,538.72255658921,-35.0221601717608)) ;
#71590 = CARTESIAN_POINT('Origin',(202.262277625407,538.72255658921,-35.2721601717609)) ;
#71591 = CARTESIAN_POINT('Origin',(202.262277625407,539.09755658921,-35.0221601717608)) ;
#71592 = CARTESIAN_POINT('Origin',(202.262277625407,539.09755658921,-35.2721601717609)) ;
#71593 = CARTESIAN_POINT('Origin',(205.938476772278,538.72255658921,-35.2721601717609)) ;
#71594 = CARTESIAN_POINT('',(201.559777625407,538.97255658921,-35.2721601717607)) ;
#71595 = CARTESIAN_POINT('',(201.559777625407,538.72255658921,-35.0221601717607)) ;
#71596 = CARTESIAN_POINT('Origin',(201.559777625407,538.72255658921,-35.2721601717607)) ;
#71597 = CARTESIAN_POINT('',(205.938476772278,538.72255658921,-35.0221601717609)) ;
#71598 = CARTESIAN_POINT('',(205.938476772278,538.97255658921,-35.2721601717609)) ;
#71599 = CARTESIAN_POINT('Origin',(201.559777625407,539.09755658921,-35.2721601717609)) ;
#71600 = CARTESIAN_POINT('',(201.184777625407,539.09755658921,-35.0221601717607)) ;
#71601 = CARTESIAN_POINT('Origin',(201.184777625407,539.09755658921,-35.2721601717609)) ;
#71602 = CARTESIAN_POINT('Origin',(201.559777625407,539.09755658921,-35.0221601717607)) ;
#71603 = CARTESIAN_POINT('Origin',(201.559777625407,539.09755658921,-35.2721601717609)) ;
#71604 = CARTESIAN_POINT('Origin',(201.184777625407,557.670681589221,-35.2721601717607)) ;
#71605 = CARTESIAN_POINT('',(201.184777625407,542.847556589211,-35.0221601717607)) ;
#71606 = CARTESIAN_POINT('Origin',(201.184777625407,542.847556589211,-35.2721601717607)) ;
#71607 = CARTESIAN_POINT('',(201.184777625407,557.670681589221,-35.0221601717607)) ;
#71608 = CARTESIAN_POINT('Origin',(201.559777625407,542.847556589211,-35.2721601717609)) ;
#71609 = CARTESIAN_POINT('Origin',(201.559777625407,542.847556589211,-35.0221601717607)) ;
#71610 = CARTESIAN_POINT('Origin',(201.559777625407,542.847556589211,-35.2721601717609)) ;
#71611 = CARTESIAN_POINT('Origin',(202.262277625408,539.09755658921,-35.8624540214915)) ;
#71612 = CARTESIAN_POINT('',(202.387277625408,539.09755658921,-39.2297700580612)) ;
#71613 = CARTESIAN_POINT('',(202.387277625408,539.09755658921,-35.8624540214915)) ;
#71614 = CARTESIAN_POINT('',(202.262277625408,538.97255658921,-39.2297700580612)) ;
#71615 = CARTESIAN_POINT('Origin',(202.262277625408,539.09755658921,-39.2297700580612)) ;
#71616 = CARTESIAN_POINT('',(202.262277625408,538.97255658921,-35.8624540214915)) ;
#71617 = CARTESIAN_POINT('Origin',(202.387277625408,536.368806589211,-33.7667690928544)) ;
#71618 = CARTESIAN_POINT('',(202.387277625408,540.462556589212,-39.4182700580611)) ;
#71619 = CARTESIAN_POINT('',(202.387277625408,540.462556589212,-37.6444650424525)) ;
#71620 = CARTESIAN_POINT('',(202.387277625408,540.274056589212,-39.2297700580612)) ;
#71621 = CARTESIAN_POINT('Origin',(202.387277625408,540.274056589212,-39.4182700580611)) ;
#71622 = CARTESIAN_POINT('',(202.387277625408,538.988181589211,-39.2297700580612)) ;
#71623 = CARTESIAN_POINT('',(202.387277625408,542.847556589211,-39.2297700580612)) ;
#71624 = CARTESIAN_POINT('',(202.387277625408,542.847556589211,-33.8937690928544)) ;
#71625 = CARTESIAN_POINT('',(202.387277625408,541.671056589212,-39.2297700580612)) ;
#71626 = CARTESIAN_POINT('',(202.387277625408,538.988181589211,-39.2297700580612)) ;
#71627 = CARTESIAN_POINT('',(202.387277625408,541.482556589212,-39.4182700580611)) ;
#71628 = CARTESIAN_POINT('Origin',(202.387277625408,541.671056589212,-39.4182700580612)) ;
#71629 = CARTESIAN_POINT('',(202.387277625408,541.482556589212,-39.8669650424525)) ;
#71630 = CARTESIAN_POINT('Origin',(202.262277625408,542.847556589211,-33.8937690928544)) ;
#71631 = CARTESIAN_POINT('',(202.262277625408,542.972556589211,-39.2297700580612)) ;
#71632 = CARTESIAN_POINT('',(202.262277625408,542.972556589211,-33.8937690928544)) ;
#71633 = CARTESIAN_POINT('Origin',(202.262277625408,542.847556589211,-39.2297700580612)) ;
#71634 = CARTESIAN_POINT('Origin',(197.307277625408,542.972556589211,-34.0207690928544)) ;
#71635 = CARTESIAN_POINT('',(201.559777625409,542.972556589211,-39.2297700580612)) ;
#71636 = CARTESIAN_POINT('',(201.559777625409,542.972556589211,-38.5610190928544)) ;
#71637 = CARTESIAN_POINT('',(207.753027625408,542.972556589211,-39.2297700580612)) ;
#71638 = CARTESIAN_POINT('Origin',(201.57290262541,533.722556589211,-35.2721601717607)) ;
#71639 = CARTESIAN_POINT('',(209.814777625407,533.722556589211,-35.0221601717611)) ;
#71640 = CARTESIAN_POINT('',(209.814777625407,533.472556589211,-35.2721601717611)) ;
#71641 = CARTESIAN_POINT('Origin',(209.814777625407,533.722556589211,-35.2721601717611)) ;
#71642 = CARTESIAN_POINT('',(210.517277625407,533.472556589211,-35.2721601717611)) ;
#71643 = CARTESIAN_POINT('',(201.57290262541,533.472556589211,-35.2721601717607)) ;
#71644 = CARTESIAN_POINT('',(210.517277625407,533.722556589211,-35.0221601717611)) ;
#71645 = CARTESIAN_POINT('Origin',(210.517277625407,533.722556589211,-35.2721601717611)) ;
#71646 = CARTESIAN_POINT('',(201.57290262541,533.722556589211,-35.0221601717607)) ;
#71647 = CARTESIAN_POINT('Origin',(210.517277625407,533.347556589211,-35.2721601717609)) ;
#71648 = CARTESIAN_POINT('',(210.642277625407,533.347556589211,-35.2721601717609)) ;
#71649 = CARTESIAN_POINT('',(210.892277625407,533.347556589211,-35.0221601717612)) ;
#71650 = CARTESIAN_POINT('Origin',(210.892277625407,533.347556589211,-35.2721601717609)) ;
#71651 = CARTESIAN_POINT('Origin',(210.517277625407,533.347556589211,-35.0221601717611)) ;
#71652 = CARTESIAN_POINT('Origin',(210.517277625407,533.347556589211,-35.2721601717609)) ;
#71653 = CARTESIAN_POINT('Origin',(210.892277625407,548.170681589221,-35.2721601717611)) ;
#71654 = CARTESIAN_POINT('',(210.642277625407,529.59755658921,-35.2721601717612)) ;
#71655 = CARTESIAN_POINT('',(210.892277625407,529.59755658921,-35.0221601717612)) ;
#71656 = CARTESIAN_POINT('Origin',(210.892277625407,529.59755658921,-35.2721601717612)) ;
#71657 = CARTESIAN_POINT('',(210.892277625407,548.170681589221,-35.0221601717611)) ;
#71658 = CARTESIAN_POINT('',(210.642277625407,548.170681589221,-35.2721601717611)) ;
#71659 = CARTESIAN_POINT('Origin',(210.517277625407,529.59755658921,-35.2721601717609)) ;
#71660 = CARTESIAN_POINT('',(210.517277625407,529.47255658921,-35.2721601717609)) ;
#71661 = CARTESIAN_POINT('',(210.517277625407,529.22255658921,-35.0221601717611)) ;
#71662 = CARTESIAN_POINT('Origin',(210.517277625407,529.22255658921,-35.2721601717609)) ;
#71663 = CARTESIAN_POINT('Origin',(210.517277625407,529.59755658921,-35.0221601717611)) ;
#71664 = CARTESIAN_POINT('Origin',(210.517277625407,529.59755658921,-35.2721601717609)) ;
#71665 = CARTESIAN_POINT('Origin',(205.938476772278,529.22255658921,-35.2721601717609)) ;
#71666 = CARTESIAN_POINT('',(209.814777625407,529.47255658921,-35.2721601717611)) ;
#71667 = CARTESIAN_POINT('',(209.814777625407,529.22255658921,-35.0221601717611)) ;
#71668 = CARTESIAN_POINT('Origin',(209.814777625407,529.22255658921,-35.2721601717611)) ;
#71669 = CARTESIAN_POINT('',(205.938476772278,529.22255658921,-35.0221601717609)) ;
#71670 = CARTESIAN_POINT('',(205.938476772278,529.47255658921,-35.2721601717609)) ;
#71671 = CARTESIAN_POINT('Origin',(209.814777625407,529.59755658921,-35.2721601717609)) ;
#71672 = CARTESIAN_POINT('',(209.689777625407,529.59755658921,-35.2721601717609)) ;
#71673 = CARTESIAN_POINT('',(209.439777625407,529.59755658921,-35.0221601717611)) ;
#71674 = CARTESIAN_POINT('Origin',(209.439777625407,529.59755658921,-35.2721601717609)) ;
#71675 = CARTESIAN_POINT('Origin',(209.814777625407,529.59755658921,-35.0221601717611)) ;
#71676 = CARTESIAN_POINT('Origin',(209.814777625407,529.59755658921,-35.2721601717609)) ;
#71677 = CARTESIAN_POINT('Origin',(209.439777625407,548.170681589221,-35.2721601717611)) ;
#71678 = CARTESIAN_POINT('',(209.689777625407,533.347556589211,-35.2721601717611)) ;
#71679 = CARTESIAN_POINT('',(209.439777625407,533.347556589211,-35.0221601717611)) ;
#71680 = CARTESIAN_POINT('Origin',(209.439777625407,533.347556589211,-35.2721601717611)) ;
#71681 = CARTESIAN_POINT('',(209.439777625407,548.170681589221,-35.0221601717611)) ;
#71682 = CARTESIAN_POINT('',(209.689777625407,548.170681589221,-35.2721601717611)) ;
#71683 = CARTESIAN_POINT('Origin',(209.814777625407,533.347556589211,-35.2721601717609)) ;
#71684 = CARTESIAN_POINT('Origin',(209.814777625407,533.347556589211,-35.0221601717611)) ;
#71685 = CARTESIAN_POINT('Origin',(209.814777625407,533.347556589211,-35.2721601717609)) ;
#71686 = CARTESIAN_POINT('Origin',(210.517277625407,529.59755658921,-35.7037040214914)) ;
#71687 = CARTESIAN_POINT('',(210.642277625407,529.59755658921,-39.2297690928544)) ;
#71688 = CARTESIAN_POINT('',(210.642277625407,529.59755658921,-35.7037040214914)) ;
#71689 = CARTESIAN_POINT('',(210.517277625407,529.47255658921,-39.2297690928544)) ;
#71690 = CARTESIAN_POINT('Origin',(210.517277625407,529.59755658921,-39.2297690928544)) ;
#71691 = CARTESIAN_POINT('',(210.517277625407,529.47255658921,-35.7037040214914)) ;
#71692 = CARTESIAN_POINT('Origin',(210.642277625407,526.86880658921,-33.4492690928543)) ;
#71693 = CARTESIAN_POINT('',(210.642277625407,533.347556589211,-39.2297690928544)) ;
#71694 = CARTESIAN_POINT('',(210.642277625407,533.347556589211,-33.7350190928543)) ;
#71695 = CARTESIAN_POINT('',(210.642277625407,529.488181589211,-39.2297690928544)) ;
#71696 = CARTESIAN_POINT('Origin',(210.517277625407,533.347556589211,-33.7350190928543)) ;
#71697 = CARTESIAN_POINT('',(210.517277625407,533.472556589211,-39.2297690928544)) ;
#71698 = CARTESIAN_POINT('',(210.517277625407,533.472556589211,-33.7350190928543)) ;
#71699 = CARTESIAN_POINT('Origin',(210.517277625407,533.347556589211,-39.2297690928544)) ;
#71700 = CARTESIAN_POINT('Origin',(197.307277625407,533.472556589211,-34.0207690928544)) ;
#71701 = CARTESIAN_POINT('',(209.814777625407,533.472556589211,-39.2297690928544)) ;
#71702 = CARTESIAN_POINT('',(209.814777625407,533.472556589211,-38.5610190928544)) ;
#71703 = CARTESIAN_POINT('',(207.753027625407,533.472556589211,-39.2297690928544)) ;
#71704 = CARTESIAN_POINT('Origin',(205.838527625413,569.472556589231,-35.0221601717609)) ;
#71705 = CARTESIAN_POINT('',(212.088527625407,535.548005939928,-35.0221601717612)) ;
#71706 = CARTESIAN_POINT('',(199.088527625407,535.548005939932,-35.0221601717606)) ;
#71707 = CARTESIAN_POINT('',(201.838527625407,535.54800593993,-35.0221601717607)) ;
#71708 = CARTESIAN_POINT('',(199.088527625406,527.3971072385,-35.0221601717606)) ;
#71709 = CARTESIAN_POINT('',(199.08852762541,547.972556589222,-35.0221601717606)) ;
#71710 = CARTESIAN_POINT('',(212.088527625406,527.397107238496,-35.0221601717612)) ;
#71711 = CARTESIAN_POINT('',(201.838527625406,527.397107238497,-35.0221601717607)) ;
#71712 = CARTESIAN_POINT('',(212.08852762541,547.97255658922,-35.0221601717612)) ;
#71713 = CARTESIAN_POINT('',(202.262277625407,533.722556589211,-35.0221601717608)) ;
#71714 = CARTESIAN_POINT('',(201.559777625407,533.722556589211,-35.0221601717607)) ;
#71715 = CARTESIAN_POINT('',(201.57290262541,533.722556589211,-35.0221601717607)) ;
#71716 = CARTESIAN_POINT('',(202.637277625407,533.347556589211,-35.0221601717608)) ;
#71717 = CARTESIAN_POINT('Origin',(202.262277625407,533.347556589211,-35.0221601717608)) ;
#71718 = CARTESIAN_POINT('',(202.637277625407,529.59755658921,-35.0221601717608)) ;
#71719 = CARTESIAN_POINT('',(202.637277625407,548.170681589221,-35.0221601717608)) ;
#71720 = CARTESIAN_POINT('',(202.262277625407,529.22255658921,-35.0221601717608)) ;
#71721 = CARTESIAN_POINT('Origin',(202.262277625407,529.59755658921,-35.0221601717608)) ;
#71722 = CARTESIAN_POINT('',(201.559777625407,529.22255658921,-35.0221601717607)) ;
#71723 = CARTESIAN_POINT('',(205.938476772278,529.22255658921,-35.0221601717609)) ;
#71724 = CARTESIAN_POINT('',(201.184777625407,529.59755658921,-35.0221601717607)) ;
#71725 = CARTESIAN_POINT('Origin',(201.559777625407,529.59755658921,-35.0221601717607)) ;
#71726 = CARTESIAN_POINT('',(201.184777625407,533.347556589211,-35.0221601717607)) ;
#71727 = CARTESIAN_POINT('',(201.184777625407,548.170681589221,-35.0221601717607)) ;
#71728 = CARTESIAN_POINT('Origin',(201.559777625407,533.347556589211,-35.0221601717607)) ;
#71729 = CARTESIAN_POINT('',(203.155186246464,531.472556589211,-35.0221601717609)) ;
#71730 = CARTESIAN_POINT('Origin',(206.038527625407,531.472556589211,-35.0221601717609)) ;
#71731 = CARTESIAN_POINT('Origin',(201.57290262541,533.722556589211,-35.2721601717607)) ;
#71732 = CARTESIAN_POINT('',(201.559777625407,533.472556589211,-35.2721601717607)) ;
#71733 = CARTESIAN_POINT('Origin',(201.559777625407,533.722556589211,-35.2721601717607)) ;
#71734 = CARTESIAN_POINT('',(202.262277625407,533.472556589211,-35.2721601717608)) ;
#71735 = CARTESIAN_POINT('',(201.57290262541,533.472556589211,-35.2721601717607)) ;
#71736 = CARTESIAN_POINT('Origin',(202.262277625407,533.722556589211,-35.2721601717608)) ;
#71737 = CARTESIAN_POINT('Origin',(202.262277625407,533.347556589211,-35.2721601717609)) ;
#71738 = CARTESIAN_POINT('',(202.387277625407,533.347556589211,-35.2721601717609)) ;
#71739 = CARTESIAN_POINT('Origin',(202.637277625407,533.347556589211,-35.2721601717609)) ;
#71740 = CARTESIAN_POINT('Origin',(202.262277625407,533.347556589211,-35.2721601717609)) ;
#71741 = CARTESIAN_POINT('Origin',(202.637277625407,548.170681589221,-35.2721601717608)) ;
#71742 = CARTESIAN_POINT('',(202.387277625407,529.59755658921,-35.2721601717608)) ;
#71743 = CARTESIAN_POINT('Origin',(202.637277625407,529.59755658921,-35.2721601717608)) ;
#71744 = CARTESIAN_POINT('',(202.387277625407,548.170681589221,-35.2721601717608)) ;
#71745 = CARTESIAN_POINT('Origin',(202.262277625407,529.59755658921,-35.2721601717609)) ;
#71746 = CARTESIAN_POINT('',(202.262277625407,529.47255658921,-35.2721601717609)) ;
#71747 = CARTESIAN_POINT('Origin',(202.262277625407,529.22255658921,-35.2721601717609)) ;
#71748 = CARTESIAN_POINT('Origin',(202.262277625407,529.59755658921,-35.2721601717609)) ;
#71749 = CARTESIAN_POINT('Origin',(205.938476772278,529.22255658921,-35.2721601717609)) ;
#71750 = CARTESIAN_POINT('',(201.559777625407,529.47255658921,-35.2721601717607)) ;
#71751 = CARTESIAN_POINT('Origin',(201.559777625407,529.22255658921,-35.2721601717607)) ;
#71752 = CARTESIAN_POINT('',(205.938476772278,529.47255658921,-35.2721601717609)) ;
#71753 = CARTESIAN_POINT('Origin',(201.559777625407,529.59755658921,-35.2721601717609)) ;
#71754 = CARTESIAN_POINT('Origin',(201.184777625407,529.59755658921,-35.2721601717609)) ;
#71755 = CARTESIAN_POINT('Origin',(201.559777625407,529.59755658921,-35.2721601717609)) ;
#71756 = CARTESIAN_POINT('Origin',(201.184777625407,548.170681589221,-35.2721601717607)) ;
#71757 = CARTESIAN_POINT('Origin',(201.184777625407,533.347556589211,-35.2721601717607)) ;
#71758 = CARTESIAN_POINT('Origin',(201.559777625407,533.347556589211,-35.2721601717609)) ;
#71759 = CARTESIAN_POINT('Origin',(201.559777625407,533.347556589211,-35.2721601717609)) ;
#71760 = CARTESIAN_POINT('Origin',(202.262277625407,529.59755658921,-35.8624540214915)) ;
#71761 = CARTESIAN_POINT('',(202.387277625407,529.59755658921,-39.2297700580612)) ;
#71762 = CARTESIAN_POINT('',(202.387277625407,529.59755658921,-35.8624540214915)) ;
#71763 = CARTESIAN_POINT('',(202.262277625407,529.47255658921,-39.2297700580612)) ;
#71764 = CARTESIAN_POINT('Origin',(202.262277625407,529.59755658921,-39.2297700580612)) ;
#71765 = CARTESIAN_POINT('',(202.262277625407,529.47255658921,-35.8624540214915)) ;
#71766 = CARTESIAN_POINT('Origin',(202.387277625407,526.868806589211,-33.7667690928544)) ;
#71767 = CARTESIAN_POINT('',(202.387277625407,533.347556589211,-39.2297700580612)) ;
#71768 = CARTESIAN_POINT('',(202.387277625407,533.347556589211,-33.8937690928544)) ;
#71769 = CARTESIAN_POINT('',(202.387277625407,532.171056589212,-39.2297700580612)) ;
#71770 = CARTESIAN_POINT('',(202.387277625407,529.488181589211,-39.2297700580612)) ;
#71771 = CARTESIAN_POINT('',(202.387277625407,531.982556589212,-39.4182700580611)) ;
#71772 = CARTESIAN_POINT('Origin',(202.387277625407,532.171056589212,-39.4182700580612)) ;
#71773 = CARTESIAN_POINT('',(202.387277625407,531.982556589212,-39.8669650424525)) ;
#71774 = CARTESIAN_POINT('',(202.387277625407,530.962556589212,-39.4182700580611)) ;
#71775 = CARTESIAN_POINT('',(202.387277625407,530.962556589212,-37.6444650424525)) ;
#71776 = CARTESIAN_POINT('',(202.387277625407,530.774056589212,-39.2297700580612)) ;
#71777 = CARTESIAN_POINT('Origin',(202.387277625407,530.774056589212,-39.4182700580611)) ;
#71778 = CARTESIAN_POINT('',(202.387277625407,529.488181589211,-39.2297700580612)) ;
#71779 = CARTESIAN_POINT('Origin',(202.262277625407,533.347556589211,-33.8937690928544)) ;
#71780 = CARTESIAN_POINT('',(202.262277625407,533.472556589211,-39.2297700580612)) ;
#71781 = CARTESIAN_POINT('',(202.262277625407,533.472556589211,-33.8937690928544)) ;
#71782 = CARTESIAN_POINT('Origin',(202.262277625407,533.347556589211,-39.2297700580612)) ;
#71783 = CARTESIAN_POINT('Origin',(197.307277625407,533.472556589211,-34.0207690928544)) ;
#71784 = CARTESIAN_POINT('',(201.559777625407,533.472556589211,-39.2297700580612)) ;
#71785 = CARTESIAN_POINT('',(201.559777625407,533.472556589211,-38.5610190928544)) ;
#71786 = CARTESIAN_POINT('',(207.753027625407,533.472556589211,-39.2297700580612)) ;
#71787 = CARTESIAN_POINT('Origin',(206.038425919142,529.47255658921,-37.9581389501285)) ;
#71788 = CARTESIAN_POINT('',(201.559777625407,529.47255658921,-39.2297700580612)) ;
#71789 = CARTESIAN_POINT('',(212.118601772275,529.47255658921,-39.2297700580611)) ;
#71790 = CARTESIAN_POINT('',(201.559777625407,529.47255658921,-40.5297040214914)) ;
#71791 = CARTESIAN_POINT('Origin',(201.559777625407,529.59755658921,-40.5297040214914)) ;
#71792 = CARTESIAN_POINT('Origin',(201.559777625407,529.59755658921,-39.2297700580612)) ;
#71793 = CARTESIAN_POINT('Origin',(201.559777625407,533.347556589211,-38.5610190928544)) ;
#71794 = CARTESIAN_POINT('Origin',(201.559777625407,533.347556589211,-39.2297700580612)) ;
#71795 = CARTESIAN_POINT('Origin',(206.038425919142,529.47255658921,-37.9581389501285)) ;
#71796 = CARTESIAN_POINT('',(209.814777625407,529.47255658921,-39.2297690928544)) ;
#71797 = CARTESIAN_POINT('',(212.118601772275,529.47255658921,-39.2297690928544)) ;
#71798 = CARTESIAN_POINT('',(209.814777625407,529.47255658921,-40.5297040214914)) ;
#71799 = CARTESIAN_POINT('Origin',(209.814777625407,529.59755658921,-40.5297040214914)) ;
#71800 = CARTESIAN_POINT('',(209.689777625407,529.59755658921,-39.2297690928544)) ;
#71801 = CARTESIAN_POINT('Origin',(209.814777625407,529.59755658921,-39.2297690928544)) ;
#71802 = CARTESIAN_POINT('',(209.689777625407,529.59755658921,-40.5297040214914)) ;
#71803 = CARTESIAN_POINT('Origin',(209.814777625407,533.347556589211,-38.5610190928544)) ;
#71804 = CARTESIAN_POINT('',(209.689777625407,533.347556589211,-39.2297690928544)) ;
#71805 = CARTESIAN_POINT('',(209.689777625407,533.347556589211,-38.5610190928544)) ;
#71806 = CARTESIAN_POINT('Origin',(209.814777625407,533.347556589211,-39.2297690928544)) ;
#71807 = CARTESIAN_POINT('Origin',(209.689777625407,526.868806589211,-43.1012690928544)) ;
#71808 = CARTESIAN_POINT('',(209.689777625407,529.488181589211,-39.2297690928544)) ;
#71809 = CARTESIAN_POINT('Origin',(202.466652625407,535.044431589211,-37.0052690928544)) ;
#71810 = CARTESIAN_POINT('',(208.771027625407,531.472556589211,-37.0052690928544)) ;
#71811 = CARTESIAN_POINT('Origin',(206.038527625407,531.472556589211,-37.0052690928544)) ;
#71812 = CARTESIAN_POINT('Origin',(202.262277625407,531.982556589212,-39.8669650424525)) ;
#71813 = CARTESIAN_POINT('Origin',(202.262277625407,531.982556589212,-39.4182700580611)) ;
#71814 = CARTESIAN_POINT('Origin',(212.118601772275,529.59755658921,-39.2297700580611)) ;
#71815 = CARTESIAN_POINT('',(201.559777625407,529.59755658921,-39.3547700580611)) ;
#71816 = CARTESIAN_POINT('Origin',(201.559777625407,529.59755658921,-39.2297700580612)) ;
#71817 = CARTESIAN_POINT('',(202.262277625407,529.59755658921,-39.3547700580611)) ;
#71818 = CARTESIAN_POINT('Origin',(202.262277625407,529.59755658921,-39.2297700580612)) ;
#71819 = CARTESIAN_POINT('',(212.118601772275,529.59755658921,-39.3547700580611)) ;
#71820 = CARTESIAN_POINT('Origin',(202.262277625407,532.171056589212,-39.4182700580612)) ;
#71821 = CARTESIAN_POINT('',(202.262277625407,532.171056589212,-39.3547700580612)) ;
#71822 = CARTESIAN_POINT('Origin',(202.262277625407,532.171056589212,-39.4182700580612)) ;
#71823 = CARTESIAN_POINT('Origin',(202.262277625407,532.171056589212,-39.2297700580612)) ;
#71824 = CARTESIAN_POINT('Origin',(202.262277625407,529.488181589211,-39.2297700580612)) ;
#71825 = CARTESIAN_POINT('',(202.262277625407,533.347556589211,-39.3547700580612)) ;
#71826 = CARTESIAN_POINT('Origin',(202.262277625407,533.347556589211,-39.2297700580612)) ;
#71827 = CARTESIAN_POINT('',(202.262277625407,529.488181589211,-39.3547700580611)) ;
#71828 = CARTESIAN_POINT('Origin',(201.559777625407,532.171056589212,-39.4182700580612)) ;
#71829 = CARTESIAN_POINT('',(201.559777625407,532.171056589212,-39.3547700580612)) ;
#71830 = CARTESIAN_POINT('Origin',(201.559777625407,532.171056589212,-39.4182700580612)) ;
#71831 = CARTESIAN_POINT('Origin',(201.559777625407,532.171056589212,-39.2297700580612)) ;
#71832 = CARTESIAN_POINT('Origin',(202.262277625407,530.774056589212,-39.4182700580611)) ;
#71833 = CARTESIAN_POINT('',(202.262277625407,530.837556589212,-39.4182700580611)) ;
#71834 = CARTESIAN_POINT('',(202.262277625407,530.774056589212,-39.3547700580611)) ;
#71835 = CARTESIAN_POINT('Origin',(202.262277625407,530.774056589212,-39.4182700580611)) ;
#71836 = CARTESIAN_POINT('Origin',(202.262277625407,530.774056589212,-39.2297700580612)) ;
#71837 = CARTESIAN_POINT('Origin',(202.262277625407,530.962556589212,-39.4182700580611)) ;
#71838 = CARTESIAN_POINT('Origin',(202.262277625407,530.962556589212,-37.6444650424525)) ;
#71839 = CARTESIAN_POINT('',(202.262277625407,530.837556589212,-37.6444650424525)) ;
#71840 = CARTESIAN_POINT('Origin',(202.262277625407,529.488181589211,-39.2297700580612)) ;
#71841 = CARTESIAN_POINT('Origin',(202.262277625407,529.59755658921,-39.2297700580612)) ;
#71842 = CARTESIAN_POINT('',(202.262277625407,529.488181589211,-39.3547700580611)) ;
#71843 = CARTESIAN_POINT('Origin',(201.559777625407,530.774056589212,-39.4182700580611)) ;
#71844 = CARTESIAN_POINT('',(201.559777625407,530.774056589212,-39.3547700580611)) ;
#71845 = CARTESIAN_POINT('Origin',(201.559777625407,530.774056589212,-39.4182700580611)) ;
#71846 = CARTESIAN_POINT('Origin',(201.559777625407,530.774056589212,-39.2297700580612)) ;
#71847 = CARTESIAN_POINT('Origin',(201.559777625407,529.488181589211,-39.2297700580612)) ;
#71848 = CARTESIAN_POINT('Origin',(201.559777625407,529.59755658921,-39.2297700580612)) ;
#71849 = CARTESIAN_POINT('',(201.559777625407,529.488181589211,-39.3547700580611)) ;
#71850 = CARTESIAN_POINT('Origin',(219.024277625406,530.774056589212,-39.4182700580611)) ;
#71851 = CARTESIAN_POINT('',(219.024277625406,530.774056589212,-39.3547700580611)) ;
#71852 = CARTESIAN_POINT('',(219.024277625406,530.837556589212,-39.4182700580611)) ;
#71853 = CARTESIAN_POINT('Origin',(201.559777625407,529.488181589211,-39.2297700580612)) ;
#71854 = CARTESIAN_POINT('',(201.559777625407,533.347556589211,-39.3547700580611)) ;
#71855 = CARTESIAN_POINT('Origin',(201.559777625407,533.347556589211,-39.2297700580612)) ;
#71856 = CARTESIAN_POINT('',(201.559777625407,529.488181589211,-39.3547700580611)) ;
#71857 = CARTESIAN_POINT('Origin',(218.198777625406,532.171056589212,-39.4182700580611)) ;
#71858 = CARTESIAN_POINT('',(218.198777625406,532.171056589212,-39.3547700580611)) ;
#71859 = CARTESIAN_POINT('Origin',(201.559777625407,529.59755658921,-39.2297700580612)) ;
#71860 = CARTESIAN_POINT('Origin',(202.262277625407,529.59755658921,-39.2297700580612)) ;
#71861 = CARTESIAN_POINT('Origin',(207.753027625407,533.347556589211,-39.2297700580612)) ;
#71862 = CARTESIAN_POINT('Origin',(201.559777625407,533.347556589211,-39.2297700580612)) ;
#71863 = CARTESIAN_POINT('',(207.753027625407,533.347556589211,-39.3547700580611)) ;
#71864 = CARTESIAN_POINT('Origin',(202.262277625407,533.347556589211,-39.2297700580612)) ;
#71865 = CARTESIAN_POINT('Origin',(201.559777625407,533.347556589211,-39.2297700580612)) ;
#71866 = CARTESIAN_POINT('Origin',(202.262277625407,533.347556589211,-39.2297700580612)) ;
#71867 = CARTESIAN_POINT('Origin',(219.849777625406,530.837556589212,-41.5221609920506)) ;
#71868 = CARTESIAN_POINT('Origin',(218.198777625407,532.107556589211,-39.3547700580611)) ;
#71869 = CARTESIAN_POINT('Origin',(218.198777625407,532.107556589211,-39.3547700580611)) ;
#71870 = CARTESIAN_POINT('Origin',(218.198777625407,532.107556589211,-39.3547690928544)) ;
#71871 = CARTESIAN_POINT('',(209.814777625407,533.347556589211,-39.3547690928544)) ;
#71872 = CARTESIAN_POINT('',(209.814777625407,529.59755658921,-39.3547690928544)) ;
#71873 = CARTESIAN_POINT('',(209.814777625407,529.488181589211,-39.3547690928544)) ;
#71874 = CARTESIAN_POINT('',(210.517277625407,529.59755658921,-39.3547690928544)) ;
#71875 = CARTESIAN_POINT('',(212.118601772274,529.59755658921,-39.3547690928544)) ;
#71876 = CARTESIAN_POINT('',(210.517277625407,533.347556589211,-39.3547690928544)) ;
#71877 = CARTESIAN_POINT('',(210.517277625407,529.488181589211,-39.3547690928544)) ;
#71878 = CARTESIAN_POINT('',(207.753027625407,533.347556589211,-39.3547690928544)) ;
#71879 = CARTESIAN_POINT('Origin',(209.814777625407,529.59755658921,-39.2297690928544)) ;
#71880 = CARTESIAN_POINT('Origin',(209.814777625407,529.59755658921,-39.2297690928544)) ;
#71881 = CARTESIAN_POINT('Origin',(209.814777625407,529.59755658921,-39.2297690928544)) ;
#71882 = CARTESIAN_POINT('Origin',(209.814777625407,533.347556589211,-39.2297690928544)) ;
#71883 = CARTESIAN_POINT('Origin',(209.814777625407,533.347556589211,-39.2297690928544)) ;
#71884 = CARTESIAN_POINT('Origin',(209.814777625407,533.347556589211,-39.2297690928544)) ;
#71885 = CARTESIAN_POINT('Origin',(209.814777625407,529.488181589211,-39.2297690928544)) ;
#71886 = CARTESIAN_POINT('Origin',(207.753027625407,533.347556589211,-39.2297690928544)) ;
#71887 = CARTESIAN_POINT('Origin',(210.517277625407,533.347556589211,-39.2297690928544)) ;
#71888 = CARTESIAN_POINT('Origin',(212.118601772274,529.59755658921,-39.2297690928544)) ;
#71889 = CARTESIAN_POINT('Origin',(210.517277625407,529.59755658921,-39.2297690928544)) ;
#71890 = CARTESIAN_POINT('Origin',(210.517277625407,529.488181589211,-39.2297690928544)) ;
#71891 = CARTESIAN_POINT('Origin',(210.517277625407,529.59755658921,-39.2297690928544)) ;
#71892 = CARTESIAN_POINT('Origin',(210.517277625407,533.347556589211,-39.2297690928544)) ;
#71893 = CARTESIAN_POINT('Origin',(210.517277625407,529.59755658921,-39.2297690928544)) ;
#71894 = CARTESIAN_POINT('Origin',(210.517277625407,533.347556589211,-39.2297690928544)) ;
#71895 = CARTESIAN_POINT('Origin',(202.262277625408,541.482556589212,-39.8669650424525)) ;
#71896 = CARTESIAN_POINT('Origin',(202.262277625408,541.482556589212,-39.4182700580611)) ;
#71897 = CARTESIAN_POINT('Origin',(212.118601772276,539.09755658921,-39.2297700580611)) ;
#71898 = CARTESIAN_POINT('',(201.559777625409,538.97255658921,-39.2297700580612)) ;
#71899 = CARTESIAN_POINT('',(201.559777625409,539.09755658921,-39.3547700580611)) ;
#71900 = CARTESIAN_POINT('Origin',(201.559777625409,539.09755658921,-39.2297700580612)) ;
#71901 = CARTESIAN_POINT('',(212.118601772276,538.97255658921,-39.2297700580611)) ;
#71902 = CARTESIAN_POINT('',(202.262277625408,539.09755658921,-39.3547700580611)) ;
#71903 = CARTESIAN_POINT('Origin',(202.262277625408,539.09755658921,-39.2297700580612)) ;
#71904 = CARTESIAN_POINT('',(212.118601772276,539.09755658921,-39.3547700580611)) ;
#71905 = CARTESIAN_POINT('Origin',(202.262277625408,541.671056589212,-39.4182700580612)) ;
#71906 = CARTESIAN_POINT('',(202.262277625408,541.671056589212,-39.3547700580612)) ;
#71907 = CARTESIAN_POINT('Origin',(202.262277625408,541.671056589212,-39.4182700580612)) ;
#71908 = CARTESIAN_POINT('Origin',(202.262277625408,541.671056589212,-39.2297700580612)) ;
#71909 = CARTESIAN_POINT('Origin',(202.262277625408,538.988181589211,-39.2297700580612)) ;
#71910 = CARTESIAN_POINT('',(202.262277625408,542.847556589211,-39.3547700580612)) ;
#71911 = CARTESIAN_POINT('Origin',(202.262277625408,542.847556589211,-39.2297700580612)) ;
#71912 = CARTESIAN_POINT('',(202.262277625408,538.988181589211,-39.3547700580611)) ;
#71913 = CARTESIAN_POINT('Origin',(201.559777625409,541.671056589212,-39.4182700580612)) ;
#71914 = CARTESIAN_POINT('',(201.559777625409,541.671056589212,-39.3547700580612)) ;
#71915 = CARTESIAN_POINT('Origin',(201.559777625409,541.671056589212,-39.4182700580612)) ;
#71916 = CARTESIAN_POINT('Origin',(201.559777625409,541.671056589212,-39.2297700580612)) ;
#71917 = CARTESIAN_POINT('Origin',(202.262277625408,540.274056589212,-39.4182700580611)) ;
#71918 = CARTESIAN_POINT('',(202.262277625408,540.337556589212,-39.4182700580611)) ;
#71919 = CARTESIAN_POINT('',(202.262277625408,540.274056589212,-39.3547700580611)) ;
#71920 = CARTESIAN_POINT('Origin',(202.262277625408,540.274056589212,-39.4182700580611)) ;
#71921 = CARTESIAN_POINT('Origin',(202.262277625408,540.274056589212,-39.2297700580612)) ;
#71922 = CARTESIAN_POINT('Origin',(202.262277625408,540.462556589212,-39.4182700580611)) ;
#71923 = CARTESIAN_POINT('Origin',(202.262277625408,540.462556589212,-37.6444650424525)) ;
#71924 = CARTESIAN_POINT('',(202.262277625408,540.337556589212,-37.6444650424525)) ;
#71925 = CARTESIAN_POINT('Origin',(202.262277625408,538.988181589211,-39.2297700580612)) ;
#71926 = CARTESIAN_POINT('Origin',(202.262277625408,539.09755658921,-39.2297700580612)) ;
#71927 = CARTESIAN_POINT('',(202.262277625408,538.988181589211,-39.3547700580611)) ;
#71928 = CARTESIAN_POINT('Origin',(201.559777625409,540.274056589212,-39.4182700580611)) ;
#71929 = CARTESIAN_POINT('',(201.559777625409,540.274056589212,-39.3547700580611)) ;
#71930 = CARTESIAN_POINT('Origin',(201.559777625409,540.274056589212,-39.4182700580611)) ;
#71931 = CARTESIAN_POINT('Origin',(201.559777625409,540.274056589212,-39.2297700580612)) ;
#71932 = CARTESIAN_POINT('Origin',(201.559777625409,538.988181589211,-39.2297700580612)) ;
#71933 = CARTESIAN_POINT('Origin',(201.559777625409,539.09755658921,-39.2297700580612)) ;
#71934 = CARTESIAN_POINT('',(201.559777625409,538.988181589211,-39.3547700580611)) ;
#71935 = CARTESIAN_POINT('Origin',(219.024277625408,540.274056589212,-39.4182700580611)) ;
#71936 = CARTESIAN_POINT('',(219.024277625408,540.274056589212,-39.3547700580611)) ;
#71937 = CARTESIAN_POINT('',(219.024277625408,540.337556589212,-39.4182700580611)) ;
#71938 = CARTESIAN_POINT('Origin',(201.559777625409,538.988181589211,-39.2297700580612)) ;
#71939 = CARTESIAN_POINT('',(201.559777625409,542.847556589211,-39.3547700580611)) ;
#71940 = CARTESIAN_POINT('Origin',(201.559777625409,542.847556589211,-39.2297700580612)) ;
#71941 = CARTESIAN_POINT('',(201.559777625409,538.988181589211,-39.3547700580611)) ;
#71942 = CARTESIAN_POINT('Origin',(218.198777625408,541.671056589212,-39.4182700580611)) ;
#71943 = CARTESIAN_POINT('',(218.198777625408,541.671056589212,-39.3547700580611)) ;
#71944 = CARTESIAN_POINT('Origin',(201.559777625409,539.09755658921,-39.2297700580612)) ;
#71945 = CARTESIAN_POINT('Origin',(201.559777625409,539.09755658921,-39.2297700580612)) ;
#71946 = CARTESIAN_POINT('Origin',(202.262277625408,539.09755658921,-39.2297700580612)) ;
#71947 = CARTESIAN_POINT('Origin',(207.753027625408,542.847556589211,-39.2297700580612)) ;
#71948 = CARTESIAN_POINT('Origin',(201.559777625409,542.847556589211,-39.2297700580612)) ;
#71949 = CARTESIAN_POINT('',(207.753027625408,542.847556589211,-39.3547700580611)) ;
#71950 = CARTESIAN_POINT('Origin',(202.262277625408,542.847556589211,-39.2297700580612)) ;
#71951 = CARTESIAN_POINT('Origin',(201.559777625409,542.847556589211,-39.2297700580612)) ;
#71952 = CARTESIAN_POINT('Origin',(201.559777625409,542.847556589211,-39.2297700580612)) ;
#71953 = CARTESIAN_POINT('Origin',(202.262277625408,542.847556589211,-39.2297700580612)) ;
#71954 = CARTESIAN_POINT('Origin',(219.849777625407,540.337556589212,-41.5221609920506)) ;
#71955 = CARTESIAN_POINT('Origin',(218.198777625408,541.607556589211,-39.3547700580611)) ;
#71956 = CARTESIAN_POINT('Origin',(218.198777625408,541.607556589211,-39.3547700580611)) ;
#71957 = CARTESIAN_POINT('Origin',(218.198777625408,541.607556589211,-39.3547690928544)) ;
#71958 = CARTESIAN_POINT('',(209.814777625408,542.847556589211,-39.3547690928544)) ;
#71959 = CARTESIAN_POINT('',(209.814777625408,539.09755658921,-39.3547690928544)) ;
#71960 = CARTESIAN_POINT('',(209.814777625408,538.988181589211,-39.3547690928544)) ;
#71961 = CARTESIAN_POINT('',(210.517277625409,539.09755658921,-39.3547690928544)) ;
#71962 = CARTESIAN_POINT('',(212.118601772276,539.09755658921,-39.3547690928544)) ;
#71963 = CARTESIAN_POINT('',(210.517277625409,542.847556589211,-39.3547690928544)) ;
#71964 = CARTESIAN_POINT('',(210.517277625409,538.988181589211,-39.3547690928544)) ;
#71965 = CARTESIAN_POINT('',(207.753027625408,542.847556589211,-39.3547690928544)) ;
#71966 = CARTESIAN_POINT('Origin',(209.814777625408,539.09755658921,-39.2297690928544)) ;
#71967 = CARTESIAN_POINT('',(209.814777625408,538.97255658921,-39.2297690928544)) ;
#71968 = CARTESIAN_POINT('Origin',(209.814777625408,539.09755658921,-39.2297690928544)) ;
#71969 = CARTESIAN_POINT('',(209.689777625408,539.09755658921,-39.2297690928544)) ;
#71970 = CARTESIAN_POINT('Origin',(209.814777625408,539.09755658921,-39.2297690928544)) ;
#71971 = CARTESIAN_POINT('Origin',(209.814777625408,539.09755658921,-39.2297690928544)) ;
#71972 = CARTESIAN_POINT('Origin',(209.814777625408,542.847556589211,-39.2297690928544)) ;
#71973 = CARTESIAN_POINT('',(209.689777625408,542.847556589211,-39.2297690928544)) ;
#71974 = CARTESIAN_POINT('Origin',(209.814777625408,542.847556589211,-39.2297690928544)) ;
#71975 = CARTESIAN_POINT('Origin',(209.814777625408,542.847556589211,-39.2297690928544)) ;
#71976 = CARTESIAN_POINT('Origin',(209.814777625408,542.847556589211,-39.2297690928544)) ;
#71977 = CARTESIAN_POINT('Origin',(209.814777625408,538.988181589211,-39.2297690928544)) ;
#71978 = CARTESIAN_POINT('',(209.689777625408,538.988181589211,-39.2297690928544)) ;
#71979 = CARTESIAN_POINT('Origin',(207.753027625408,542.847556589211,-39.2297690928544)) ;
#71980 = CARTESIAN_POINT('Origin',(210.517277625409,542.847556589211,-39.2297690928544)) ;
#71981 = CARTESIAN_POINT('Origin',(212.118601772276,539.09755658921,-39.2297690928544)) ;
#71982 = CARTESIAN_POINT('',(212.118601772276,538.97255658921,-39.2297690928544)) ;
#71983 = CARTESIAN_POINT('Origin',(210.517277625409,539.09755658921,-39.2297690928544)) ;
#71984 = CARTESIAN_POINT('Origin',(210.517277625409,538.988181589211,-39.2297690928544)) ;
#71985 = CARTESIAN_POINT('Origin',(210.517277625409,539.09755658921,-39.2297690928544)) ;
#71986 = CARTESIAN_POINT('Origin',(210.517277625409,542.847556589211,-39.2297690928544)) ;
#71987 = CARTESIAN_POINT('Origin',(210.517277625409,539.09755658921,-39.2297690928544)) ;
#71988 = CARTESIAN_POINT('Origin',(210.517277625409,542.847556589211,-39.2297690928544)) ;
#71989 = CARTESIAN_POINT('Origin',(202.26227762541,550.982556589212,-39.8669650424525)) ;
#71990 = CARTESIAN_POINT('Origin',(202.26227762541,550.982556589212,-39.4182700580611)) ;
#71991 = CARTESIAN_POINT('Origin',(212.118601772278,548.59755658921,-39.2297700580611)) ;
#71992 = CARTESIAN_POINT('',(201.55977762541,548.47255658921,-39.2297700580612)) ;
#71993 = CARTESIAN_POINT('',(201.55977762541,548.59755658921,-39.3547700580611)) ;
#71994 = CARTESIAN_POINT('Origin',(201.55977762541,548.59755658921,-39.2297700580612)) ;
#71995 = CARTESIAN_POINT('',(212.118601772278,548.47255658921,-39.2297700580611)) ;
#71996 = CARTESIAN_POINT('',(202.26227762541,548.59755658921,-39.3547700580611)) ;
#71997 = CARTESIAN_POINT('Origin',(202.26227762541,548.59755658921,-39.2297700580612)) ;
#71998 = CARTESIAN_POINT('',(212.118601772278,548.59755658921,-39.3547700580611)) ;
#71999 = CARTESIAN_POINT('Origin',(202.26227762541,551.171056589212,-39.4182700580612)) ;
#72000 = CARTESIAN_POINT('',(202.26227762541,551.171056589212,-39.3547700580612)) ;
#72001 = CARTESIAN_POINT('Origin',(202.26227762541,551.171056589212,-39.4182700580612)) ;
#72002 = CARTESIAN_POINT('Origin',(202.26227762541,551.171056589212,-39.2297700580612)) ;
#72003 = CARTESIAN_POINT('Origin',(202.26227762541,548.488181589211,-39.2297700580612)) ;
#72004 = CARTESIAN_POINT('',(202.26227762541,552.347556589211,-39.3547700580612)) ;
#72005 = CARTESIAN_POINT('Origin',(202.26227762541,552.347556589211,-39.2297700580612)) ;
#72006 = CARTESIAN_POINT('',(202.26227762541,548.488181589211,-39.3547700580611)) ;
#72007 = CARTESIAN_POINT('Origin',(201.55977762541,551.171056589212,-39.4182700580612)) ;
#72008 = CARTESIAN_POINT('',(201.55977762541,551.171056589212,-39.3547700580612)) ;
#72009 = CARTESIAN_POINT('Origin',(201.55977762541,551.171056589212,-39.4182700580612)) ;
#72010 = CARTESIAN_POINT('Origin',(201.55977762541,551.171056589212,-39.2297700580612)) ;
#72011 = CARTESIAN_POINT('Origin',(202.26227762541,549.774056589212,-39.4182700580611)) ;
#72012 = CARTESIAN_POINT('',(202.26227762541,549.837556589212,-39.4182700580611)) ;
#72013 = CARTESIAN_POINT('',(202.26227762541,549.774056589212,-39.3547700580611)) ;
#72014 = CARTESIAN_POINT('Origin',(202.26227762541,549.774056589212,-39.4182700580611)) ;
#72015 = CARTESIAN_POINT('Origin',(202.26227762541,549.774056589212,-39.2297700580612)) ;
#72016 = CARTESIAN_POINT('Origin',(202.26227762541,549.962556589212,-39.4182700580611)) ;
#72017 = CARTESIAN_POINT('Origin',(202.26227762541,549.962556589212,-37.6444650424525)) ;
#72018 = CARTESIAN_POINT('',(202.26227762541,549.837556589212,-37.6444650424525)) ;
#72019 = CARTESIAN_POINT('Origin',(202.26227762541,548.488181589211,-39.2297700580612)) ;
#72020 = CARTESIAN_POINT('Origin',(202.26227762541,548.59755658921,-39.2297700580612)) ;
#72021 = CARTESIAN_POINT('',(202.26227762541,548.488181589211,-39.3547700580611)) ;
#72022 = CARTESIAN_POINT('Origin',(201.55977762541,549.774056589212,-39.4182700580611)) ;
#72023 = CARTESIAN_POINT('',(201.55977762541,549.774056589212,-39.3547700580611)) ;
#72024 = CARTESIAN_POINT('Origin',(201.55977762541,549.774056589212,-39.4182700580611)) ;
#72025 = CARTESIAN_POINT('Origin',(201.55977762541,549.774056589212,-39.2297700580612)) ;
#72026 = CARTESIAN_POINT('Origin',(201.55977762541,548.488181589211,-39.2297700580612)) ;
#72027 = CARTESIAN_POINT('Origin',(201.55977762541,548.59755658921,-39.2297700580612)) ;
#72028 = CARTESIAN_POINT('',(201.55977762541,548.488181589211,-39.3547700580611)) ;
#72029 = CARTESIAN_POINT('Origin',(219.024277625409,549.774056589212,-39.4182700580611)) ;
#72030 = CARTESIAN_POINT('',(219.024277625409,549.774056589212,-39.3547700580611)) ;
#72031 = CARTESIAN_POINT('',(219.024277625409,549.837556589212,-39.4182700580611)) ;
#72032 = CARTESIAN_POINT('Origin',(201.55977762541,548.488181589211,-39.2297700580612)) ;
#72033 = CARTESIAN_POINT('',(201.55977762541,552.347556589211,-39.3547700580611)) ;
#72034 = CARTESIAN_POINT('Origin',(201.55977762541,552.347556589211,-39.2297700580612)) ;
#72035 = CARTESIAN_POINT('',(201.55977762541,548.488181589211,-39.3547700580611)) ;
#72036 = CARTESIAN_POINT('Origin',(218.198777625409,551.171056589212,-39.4182700580611)) ;
#72037 = CARTESIAN_POINT('',(218.198777625409,551.171056589212,-39.3547700580611)) ;
#72038 = CARTESIAN_POINT('Origin',(201.55977762541,548.59755658921,-39.2297700580612)) ;
#72039 = CARTESIAN_POINT('Origin',(201.55977762541,548.59755658921,-39.2297700580612)) ;
#72040 = CARTESIAN_POINT('Origin',(202.26227762541,548.59755658921,-39.2297700580612)) ;
#72041 = CARTESIAN_POINT('Origin',(207.75302762541,552.347556589211,-39.2297700580612)) ;
#72042 = CARTESIAN_POINT('Origin',(201.55977762541,552.347556589211,-39.2297700580612)) ;
#72043 = CARTESIAN_POINT('',(207.75302762541,552.347556589211,-39.3547700580611)) ;
#72044 = CARTESIAN_POINT('Origin',(202.26227762541,552.347556589211,-39.2297700580612)) ;
#72045 = CARTESIAN_POINT('Origin',(201.55977762541,552.347556589211,-39.2297700580612)) ;
#72046 = CARTESIAN_POINT('Origin',(201.55977762541,552.347556589211,-39.2297700580612)) ;
#72047 = CARTESIAN_POINT('Origin',(202.26227762541,552.347556589211,-39.2297700580612)) ;
#72048 = CARTESIAN_POINT('Origin',(219.849777625409,549.837556589212,-41.5221609920506)) ;
#72049 = CARTESIAN_POINT('Origin',(218.19877762541,551.107556589211,-39.3547700580611)) ;
#72050 = CARTESIAN_POINT('Origin',(218.19877762541,551.107556589211,-39.3547700580611)) ;
#72051 = CARTESIAN_POINT('Origin',(218.19877762541,551.107556589211,-39.3547690928544)) ;
#72052 = CARTESIAN_POINT('',(209.81477762541,552.347556589211,-39.3547690928544)) ;
#72053 = CARTESIAN_POINT('',(209.81477762541,548.59755658921,-39.3547690928544)) ;
#72054 = CARTESIAN_POINT('',(209.81477762541,548.488181589211,-39.3547690928544)) ;
#72055 = CARTESIAN_POINT('',(210.51727762541,548.59755658921,-39.3547690928544)) ;
#72056 = CARTESIAN_POINT('',(212.118601772278,548.59755658921,-39.3547690928544)) ;
#72057 = CARTESIAN_POINT('',(210.51727762541,552.347556589211,-39.3547690928544)) ;
#72058 = CARTESIAN_POINT('',(210.51727762541,548.488181589211,-39.3547690928544)) ;
#72059 = CARTESIAN_POINT('',(207.75302762541,552.347556589211,-39.3547690928544)) ;
#72060 = CARTESIAN_POINT('Origin',(209.81477762541,548.59755658921,-39.2297690928544)) ;
#72061 = CARTESIAN_POINT('',(209.81477762541,548.47255658921,-39.2297690928544)) ;
#72062 = CARTESIAN_POINT('Origin',(209.81477762541,548.59755658921,-39.2297690928544)) ;
#72063 = CARTESIAN_POINT('',(209.68977762541,548.59755658921,-39.2297690928544)) ;
#72064 = CARTESIAN_POINT('Origin',(209.81477762541,548.59755658921,-39.2297690928544)) ;
#72065 = CARTESIAN_POINT('Origin',(209.81477762541,548.59755658921,-39.2297690928544)) ;
#72066 = CARTESIAN_POINT('Origin',(209.81477762541,552.347556589211,-39.2297690928544)) ;
#72067 = CARTESIAN_POINT('',(209.68977762541,552.347556589211,-39.2297690928544)) ;
#72068 = CARTESIAN_POINT('Origin',(209.81477762541,552.347556589211,-39.2297690928544)) ;
#72069 = CARTESIAN_POINT('Origin',(209.81477762541,552.347556589211,-39.2297690928544)) ;
#72070 = CARTESIAN_POINT('Origin',(209.81477762541,552.347556589211,-39.2297690928544)) ;
#72071 = CARTESIAN_POINT('Origin',(209.81477762541,548.488181589211,-39.2297690928544)) ;
#72072 = CARTESIAN_POINT('',(209.68977762541,548.488181589211,-39.2297690928544)) ;
#72073 = CARTESIAN_POINT('Origin',(207.75302762541,552.347556589211,-39.2297690928544)) ;
#72074 = CARTESIAN_POINT('Origin',(210.51727762541,552.347556589211,-39.2297690928544)) ;
#72075 = CARTESIAN_POINT('Origin',(212.118601772278,548.59755658921,-39.2297690928544)) ;
#72076 = CARTESIAN_POINT('',(212.118601772278,548.47255658921,-39.2297690928544)) ;
#72077 = CARTESIAN_POINT('Origin',(210.51727762541,548.59755658921,-39.2297690928544)) ;
#72078 = CARTESIAN_POINT('Origin',(210.51727762541,548.488181589211,-39.2297690928544)) ;
#72079 = CARTESIAN_POINT('Origin',(210.51727762541,548.59755658921,-39.2297690928544)) ;
#72080 = CARTESIAN_POINT('Origin',(210.51727762541,552.347556589211,-39.2297690928544)) ;
#72081 = CARTESIAN_POINT('Origin',(210.51727762541,548.59755658921,-39.2297690928544)) ;
#72082 = CARTESIAN_POINT('Origin',(210.51727762541,552.347556589211,-39.2297690928544)) ;
#72083 = CARTESIAN_POINT('Origin',(202.262277625412,560.482556589212,-39.8669650424525)) ;
#72084 = CARTESIAN_POINT('Origin',(202.262277625412,560.482556589212,-39.4182700580611)) ;
#72085 = CARTESIAN_POINT('Origin',(212.118601772279,558.097556589211,-39.2297700580611)) ;
#72086 = CARTESIAN_POINT('',(201.559777625412,557.97255658921,-39.2297700580612)) ;
#72087 = CARTESIAN_POINT('',(201.559777625412,558.097556589211,-39.3547700580611)) ;
#72088 = CARTESIAN_POINT('Origin',(201.559777625412,558.097556589211,-39.2297700580612)) ;
#72089 = CARTESIAN_POINT('',(212.11860177228,557.97255658921,-39.2297700580611)) ;
#72090 = CARTESIAN_POINT('',(202.262277625412,558.09755658921,-39.3547700580611)) ;
#72091 = CARTESIAN_POINT('Origin',(202.262277625412,558.097556589211,-39.2297700580612)) ;
#72092 = CARTESIAN_POINT('',(212.118601772279,558.097556589211,-39.3547700580611)) ;
#72093 = CARTESIAN_POINT('Origin',(202.262277625412,560.671056589212,-39.4182700580612)) ;
#72094 = CARTESIAN_POINT('',(202.262277625412,560.671056589212,-39.3547700580612)) ;
#72095 = CARTESIAN_POINT('Origin',(202.262277625412,560.671056589212,-39.4182700580612)) ;
#72096 = CARTESIAN_POINT('Origin',(202.262277625412,560.671056589212,-39.2297700580612)) ;
#72097 = CARTESIAN_POINT('Origin',(202.262277625412,557.988181589211,-39.2297700580612)) ;
#72098 = CARTESIAN_POINT('',(202.262277625412,561.847556589211,-39.3547700580612)) ;
#72099 = CARTESIAN_POINT('Origin',(202.262277625412,561.847556589211,-39.2297700580612)) ;
#72100 = CARTESIAN_POINT('',(202.262277625412,557.988181589211,-39.3547700580611)) ;
#72101 = CARTESIAN_POINT('Origin',(201.559777625412,560.671056589212,-39.4182700580612)) ;
#72102 = CARTESIAN_POINT('',(201.559777625412,560.671056589212,-39.3547700580612)) ;
#72103 = CARTESIAN_POINT('Origin',(201.559777625412,560.671056589212,-39.4182700580612)) ;
#72104 = CARTESIAN_POINT('Origin',(201.559777625412,560.671056589212,-39.2297700580612)) ;
#72105 = CARTESIAN_POINT('Origin',(202.262277625412,559.274056589212,-39.4182700580611)) ;
#72106 = CARTESIAN_POINT('',(202.262277625412,559.337556589212,-39.4182700580611)) ;
#72107 = CARTESIAN_POINT('',(202.262277625412,559.274056589212,-39.3547700580611)) ;
#72108 = CARTESIAN_POINT('Origin',(202.262277625412,559.274056589212,-39.4182700580611)) ;
#72109 = CARTESIAN_POINT('Origin',(202.262277625412,559.274056589212,-39.2297700580612)) ;
#72110 = CARTESIAN_POINT('Origin',(202.262277625412,559.462556589212,-39.4182700580611)) ;
#72111 = CARTESIAN_POINT('Origin',(202.262277625412,559.462556589212,-37.6444650424525)) ;
#72112 = CARTESIAN_POINT('',(202.262277625412,559.337556589212,-37.6444650424525)) ;
#72113 = CARTESIAN_POINT('Origin',(202.262277625412,557.988181589211,-39.2297700580612)) ;
#72114 = CARTESIAN_POINT('Origin',(202.262277625412,558.09755658921,-39.2297700580612)) ;
#72115 = CARTESIAN_POINT('',(202.262277625412,557.988181589211,-39.3547700580611)) ;
#72116 = CARTESIAN_POINT('Origin',(201.559777625412,559.274056589212,-39.4182700580611)) ;
#72117 = CARTESIAN_POINT('',(201.559777625412,559.274056589212,-39.3547700580611)) ;
#72118 = CARTESIAN_POINT('Origin',(201.559777625412,559.274056589212,-39.4182700580611)) ;
#72119 = CARTESIAN_POINT('Origin',(201.559777625412,559.274056589212,-39.2297700580612)) ;
#72120 = CARTESIAN_POINT('Origin',(201.559777625412,557.988181589211,-39.2297700580612)) ;
#72121 = CARTESIAN_POINT('Origin',(201.559777625412,558.097556589211,-39.2297700580612)) ;
#72122 = CARTESIAN_POINT('',(201.559777625412,557.988181589211,-39.3547700580611)) ;
#72123 = CARTESIAN_POINT('Origin',(219.024277625411,559.274056589212,-39.4182700580611)) ;
#72124 = CARTESIAN_POINT('',(219.024277625411,559.274056589212,-39.3547700580611)) ;
#72125 = CARTESIAN_POINT('',(219.024277625411,559.337556589212,-39.4182700580611)) ;
#72126 = CARTESIAN_POINT('Origin',(201.559777625412,557.988181589211,-39.2297700580612)) ;
#72127 = CARTESIAN_POINT('',(201.559777625412,561.847556589211,-39.3547700580611)) ;
#72128 = CARTESIAN_POINT('Origin',(201.559777625412,561.847556589211,-39.2297700580612)) ;
#72129 = CARTESIAN_POINT('',(201.559777625412,557.988181589211,-39.3547700580611)) ;
#72130 = CARTESIAN_POINT('Origin',(218.198777625411,560.671056589212,-39.4182700580611)) ;
#72131 = CARTESIAN_POINT('',(218.198777625411,560.671056589212,-39.3547700580611)) ;
#72132 = CARTESIAN_POINT('Origin',(201.559777625412,558.097556589211,-39.2297700580612)) ;
#72133 = CARTESIAN_POINT('Origin',(201.559777625412,558.097556589211,-39.2297700580612)) ;
#72134 = CARTESIAN_POINT('Origin',(202.262277625412,558.09755658921,-39.2297700580612)) ;
#72135 = CARTESIAN_POINT('Origin',(207.753027625412,561.847556589211,-39.2297700580612)) ;
#72136 = CARTESIAN_POINT('Origin',(201.559777625412,561.847556589211,-39.2297700580612)) ;
#72137 = CARTESIAN_POINT('',(207.753027625412,561.847556589211,-39.3547700580611)) ;
#72138 = CARTESIAN_POINT('Origin',(202.262277625412,561.847556589211,-39.2297700580612)) ;
#72139 = CARTESIAN_POINT('Origin',(201.559777625412,561.847556589211,-39.2297700580612)) ;
#72140 = CARTESIAN_POINT('Origin',(201.559777625412,561.847556589211,-39.2297700580612)) ;
#72141 = CARTESIAN_POINT('Origin',(202.262277625412,561.847556589211,-39.2297700580612)) ;
#72142 = CARTESIAN_POINT('Origin',(219.849777625411,559.337556589212,-41.5221609920506)) ;
#72143 = CARTESIAN_POINT('Origin',(218.198777625412,560.607556589211,-39.3547700580611)) ;
#72144 = CARTESIAN_POINT('Origin',(218.198777625412,560.607556589211,-39.3547700580611)) ;
#72145 = CARTESIAN_POINT('Origin',(218.198777625412,560.607556589211,-39.3547690928544)) ;
#72146 = CARTESIAN_POINT('',(209.814777625412,561.847556589211,-39.3547690928544)) ;
#72147 = CARTESIAN_POINT('',(209.814777625412,558.097556589211,-39.3547690928544)) ;
#72148 = CARTESIAN_POINT('',(209.814777625412,557.988181589211,-39.3547690928544)) ;
#72149 = CARTESIAN_POINT('',(210.517277625412,558.097556589211,-39.3547690928544)) ;
#72150 = CARTESIAN_POINT('',(212.118601772279,558.097556589211,-39.3547690928544)) ;
#72151 = CARTESIAN_POINT('',(210.517277625412,561.847556589211,-39.3547690928544)) ;
#72152 = CARTESIAN_POINT('',(210.517277625412,557.988181589211,-39.3547690928544)) ;
#72153 = CARTESIAN_POINT('',(207.753027625412,561.847556589211,-39.3547690928544)) ;
#72154 = CARTESIAN_POINT('Origin',(209.814777625412,558.097556589211,-39.2297690928544)) ;
#72155 = CARTESIAN_POINT('',(209.814777625412,557.97255658921,-39.2297690928544)) ;
#72156 = CARTESIAN_POINT('Origin',(209.814777625412,558.097556589211,-39.2297690928544)) ;
#72157 = CARTESIAN_POINT('',(209.689777625412,558.097556589211,-39.2297690928544)) ;
#72158 = CARTESIAN_POINT('Origin',(209.814777625412,558.097556589211,-39.2297690928544)) ;
#72159 = CARTESIAN_POINT('Origin',(209.814777625412,558.097556589211,-39.2297690928544)) ;
#72160 = CARTESIAN_POINT('Origin',(209.814777625412,561.847556589211,-39.2297690928544)) ;
#72161 = CARTESIAN_POINT('',(209.689777625412,561.847556589211,-39.2297690928544)) ;
#72162 = CARTESIAN_POINT('Origin',(209.814777625412,561.847556589211,-39.2297690928544)) ;
#72163 = CARTESIAN_POINT('Origin',(209.814777625412,561.847556589211,-39.2297690928544)) ;
#72164 = CARTESIAN_POINT('Origin',(209.814777625412,561.847556589211,-39.2297690928544)) ;
#72165 = CARTESIAN_POINT('Origin',(209.814777625412,557.988181589211,-39.2297690928544)) ;
#72166 = CARTESIAN_POINT('',(209.689777625412,557.988181589211,-39.2297690928544)) ;
#72167 = CARTESIAN_POINT('Origin',(207.753027625412,561.847556589211,-39.2297690928544)) ;
#72168 = CARTESIAN_POINT('Origin',(210.517277625412,561.847556589211,-39.2297690928544)) ;
#72169 = CARTESIAN_POINT('Origin',(212.118601772279,558.097556589211,-39.2297690928544)) ;
#72170 = CARTESIAN_POINT('',(212.118601772279,557.97255658921,-39.2297690928544)) ;
#72171 = CARTESIAN_POINT('Origin',(210.517277625412,558.097556589211,-39.2297690928544)) ;
#72172 = CARTESIAN_POINT('Origin',(210.517277625412,557.988181589211,-39.2297690928544)) ;
#72173 = CARTESIAN_POINT('Origin',(210.517277625412,558.097556589211,-39.2297690928544)) ;
#72174 = CARTESIAN_POINT('Origin',(210.517277625412,561.847556589211,-39.2297690928544)) ;
#72175 = CARTESIAN_POINT('Origin',(210.517277625412,558.097556589211,-39.2297690928544)) ;
#72176 = CARTESIAN_POINT('Origin',(210.517277625412,561.847556589211,-39.2297690928544)) ;
#72177 = CARTESIAN_POINT('Origin',(202.262277625413,569.982556589212,-39.8669650424525)) ;
#72178 = CARTESIAN_POINT('Origin',(202.262277625413,569.982556589212,-39.4182700580611)) ;
#72179 = CARTESIAN_POINT('Origin',(212.118601772281,567.59755658921,-39.2297700580611)) ;
#72180 = CARTESIAN_POINT('',(201.559777625414,567.47255658921,-39.2297700580612)) ;
#72181 = CARTESIAN_POINT('',(201.559777625414,567.59755658921,-39.3547700580611)) ;
#72182 = CARTESIAN_POINT('Origin',(201.559777625414,567.59755658921,-39.2297700580612)) ;
#72183 = CARTESIAN_POINT('',(212.118601772281,567.47255658921,-39.2297700580611)) ;
#72184 = CARTESIAN_POINT('',(202.262277625413,567.59755658921,-39.3547700580611)) ;
#72185 = CARTESIAN_POINT('Origin',(202.262277625413,567.59755658921,-39.2297700580612)) ;
#72186 = CARTESIAN_POINT('',(212.118601772281,567.59755658921,-39.3547700580611)) ;
#72187 = CARTESIAN_POINT('Origin',(202.262277625413,570.171056589212,-39.4182700580612)) ;
#72188 = CARTESIAN_POINT('',(202.262277625413,570.171056589212,-39.3547700580612)) ;
#72189 = CARTESIAN_POINT('Origin',(202.262277625413,570.171056589212,-39.4182700580612)) ;
#72190 = CARTESIAN_POINT('Origin',(202.262277625413,570.171056589212,-39.2297700580612)) ;
#72191 = CARTESIAN_POINT('Origin',(202.262277625413,567.488181589211,-39.2297700580612)) ;
#72192 = CARTESIAN_POINT('',(202.262277625413,571.347556589211,-39.3547700580612)) ;
#72193 = CARTESIAN_POINT('Origin',(202.262277625413,571.347556589211,-39.2297700580612)) ;
#72194 = CARTESIAN_POINT('',(202.262277625413,567.488181589211,-39.3547700580611)) ;
#72195 = CARTESIAN_POINT('Origin',(201.559777625414,570.171056589212,-39.4182700580612)) ;
#72196 = CARTESIAN_POINT('',(201.559777625414,570.171056589212,-39.3547700580612)) ;
#72197 = CARTESIAN_POINT('Origin',(201.559777625414,570.171056589212,-39.4182700580612)) ;
#72198 = CARTESIAN_POINT('Origin',(201.559777625414,570.171056589212,-39.2297700580612)) ;
#72199 = CARTESIAN_POINT('Origin',(202.262277625413,568.774056589212,-39.4182700580611)) ;
#72200 = CARTESIAN_POINT('',(202.262277625413,568.837556589212,-39.4182700580611)) ;
#72201 = CARTESIAN_POINT('',(202.262277625413,568.774056589212,-39.3547700580611)) ;
#72202 = CARTESIAN_POINT('Origin',(202.262277625413,568.774056589212,-39.4182700580611)) ;
#72203 = CARTESIAN_POINT('Origin',(202.262277625413,568.774056589212,-39.2297700580612)) ;
#72204 = CARTESIAN_POINT('Origin',(202.262277625413,568.962556589212,-39.4182700580611)) ;
#72205 = CARTESIAN_POINT('Origin',(202.262277625413,568.962556589212,-37.6444650424525)) ;
#72206 = CARTESIAN_POINT('',(202.262277625413,568.837556589212,-37.6444650424525)) ;
#72207 = CARTESIAN_POINT('Origin',(202.262277625413,567.488181589211,-39.2297700580612)) ;
#72208 = CARTESIAN_POINT('Origin',(202.262277625413,567.59755658921,-39.2297700580612)) ;
#72209 = CARTESIAN_POINT('',(202.262277625413,567.488181589211,-39.3547700580611)) ;
#72210 = CARTESIAN_POINT('Origin',(201.559777625414,568.774056589212,-39.4182700580611)) ;
#72211 = CARTESIAN_POINT('',(201.559777625414,568.774056589212,-39.3547700580611)) ;
#72212 = CARTESIAN_POINT('Origin',(201.559777625414,568.774056589212,-39.4182700580611)) ;
#72213 = CARTESIAN_POINT('Origin',(201.559777625414,568.774056589212,-39.2297700580612)) ;
#72214 = CARTESIAN_POINT('Origin',(201.559777625414,567.488181589211,-39.2297700580612)) ;
#72215 = CARTESIAN_POINT('Origin',(201.559777625414,567.59755658921,-39.2297700580612)) ;
#72216 = CARTESIAN_POINT('',(201.559777625414,567.488181589211,-39.3547700580611)) ;
#72217 = CARTESIAN_POINT('Origin',(219.024277625413,568.774056589212,-39.4182700580611)) ;
#72218 = CARTESIAN_POINT('',(219.024277625413,568.774056589212,-39.3547700580611)) ;
#72219 = CARTESIAN_POINT('',(219.024277625413,568.837556589212,-39.4182700580611)) ;
#72220 = CARTESIAN_POINT('Origin',(201.559777625414,567.488181589211,-39.2297700580612)) ;
#72221 = CARTESIAN_POINT('',(201.559777625414,571.347556589211,-39.3547700580611)) ;
#72222 = CARTESIAN_POINT('Origin',(201.559777625414,571.347556589211,-39.2297700580612)) ;
#72223 = CARTESIAN_POINT('',(201.559777625414,567.488181589211,-39.3547700580611)) ;
#72224 = CARTESIAN_POINT('Origin',(218.198777625413,570.171056589212,-39.4182700580611)) ;
#72225 = CARTESIAN_POINT('',(218.198777625413,570.171056589212,-39.3547700580611)) ;
#72226 = CARTESIAN_POINT('Origin',(201.559777625414,567.59755658921,-39.2297700580612)) ;
#72227 = CARTESIAN_POINT('Origin',(201.559777625414,567.59755658921,-39.2297700580612)) ;
#72228 = CARTESIAN_POINT('Origin',(202.262277625413,567.59755658921,-39.2297700580612)) ;
#72229 = CARTESIAN_POINT('Origin',(207.753027625413,571.347556589211,-39.2297700580612)) ;
#72230 = CARTESIAN_POINT('Origin',(201.559777625414,571.347556589211,-39.2297700580612)) ;
#72231 = CARTESIAN_POINT('',(207.753027625413,571.347556589211,-39.3547700580611)) ;
#72232 = CARTESIAN_POINT('Origin',(202.262277625413,571.347556589211,-39.2297700580612)) ;
#72233 = CARTESIAN_POINT('Origin',(201.559777625414,571.347556589211,-39.2297700580612)) ;
#72234 = CARTESIAN_POINT('Origin',(201.559777625414,571.347556589211,-39.2297700580612)) ;
#72235 = CARTESIAN_POINT('Origin',(202.262277625413,571.347556589211,-39.2297700580612)) ;
#72236 = CARTESIAN_POINT('Origin',(219.849777625412,568.837556589212,-41.5221609920506)) ;
#72237 = CARTESIAN_POINT('Origin',(218.198777625413,570.107556589211,-39.3547700580611)) ;
#72238 = CARTESIAN_POINT('Origin',(218.198777625413,570.107556589211,-39.3547700580611)) ;
#72239 = CARTESIAN_POINT('Origin',(218.198777625413,570.107556589211,-39.3547690928544)) ;
#72240 = CARTESIAN_POINT('',(209.814777625413,571.347556589211,-39.3547690928544)) ;
#72241 = CARTESIAN_POINT('',(209.814777625413,567.59755658921,-39.3547690928544)) ;
#72242 = CARTESIAN_POINT('',(209.814777625413,567.488181589211,-39.3547690928544)) ;
#72243 = CARTESIAN_POINT('',(210.517277625414,567.59755658921,-39.3547690928544)) ;
#72244 = CARTESIAN_POINT('',(212.118601772281,567.59755658921,-39.3547690928544)) ;
#72245 = CARTESIAN_POINT('',(210.517277625414,571.347556589211,-39.3547690928544)) ;
#72246 = CARTESIAN_POINT('',(210.517277625414,567.488181589211,-39.3547690928544)) ;
#72247 = CARTESIAN_POINT('',(207.753027625413,571.347556589211,-39.3547690928544)) ;
#72248 = CARTESIAN_POINT('Origin',(209.814777625413,567.59755658921,-39.2297690928544)) ;
#72249 = CARTESIAN_POINT('',(209.814777625413,567.47255658921,-39.2297690928544)) ;
#72250 = CARTESIAN_POINT('Origin',(209.814777625413,567.59755658921,-39.2297690928544)) ;
#72251 = CARTESIAN_POINT('',(209.689777625413,567.59755658921,-39.2297690928544)) ;
#72252 = CARTESIAN_POINT('Origin',(209.814777625413,567.59755658921,-39.2297690928544)) ;
#72253 = CARTESIAN_POINT('Origin',(209.814777625413,567.59755658921,-39.2297690928544)) ;
#72254 = CARTESIAN_POINT('Origin',(209.814777625413,571.347556589211,-39.2297690928544)) ;
#72255 = CARTESIAN_POINT('',(209.689777625413,571.347556589211,-39.2297690928544)) ;
#72256 = CARTESIAN_POINT('Origin',(209.814777625413,571.347556589211,-39.2297690928544)) ;
#72257 = CARTESIAN_POINT('Origin',(209.814777625413,571.347556589211,-39.2297690928544)) ;
#72258 = CARTESIAN_POINT('Origin',(209.814777625413,571.347556589211,-39.2297690928544)) ;
#72259 = CARTESIAN_POINT('Origin',(209.814777625413,567.488181589211,-39.2297690928544)) ;
#72260 = CARTESIAN_POINT('',(209.689777625413,567.488181589211,-39.2297690928544)) ;
#72261 = CARTESIAN_POINT('Origin',(207.753027625413,571.347556589211,-39.2297690928544)) ;
#72262 = CARTESIAN_POINT('Origin',(210.517277625414,571.347556589211,-39.2297690928544)) ;
#72263 = CARTESIAN_POINT('Origin',(212.118601772281,567.59755658921,-39.2297690928544)) ;
#72264 = CARTESIAN_POINT('',(212.118601772281,567.47255658921,-39.2297690928544)) ;
#72265 = CARTESIAN_POINT('Origin',(210.517277625414,567.59755658921,-39.2297690928544)) ;
#72266 = CARTESIAN_POINT('Origin',(210.517277625414,567.488181589211,-39.2297690928544)) ;
#72267 = CARTESIAN_POINT('Origin',(210.517277625414,567.59755658921,-39.2297690928544)) ;
#72268 = CARTESIAN_POINT('Origin',(210.517277625414,571.347556589211,-39.2297690928544)) ;
#72269 = CARTESIAN_POINT('Origin',(210.517277625414,567.59755658921,-39.2297690928544)) ;
#72270 = CARTESIAN_POINT('Origin',(210.517277625414,571.347556589211,-39.2297690928544)) ;
#72271 = CARTESIAN_POINT('Origin',(202.262277625415,579.482556589212,-39.8669650424525)) ;
#72272 = CARTESIAN_POINT('Origin',(202.262277625415,579.482556589212,-39.4182700580611)) ;
#72273 = CARTESIAN_POINT('Origin',(212.118601772283,577.097556589211,-39.2297700580611)) ;
#72274 = CARTESIAN_POINT('',(201.559777625416,576.972556589211,-39.2297700580612)) ;
#72275 = CARTESIAN_POINT('',(201.559777625415,577.097556589211,-39.3547700580611)) ;
#72276 = CARTESIAN_POINT('Origin',(201.559777625415,577.097556589211,-39.2297700580612)) ;
#72277 = CARTESIAN_POINT('',(212.118601772283,576.972556589211,-39.2297700580611)) ;
#72278 = CARTESIAN_POINT('',(202.262277625415,577.097556589211,-39.3547700580611)) ;
#72279 = CARTESIAN_POINT('Origin',(202.262277625415,577.097556589211,-39.2297700580612)) ;
#72280 = CARTESIAN_POINT('',(212.118601772283,577.097556589211,-39.3547700580611)) ;
#72281 = CARTESIAN_POINT('Origin',(202.262277625415,579.671056589212,-39.4182700580612)) ;
#72282 = CARTESIAN_POINT('',(202.262277625415,579.671056589212,-39.3547700580612)) ;
#72283 = CARTESIAN_POINT('Origin',(202.262277625415,579.671056589212,-39.4182700580612)) ;
#72284 = CARTESIAN_POINT('Origin',(202.262277625415,579.671056589212,-39.2297700580612)) ;
#72285 = CARTESIAN_POINT('Origin',(202.262277625415,576.988181589211,-39.2297700580612)) ;
#72286 = CARTESIAN_POINT('',(202.262277625415,580.847556589211,-39.3547700580612)) ;
#72287 = CARTESIAN_POINT('Origin',(202.262277625415,580.847556589211,-39.2297700580612)) ;
#72288 = CARTESIAN_POINT('',(202.262277625415,576.988181589211,-39.3547700580611)) ;
#72289 = CARTESIAN_POINT('Origin',(201.559777625415,579.671056589212,-39.4182700580612)) ;
#72290 = CARTESIAN_POINT('',(201.559777625415,579.671056589212,-39.3547700580612)) ;
#72291 = CARTESIAN_POINT('Origin',(201.559777625415,579.671056589212,-39.4182700580612)) ;
#72292 = CARTESIAN_POINT('Origin',(201.559777625415,579.671056589212,-39.2297700580612)) ;
#72293 = CARTESIAN_POINT('Origin',(202.262277625415,578.274056589212,-39.4182700580611)) ;
#72294 = CARTESIAN_POINT('',(202.262277625415,578.337556589212,-39.4182700580611)) ;
#72295 = CARTESIAN_POINT('',(202.262277625415,578.274056589212,-39.3547700580611)) ;
#72296 = CARTESIAN_POINT('Origin',(202.262277625415,578.274056589212,-39.4182700580611)) ;
#72297 = CARTESIAN_POINT('Origin',(202.262277625415,578.274056589212,-39.2297700580612)) ;
#72298 = CARTESIAN_POINT('Origin',(202.262277625415,578.462556589212,-39.4182700580611)) ;
#72299 = CARTESIAN_POINT('Origin',(202.262277625415,578.462556589212,-37.6444650424525)) ;
#72300 = CARTESIAN_POINT('',(202.262277625415,578.337556589212,-37.6444650424525)) ;
#72301 = CARTESIAN_POINT('Origin',(202.262277625415,576.988181589211,-39.2297700580612)) ;
#72302 = CARTESIAN_POINT('Origin',(202.262277625415,577.097556589211,-39.2297700580612)) ;
#72303 = CARTESIAN_POINT('',(202.262277625415,576.988181589211,-39.3547700580611)) ;
#72304 = CARTESIAN_POINT('Origin',(201.559777625415,578.274056589212,-39.4182700580611)) ;
#72305 = CARTESIAN_POINT('',(201.559777625415,578.274056589212,-39.3547700580611)) ;
#72306 = CARTESIAN_POINT('Origin',(201.559777625415,578.274056589212,-39.4182700580611)) ;
#72307 = CARTESIAN_POINT('Origin',(201.559777625415,578.274056589212,-39.2297700580612)) ;
#72308 = CARTESIAN_POINT('Origin',(201.559777625415,576.988181589211,-39.2297700580612)) ;
#72309 = CARTESIAN_POINT('Origin',(201.559777625415,577.097556589211,-39.2297700580612)) ;
#72310 = CARTESIAN_POINT('',(201.559777625415,576.988181589211,-39.3547700580611)) ;
#72311 = CARTESIAN_POINT('Origin',(219.024277625414,578.274056589212,-39.4182700580611)) ;
#72312 = CARTESIAN_POINT('',(219.024277625414,578.274056589212,-39.3547700580611)) ;
#72313 = CARTESIAN_POINT('',(219.024277625414,578.337556589212,-39.4182700580611)) ;
#72314 = CARTESIAN_POINT('Origin',(201.559777625415,576.988181589211,-39.2297700580612)) ;
#72315 = CARTESIAN_POINT('',(201.559777625415,580.847556589211,-39.3547700580611)) ;
#72316 = CARTESIAN_POINT('Origin',(201.559777625415,580.847556589211,-39.2297700580612)) ;
#72317 = CARTESIAN_POINT('',(201.559777625415,576.988181589211,-39.3547700580611)) ;
#72318 = CARTESIAN_POINT('Origin',(218.198777625414,579.671056589212,-39.4182700580611)) ;
#72319 = CARTESIAN_POINT('',(218.198777625414,579.671056589212,-39.3547700580611)) ;
#72320 = CARTESIAN_POINT('Origin',(201.559777625415,577.097556589211,-39.2297700580612)) ;
#72321 = CARTESIAN_POINT('Origin',(201.559777625415,577.097556589211,-39.2297700580612)) ;
#72322 = CARTESIAN_POINT('Origin',(202.262277625415,577.097556589211,-39.2297700580612)) ;
#72323 = CARTESIAN_POINT('Origin',(207.753027625415,580.847556589211,-39.2297700580612)) ;
#72324 = CARTESIAN_POINT('Origin',(201.559777625415,580.847556589211,-39.2297700580612)) ;
#72325 = CARTESIAN_POINT('',(207.753027625415,580.847556589211,-39.3547700580611)) ;
#72326 = CARTESIAN_POINT('Origin',(202.262277625415,580.847556589211,-39.2297700580612)) ;
#72327 = CARTESIAN_POINT('Origin',(201.559777625415,580.847556589211,-39.2297700580612)) ;
#72328 = CARTESIAN_POINT('Origin',(201.559777625415,580.847556589211,-39.2297700580612)) ;
#72329 = CARTESIAN_POINT('Origin',(202.262277625415,580.847556589211,-39.2297700580612)) ;
#72330 = CARTESIAN_POINT('Origin',(219.849777625414,578.337556589212,-41.5221609920506)) ;
#72331 = CARTESIAN_POINT('Origin',(218.198777625415,579.607556589211,-39.3547700580611)) ;
#72332 = CARTESIAN_POINT('Origin',(218.198777625415,579.607556589211,-39.3547700580611)) ;
#72333 = CARTESIAN_POINT('Origin',(218.198777625415,579.607556589211,-39.3547690928544)) ;
#72334 = CARTESIAN_POINT('',(209.814777625415,580.847556589211,-39.3547690928544)) ;
#72335 = CARTESIAN_POINT('',(209.814777625415,577.097556589211,-39.3547690928544)) ;
#72336 = CARTESIAN_POINT('',(209.814777625415,576.988181589211,-39.3547690928544)) ;
#72337 = CARTESIAN_POINT('',(210.517277625416,577.097556589211,-39.3547690928544)) ;
#72338 = CARTESIAN_POINT('',(212.118601772283,577.097556589211,-39.3547690928544)) ;
#72339 = CARTESIAN_POINT('',(210.517277625416,580.847556589211,-39.3547690928544)) ;
#72340 = CARTESIAN_POINT('',(210.517277625416,576.988181589211,-39.3547690928544)) ;
#72341 = CARTESIAN_POINT('',(207.753027625415,580.847556589211,-39.3547690928544)) ;
#72342 = CARTESIAN_POINT('Origin',(209.814777625415,577.097556589211,-39.2297690928544)) ;
#72343 = CARTESIAN_POINT('',(209.814777625415,576.972556589211,-39.2297690928544)) ;
#72344 = CARTESIAN_POINT('Origin',(209.814777625415,577.097556589211,-39.2297690928544)) ;
#72345 = CARTESIAN_POINT('',(209.689777625415,577.097556589211,-39.2297690928544)) ;
#72346 = CARTESIAN_POINT('Origin',(209.814777625415,577.097556589211,-39.2297690928544)) ;
#72347 = CARTESIAN_POINT('Origin',(209.814777625415,577.097556589211,-39.2297690928544)) ;
#72348 = CARTESIAN_POINT('Origin',(209.814777625415,580.847556589211,-39.2297690928544)) ;
#72349 = CARTESIAN_POINT('',(209.689777625415,580.847556589211,-39.2297690928544)) ;
#72350 = CARTESIAN_POINT('Origin',(209.814777625415,580.847556589211,-39.2297690928544)) ;
#72351 = CARTESIAN_POINT('Origin',(209.814777625415,580.847556589211,-39.2297690928544)) ;
#72352 = CARTESIAN_POINT('Origin',(209.814777625415,580.847556589211,-39.2297690928544)) ;
#72353 = CARTESIAN_POINT('Origin',(209.814777625415,576.988181589211,-39.2297690928544)) ;
#72354 = CARTESIAN_POINT('',(209.689777625415,576.988181589211,-39.2297690928544)) ;
#72355 = CARTESIAN_POINT('Origin',(207.753027625415,580.847556589211,-39.2297690928544)) ;
#72356 = CARTESIAN_POINT('Origin',(210.517277625416,580.847556589211,-39.2297690928544)) ;
#72357 = CARTESIAN_POINT('Origin',(212.118601772283,577.097556589211,-39.2297690928544)) ;
#72358 = CARTESIAN_POINT('',(212.118601772283,576.972556589211,-39.2297690928544)) ;
#72359 = CARTESIAN_POINT('Origin',(210.517277625416,577.097556589211,-39.2297690928544)) ;
#72360 = CARTESIAN_POINT('Origin',(210.517277625416,576.988181589211,-39.2297690928544)) ;
#72361 = CARTESIAN_POINT('Origin',(210.517277625416,577.097556589211,-39.2297690928544)) ;
#72362 = CARTESIAN_POINT('Origin',(210.517277625416,580.847556589211,-39.2297690928544)) ;
#72363 = CARTESIAN_POINT('Origin',(210.517277625416,577.097556589211,-39.2297690928544)) ;
#72364 = CARTESIAN_POINT('Origin',(210.517277625416,580.847556589211,-39.2297690928544)) ;
#72365 = CARTESIAN_POINT('Origin',(202.262277625416,588.982556589212,-39.8669650424525)) ;
#72366 = CARTESIAN_POINT('Origin',(202.262277625416,588.982556589212,-39.4182700580611)) ;
#72367 = CARTESIAN_POINT('Origin',(212.118601772284,586.597556589211,-39.2297700580611)) ;
#72368 = CARTESIAN_POINT('',(201.559777625417,586.472556589211,-39.2297700580612)) ;
#72369 = CARTESIAN_POINT('',(201.559777625417,586.597556589211,-39.3547700580611)) ;
#72370 = CARTESIAN_POINT('Origin',(201.559777625417,586.597556589211,-39.2297700580612)) ;
#72371 = CARTESIAN_POINT('',(212.118601772284,586.472556589211,-39.2297700580611)) ;
#72372 = CARTESIAN_POINT('',(202.262277625417,586.597556589211,-39.3547700580611)) ;
#72373 = CARTESIAN_POINT('Origin',(202.262277625417,586.597556589211,-39.2297700580612)) ;
#72374 = CARTESIAN_POINT('',(212.118601772284,586.597556589211,-39.3547700580611)) ;
#72375 = CARTESIAN_POINT('Origin',(202.262277625416,589.171056589212,-39.4182700580612)) ;
#72376 = CARTESIAN_POINT('',(202.262277625417,589.171056589212,-39.3547700580612)) ;
#72377 = CARTESIAN_POINT('Origin',(202.262277625417,589.171056589212,-39.4182700580612)) ;
#72378 = CARTESIAN_POINT('Origin',(202.262277625417,589.171056589212,-39.2297700580612)) ;
#72379 = CARTESIAN_POINT('Origin',(202.262277625417,586.488181589211,-39.2297700580612)) ;
#72380 = CARTESIAN_POINT('',(202.262277625417,590.347556589211,-39.3547700580612)) ;
#72381 = CARTESIAN_POINT('Origin',(202.262277625417,590.347556589211,-39.2297700580612)) ;
#72382 = CARTESIAN_POINT('',(202.262277625417,586.488181589211,-39.3547700580611)) ;
#72383 = CARTESIAN_POINT('Origin',(201.559777625417,589.171056589212,-39.4182700580612)) ;
#72384 = CARTESIAN_POINT('',(201.559777625417,589.171056589212,-39.3547700580612)) ;
#72385 = CARTESIAN_POINT('Origin',(201.559777625417,589.171056589212,-39.4182700580612)) ;
#72386 = CARTESIAN_POINT('Origin',(201.559777625417,589.171056589212,-39.2297700580612)) ;
#72387 = CARTESIAN_POINT('Origin',(202.262277625417,587.774056589212,-39.4182700580611)) ;
#72388 = CARTESIAN_POINT('',(202.262277625417,587.837556589212,-39.4182700580611)) ;
#72389 = CARTESIAN_POINT('',(202.262277625417,587.774056589212,-39.3547700580611)) ;
#72390 = CARTESIAN_POINT('Origin',(202.262277625417,587.774056589212,-39.4182700580611)) ;
#72391 = CARTESIAN_POINT('Origin',(202.262277625417,587.774056589212,-39.2297700580612)) ;
#72392 = CARTESIAN_POINT('Origin',(202.262277625417,587.962556589212,-39.4182700580611)) ;
#72393 = CARTESIAN_POINT('Origin',(202.262277625417,587.962556589212,-37.6444650424525)) ;
#72394 = CARTESIAN_POINT('',(202.262277625417,587.837556589212,-37.6444650424525)) ;
#72395 = CARTESIAN_POINT('Origin',(202.262277625417,586.488181589211,-39.2297700580612)) ;
#72396 = CARTESIAN_POINT('Origin',(202.262277625417,586.597556589211,-39.2297700580612)) ;
#72397 = CARTESIAN_POINT('',(202.262277625417,586.488181589211,-39.3547700580611)) ;
#72398 = CARTESIAN_POINT('Origin',(201.559777625417,587.774056589212,-39.4182700580611)) ;
#72399 = CARTESIAN_POINT('',(201.559777625417,587.774056589212,-39.3547700580611)) ;
#72400 = CARTESIAN_POINT('Origin',(201.559777625417,587.774056589212,-39.4182700580611)) ;
#72401 = CARTESIAN_POINT('Origin',(201.559777625417,587.774056589212,-39.2297700580612)) ;
#72402 = CARTESIAN_POINT('Origin',(201.559777625417,586.488181589211,-39.2297700580612)) ;
#72403 = CARTESIAN_POINT('Origin',(201.559777625417,586.597556589211,-39.2297700580612)) ;
#72404 = CARTESIAN_POINT('',(201.559777625417,586.488181589211,-39.3547700580611)) ;
#72405 = CARTESIAN_POINT('Origin',(219.024277625416,587.774056589212,-39.4182700580611)) ;
#72406 = CARTESIAN_POINT('',(219.024277625416,587.774056589212,-39.3547700580611)) ;
#72407 = CARTESIAN_POINT('',(219.024277625416,587.837556589212,-39.4182700580611)) ;
#72408 = CARTESIAN_POINT('Origin',(201.559777625417,586.488181589211,-39.2297700580612)) ;
#72409 = CARTESIAN_POINT('',(201.559777625417,590.347556589211,-39.3547700580611)) ;
#72410 = CARTESIAN_POINT('Origin',(201.559777625417,590.347556589211,-39.2297700580612)) ;
#72411 = CARTESIAN_POINT('',(201.559777625417,586.488181589211,-39.3547700580611)) ;
#72412 = CARTESIAN_POINT('Origin',(218.198777625416,589.171056589212,-39.4182700580611)) ;
#72413 = CARTESIAN_POINT('',(218.198777625416,589.171056589212,-39.3547700580611)) ;
#72414 = CARTESIAN_POINT('Origin',(201.559777625417,586.597556589211,-39.2297700580612)) ;
#72415 = CARTESIAN_POINT('Origin',(201.559777625417,586.597556589211,-39.2297700580612)) ;
#72416 = CARTESIAN_POINT('Origin',(202.262277625417,586.597556589211,-39.2297700580612)) ;
#72417 = CARTESIAN_POINT('Origin',(207.753027625417,590.347556589211,-39.2297700580612)) ;
#72418 = CARTESIAN_POINT('Origin',(201.559777625417,590.347556589211,-39.2297700580612)) ;
#72419 = CARTESIAN_POINT('',(207.753027625417,590.347556589211,-39.3547700580611)) ;
#72420 = CARTESIAN_POINT('Origin',(202.262277625417,590.347556589211,-39.2297700580612)) ;
#72421 = CARTESIAN_POINT('Origin',(201.559777625417,590.347556589211,-39.2297700580612)) ;
#72422 = CARTESIAN_POINT('Origin',(201.559777625417,590.347556589211,-39.2297700580612)) ;
#72423 = CARTESIAN_POINT('Origin',(202.262277625417,590.347556589211,-39.2297700580612)) ;
#72424 = CARTESIAN_POINT('Origin',(219.849777625416,587.837556589212,-41.5221609920506)) ;
#72425 = CARTESIAN_POINT('Origin',(218.198777625417,589.107556589211,-39.3547700580611)) ;
#72426 = CARTESIAN_POINT('Origin',(218.198777625417,589.107556589211,-39.3547700580611)) ;
#72427 = CARTESIAN_POINT('Origin',(218.198777625417,589.107556589211,-39.3547690928544)) ;
#72428 = CARTESIAN_POINT('',(209.814777625417,590.347556589211,-39.3547690928544)) ;
#72429 = CARTESIAN_POINT('',(209.814777625417,586.597556589211,-39.3547690928544)) ;
#72430 = CARTESIAN_POINT('',(209.814777625417,586.488181589211,-39.3547690928544)) ;
#72431 = CARTESIAN_POINT('',(210.517277625417,586.597556589211,-39.3547690928544)) ;
#72432 = CARTESIAN_POINT('',(212.118601772284,586.597556589211,-39.3547690928544)) ;
#72433 = CARTESIAN_POINT('',(210.517277625417,590.347556589211,-39.3547690928544)) ;
#72434 = CARTESIAN_POINT('',(210.517277625417,586.488181589211,-39.3547690928544)) ;
#72435 = CARTESIAN_POINT('',(207.753027625417,590.347556589211,-39.3547690928544)) ;
#72436 = CARTESIAN_POINT('Origin',(209.814777625417,586.597556589211,-39.2297690928544)) ;
#72437 = CARTESIAN_POINT('',(209.814777625417,586.472556589211,-39.2297690928544)) ;
#72438 = CARTESIAN_POINT('Origin',(209.814777625417,586.597556589211,-39.2297690928544)) ;
#72439 = CARTESIAN_POINT('',(209.689777625417,586.597556589211,-39.2297690928544)) ;
#72440 = CARTESIAN_POINT('Origin',(209.814777625417,586.597556589211,-39.2297690928544)) ;
#72441 = CARTESIAN_POINT('Origin',(209.814777625417,586.597556589211,-39.2297690928544)) ;
#72442 = CARTESIAN_POINT('Origin',(209.814777625417,590.347556589211,-39.2297690928544)) ;
#72443 = CARTESIAN_POINT('',(209.689777625417,590.347556589211,-39.2297690928544)) ;
#72444 = CARTESIAN_POINT('Origin',(209.814777625417,590.347556589211,-39.2297690928544)) ;
#72445 = CARTESIAN_POINT('Origin',(209.814777625417,590.347556589211,-39.2297690928544)) ;
#72446 = CARTESIAN_POINT('Origin',(209.814777625417,590.347556589211,-39.2297690928544)) ;
#72447 = CARTESIAN_POINT('Origin',(209.814777625417,586.488181589211,-39.2297690928544)) ;
#72448 = CARTESIAN_POINT('',(209.689777625417,586.488181589211,-39.2297690928544)) ;
#72449 = CARTESIAN_POINT('Origin',(207.753027625417,590.347556589211,-39.2297690928544)) ;
#72450 = CARTESIAN_POINT('Origin',(210.517277625417,590.347556589211,-39.2297690928544)) ;
#72451 = CARTESIAN_POINT('Origin',(212.118601772284,586.597556589211,-39.2297690928544)) ;
#72452 = CARTESIAN_POINT('',(212.118601772284,586.472556589211,-39.2297690928544)) ;
#72453 = CARTESIAN_POINT('Origin',(210.517277625417,586.597556589211,-39.2297690928544)) ;
#72454 = CARTESIAN_POINT('Origin',(210.517277625417,586.488181589211,-39.2297690928544)) ;
#72455 = CARTESIAN_POINT('Origin',(210.517277625417,586.597556589211,-39.2297690928544)) ;
#72456 = CARTESIAN_POINT('Origin',(210.517277625417,590.347556589211,-39.2297690928544)) ;
#72457 = CARTESIAN_POINT('Origin',(210.517277625417,586.597556589211,-39.2297690928544)) ;
#72458 = CARTESIAN_POINT('Origin',(210.517277625417,590.347556589211,-39.2297690928544)) ;
#72459 = CARTESIAN_POINT('Origin',(202.262277625418,598.482556589212,-39.8669650424525)) ;
#72460 = CARTESIAN_POINT('Origin',(202.262277625418,598.482556589212,-39.4182700580611)) ;
#72461 = CARTESIAN_POINT('Origin',(212.118601772286,596.097556589211,-39.2297700580611)) ;
#72462 = CARTESIAN_POINT('',(201.559777625419,595.972556589211,-39.2297700580612)) ;
#72463 = CARTESIAN_POINT('',(201.559777625419,596.097556589211,-39.3547700580611)) ;
#72464 = CARTESIAN_POINT('Origin',(201.559777625419,596.097556589211,-39.2297700580612)) ;
#72465 = CARTESIAN_POINT('',(212.118601772286,595.972556589211,-39.2297700580611)) ;
#72466 = CARTESIAN_POINT('',(202.262277625418,596.097556589211,-39.3547700580611)) ;
#72467 = CARTESIAN_POINT('Origin',(202.262277625418,596.097556589211,-39.2297700580612)) ;
#72468 = CARTESIAN_POINT('',(212.118601772286,596.097556589211,-39.3547700580611)) ;
#72469 = CARTESIAN_POINT('Origin',(202.262277625418,598.671056589212,-39.4182700580612)) ;
#72470 = CARTESIAN_POINT('',(202.262277625418,598.671056589212,-39.3547700580612)) ;
#72471 = CARTESIAN_POINT('Origin',(202.262277625418,598.671056589212,-39.4182700580612)) ;
#72472 = CARTESIAN_POINT('Origin',(202.262277625418,598.671056589212,-39.2297700580612)) ;
#72473 = CARTESIAN_POINT('Origin',(202.262277625418,595.988181589211,-39.2297700580612)) ;
#72474 = CARTESIAN_POINT('',(202.262277625418,599.847556589211,-39.3547700580612)) ;
#72475 = CARTESIAN_POINT('Origin',(202.262277625418,599.847556589211,-39.2297700580612)) ;
#72476 = CARTESIAN_POINT('',(202.262277625418,595.988181589211,-39.3547700580611)) ;
#72477 = CARTESIAN_POINT('Origin',(201.559777625419,598.671056589212,-39.4182700580612)) ;
#72478 = CARTESIAN_POINT('',(201.559777625419,598.671056589212,-39.3547700580612)) ;
#72479 = CARTESIAN_POINT('Origin',(201.559777625419,598.671056589212,-39.4182700580612)) ;
#72480 = CARTESIAN_POINT('Origin',(201.559777625419,598.671056589212,-39.2297700580612)) ;
#72481 = CARTESIAN_POINT('Origin',(202.262277625418,597.274056589212,-39.4182700580611)) ;
#72482 = CARTESIAN_POINT('',(202.262277625418,597.337556589212,-39.4182700580611)) ;
#72483 = CARTESIAN_POINT('',(202.262277625418,597.274056589212,-39.3547700580611)) ;
#72484 = CARTESIAN_POINT('Origin',(202.262277625418,597.274056589212,-39.4182700580611)) ;
#72485 = CARTESIAN_POINT('Origin',(202.262277625418,597.274056589212,-39.2297700580612)) ;
#72486 = CARTESIAN_POINT('Origin',(202.262277625418,597.462556589212,-39.4182700580611)) ;
#72487 = CARTESIAN_POINT('Origin',(202.262277625418,597.462556589212,-37.6444650424525)) ;
#72488 = CARTESIAN_POINT('',(202.262277625418,597.337556589212,-37.6444650424525)) ;
#72489 = CARTESIAN_POINT('Origin',(202.262277625418,595.988181589211,-39.2297700580612)) ;
#72490 = CARTESIAN_POINT('Origin',(202.262277625418,596.097556589211,-39.2297700580612)) ;
#72491 = CARTESIAN_POINT('',(202.262277625418,595.988181589211,-39.3547700580611)) ;
#72492 = CARTESIAN_POINT('Origin',(201.559777625419,597.274056589212,-39.4182700580611)) ;
#72493 = CARTESIAN_POINT('',(201.559777625419,597.274056589212,-39.3547700580611)) ;
#72494 = CARTESIAN_POINT('Origin',(201.559777625419,597.274056589212,-39.4182700580611)) ;
#72495 = CARTESIAN_POINT('Origin',(201.559777625419,597.274056589212,-39.2297700580612)) ;
#72496 = CARTESIAN_POINT('Origin',(201.559777625419,595.988181589211,-39.2297700580612)) ;
#72497 = CARTESIAN_POINT('Origin',(201.559777625419,596.097556589211,-39.2297700580612)) ;
#72498 = CARTESIAN_POINT('',(201.559777625419,595.988181589211,-39.3547700580611)) ;
#72499 = CARTESIAN_POINT('Origin',(219.024277625418,597.274056589212,-39.4182700580611)) ;
#72500 = CARTESIAN_POINT('',(219.024277625418,597.274056589212,-39.3547700580611)) ;
#72501 = CARTESIAN_POINT('',(219.024277625418,597.337556589212,-39.4182700580611)) ;
#72502 = CARTESIAN_POINT('Origin',(201.559777625419,595.988181589211,-39.2297700580612)) ;
#72503 = CARTESIAN_POINT('',(201.559777625419,599.847556589211,-39.3547700580611)) ;
#72504 = CARTESIAN_POINT('Origin',(201.559777625419,599.847556589211,-39.2297700580612)) ;
#72505 = CARTESIAN_POINT('',(201.559777625419,595.988181589211,-39.3547700580611)) ;
#72506 = CARTESIAN_POINT('Origin',(218.198777625418,598.671056589212,-39.4182700580611)) ;
#72507 = CARTESIAN_POINT('',(218.198777625418,598.671056589212,-39.3547700580611)) ;
#72508 = CARTESIAN_POINT('Origin',(201.559777625419,596.097556589211,-39.2297700580612)) ;
#72509 = CARTESIAN_POINT('Origin',(201.559777625419,596.097556589211,-39.2297700580612)) ;
#72510 = CARTESIAN_POINT('Origin',(202.262277625418,596.097556589211,-39.2297700580612)) ;
#72511 = CARTESIAN_POINT('Origin',(207.753027625418,599.847556589211,-39.2297700580612)) ;
#72512 = CARTESIAN_POINT('Origin',(201.559777625419,599.847556589211,-39.2297700580612)) ;
#72513 = CARTESIAN_POINT('',(207.753027625418,599.847556589211,-39.3547700580611)) ;
#72514 = CARTESIAN_POINT('Origin',(202.262277625418,599.847556589211,-39.2297700580612)) ;
#72515 = CARTESIAN_POINT('Origin',(201.559777625419,599.847556589211,-39.2297700580612)) ;
#72516 = CARTESIAN_POINT('Origin',(201.559777625419,599.847556589211,-39.2297700580612)) ;
#72517 = CARTESIAN_POINT('Origin',(202.262277625418,599.847556589211,-39.2297700580612)) ;
#72518 = CARTESIAN_POINT('Origin',(219.849777625417,597.337556589212,-41.5221609920506)) ;
#72519 = CARTESIAN_POINT('Origin',(218.198777625418,598.607556589211,-39.3547700580611)) ;
#72520 = CARTESIAN_POINT('Origin',(218.198777625418,598.607556589211,-39.3547700580611)) ;
#72521 = CARTESIAN_POINT('Origin',(218.198777625418,598.607556589211,-39.3547690928544)) ;
#72522 = CARTESIAN_POINT('',(209.814777625418,599.847556589211,-39.3547690928544)) ;
#72523 = CARTESIAN_POINT('',(209.814777625418,596.097556589211,-39.3547690928544)) ;
#72524 = CARTESIAN_POINT('',(209.814777625418,595.988181589211,-39.3547690928544)) ;
#72525 = CARTESIAN_POINT('',(210.517277625419,596.097556589211,-39.3547690928544)) ;
#72526 = CARTESIAN_POINT('',(212.118601772286,596.097556589211,-39.3547690928544)) ;
#72527 = CARTESIAN_POINT('',(210.517277625419,599.847556589211,-39.3547690928544)) ;
#72528 = CARTESIAN_POINT('',(210.517277625419,595.988181589211,-39.3547690928544)) ;
#72529 = CARTESIAN_POINT('',(207.753027625418,599.847556589211,-39.3547690928544)) ;
#72530 = CARTESIAN_POINT('Origin',(209.814777625418,596.097556589211,-39.2297690928544)) ;
#72531 = CARTESIAN_POINT('',(209.814777625418,595.972556589211,-39.2297690928544)) ;
#72532 = CARTESIAN_POINT('Origin',(209.814777625418,596.097556589211,-39.2297690928544)) ;
#72533 = CARTESIAN_POINT('',(209.689777625418,596.097556589211,-39.2297690928544)) ;
#72534 = CARTESIAN_POINT('Origin',(209.814777625418,596.097556589211,-39.2297690928544)) ;
#72535 = CARTESIAN_POINT('Origin',(209.814777625418,596.097556589211,-39.2297690928544)) ;
#72536 = CARTESIAN_POINT('Origin',(209.814777625418,599.847556589211,-39.2297690928544)) ;
#72537 = CARTESIAN_POINT('',(209.689777625418,599.847556589211,-39.2297690928544)) ;
#72538 = CARTESIAN_POINT('Origin',(209.814777625418,599.847556589211,-39.2297690928544)) ;
#72539 = CARTESIAN_POINT('Origin',(209.814777625418,599.847556589211,-39.2297690928544)) ;
#72540 = CARTESIAN_POINT('Origin',(209.814777625418,599.847556589211,-39.2297690928544)) ;
#72541 = CARTESIAN_POINT('Origin',(209.814777625418,595.988181589211,-39.2297690928544)) ;
#72542 = CARTESIAN_POINT('',(209.689777625418,595.988181589211,-39.2297690928544)) ;
#72543 = CARTESIAN_POINT('Origin',(207.753027625418,599.847556589211,-39.2297690928544)) ;
#72544 = CARTESIAN_POINT('Origin',(210.517277625419,599.847556589211,-39.2297690928544)) ;
#72545 = CARTESIAN_POINT('Origin',(212.118601772286,596.097556589211,-39.2297690928544)) ;
#72546 = CARTESIAN_POINT('',(212.118601772286,595.972556589211,-39.2297690928544)) ;
#72547 = CARTESIAN_POINT('Origin',(210.517277625419,596.097556589211,-39.2297690928544)) ;
#72548 = CARTESIAN_POINT('Origin',(210.517277625419,595.988181589211,-39.2297690928544)) ;
#72549 = CARTESIAN_POINT('Origin',(210.517277625419,596.097556589211,-39.2297690928544)) ;
#72550 = CARTESIAN_POINT('Origin',(210.517277625419,599.847556589211,-39.2297690928544)) ;
#72551 = CARTESIAN_POINT('Origin',(210.517277625419,596.097556589211,-39.2297690928544)) ;
#72552 = CARTESIAN_POINT('Origin',(210.517277625419,599.847556589211,-39.2297690928544)) ;
#72553 = CARTESIAN_POINT('Origin',(202.26227762542,607.982556589212,-39.8669650424525)) ;
#72554 = CARTESIAN_POINT('Origin',(202.26227762542,607.982556589212,-39.4182700580611)) ;
#72555 = CARTESIAN_POINT('Origin',(212.118601772288,605.597556589211,-39.2297700580611)) ;
#72556 = CARTESIAN_POINT('',(201.55977762542,605.472556589211,-39.2297700580612)) ;
#72557 = CARTESIAN_POINT('',(201.55977762542,605.597556589211,-39.3547700580611)) ;
#72558 = CARTESIAN_POINT('Origin',(201.55977762542,605.597556589211,-39.2297700580612)) ;
#72559 = CARTESIAN_POINT('',(212.118601772288,605.472556589211,-39.2297700580611)) ;
#72560 = CARTESIAN_POINT('',(202.26227762542,605.597556589211,-39.3547700580611)) ;
#72561 = CARTESIAN_POINT('Origin',(202.26227762542,605.597556589211,-39.2297700580612)) ;
#72562 = CARTESIAN_POINT('',(212.118601772288,605.597556589211,-39.3547700580611)) ;
#72563 = CARTESIAN_POINT('Origin',(202.26227762542,608.171056589212,-39.4182700580612)) ;
#72564 = CARTESIAN_POINT('',(202.26227762542,608.171056589212,-39.3547700580612)) ;
#72565 = CARTESIAN_POINT('Origin',(202.26227762542,608.171056589212,-39.4182700580612)) ;
#72566 = CARTESIAN_POINT('Origin',(202.26227762542,608.171056589212,-39.2297700580612)) ;
#72567 = CARTESIAN_POINT('Origin',(202.26227762542,605.488181589211,-39.2297700580612)) ;
#72568 = CARTESIAN_POINT('',(202.26227762542,609.347556589211,-39.3547700580612)) ;
#72569 = CARTESIAN_POINT('Origin',(202.26227762542,609.347556589211,-39.2297700580612)) ;
#72570 = CARTESIAN_POINT('',(202.26227762542,605.488181589211,-39.3547700580611)) ;
#72571 = CARTESIAN_POINT('Origin',(201.55977762542,608.171056589212,-39.4182700580612)) ;
#72572 = CARTESIAN_POINT('',(201.55977762542,608.171056589212,-39.3547700580612)) ;
#72573 = CARTESIAN_POINT('Origin',(201.55977762542,608.171056589212,-39.4182700580612)) ;
#72574 = CARTESIAN_POINT('Origin',(201.55977762542,608.171056589212,-39.2297700580612)) ;
#72575 = CARTESIAN_POINT('Origin',(202.26227762542,606.774056589212,-39.4182700580611)) ;
#72576 = CARTESIAN_POINT('',(202.26227762542,606.837556589212,-39.4182700580611)) ;
#72577 = CARTESIAN_POINT('',(202.26227762542,606.774056589212,-39.3547700580611)) ;
#72578 = CARTESIAN_POINT('Origin',(202.26227762542,606.774056589212,-39.4182700580611)) ;
#72579 = CARTESIAN_POINT('Origin',(202.26227762542,606.774056589212,-39.2297700580612)) ;
#72580 = CARTESIAN_POINT('Origin',(202.26227762542,606.962556589212,-39.4182700580611)) ;
#72581 = CARTESIAN_POINT('Origin',(202.26227762542,606.962556589212,-37.6444650424525)) ;
#72582 = CARTESIAN_POINT('',(202.26227762542,606.837556589212,-37.6444650424525)) ;
#72583 = CARTESIAN_POINT('Origin',(202.26227762542,605.488181589211,-39.2297700580612)) ;
#72584 = CARTESIAN_POINT('Origin',(202.26227762542,605.597556589211,-39.2297700580612)) ;
#72585 = CARTESIAN_POINT('',(202.26227762542,605.488181589211,-39.3547700580611)) ;
#72586 = CARTESIAN_POINT('Origin',(201.55977762542,606.774056589212,-39.4182700580611)) ;
#72587 = CARTESIAN_POINT('',(201.55977762542,606.774056589212,-39.3547700580611)) ;
#72588 = CARTESIAN_POINT('Origin',(201.55977762542,606.774056589212,-39.4182700580611)) ;
#72589 = CARTESIAN_POINT('Origin',(201.55977762542,606.774056589212,-39.2297700580612)) ;
#72590 = CARTESIAN_POINT('Origin',(201.55977762542,605.488181589211,-39.2297700580612)) ;
#72591 = CARTESIAN_POINT('Origin',(201.55977762542,605.597556589211,-39.2297700580612)) ;
#72592 = CARTESIAN_POINT('',(201.55977762542,605.488181589211,-39.3547700580611)) ;
#72593 = CARTESIAN_POINT('Origin',(219.024277625419,606.774056589212,-39.4182700580611)) ;
#72594 = CARTESIAN_POINT('',(219.024277625419,606.774056589212,-39.3547700580611)) ;
#72595 = CARTESIAN_POINT('',(219.024277625419,606.837556589212,-39.4182700580611)) ;
#72596 = CARTESIAN_POINT('Origin',(201.55977762542,605.488181589211,-39.2297700580612)) ;
#72597 = CARTESIAN_POINT('',(201.55977762542,609.347556589211,-39.3547700580611)) ;
#72598 = CARTESIAN_POINT('Origin',(201.55977762542,609.347556589211,-39.2297700580612)) ;
#72599 = CARTESIAN_POINT('',(201.55977762542,605.488181589211,-39.3547700580611)) ;
#72600 = CARTESIAN_POINT('Origin',(218.198777625419,608.171056589212,-39.4182700580611)) ;
#72601 = CARTESIAN_POINT('',(218.198777625419,608.171056589212,-39.3547700580611)) ;
#72602 = CARTESIAN_POINT('Origin',(201.55977762542,605.597556589211,-39.2297700580612)) ;
#72603 = CARTESIAN_POINT('Origin',(201.55977762542,605.597556589211,-39.2297700580612)) ;
#72604 = CARTESIAN_POINT('Origin',(202.26227762542,605.597556589211,-39.2297700580612)) ;
#72605 = CARTESIAN_POINT('Origin',(207.75302762542,609.347556589211,-39.2297700580612)) ;
#72606 = CARTESIAN_POINT('Origin',(201.55977762542,609.347556589211,-39.2297700580612)) ;
#72607 = CARTESIAN_POINT('',(207.75302762542,609.347556589211,-39.3547700580611)) ;
#72608 = CARTESIAN_POINT('Origin',(202.26227762542,609.347556589211,-39.2297700580612)) ;
#72609 = CARTESIAN_POINT('Origin',(201.55977762542,609.347556589211,-39.2297700580612)) ;
#72610 = CARTESIAN_POINT('Origin',(201.55977762542,609.347556589211,-39.2297700580612)) ;
#72611 = CARTESIAN_POINT('Origin',(202.26227762542,609.347556589211,-39.2297700580612)) ;
#72612 = CARTESIAN_POINT('Origin',(219.849777625419,606.837556589212,-41.5221609920506)) ;
#72613 = CARTESIAN_POINT('Origin',(218.19877762542,608.107556589211,-39.3547700580611)) ;
#72614 = CARTESIAN_POINT('Origin',(218.19877762542,608.107556589211,-39.3547700580611)) ;
#72615 = CARTESIAN_POINT('Origin',(218.19877762542,608.107556589211,-39.3547690928544)) ;
#72616 = CARTESIAN_POINT('',(209.81477762542,609.347556589211,-39.3547690928544)) ;
#72617 = CARTESIAN_POINT('',(209.81477762542,605.597556589211,-39.3547690928544)) ;
#72618 = CARTESIAN_POINT('',(209.81477762542,605.488181589211,-39.3547690928544)) ;
#72619 = CARTESIAN_POINT('',(210.51727762542,605.597556589211,-39.3547690928544)) ;
#72620 = CARTESIAN_POINT('',(212.118601772288,605.597556589211,-39.3547690928544)) ;
#72621 = CARTESIAN_POINT('',(210.51727762542,609.347556589211,-39.3547690928544)) ;
#72622 = CARTESIAN_POINT('',(210.51727762542,605.488181589211,-39.3547690928544)) ;
#72623 = CARTESIAN_POINT('',(207.75302762542,609.347556589211,-39.3547690928544)) ;
#72624 = CARTESIAN_POINT('Origin',(209.81477762542,605.597556589211,-39.2297690928544)) ;
#72625 = CARTESIAN_POINT('',(209.81477762542,605.472556589211,-39.2297690928544)) ;
#72626 = CARTESIAN_POINT('Origin',(209.81477762542,605.597556589211,-39.2297690928544)) ;
#72627 = CARTESIAN_POINT('',(209.68977762542,605.597556589211,-39.2297690928544)) ;
#72628 = CARTESIAN_POINT('Origin',(209.81477762542,605.597556589211,-39.2297690928544)) ;
#72629 = CARTESIAN_POINT('Origin',(209.81477762542,605.597556589211,-39.2297690928544)) ;
#72630 = CARTESIAN_POINT('Origin',(209.81477762542,609.347556589211,-39.2297690928544)) ;
#72631 = CARTESIAN_POINT('',(209.68977762542,609.347556589211,-39.2297690928544)) ;
#72632 = CARTESIAN_POINT('Origin',(209.81477762542,609.347556589211,-39.2297690928544)) ;
#72633 = CARTESIAN_POINT('Origin',(209.81477762542,609.347556589211,-39.2297690928544)) ;
#72634 = CARTESIAN_POINT('Origin',(209.81477762542,609.347556589211,-39.2297690928544)) ;
#72635 = CARTESIAN_POINT('Origin',(209.81477762542,605.488181589211,-39.2297690928544)) ;
#72636 = CARTESIAN_POINT('',(209.68977762542,605.488181589211,-39.2297690928544)) ;
#72637 = CARTESIAN_POINT('Origin',(207.75302762542,609.347556589211,-39.2297690928544)) ;
#72638 = CARTESIAN_POINT('Origin',(210.51727762542,609.347556589211,-39.2297690928544)) ;
#72639 = CARTESIAN_POINT('Origin',(212.118601772288,605.597556589211,-39.2297690928544)) ;
#72640 = CARTESIAN_POINT('',(212.118601772288,605.472556589211,-39.2297690928544)) ;
#72641 = CARTESIAN_POINT('Origin',(210.51727762542,605.597556589211,-39.2297690928544)) ;
#72642 = CARTESIAN_POINT('Origin',(210.51727762542,605.488181589211,-39.2297690928544)) ;
#72643 = CARTESIAN_POINT('Origin',(210.51727762542,605.597556589211,-39.2297690928544)) ;
#72644 = CARTESIAN_POINT('Origin',(210.51727762542,609.347556589211,-39.2297690928544)) ;
#72645 = CARTESIAN_POINT('Origin',(210.51727762542,605.597556589211,-39.2297690928544)) ;
#72646 = CARTESIAN_POINT('Origin',(210.51727762542,609.347556589211,-39.2297690928544)) ;
#72647 = CARTESIAN_POINT('Origin',(199.088527625413,569.472556589217,-34.0221601717606)) ;
#72648 = CARTESIAN_POINT('',(199.088527625421,611.548005939917,-41.5221601717606)) ;
#72649 = CARTESIAN_POINT('',(199.088527625419,603.397107238494,-41.5221601717606)) ;
#72650 = CARTESIAN_POINT('Origin',(199.088527625413,569.472556589217,-34.0221601717606)) ;
#72651 = CARTESIAN_POINT('',(199.088527625417,593.897107238495,-41.5221601717606)) ;
#72652 = CARTESIAN_POINT('',(199.088527625419,602.048005939937,-41.5221601717606)) ;
#72653 = CARTESIAN_POINT('Origin',(199.088527625413,569.472556589217,-34.0221601717606)) ;
#72654 = CARTESIAN_POINT('',(199.088527625416,584.397107238494,-41.5221601717606)) ;
#72655 = CARTESIAN_POINT('',(199.088527625417,592.548005939937,-41.5221601717606)) ;
#72656 = CARTESIAN_POINT('Origin',(199.088527625413,569.472556589217,-34.0221601717606)) ;
#72657 = CARTESIAN_POINT('',(199.088527625414,574.897107238494,-41.5221601717606)) ;
#72658 = CARTESIAN_POINT('',(199.088527625416,583.048005939937,-41.5221601717606)) ;
#72659 = CARTESIAN_POINT('Origin',(199.088527625413,569.472556589217,-34.0221601717606)) ;
#72660 = CARTESIAN_POINT('',(199.088527625412,565.397107238498,-41.5221601717606)) ;
#72661 = CARTESIAN_POINT('',(199.088527625414,573.548005939937,-41.5221601717606)) ;
#72662 = CARTESIAN_POINT('Origin',(199.088527625413,569.472556589217,-34.0221601717606)) ;
#72663 = CARTESIAN_POINT('',(199.088527625411,555.897107238498,-41.5221601717606)) ;
#72664 = CARTESIAN_POINT('',(199.088527625412,564.04800593993,-41.5221601717606)) ;
#72665 = CARTESIAN_POINT('Origin',(199.088527625413,569.472556589217,-34.0221601717606)) ;
#72666 = CARTESIAN_POINT('',(199.088527625409,546.397107238498,-41.5221601717606)) ;
#72667 = CARTESIAN_POINT('',(199.088527625411,554.54800593993,-41.5221601717606)) ;
#72668 = CARTESIAN_POINT('Origin',(199.088527625413,569.472556589217,-34.0221601717606)) ;
#72669 = CARTESIAN_POINT('',(199.088527625407,536.897107238498,-41.5221601717606)) ;
#72670 = CARTESIAN_POINT('',(199.088527625409,545.04800593993,-41.5221601717606)) ;
#72671 = CARTESIAN_POINT('Origin',(199.088527625413,569.472556589217,-34.0221601717606)) ;
#72672 = CARTESIAN_POINT('',(199.088527625406,527.397107238498,-41.5221601717606)) ;
#72673 = CARTESIAN_POINT('',(199.088527625407,535.54800593993,-41.5221601717606)) ;
#72674 = CARTESIAN_POINT('Origin',(199.088527625416,584.397107238494,-41.5221601717606)) ;
#72675 = CARTESIAN_POINT('',(212.588527625416,584.397107238492,-38.2721601717612)) ;
#72676 = CARTESIAN_POINT('Origin',(212.588527625417,592.548005939935,-41.5221601717612)) ;
#72677 = CARTESIAN_POINT('',(212.588527625417,592.548005939935,-38.2721601717612)) ;
#72678 = CARTESIAN_POINT('Origin',(212.588527625411,554.548005939928,-41.5221601717612)) ;
#72679 = CARTESIAN_POINT('',(212.588527625411,554.548005939928,-38.2721601717612)) ;
#72680 = CARTESIAN_POINT('Origin',(199.088527625409,546.397107238498,-41.5221601717606)) ;
#72681 = CARTESIAN_POINT('',(212.588527625409,546.397107238495,-38.2721601717612)) ;
#72682 = CARTESIAN_POINT('Origin',(212.588527625409,545.048005939928,-41.5221601717612)) ;
#72683 = CARTESIAN_POINT('',(212.588527625409,545.048005939928,-38.2721601717612)) ;
#72684 = CARTESIAN_POINT('Origin',(199.088527625407,536.897107238498,-41.5221601717606)) ;
#72685 = CARTESIAN_POINT('',(212.588527625408,536.897107238495,-38.2721601717612)) ;
#72686 = CARTESIAN_POINT('Origin',(199.088527625414,574.897107238495,-41.5221601717606)) ;
#72687 = CARTESIAN_POINT('',(212.588527625414,574.897107238492,-38.2721601717612)) ;
#72688 = CARTESIAN_POINT('Origin',(212.588527625416,583.048005939935,-41.5221601717612)) ;
#72689 = CARTESIAN_POINT('',(212.588527625416,583.048005939935,-38.2721601717612)) ;
#72690 = CARTESIAN_POINT('Origin',(199.088527625417,593.897107238495,-41.5221601717606)) ;
#72691 = CARTESIAN_POINT('',(212.588527625418,593.897107238492,-38.2721601717612)) ;
#72692 = CARTESIAN_POINT('Origin',(212.588527625419,602.048005939935,-41.5221601717612)) ;
#72693 = CARTESIAN_POINT('',(212.588527625419,602.048005939935,-38.2721601717612)) ;
#72694 = CARTESIAN_POINT('Origin',(212.588527625412,564.048005939928,-41.5221601717612)) ;
#72695 = CARTESIAN_POINT('',(212.588527625412,564.048005939928,-38.2721601717612)) ;
#72696 = CARTESIAN_POINT('Origin',(199.088527625411,555.897107238498,-41.5221601717606)) ;
#72697 = CARTESIAN_POINT('',(212.588527625411,555.897107238495,-38.2721601717612)) ;
#72698 = CARTESIAN_POINT('Origin',(212.588527625407,535.548005939928,-41.5221601717612)) ;
#72699 = CARTESIAN_POINT('',(212.588527625407,535.548005939928,-38.2721601717612)) ;
#72700 = CARTESIAN_POINT('Origin',(199.088527625406,527.397107238498,-41.5221601717606)) ;
#72701 = CARTESIAN_POINT('',(212.588527625406,527.397107238495,-38.2721601717612)) ;
#72702 = CARTESIAN_POINT('Origin',(212.588527625414,573.548005939935,-41.5221601717612)) ;
#72703 = CARTESIAN_POINT('',(212.588527625414,573.548005939935,-38.2721601717612)) ;
#72704 = CARTESIAN_POINT('Origin',(199.088527625412,565.397107238498,-41.5221601717606)) ;
#72705 = CARTESIAN_POINT('',(212.588527625413,565.397107238495,-38.2721601717612)) ;
#72706 = CARTESIAN_POINT('Origin',(199.088527625419,603.397107238494,-41.5221601717606)) ;
#72707 = CARTESIAN_POINT('',(212.588527625419,603.397107238492,-38.2721601717612)) ;
#72708 = CARTESIAN_POINT('Origin',(212.58852762542,611.548005939915,-41.5221601717612)) ;
#72709 = CARTESIAN_POINT('',(212.588527625421,611.548005939915,-38.2721601717612)) ;
#72710 = CARTESIAN_POINT('Origin',(211.838527625423,621.71816687483,-26.5221601717612)) ;
#72711 = CARTESIAN_POINT('',(199.088527625407,535.696374002382,-26.5221601716848)) ;
#72712 = CARTESIAN_POINT('',(211.838533909042,535.6963740129,-26.52216017177)) ;
#72713 = CARTESIAN_POINT('',(199.838521341308,535.696374013642,-26.5221601717606)) ;
#72714 = CARTESIAN_POINT('',(211.838533909108,536.74873917605,-26.52216017177)) ;
#72715 = CARTESIAN_POINT('',(211.838533909108,536.74873916479,-26.5221601717612)) ;
#72716 = CARTESIAN_POINT('',(199.088527625408,536.748739186608,-26.5221601717606)) ;
#72717 = CARTESIAN_POINT('',(204.838527625408,536.748739186607,-26.5221601717609)) ;
#72718 = CARTESIAN_POINT('',(199.088527625409,545.196374002382,-26.5221601716848)) ;
#72719 = CARTESIAN_POINT('',(199.088527625421,612.748739186625,-26.5221601717606)) ;
#72720 = CARTESIAN_POINT('',(211.838533909044,545.1963740129,-26.52216017177)) ;
#72721 = CARTESIAN_POINT('',(199.83852134131,545.196374013642,-26.5221601717606)) ;
#72722 = CARTESIAN_POINT('',(211.83853390911,546.24873917605,-26.52216017177)) ;
#72723 = CARTESIAN_POINT('',(211.83853390911,546.24873916479,-26.5221601717612)) ;
#72724 = CARTESIAN_POINT('',(199.08852762541,546.248739186608,-26.5221601717606)) ;
#72725 = CARTESIAN_POINT('',(204.83852762541,546.248739186607,-26.5221601717609)) ;
#72726 = CARTESIAN_POINT('',(199.088527625411,554.696374002382,-26.5221601716848)) ;
#72727 = CARTESIAN_POINT('',(199.088527625421,612.748739186625,-26.5221601717606)) ;
#72728 = CARTESIAN_POINT('',(211.838533909045,554.6963740129,-26.52216017177)) ;
#72729 = CARTESIAN_POINT('',(199.838521341311,554.696374013642,-26.5221601717606)) ;
#72730 = CARTESIAN_POINT('',(211.838533909111,555.74873917605,-26.52216017177)) ;
#72731 = CARTESIAN_POINT('',(211.838533909111,555.74873916479,-26.5221601717612)) ;
#72732 = CARTESIAN_POINT('',(199.088527625411,555.748739186608,-26.5221601717606)) ;
#72733 = CARTESIAN_POINT('',(204.838527625411,555.748739186607,-26.5221601717609)) ;
#72734 = CARTESIAN_POINT('',(199.088527625412,564.196374002382,-26.5221601716848)) ;
#72735 = CARTESIAN_POINT('',(199.088527625421,612.748739186625,-26.5221601717606)) ;
#72736 = CARTESIAN_POINT('',(211.838533909047,564.1963740129,-26.5221601717699)) ;
#72737 = CARTESIAN_POINT('',(199.838521341313,564.196374013642,-26.5221601717606)) ;
#72738 = CARTESIAN_POINT('',(211.838533909113,565.24873917605,-26.52216017177)) ;
#72739 = CARTESIAN_POINT('',(211.838533909113,565.24873916479,-26.5221601717612)) ;
#72740 = CARTESIAN_POINT('',(199.088527625413,565.248739186608,-26.5221601717606)) ;
#72741 = CARTESIAN_POINT('',(204.838527625413,565.248739186607,-26.5221601717609)) ;
#72742 = CARTESIAN_POINT('',(199.088527625414,573.696374002382,-26.5221601716848)) ;
#72743 = CARTESIAN_POINT('',(199.088527625421,612.748739186625,-26.5221601717606)) ;
#72744 = CARTESIAN_POINT('',(211.838533909049,573.6963740129,-26.5221601717699)) ;
#72745 = CARTESIAN_POINT('',(199.838521341315,573.696374013642,-26.5221601717606)) ;
#72746 = CARTESIAN_POINT('',(211.838533909115,574.74873916553,-26.52216017177)) ;
#72747 = CARTESIAN_POINT('',(211.838533909115,574.74873916479,-26.5221601717612)) ;
#72748 = CARTESIAN_POINT('',(199.088527625415,574.748739176051,-26.5221601716848)) ;
#72749 = CARTESIAN_POINT('',(199.838521396415,574.748739164792,-26.5221601717606)) ;
#72750 = CARTESIAN_POINT('',(199.088527625416,583.196374002382,-26.5221601716848)) ;
#72751 = CARTESIAN_POINT('',(199.088527625421,612.748739186625,-26.5221601717606)) ;
#72752 = CARTESIAN_POINT('',(211.838533909051,583.1963740129,-26.5221601717699)) ;
#72753 = CARTESIAN_POINT('',(199.838521341316,583.196374013642,-26.5221601717606)) ;
#72754 = CARTESIAN_POINT('',(211.838533909116,584.24873916553,-26.52216017177)) ;
#72755 = CARTESIAN_POINT('',(211.838533909116,584.24873916479,-26.5221601717612)) ;
#72756 = CARTESIAN_POINT('',(199.088527625416,584.248739176051,-26.5221601716848)) ;
#72757 = CARTESIAN_POINT('',(199.838521396416,584.248739164792,-26.5221601717606)) ;
#72758 = CARTESIAN_POINT('',(199.088527625417,592.696374002382,-26.5221601716848)) ;
#72759 = CARTESIAN_POINT('',(199.088527625421,612.748739186625,-26.5221601717606)) ;
#72760 = CARTESIAN_POINT('',(211.838533909052,592.6963740129,-26.5221601717699)) ;
#72761 = CARTESIAN_POINT('',(199.838521341318,592.696374013642,-26.5221601717606)) ;
#72762 = CARTESIAN_POINT('',(211.838533909118,593.74873916553,-26.52216017177)) ;
#72763 = CARTESIAN_POINT('',(211.838533909118,593.74873916479,-26.5221601717612)) ;
#72764 = CARTESIAN_POINT('',(199.088527625418,593.748739176051,-26.5221601716848)) ;
#72765 = CARTESIAN_POINT('',(199.838521396418,593.748739164792,-26.5221601717606)) ;
#72766 = CARTESIAN_POINT('',(199.088527625419,602.196374002382,-26.5221601716848)) ;
#72767 = CARTESIAN_POINT('',(199.088527625421,612.748739186625,-26.5221601717606)) ;
#72768 = CARTESIAN_POINT('',(211.838533909054,602.1963740129,-26.52216017177)) ;
#72769 = CARTESIAN_POINT('',(199.83852134132,602.196374013642,-26.5221601717606)) ;
#72770 = CARTESIAN_POINT('',(211.83853390912,603.24873916553,-26.52216017177)) ;
#72771 = CARTESIAN_POINT('',(211.83853390912,603.24873916479,-26.5221601717612)) ;
#72772 = CARTESIAN_POINT('',(199.08852762542,603.248739176051,-26.5221601716848)) ;
#72773 = CARTESIAN_POINT('',(199.83852134132,603.248739164792,-26.5221601717606)) ;
#72774 = CARTESIAN_POINT('',(199.088527625421,611.696374002377,-26.5221601716849)) ;
#72775 = CARTESIAN_POINT('',(199.088527625421,612.748739186625,-26.5221601717606)) ;
#72776 = CARTESIAN_POINT('',(211.838533909055,611.69637401289,-26.52216017177)) ;
#72777 = CARTESIAN_POINT('',(199.838521341321,611.696374013632,-26.5221601717606)) ;
#72778 = CARTESIAN_POINT('',(211.838533909121,612.748739176079,-26.52216017177)) ;
#72779 = CARTESIAN_POINT('',(211.838533909121,612.74873916483,-26.5221601717612)) ;
#72780 = CARTESIAN_POINT('',(194.588527625421,612.748739186625,-26.5221601717604)) ;
#72781 = CARTESIAN_POINT('',(199.088527625421,612.748739186625,-26.5221601717606)) ;
#72782 = CARTESIAN_POINT('',(194.588527625406,526.196373991821,-26.5221601717604)) ;
#72783 = CARTESIAN_POINT('',(194.588527625421,612.748739186625,-26.5221601717604)) ;
#72784 = CARTESIAN_POINT('',(211.838533909041,526.196374002377,-26.52216017177)) ;
#72785 = CARTESIAN_POINT('',(199.088527625406,526.19637399182,-26.5221601717606)) ;
#72786 = CARTESIAN_POINT('',(211.838533909106,527.24873917605,-26.52216017177)) ;
#72787 = CARTESIAN_POINT('',(211.838533909106,527.24873916479,-26.5221601717612)) ;
#72788 = CARTESIAN_POINT('',(199.088527625406,527.248739186608,-26.5221601717606)) ;
#72789 = CARTESIAN_POINT('',(204.838527625406,527.248739186607,-26.5221601717609)) ;
#72790 = CARTESIAN_POINT('',(199.088527625421,612.748739186625,-26.5221601717606)) ;
#72791 = CARTESIAN_POINT('Origin',(211.838527625423,621.71816687483,-27.2721601717612)) ;
#72792 = CARTESIAN_POINT('',(212.588527625408,535.68328258344,-27.2721664559512)) ;
#72793 = CARTESIAN_POINT('Origin',(211.83852762055,535.683282730381,-27.2721601756534)) ;
#72794 = CARTESIAN_POINT('',(212.588527625408,536.76183059499,-27.2721664560112)) ;
#72795 = CARTESIAN_POINT('',(212.588527625408,535.68328258344,-27.2721664559512)) ;
#72796 = CARTESIAN_POINT('Origin',(211.838527620551,536.761830448045,-27.2721601756523)) ;
#72797 = CARTESIAN_POINT('Origin',(197.838527625408,535.722556589213,-25.0221601717606)) ;
#72798 = CARTESIAN_POINT('',(199.088527625407,535.548005939932,-35.0221601717606)) ;
#72799 = CARTESIAN_POINT('',(212.588527625407,535.539278407464,-35.5221601717612)) ;
#72800 = CARTESIAN_POINT('',(206.096960845768,535.652589127089,-29.0305933921213)) ;
#72801 = CARTESIAN_POINT('',(212.588527625408,535.68328258344,-27.2721664559512)) ;
#72802 = CARTESIAN_POINT('Origin',(211.838527625423,621.71816687483,-27.2721601717612)) ;
#72803 = CARTESIAN_POINT('',(212.588527625409,545.18328258344,-27.2721664559512)) ;
#72804 = CARTESIAN_POINT('',(212.58852762541,546.26183059499,-27.2721664560112)) ;
#72805 = CARTESIAN_POINT('',(212.588527625409,545.18328258344,-27.2721664559512)) ;
#72806 = CARTESIAN_POINT('Origin',(211.838527620553,546.261830448045,-27.2721601756518)) ;
#72807 = CARTESIAN_POINT('Origin',(211.838527620552,545.183282730381,-27.2721601756526)) ;
#72808 = CARTESIAN_POINT('Origin',(211.838527625423,621.71816687483,-27.2721601717612)) ;
#72809 = CARTESIAN_POINT('',(212.588527625411,554.68328258344,-27.2721664559512)) ;
#72810 = CARTESIAN_POINT('Origin',(211.838527620553,554.683282730381,-27.2721601756534)) ;
#72811 = CARTESIAN_POINT('',(212.588527625411,555.76183059499,-27.2721664560112)) ;
#72812 = CARTESIAN_POINT('',(212.588527625411,554.68328258344,-27.2721664559512)) ;
#72813 = CARTESIAN_POINT('Origin',(211.838527620554,555.761830448045,-27.2721601756524)) ;
#72814 = CARTESIAN_POINT('Origin',(211.838527625423,621.71816687483,-27.2721601717612)) ;
#72815 = CARTESIAN_POINT('',(212.588527625413,564.18328258344,-27.2721664559512)) ;
#72816 = CARTESIAN_POINT('Origin',(211.838527620556,564.183282730381,-27.2721601756519)) ;
#72817 = CARTESIAN_POINT('',(212.588527625413,565.26183059499,-27.2721664560112)) ;
#72818 = CARTESIAN_POINT('',(212.588527625413,564.18328258344,-27.2721664559512)) ;
#72819 = CARTESIAN_POINT('Origin',(211.838527620555,565.261830448045,-27.2721601756536)) ;
#72820 = CARTESIAN_POINT('Origin',(211.838527625423,621.71816687483,-27.2721601717612)) ;
#72821 = CARTESIAN_POINT('',(212.588527625415,573.68328258343,-27.2721664559512)) ;
#72822 = CARTESIAN_POINT('',(212.588527625415,574.76183059499,-27.2721664560112)) ;
#72823 = CARTESIAN_POINT('',(212.588527625415,573.68328258344,-27.2721664559512)) ;
#72824 = CARTESIAN_POINT('Origin',(211.838527620558,574.761830448045,-27.2721601756523)) ;
#72825 = CARTESIAN_POINT('Origin',(211.838527620555,573.683282730364,-27.2721601756541)) ;
#72826 = CARTESIAN_POINT('Origin',(211.838527625423,621.71816687483,-27.2721601717612)) ;
#72827 = CARTESIAN_POINT('',(212.588527625416,583.18328258344,-27.2721664559512)) ;
#72828 = CARTESIAN_POINT('',(212.588527625416,584.26183059499,-27.2721664560112)) ;
#72829 = CARTESIAN_POINT('',(212.588527625416,583.18328258344,-27.2721664559512)) ;
#72830 = CARTESIAN_POINT('Origin',(211.83852762056,584.261830448045,-27.2721601756523)) ;
#72831 = CARTESIAN_POINT('Origin',(211.838527620558,583.183282730381,-27.2721601756534)) ;
#72832 = CARTESIAN_POINT('Origin',(211.838527625423,621.71816687483,-27.2721601717612)) ;
#72833 = CARTESIAN_POINT('',(212.588527625418,592.68328258344,-27.2721664559512)) ;
#72834 = CARTESIAN_POINT('',(212.588527625418,593.76183059499,-27.2721664560112)) ;
#72835 = CARTESIAN_POINT('',(212.588527625418,592.68328258344,-27.2721664559512)) ;
#72836 = CARTESIAN_POINT('Origin',(211.838527620561,593.761830448045,-27.2721601756523)) ;
#72837 = CARTESIAN_POINT('Origin',(211.838527620559,592.683282730381,-27.2721601756542)) ;
#72838 = CARTESIAN_POINT('Origin',(211.838527625423,621.71816687483,-27.2721601717612)) ;
#72839 = CARTESIAN_POINT('',(212.588527625419,602.18328258344,-27.2721664559512)) ;
#72840 = CARTESIAN_POINT('Origin',(211.838527620561,602.183282730381,-27.2721601756535)) ;
#72841 = CARTESIAN_POINT('',(212.58852762542,603.26183059499,-27.2721664560112)) ;
#72842 = CARTESIAN_POINT('',(212.588527625419,602.18328258344,-27.2721664559512)) ;
#72843 = CARTESIAN_POINT('Origin',(211.838527620563,603.261830448045,-27.2721601756519)) ;
#72844 = CARTESIAN_POINT('Origin',(211.838527625423,621.71816687483,-27.2721601717612)) ;
#72845 = CARTESIAN_POINT('',(212.588527625421,611.68328258343,-27.2721664559512)) ;
#72846 = CARTESIAN_POINT('',(212.588527625421,612.76183059503,-27.2721664560112)) ;
#72847 = CARTESIAN_POINT('',(212.588527625421,611.68328258343,-27.2721664559512)) ;
#72848 = CARTESIAN_POINT('Origin',(211.838527620563,612.761830448138,-27.2721601756519)) ;
#72849 = CARTESIAN_POINT('Origin',(211.838527620567,611.683282730347,-27.2721601756485)) ;
#72850 = CARTESIAN_POINT('Origin',(197.838527625406,527.449472433283,-38.0221601717605)) ;
#72851 = CARTESIAN_POINT('',(212.588527625406,527.26183059499,-27.2721664560112)) ;
#72852 = CARTESIAN_POINT('Origin',(211.838527620549,527.261830448045,-27.2721601756523)) ;
#72853 = CARTESIAN_POINT('',(212.588527625406,527.405834770959,-35.5221601717612)) ;
#72854 = CARTESIAN_POINT('',(212.588527625406,527.3971072385,-35.0221601717612)) ;
#72855 = CARTESIAN_POINT('',(209.49143822564,527.351774874399,-32.4250707719951)) ;
#72856 = CARTESIAN_POINT('',(199.088527625406,527.261830594102,-27.2721664048106)) ;
#72857 = CARTESIAN_POINT('Origin',(211.838527625423,621.71816687483,-27.2721601717612)) ;
#72858 = CARTESIAN_POINT('',(212.588527625406,526.18328258344,-27.2721664559512)) ;
#72859 = CARTESIAN_POINT('',(212.588527625406,526.18328258344,-27.2721664559512)) ;
#72860 = CARTESIAN_POINT('Origin',(211.838527620549,526.183282730381,-27.2721601756526)) ;
#72861 = CARTESIAN_POINT('Origin',(212.33852762541,547.97255658922,-35.2721601717612)) ;
#72862 = CARTESIAN_POINT('',(212.58852762541,547.97255658922,-35.5221601717612)) ;
#72863 = CARTESIAN_POINT('Origin',(212.33852762541,547.97255658922,-35.2721601717612)) ;
#72864 = CARTESIAN_POINT('',(212.088527625408,536.897107238495,-35.0221601717612)) ;
#72865 = CARTESIAN_POINT('',(212.588527625408,536.905834770959,-35.5221601717612)) ;
#72866 = CARTESIAN_POINT('',(209.449988760834,536.851051371299,-32.3836213071874)) ;
#72867 = CARTESIAN_POINT('',(212.588527625409,545.039278407464,-35.5221601717612)) ;
#72868 = CARTESIAN_POINT('',(212.58852762541,547.97255658922,-35.5221601717612)) ;
#72869 = CARTESIAN_POINT('',(212.088527625409,545.048005939928,-35.0221601717612)) ;
#72870 = CARTESIAN_POINT('',(206.138410310577,545.15186562399,-29.0720428569291)) ;
#72871 = CARTESIAN_POINT('',(212.08852762541,547.97255658922,-35.0221601717612)) ;
#72872 = CARTESIAN_POINT('Origin',(212.33852762541,547.97255658922,-35.2721601717612)) ;
#72873 = CARTESIAN_POINT('',(212.088527625409,546.397107238495,-35.0221601717612)) ;
#72874 = CARTESIAN_POINT('',(212.588527625409,546.405834770959,-35.5221601717612)) ;
#72875 = CARTESIAN_POINT('',(209.408539296028,546.3503278682,-32.3421718423797)) ;
#72876 = CARTESIAN_POINT('',(212.588527625411,554.539278407464,-35.5221601717612)) ;
#72877 = CARTESIAN_POINT('',(212.58852762541,547.97255658922,-35.5221601717612)) ;
#72878 = CARTESIAN_POINT('',(212.088527625411,554.548005939928,-35.0221601717612)) ;
#72879 = CARTESIAN_POINT('',(206.179859775386,554.65114212089,-29.1134923217368)) ;
#72880 = CARTESIAN_POINT('',(212.08852762541,547.97255658922,-35.0221601717612)) ;
#72881 = CARTESIAN_POINT('Origin',(212.33852762541,547.97255658922,-35.2721601717612)) ;
#72882 = CARTESIAN_POINT('',(212.088527625411,555.897107238495,-35.0221601717612)) ;
#72883 = CARTESIAN_POINT('',(212.588527625411,555.90583477096,-35.5221601717612)) ;
#72884 = CARTESIAN_POINT('',(209.367089831222,555.8496043651,-32.300722377572)) ;
#72885 = CARTESIAN_POINT('',(212.588527625412,564.039278407464,-35.5221601717612)) ;
#72886 = CARTESIAN_POINT('',(212.58852762541,547.97255658922,-35.5221601717612)) ;
#72887 = CARTESIAN_POINT('',(212.088527625412,564.048005939928,-35.0221601717612)) ;
#72888 = CARTESIAN_POINT('',(206.221309240196,564.150418617791,-29.1549417865445)) ;
#72889 = CARTESIAN_POINT('',(212.08852762541,547.97255658922,-35.0221601717612)) ;
#72890 = CARTESIAN_POINT('Origin',(212.33852762541,547.97255658922,-35.2721601717612)) ;
#72891 = CARTESIAN_POINT('',(212.088527625413,565.397107238495,-35.0221601717612)) ;
#72892 = CARTESIAN_POINT('',(212.588527625413,565.405834770959,-35.5221601717612)) ;
#72893 = CARTESIAN_POINT('',(209.325640366416,565.348880862001,-32.2592729127642)) ;
#72894 = CARTESIAN_POINT('',(212.588527625414,573.53927840747,-35.5221601717612)) ;
#72895 = CARTESIAN_POINT('',(212.58852762541,547.97255658922,-35.5221601717612)) ;
#72896 = CARTESIAN_POINT('',(212.088527625414,573.548005939935,-35.0221601717612)) ;
#72897 = CARTESIAN_POINT('',(209.513253733442,573.592957512927,-32.4468862797886)) ;
#72898 = CARTESIAN_POINT('',(212.08852762541,547.97255658922,-35.0221601717612)) ;
#72899 = CARTESIAN_POINT('Origin',(212.33852762541,547.97255658922,-35.2721601717612)) ;
#72900 = CARTESIAN_POINT('',(212.088527625414,574.897107238492,-35.0221601717612)) ;
#72901 = CARTESIAN_POINT('',(212.588527625414,574.905834770956,-35.5221601717612)) ;
#72902 = CARTESIAN_POINT('',(206.033695873173,574.791419757129,-28.9673284195202)) ;
#72903 = CARTESIAN_POINT('',(212.588527625416,583.039278407471,-35.5221601717612)) ;
#72904 = CARTESIAN_POINT('',(212.58852762541,547.97255658922,-35.5221601717612)) ;
#72905 = CARTESIAN_POINT('',(212.088527625416,583.048005939935,-35.0221601717612)) ;
#72906 = CARTESIAN_POINT('',(209.554703198251,583.092234009828,-32.4883357445963)) ;
#72907 = CARTESIAN_POINT('',(212.08852762541,547.97255658922,-35.0221601717612)) ;
#72908 = CARTESIAN_POINT('Origin',(212.33852762541,547.97255658922,-35.2721601717612)) ;
#72909 = CARTESIAN_POINT('',(212.088527625416,584.397107238492,-35.0221601717612)) ;
#72910 = CARTESIAN_POINT('',(212.588527625416,584.405834770956,-35.5221601717612)) ;
#72911 = CARTESIAN_POINT('',(205.992246408367,584.290696254029,-28.9258789547125)) ;
#72912 = CARTESIAN_POINT('',(212.588527625417,592.539278407471,-35.5221601717612)) ;
#72913 = CARTESIAN_POINT('',(212.58852762541,547.97255658922,-35.5221601717612)) ;
#72914 = CARTESIAN_POINT('',(212.088527625417,592.548005939935,-35.0221601717612)) ;
#72915 = CARTESIAN_POINT('',(209.59615266306,592.591510506729,-32.529785209404)) ;
#72916 = CARTESIAN_POINT('',(212.08852762541,547.97255658922,-35.0221601717612)) ;
#72917 = CARTESIAN_POINT('Origin',(212.33852762541,547.97255658922,-35.2721601717612)) ;
#72918 = CARTESIAN_POINT('',(212.088527625418,593.897107238492,-35.0221601717612)) ;
#72919 = CARTESIAN_POINT('',(212.588527625418,593.905834770956,-35.5221601717612)) ;
#72920 = CARTESIAN_POINT('',(205.950796943561,593.78997275093,-28.8844294899048)) ;
#72921 = CARTESIAN_POINT('',(212.588527625419,602.039278407471,-35.5221601717612)) ;
#72922 = CARTESIAN_POINT('',(212.58852762541,547.97255658922,-35.5221601717612)) ;
#72923 = CARTESIAN_POINT('',(212.088527625419,602.048005939935,-35.0221601717612)) ;
#72924 = CARTESIAN_POINT('',(209.63760212787,602.090787003629,-32.5712346742117)) ;
#72925 = CARTESIAN_POINT('',(212.08852762541,547.97255658922,-35.0221601717612)) ;
#72926 = CARTESIAN_POINT('Origin',(212.33852762541,547.97255658922,-35.2721601717612)) ;
#72927 = CARTESIAN_POINT('',(212.088527625419,603.397107238492,-35.0221601717612)) ;
#72928 = CARTESIAN_POINT('',(212.588527625419,603.405834770956,-35.5221601717612)) ;
#72929 = CARTESIAN_POINT('',(205.909347478755,603.28924924783,-28.842980025097)) ;
#72930 = CARTESIAN_POINT('',(212.588527625421,611.539278407451,-35.5221601717612)) ;
#72931 = CARTESIAN_POINT('',(212.58852762541,547.97255658922,-35.5221601717612)) ;
#72932 = CARTESIAN_POINT('',(212.088527625421,611.548005939915,-35.0221601717612)) ;
#72933 = CARTESIAN_POINT('',(209.679051592679,611.59006350051,-32.6126841390194)) ;
#72934 = CARTESIAN_POINT('',(212.08852762541,547.97255658922,-35.0221601717612)) ;
#72935 = CARTESIAN_POINT('Origin',(197.838527625406,526.222556589213,-25.0221601717606)) ;
#72936 = CARTESIAN_POINT('',(212.588527625406,526.18328258344,-27.2721664559512)) ;
#72937 = CARTESIAN_POINT('',(194.588527625405,525.934548017903,-41.5221601717604)) ;
#72938 = CARTESIAN_POINT('Origin',(197.838527625408,536.949472433283,-38.0221601717605)) ;
#72939 = CARTESIAN_POINT('',(212.588527625408,536.8971072385,-35.0221601717612)) ;
#72940 = CARTESIAN_POINT('',(199.088527625408,536.897107238499,-35.0221601717606)) ;
#72941 = CARTESIAN_POINT('',(201.838527625408,536.897107238497,-35.0221601717607)) ;
#72942 = CARTESIAN_POINT('',(199.088527625408,536.761830595002,-27.2721664563906)) ;
#72943 = CARTESIAN_POINT('Origin',(197.83852762541,545.222556589213,-25.0221601717606)) ;
#72944 = CARTESIAN_POINT('',(199.088527625409,545.048005939932,-35.0221601717606)) ;
#72945 = CARTESIAN_POINT('',(199.088527625409,545.048005939932,-35.0221601717606)) ;
#72946 = CARTESIAN_POINT('',(201.838527625409,545.04800593993,-35.0221601717607)) ;
#72947 = CARTESIAN_POINT('',(212.588527625409,545.18328258344,-27.2721664559512)) ;
#72948 = CARTESIAN_POINT('Origin',(197.838527625409,546.449472433283,-38.0221601717605)) ;
#72949 = CARTESIAN_POINT('',(212.588527625409,546.3971072385,-35.0221601717612)) ;
#72950 = CARTESIAN_POINT('',(199.088527625409,546.3971072385,-35.0221601717606)) ;
#72951 = CARTESIAN_POINT('',(201.838527625409,546.397107238497,-35.0221601717607)) ;
#72952 = CARTESIAN_POINT('',(199.08852762541,546.261830594102,-27.2721664048106)) ;
#72953 = CARTESIAN_POINT('Origin',(197.838527625411,554.722556589213,-25.0221601717605)) ;
#72954 = CARTESIAN_POINT('',(199.088527625411,554.548005939932,-35.0221601717606)) ;
#72955 = CARTESIAN_POINT('',(199.088527625411,554.548005939932,-35.0221601717606)) ;
#72956 = CARTESIAN_POINT('',(201.838527625411,554.54800593993,-35.0221601717607)) ;
#72957 = CARTESIAN_POINT('',(212.588527625411,554.68328258344,-27.2721664559512)) ;
#72958 = CARTESIAN_POINT('Origin',(197.838527625411,555.949472433283,-38.0221601717606)) ;
#72959 = CARTESIAN_POINT('',(212.588527625411,555.8971072385,-35.0221601717612)) ;
#72960 = CARTESIAN_POINT('',(199.088527625411,555.897107238499,-35.0221601717606)) ;
#72961 = CARTESIAN_POINT('',(201.838527625411,555.897107238497,-35.0221601717607)) ;
#72962 = CARTESIAN_POINT('',(199.088527625411,555.761830595002,-27.2721664563906)) ;
#72963 = CARTESIAN_POINT('Origin',(197.838527625413,564.222556589213,-25.0221601717605)) ;
#72964 = CARTESIAN_POINT('',(199.088527625412,564.048005939932,-35.0221601717606)) ;
#72965 = CARTESIAN_POINT('',(199.088527625412,564.048005939932,-35.0221601717606)) ;
#72966 = CARTESIAN_POINT('',(201.838527625412,564.04800593993,-35.0221601717607)) ;
#72967 = CARTESIAN_POINT('',(212.588527625413,564.18328258344,-27.2721664559512)) ;
#72968 = CARTESIAN_POINT('Origin',(197.838527625413,565.449472433283,-38.0221601717606)) ;
#72969 = CARTESIAN_POINT('',(212.588527625413,565.3971072385,-35.0221601717612)) ;
#72970 = CARTESIAN_POINT('',(199.088527625413,565.397107238499,-35.0221601717606)) ;
#72971 = CARTESIAN_POINT('',(201.838527625413,565.397107238497,-35.0221601717607)) ;
#72972 = CARTESIAN_POINT('',(199.088527625413,565.261830595002,-27.2721664563906)) ;
#72973 = CARTESIAN_POINT('Origin',(197.838527625414,573.495640745153,-38.0221601717606)) ;
#72974 = CARTESIAN_POINT('',(199.088527625414,573.548005939932,-35.0221601717606)) ;
#72975 = CARTESIAN_POINT('',(199.088527625414,573.548005939932,-35.0221601717606)) ;
#72976 = CARTESIAN_POINT('',(201.838527625414,573.548005939937,-35.0221601717607)) ;
#72977 = CARTESIAN_POINT('',(212.588527625415,573.68328258344,-27.2721664559512)) ;
#72978 = CARTESIAN_POINT('Origin',(197.838527625415,574.722556589213,-25.0221601717605)) ;
#72979 = CARTESIAN_POINT('',(212.588527625414,574.8971072385,-35.0221601717612)) ;
#72980 = CARTESIAN_POINT('',(199.088527625414,574.897107238499,-35.0221601717606)) ;
#72981 = CARTESIAN_POINT('',(201.838527625414,574.897107238494,-35.0221601717607)) ;
#72982 = CARTESIAN_POINT('',(199.088527625415,574.761830594102,-27.2721664048106)) ;
#72983 = CARTESIAN_POINT('Origin',(197.838527625416,582.995640745153,-38.0221601717605)) ;
#72984 = CARTESIAN_POINT('',(199.088527625416,583.048005939932,-35.0221601717606)) ;
#72985 = CARTESIAN_POINT('',(199.088527625416,583.048005939932,-35.0221601717606)) ;
#72986 = CARTESIAN_POINT('',(201.838527625416,583.048005939937,-35.0221601717607)) ;
#72987 = CARTESIAN_POINT('',(212.588527625416,583.18328258344,-27.2721664559512)) ;
#72988 = CARTESIAN_POINT('Origin',(197.838527625416,584.222556589213,-25.0221601717606)) ;
#72989 = CARTESIAN_POINT('',(212.588527625416,584.3971072385,-35.0221601717612)) ;
#72990 = CARTESIAN_POINT('',(199.088527625416,584.3971072385,-35.0221601717606)) ;
#72991 = CARTESIAN_POINT('',(201.838527625416,584.397107238494,-35.0221601717607)) ;
#72992 = CARTESIAN_POINT('',(199.088527625416,584.261830594102,-27.2721664048106)) ;
#72993 = CARTESIAN_POINT('Origin',(197.838527625417,592.495640745153,-38.0221601717606)) ;
#72994 = CARTESIAN_POINT('',(199.088527625417,592.548005939932,-35.0221601717606)) ;
#72995 = CARTESIAN_POINT('',(199.088527625417,592.548005939932,-35.0221601717606)) ;
#72996 = CARTESIAN_POINT('',(201.838527625417,592.548005939937,-35.0221601717607)) ;
#72997 = CARTESIAN_POINT('',(212.588527625418,592.68328258344,-27.2721664559512)) ;
#72998 = CARTESIAN_POINT('Origin',(197.838527625418,593.722556589213,-25.0221601717605)) ;
#72999 = CARTESIAN_POINT('',(212.588527625418,593.8971072385,-35.0221601717612)) ;
#73000 = CARTESIAN_POINT('',(199.088527625418,593.8971072385,-35.0221601717606)) ;
#73001 = CARTESIAN_POINT('',(201.838527625418,593.897107238494,-35.0221601717607)) ;
#73002 = CARTESIAN_POINT('',(199.088527625418,593.761830594102,-27.2721664048106)) ;
#73003 = CARTESIAN_POINT('Origin',(197.838527625419,601.995640745153,-38.0221601717605)) ;
#73004 = CARTESIAN_POINT('',(199.088527625419,602.048005939932,-35.0221601717606)) ;
#73005 = CARTESIAN_POINT('',(199.088527625419,602.048005939932,-35.0221601717606)) ;
#73006 = CARTESIAN_POINT('',(201.838527625419,602.048005939937,-35.0221601717607)) ;
#73007 = CARTESIAN_POINT('',(212.588527625419,602.18328258344,-27.2721664559512)) ;
#73008 = CARTESIAN_POINT('Origin',(197.83852762542,603.222556589213,-25.0221601717605)) ;
#73009 = CARTESIAN_POINT('',(212.588527625419,603.3971072385,-35.0221601717612)) ;
#73010 = CARTESIAN_POINT('',(199.088527625419,603.397107238499,-35.0221601717606)) ;
#73011 = CARTESIAN_POINT('',(201.838527625419,603.397107238494,-35.0221601717607)) ;
#73012 = CARTESIAN_POINT('',(199.08852762542,603.261830595002,-27.2721664563906)) ;
#73013 = CARTESIAN_POINT('Origin',(197.838527625421,611.495640745133,-38.0221601717605)) ;
#73014 = CARTESIAN_POINT('',(199.088527625421,611.548005939932,-35.0221601717606)) ;
#73015 = CARTESIAN_POINT('',(199.088527625421,611.548005939932,-35.0221601717606)) ;
#73016 = CARTESIAN_POINT('',(201.838527625421,611.548005939917,-35.0221601717607)) ;
#73017 = CARTESIAN_POINT('',(212.588527625421,611.68328258343,-27.2721664559512)) ;
#73018 = CARTESIAN_POINT('Origin',(199.088527625413,569.472556589217,-34.0221601717606)) ;
#73019 = CARTESIAN_POINT('Origin',(194.588527625414,569.472556589218,-34.0221601717604)) ;
#73020 = CARTESIAN_POINT('',(194.588527625421,612.748739186625,-26.5221601717604)) ;
#73021 = CARTESIAN_POINT('Origin',(199.088527625413,569.472556589217,-34.0221601717606)) ;
#73022 = CARTESIAN_POINT('',(199.08852762541,547.972556589222,-35.0221601717606)) ;
#73023 = CARTESIAN_POINT('Origin',(199.088527625413,569.472556589217,-34.0221601717606)) ;
#73024 = CARTESIAN_POINT('',(199.08852762541,547.972556589222,-35.0221601717606)) ;
#73025 = CARTESIAN_POINT('Origin',(199.088527625413,569.472556589217,-34.0221601717606)) ;
#73026 = CARTESIAN_POINT('',(199.08852762541,547.972556589222,-35.0221601717606)) ;
#73027 = CARTESIAN_POINT('Origin',(199.088527625413,569.472556589217,-34.0221601717606)) ;
#73028 = CARTESIAN_POINT('',(199.08852762541,547.972556589222,-35.0221601717606)) ;
#73029 = CARTESIAN_POINT('Origin',(199.088527625413,569.472556589217,-34.0221601717606)) ;
#73030 = CARTESIAN_POINT('',(199.08852762541,547.972556589222,-35.0221601717606)) ;
#73031 = CARTESIAN_POINT('Origin',(199.088527625413,569.472556589217,-34.0221601717606)) ;
#73032 = CARTESIAN_POINT('',(199.08852762541,547.972556589222,-35.0221601717606)) ;
#73033 = CARTESIAN_POINT('Origin',(199.088527625413,569.472556589217,-34.0221601717606)) ;
#73034 = CARTESIAN_POINT('',(199.08852762541,547.972556589222,-35.0221601717606)) ;
#73035 = CARTESIAN_POINT('Origin',(199.088527625413,569.472556589217,-34.0221601717606)) ;
#73036 = CARTESIAN_POINT('',(199.08852762541,547.972556589222,-35.0221601717606)) ;
#73037 = CARTESIAN_POINT('Origin',(205.838527625413,569.472556589231,-35.0221601717609)) ;
#73038 = CARTESIAN_POINT('',(203.155186246477,607.472556589211,-35.0221601717609)) ;
#73039 = CARTESIAN_POINT('Origin',(206.03852762542,607.472556589211,-35.0221601717609)) ;
#73040 = CARTESIAN_POINT('Origin',(206.03852762542,607.472556589211,-35.0982690928543)) ;
#73041 = CARTESIAN_POINT('',(208.89602762542,607.472556589211,-35.0982690928543)) ;
#73042 = CARTESIAN_POINT('',(203.18102762542,607.472556589211,-35.0982690928543)) ;
#73043 = CARTESIAN_POINT('Origin',(206.03852762542,607.472556589211,-35.0982690928543)) ;
#73044 = CARTESIAN_POINT('Origin',(206.03852762542,607.472556589211,-35.0982690928543)) ;
#73045 = CARTESIAN_POINT('Origin',(203.05602762542,607.472556589211,-35.0982690928543)) ;
#73046 = CARTESIAN_POINT('Origin',(206.03852762542,607.472556589211,-34.9732690928544)) ;
#73047 = CARTESIAN_POINT('',(208.89602762542,607.472556589211,-36.8802690928544)) ;
#73048 = CARTESIAN_POINT('Origin',(206.03852762542,607.472556589211,-36.8802690928544)) ;
#73049 = CARTESIAN_POINT('',(208.89602762542,607.472556589211,-34.9732690928544)) ;
#73050 = CARTESIAN_POINT('Origin',(206.03852762542,607.472556589211,-36.8802690928544)) ;
#73051 = CARTESIAN_POINT('Origin',(208.77102762542,607.472556589211,-36.8802690928544)) ;
#73052 = CARTESIAN_POINT('Origin',(206.038425919156,605.472556589211,-37.9581389501285)) ;
#73053 = CARTESIAN_POINT('',(201.55977762542,605.472556589211,-40.5297040214914)) ;
#73054 = CARTESIAN_POINT('Origin',(201.55977762542,605.597556589211,-40.5297040214914)) ;
#73055 = CARTESIAN_POINT('Origin',(205.838527625413,569.472556589231,-35.0221601717609)) ;
#73056 = CARTESIAN_POINT('',(203.155186246476,597.972556589211,-35.0221601717609)) ;
#73057 = CARTESIAN_POINT('Origin',(206.038527625418,597.972556589211,-35.0221601717609)) ;
#73058 = CARTESIAN_POINT('Origin',(206.038527625418,597.972556589211,-35.0982690928543)) ;
#73059 = CARTESIAN_POINT('',(208.896027625418,597.972556589211,-35.0982690928543)) ;
#73060 = CARTESIAN_POINT('',(203.181027625418,597.972556589211,-35.0982690928543)) ;
#73061 = CARTESIAN_POINT('Origin',(206.038527625418,597.972556589211,-35.0982690928543)) ;
#73062 = CARTESIAN_POINT('Origin',(206.038527625418,597.972556589211,-35.0982690928543)) ;
#73063 = CARTESIAN_POINT('Origin',(203.056027625418,597.972556589211,-35.0982690928543)) ;
#73064 = CARTESIAN_POINT('Origin',(206.038527625418,597.972556589211,-34.9732690928544)) ;
#73065 = CARTESIAN_POINT('',(208.896027625418,597.972556589211,-36.8802690928544)) ;
#73066 = CARTESIAN_POINT('Origin',(206.038527625418,597.972556589211,-36.8802690928544)) ;
#73067 = CARTESIAN_POINT('',(208.896027625418,597.972556589211,-34.9732690928544)) ;
#73068 = CARTESIAN_POINT('Origin',(206.038527625418,597.972556589211,-36.8802690928544)) ;
#73069 = CARTESIAN_POINT('Origin',(208.771027625418,597.972556589211,-36.8802690928544)) ;
#73070 = CARTESIAN_POINT('Origin',(206.038425919154,595.972556589211,-37.9581389501285)) ;
#73071 = CARTESIAN_POINT('',(201.559777625419,595.972556589211,-40.5297040214914)) ;
#73072 = CARTESIAN_POINT('Origin',(201.559777625419,596.097556589211,-40.5297040214914)) ;
#73073 = CARTESIAN_POINT('Origin',(205.838527625413,569.472556589231,-35.0221601717609)) ;
#73074 = CARTESIAN_POINT('',(203.155186246474,588.472556589211,-35.0221601717609)) ;
#73075 = CARTESIAN_POINT('Origin',(206.038527625417,588.472556589211,-35.0221601717609)) ;
#73076 = CARTESIAN_POINT('Origin',(206.038527625417,588.472556589211,-35.0982690928543)) ;
#73077 = CARTESIAN_POINT('',(208.896027625417,588.472556589211,-35.0982690928543)) ;
#73078 = CARTESIAN_POINT('',(203.181027625417,588.472556589211,-35.0982690928543)) ;
#73079 = CARTESIAN_POINT('Origin',(206.038527625417,588.472556589211,-35.0982690928543)) ;
#73080 = CARTESIAN_POINT('Origin',(206.038527625417,588.472556589211,-35.0982690928543)) ;
#73081 = CARTESIAN_POINT('Origin',(203.056027625417,588.472556589211,-35.0982690928543)) ;
#73082 = CARTESIAN_POINT('Origin',(206.038527625417,588.472556589211,-34.9732690928544)) ;
#73083 = CARTESIAN_POINT('',(208.896027625417,588.472556589211,-36.8802690928544)) ;
#73084 = CARTESIAN_POINT('Origin',(206.038527625417,588.472556589211,-36.8802690928544)) ;
#73085 = CARTESIAN_POINT('',(208.896027625417,588.472556589211,-34.9732690928544)) ;
#73086 = CARTESIAN_POINT('Origin',(206.038527625417,588.472556589211,-36.8802690928544)) ;
#73087 = CARTESIAN_POINT('Origin',(208.771027625417,588.472556589211,-36.8802690928544)) ;
#73088 = CARTESIAN_POINT('Origin',(206.038425919152,586.472556589211,-37.9581389501285)) ;
#73089 = CARTESIAN_POINT('',(201.559777625417,586.472556589211,-40.5297040214914)) ;
#73090 = CARTESIAN_POINT('Origin',(201.559777625417,586.597556589211,-40.5297040214914)) ;
#73091 = CARTESIAN_POINT('Origin',(205.838527625413,569.472556589231,-35.0221601717609)) ;
#73092 = CARTESIAN_POINT('',(203.155186246472,578.972556589211,-35.0221601717609)) ;
#73093 = CARTESIAN_POINT('Origin',(206.038527625415,578.972556589211,-35.0221601717609)) ;
#73094 = CARTESIAN_POINT('Origin',(206.038527625415,578.972556589211,-35.0982690928543)) ;
#73095 = CARTESIAN_POINT('',(208.896027625415,578.972556589211,-35.0982690928543)) ;
#73096 = CARTESIAN_POINT('',(203.181027625415,578.972556589211,-35.0982690928543)) ;
#73097 = CARTESIAN_POINT('Origin',(206.038527625415,578.972556589211,-35.0982690928543)) ;
#73098 = CARTESIAN_POINT('Origin',(206.038527625415,578.972556589211,-35.0982690928543)) ;
#73099 = CARTESIAN_POINT('Origin',(203.056027625415,578.972556589211,-35.0982690928543)) ;
#73100 = CARTESIAN_POINT('Origin',(206.038527625415,578.972556589211,-34.9732690928544)) ;
#73101 = CARTESIAN_POINT('',(208.896027625415,578.972556589211,-36.8802690928544)) ;
#73102 = CARTESIAN_POINT('Origin',(206.038527625415,578.972556589211,-36.8802690928544)) ;
#73103 = CARTESIAN_POINT('',(208.896027625415,578.972556589211,-34.9732690928544)) ;
#73104 = CARTESIAN_POINT('Origin',(206.038527625415,578.972556589211,-36.8802690928544)) ;
#73105 = CARTESIAN_POINT('Origin',(208.771027625415,578.972556589211,-36.8802690928544)) ;
#73106 = CARTESIAN_POINT('Origin',(206.038425919151,576.972556589211,-37.9581389501285)) ;
#73107 = CARTESIAN_POINT('',(201.559777625416,576.972556589211,-40.5297040214914)) ;
#73108 = CARTESIAN_POINT('Origin',(201.559777625415,577.097556589211,-40.5297040214914)) ;
#73109 = CARTESIAN_POINT('Origin',(205.838527625413,569.472556589231,-35.0221601717609)) ;
#73110 = CARTESIAN_POINT('',(203.155186246471,569.472556589211,-35.0221601717609)) ;
#73111 = CARTESIAN_POINT('Origin',(206.038527625413,569.472556589211,-35.0221601717609)) ;
#73112 = CARTESIAN_POINT('Origin',(206.038527625413,569.472556589211,-35.0982690928543)) ;
#73113 = CARTESIAN_POINT('',(208.896027625413,569.472556589211,-35.0982690928543)) ;
#73114 = CARTESIAN_POINT('',(203.181027625413,569.472556589211,-35.0982690928543)) ;
#73115 = CARTESIAN_POINT('Origin',(206.038527625413,569.472556589211,-35.0982690928543)) ;
#73116 = CARTESIAN_POINT('Origin',(206.038527625413,569.472556589211,-35.0982690928543)) ;
#73117 = CARTESIAN_POINT('Origin',(203.056027625413,569.472556589211,-35.0982690928543)) ;
#73118 = CARTESIAN_POINT('Origin',(206.038527625413,569.472556589211,-34.9732690928544)) ;
#73119 = CARTESIAN_POINT('',(208.896027625413,569.472556589211,-36.8802690928544)) ;
#73120 = CARTESIAN_POINT('Origin',(206.038527625413,569.472556589211,-36.8802690928544)) ;
#73121 = CARTESIAN_POINT('',(208.896027625413,569.472556589211,-34.9732690928544)) ;
#73122 = CARTESIAN_POINT('Origin',(206.038527625413,569.472556589211,-36.8802690928544)) ;
#73123 = CARTESIAN_POINT('Origin',(208.771027625413,569.472556589211,-36.8802690928544)) ;
#73124 = CARTESIAN_POINT('Origin',(206.038425919149,567.47255658921,-37.9581389501285)) ;
#73125 = CARTESIAN_POINT('',(201.559777625414,567.47255658921,-40.5297040214914)) ;
#73126 = CARTESIAN_POINT('Origin',(201.559777625414,567.59755658921,-40.5297040214914)) ;
#73127 = CARTESIAN_POINT('Origin',(205.838527625413,569.472556589231,-35.0221601717609)) ;
#73128 = CARTESIAN_POINT('',(203.155186246469,559.972556589211,-35.0221601717609)) ;
#73129 = CARTESIAN_POINT('Origin',(206.038527625412,559.972556589211,-35.0221601717609)) ;
#73130 = CARTESIAN_POINT('Origin',(206.038527625412,559.972556589211,-35.0982690928543)) ;
#73131 = CARTESIAN_POINT('',(208.896027625412,559.972556589211,-35.0982690928543)) ;
#73132 = CARTESIAN_POINT('',(203.181027625412,559.972556589211,-35.0982690928543)) ;
#73133 = CARTESIAN_POINT('Origin',(206.038527625412,559.972556589211,-35.0982690928543)) ;
#73134 = CARTESIAN_POINT('Origin',(206.038527625412,559.972556589211,-35.0982690928543)) ;
#73135 = CARTESIAN_POINT('Origin',(203.056027625412,559.972556589211,-35.0982690928543)) ;
#73136 = CARTESIAN_POINT('Origin',(206.038527625412,559.972556589211,-34.9732690928544)) ;
#73137 = CARTESIAN_POINT('',(208.896027625412,559.972556589211,-36.8802690928544)) ;
#73138 = CARTESIAN_POINT('Origin',(206.038527625412,559.972556589211,-36.8802690928544)) ;
#73139 = CARTESIAN_POINT('',(208.896027625412,559.972556589211,-34.9732690928544)) ;
#73140 = CARTESIAN_POINT('Origin',(206.038527625412,559.972556589211,-36.8802690928544)) ;
#73141 = CARTESIAN_POINT('Origin',(208.771027625412,559.972556589211,-36.8802690928544)) ;
#73142 = CARTESIAN_POINT('Origin',(206.038425919147,557.97255658921,-37.9581389501285)) ;
#73143 = CARTESIAN_POINT('',(201.559777625412,557.97255658921,-40.5297040214914)) ;
#73144 = CARTESIAN_POINT('Origin',(201.559777625412,558.097556589211,-40.5297040214914)) ;
#73145 = CARTESIAN_POINT('Origin',(205.838527625413,569.472556589231,-35.0221601717609)) ;
#73146 = CARTESIAN_POINT('',(203.155186246467,550.472556589211,-35.0221601717609)) ;
#73147 = CARTESIAN_POINT('Origin',(206.03852762541,550.472556589211,-35.0221601717609)) ;
#73148 = CARTESIAN_POINT('Origin',(206.03852762541,550.472556589211,-35.0982690928543)) ;
#73149 = CARTESIAN_POINT('',(208.89602762541,550.472556589211,-35.0982690928543)) ;
#73150 = CARTESIAN_POINT('',(203.18102762541,550.472556589211,-35.0982690928543)) ;
#73151 = CARTESIAN_POINT('Origin',(206.03852762541,550.472556589211,-35.0982690928543)) ;
#73152 = CARTESIAN_POINT('Origin',(206.03852762541,550.472556589211,-35.0982690928543)) ;
#73153 = CARTESIAN_POINT('Origin',(203.05602762541,550.472556589211,-35.0982690928543)) ;
#73154 = CARTESIAN_POINT('Origin',(206.03852762541,550.472556589211,-34.9732690928544)) ;
#73155 = CARTESIAN_POINT('',(208.89602762541,550.472556589211,-36.8802690928544)) ;
#73156 = CARTESIAN_POINT('Origin',(206.03852762541,550.472556589211,-36.8802690928544)) ;
#73157 = CARTESIAN_POINT('',(208.89602762541,550.472556589211,-34.9732690928544)) ;
#73158 = CARTESIAN_POINT('Origin',(206.03852762541,550.472556589211,-36.8802690928544)) ;
#73159 = CARTESIAN_POINT('Origin',(208.77102762541,550.472556589211,-36.8802690928544)) ;
#73160 = CARTESIAN_POINT('Origin',(206.038425919146,548.47255658921,-37.9581389501285)) ;
#73161 = CARTESIAN_POINT('',(201.55977762541,548.47255658921,-40.5297040214914)) ;
#73162 = CARTESIAN_POINT('Origin',(201.55977762541,548.59755658921,-40.5297040214914)) ;
#73163 = CARTESIAN_POINT('Origin',(205.838527625413,569.472556589231,-35.0221601717609)) ;
#73164 = CARTESIAN_POINT('',(203.155186246466,540.972556589211,-35.0221601717609)) ;
#73165 = CARTESIAN_POINT('Origin',(206.038527625408,540.972556589211,-35.0221601717609)) ;
#73166 = CARTESIAN_POINT('Origin',(206.038527625408,540.972556589211,-35.0982690928543)) ;
#73167 = CARTESIAN_POINT('',(208.896027625408,540.972556589211,-35.0982690928543)) ;
#73168 = CARTESIAN_POINT('',(203.181027625408,540.972556589211,-35.0982690928543)) ;
#73169 = CARTESIAN_POINT('Origin',(206.038527625408,540.972556589211,-35.0982690928543)) ;
#73170 = CARTESIAN_POINT('Origin',(206.038527625408,540.972556589211,-35.0982690928543)) ;
#73171 = CARTESIAN_POINT('Origin',(203.056027625408,540.972556589211,-35.0982690928543)) ;
#73172 = CARTESIAN_POINT('Origin',(206.038527625408,540.972556589211,-34.9732690928544)) ;
#73173 = CARTESIAN_POINT('',(208.896027625408,540.972556589211,-36.8802690928544)) ;
#73174 = CARTESIAN_POINT('Origin',(206.038527625408,540.972556589211,-36.8802690928544)) ;
#73175 = CARTESIAN_POINT('',(208.896027625408,540.972556589211,-34.9732690928544)) ;
#73176 = CARTESIAN_POINT('Origin',(206.038527625408,540.972556589211,-36.8802690928544)) ;
#73177 = CARTESIAN_POINT('Origin',(208.771027625408,540.972556589211,-36.8802690928544)) ;
#73178 = CARTESIAN_POINT('Origin',(206.038425919144,538.97255658921,-37.9581389501285)) ;
#73179 = CARTESIAN_POINT('',(201.559777625409,538.97255658921,-40.5297040214914)) ;
#73180 = CARTESIAN_POINT('Origin',(201.559777625409,539.09755658921,-40.5297040214914)) ;
#73181 = CARTESIAN_POINT('Origin',(206.038527625407,531.472556589211,-35.0982690928543)) ;
#73182 = CARTESIAN_POINT('',(208.896027625407,531.472556589211,-35.0982690928543)) ;
#73183 = CARTESIAN_POINT('',(203.181027625407,531.472556589211,-35.0982690928543)) ;
#73184 = CARTESIAN_POINT('Origin',(206.038527625407,531.472556589211,-35.0982690928543)) ;
#73185 = CARTESIAN_POINT('Origin',(206.038527625407,531.472556589211,-35.0982690928543)) ;
#73186 = CARTESIAN_POINT('Origin',(203.056027625407,531.472556589211,-35.0982690928543)) ;
#73187 = CARTESIAN_POINT('Origin',(206.038527625407,531.472556589211,-34.9732690928544)) ;
#73188 = CARTESIAN_POINT('',(208.896027625407,531.472556589211,-36.8802690928544)) ;
#73189 = CARTESIAN_POINT('Origin',(206.038527625407,531.472556589211,-36.8802690928544)) ;
#73190 = CARTESIAN_POINT('',(208.896027625407,531.472556589211,-34.9732690928544)) ;
#73191 = CARTESIAN_POINT('Origin',(206.038527625407,531.472556589211,-36.8802690928544)) ;
#73192 = CARTESIAN_POINT('Origin',(208.771027625407,531.472556589211,-36.8802690928544)) ;
#73193 = CARTESIAN_POINT('Origin',(197.838527625421,612.722556589233,-25.0221601717606)) ;
#73194 = CARTESIAN_POINT('',(212.588527625421,613.01056516053,-41.5221601717612)) ;
#73195 = CARTESIAN_POINT('Origin',(212.588527625406,526.47255658921,-35.0221601717612)) ;
#73196 = CARTESIAN_POINT('Origin',(209.81477762542,609.347556589211,-38.5610190928544)) ;
#73197 = CARTESIAN_POINT('',(209.68977762542,609.347556589211,-38.5610190928544)) ;
#73198 = CARTESIAN_POINT('Origin',(209.68977762542,602.868806589211,-43.1012690928544)) ;
#73199 = CARTESIAN_POINT('',(209.68977762542,605.597556589211,-40.5297040214914)) ;
#73200 = CARTESIAN_POINT('Origin',(209.81477762542,605.597556589211,-40.5297040214914)) ;
#73201 = CARTESIAN_POINT('',(209.81477762542,605.472556589211,-40.5297040214914)) ;
#73202 = CARTESIAN_POINT('Origin',(206.038425919156,605.472556589211,-37.9581389501285)) ;
#73203 = CARTESIAN_POINT('Origin',(201.55977762542,609.347556589211,-38.5610190928544)) ;
#73204 = CARTESIAN_POINT('Origin',(209.814777625418,599.847556589211,-38.5610190928544)) ;
#73205 = CARTESIAN_POINT('',(209.689777625418,599.847556589211,-38.5610190928544)) ;
#73206 = CARTESIAN_POINT('Origin',(209.689777625418,593.368806589211,-43.1012690928544)) ;
#73207 = CARTESIAN_POINT('',(209.689777625418,596.097556589211,-40.5297040214914)) ;
#73208 = CARTESIAN_POINT('Origin',(209.814777625418,596.097556589211,-40.5297040214914)) ;
#73209 = CARTESIAN_POINT('',(209.814777625418,595.972556589211,-40.5297040214914)) ;
#73210 = CARTESIAN_POINT('Origin',(206.038425919154,595.972556589211,-37.9581389501285)) ;
#73211 = CARTESIAN_POINT('Origin',(201.559777625419,599.847556589211,-38.5610190928544)) ;
#73212 = CARTESIAN_POINT('Origin',(209.814777625417,590.347556589211,-38.5610190928544)) ;
#73213 = CARTESIAN_POINT('',(209.689777625417,590.347556589211,-38.5610190928544)) ;
#73214 = CARTESIAN_POINT('Origin',(209.689777625417,583.868806589211,-43.1012690928544)) ;
#73215 = CARTESIAN_POINT('',(209.689777625417,586.597556589211,-40.5297040214914)) ;
#73216 = CARTESIAN_POINT('Origin',(209.814777625417,586.597556589211,-40.5297040214914)) ;
#73217 = CARTESIAN_POINT('',(209.814777625417,586.472556589211,-40.5297040214914)) ;
#73218 = CARTESIAN_POINT('Origin',(206.038425919152,586.472556589211,-37.9581389501285)) ;
#73219 = CARTESIAN_POINT('Origin',(201.559777625417,590.347556589211,-38.5610190928544)) ;
#73220 = CARTESIAN_POINT('Origin',(209.814777625415,580.847556589211,-38.5610190928544)) ;
#73221 = CARTESIAN_POINT('',(209.689777625415,580.847556589211,-38.5610190928544)) ;
#73222 = CARTESIAN_POINT('Origin',(209.689777625415,574.368806589211,-43.1012690928544)) ;
#73223 = CARTESIAN_POINT('',(209.689777625415,577.097556589211,-40.5297040214914)) ;
#73224 = CARTESIAN_POINT('Origin',(209.814777625415,577.097556589211,-40.5297040214914)) ;
#73225 = CARTESIAN_POINT('',(209.814777625415,576.972556589211,-40.5297040214914)) ;
#73226 = CARTESIAN_POINT('Origin',(206.038425919151,576.972556589211,-37.9581389501285)) ;
#73227 = CARTESIAN_POINT('Origin',(201.559777625415,580.847556589211,-38.5610190928544)) ;
#73228 = CARTESIAN_POINT('Origin',(209.814777625413,571.347556589211,-38.5610190928544)) ;
#73229 = CARTESIAN_POINT('',(209.689777625413,571.347556589211,-38.5610190928544)) ;
#73230 = CARTESIAN_POINT('Origin',(209.689777625413,564.868806589211,-43.1012690928544)) ;
#73231 = CARTESIAN_POINT('',(209.689777625413,567.59755658921,-40.5297040214914)) ;
#73232 = CARTESIAN_POINT('Origin',(209.814777625413,567.59755658921,-40.5297040214914)) ;
#73233 = CARTESIAN_POINT('',(209.814777625413,567.47255658921,-40.5297040214914)) ;
#73234 = CARTESIAN_POINT('Origin',(206.038425919149,567.47255658921,-37.9581389501285)) ;
#73235 = CARTESIAN_POINT('Origin',(201.559777625414,571.347556589211,-38.5610190928544)) ;
#73236 = CARTESIAN_POINT('Origin',(209.814777625412,561.847556589211,-38.5610190928544)) ;
#73237 = CARTESIAN_POINT('',(209.689777625412,561.847556589211,-38.5610190928544)) ;
#73238 = CARTESIAN_POINT('Origin',(209.689777625412,555.368806589211,-43.1012690928544)) ;
#73239 = CARTESIAN_POINT('',(209.689777625412,558.097556589211,-40.5297040214914)) ;
#73240 = CARTESIAN_POINT('Origin',(209.814777625412,558.097556589211,-40.5297040214914)) ;
#73241 = CARTESIAN_POINT('',(209.814777625412,557.97255658921,-40.5297040214914)) ;
#73242 = CARTESIAN_POINT('Origin',(206.038425919147,557.97255658921,-37.9581389501285)) ;
#73243 = CARTESIAN_POINT('Origin',(201.559777625412,561.847556589211,-38.5610190928544)) ;
#73244 = CARTESIAN_POINT('Origin',(209.81477762541,552.347556589211,-38.5610190928544)) ;
#73245 = CARTESIAN_POINT('',(209.68977762541,552.347556589211,-38.5610190928544)) ;
#73246 = CARTESIAN_POINT('Origin',(209.68977762541,545.868806589211,-43.1012690928544)) ;
#73247 = CARTESIAN_POINT('',(209.68977762541,548.59755658921,-40.5297040214914)) ;
#73248 = CARTESIAN_POINT('Origin',(209.81477762541,548.59755658921,-40.5297040214914)) ;
#73249 = CARTESIAN_POINT('',(209.81477762541,548.47255658921,-40.5297040214914)) ;
#73250 = CARTESIAN_POINT('Origin',(206.038425919146,548.47255658921,-37.9581389501285)) ;
#73251 = CARTESIAN_POINT('Origin',(201.55977762541,552.347556589211,-38.5610190928544)) ;
#73252 = CARTESIAN_POINT('Origin',(209.814777625408,542.847556589211,-38.5610190928544)) ;
#73253 = CARTESIAN_POINT('',(209.689777625408,542.847556589211,-38.5610190928544)) ;
#73254 = CARTESIAN_POINT('Origin',(209.689777625408,536.368806589211,-43.1012690928544)) ;
#73255 = CARTESIAN_POINT('',(209.689777625408,539.09755658921,-40.5297040214914)) ;
#73256 = CARTESIAN_POINT('Origin',(209.814777625408,539.09755658921,-40.5297040214914)) ;
#73257 = CARTESIAN_POINT('',(209.814777625408,538.97255658921,-40.5297040214914)) ;
#73258 = CARTESIAN_POINT('Origin',(206.038425919144,538.97255658921,-37.9581389501285)) ;
#73259 = CARTESIAN_POINT('Origin',(201.559777625409,542.847556589211,-38.5610190928544)) ;
#73260 = CARTESIAN_POINT('',(0.,0.,0.)) ;
#73261 = CARTESIAN_POINT('',(0.,0.,0.)) ;
#73262 = CARTESIAN_POINT('Origin',(3.10601593664312E-15,-2.12330153459561E-14,
-0.34726562499997)) ;
#73263 = CARTESIAN_POINT('',(8.51359053417684E-13,-1.23704425180947,5.55625000000022)) ;
#73264 = CARTESIAN_POINT('',(3.44719424660001E-14,-1.23704425180958,5.65546875)) ;
#73265 = CARTESIAN_POINT('',(6.06053764494801E-15,-1.23704425180962,-0.347265624999939)) ;
#73266 = CARTESIAN_POINT('',(-1.23064526020309,-0.123127494296425,6.16388000977423)) ;
#73267 = CARTESIAN_POINT('Ctrl Pts',(1.63466462588189E-12,-1.23704425180947,
5.55625000000022)) ;
#73268 = CARTESIAN_POINT('Ctrl Pts',(0.032410535193708,-1.23704425180947,
5.55938790945648)) ;
#73269 = CARTESIAN_POINT('Ctrl Pts',(0.06485156327478,-1.23577059586982,5.56257984877948)) ;
#73270 = CARTESIAN_POINT('Ctrl Pts',(0.261554273988151,-1.22025878337805,
5.58224620102718)) ;
#73271 = CARTESIAN_POINT('Ctrl Pts',(0.421583054731985,-1.17459990755325,
5.59957086456626)) ;
#73272 = CARTESIAN_POINT('Ctrl Pts',(0.709312921724199,-1.02590447288471,
5.63339132862922)) ;
#73273 = CARTESIAN_POINT('Ctrl Pts',(0.835234563292027,-0.926268012883034,
5.64889464075713)) ;
#73274 = CARTESIAN_POINT('Ctrl Pts',(1.0461788342556,-0.680415129648602,5.68115705137086)) ;
#73275 = CARTESIAN_POINT('Ctrl Pts',(1.12741507524917,-0.535130549153963,
5.69848098170242)) ;
#73276 = CARTESIAN_POINT('Ctrl Pts',(1.22646116995911,-0.226717318521629,
5.73231286381708)) ;
#73277 = CARTESIAN_POINT('Ctrl Pts',(1.24541854129917,-0.0672584313812708,
5.74783986629028)) ;
#73278 = CARTESIAN_POINT('Ctrl Pts',(1.22147882786804,0.255844813611181,5.78008199728177)) ;
#73279 = CARTESIAN_POINT('Ctrl Pts',(1.17654329196774,0.416157461096852,5.797405135899)) ;
#73280 = CARTESIAN_POINT('Ctrl Pts',(1.02911988768562,0.704643939698382,5.83124784083467)) ;
#73281 = CARTESIAN_POINT('Ctrl Pts',(0.930044054170639,0.831030132889457,
5.84679794267637)) ;
#73282 = CARTESIAN_POINT('Ctrl Pts',(0.685083752317439,1.04313900555543,5.8790206399247)) ;
#73283 = CARTESIAN_POINT('Ctrl Pts',(0.540097293143178,1.1250543206284,5.89634293988441)) ;
#73284 = CARTESIAN_POINT('Ctrl Pts',(0.232033318192428,1.2254691170157,5.93019589716347)) ;
#73285 = CARTESIAN_POINT('Ctrl Pts',(0.0726391820466259,1.24511793858861,
5.94576847016992)) ;
#73286 = CARTESIAN_POINT('Ctrl Pts',(-0.2506458377757,1.22256553715424,5.97797256457448)) ;
#73287 = CARTESIAN_POINT('Ctrl Pts',(-0.411213940163794,1.17828945821474,
5.99529398941272)) ;
#73288 = CARTESIAN_POINT('Ctrl Pts',(-0.700386660668012,1.03202510449678,
6.02915665304384)) ;
#73289 = CARTESIAN_POINT('Ctrl Pts',(-0.827195214883551,0.93345884249799,
6.04475103884394)) ;
#73290 = CARTESIAN_POINT('Ctrl Pts',(-1.04036027204184,0.689311906417811,
6.07693734431807)) ;
#73291 = CARTESIAN_POINT('Ctrl Pts',(-1.12289141919012,0.544598890120713,
6.09425786700923)) ;
#73292 = CARTESIAN_POINT('Ctrl Pts',(-1.20198911794031,0.305149566984994,
6.1206128371872)) ;
#73293 = CARTESIAN_POINT('Ctrl Pts',(-1.22052187953621,0.219605249836496,
6.12963825279501)) ;
#73294 = CARTESIAN_POINT('Ctrl Pts',(-1.23907720793799,0.0477697380486169,
6.14701907770368)) ;
#73295 = CARTESIAN_POINT('Ctrl Pts',(-1.2394166269485,-0.0379502076343803,
6.15514160739101)) ;
#73296 = CARTESIAN_POINT('Ctrl Pts',(-1.23090852815641,-0.123055581940823,
6.1637225050298)) ;
#73297 = CARTESIAN_POINT('',(-1.18366931688486,-0.359039527537319,6.28795132031109)) ;
#73298 = CARTESIAN_POINT('Ctrl Pts',(-1.23090128330268,-0.123128029703915,
6.1637298109973)) ;
#73299 = CARTESIAN_POINT('Ctrl Pts',(-1.22220034015823,-0.210110677832008,
6.17250309915399)) ;
#73300 = CARTESIAN_POINT('Ctrl Pts',(-1.20583575204488,-0.280578131537651,
6.18520779853968)) ;
#73301 = CARTESIAN_POINT('Ctrl Pts',(-1.18696998481902,-0.349039280868321,
6.20671103290821)) ;
#73302 = CARTESIAN_POINT('Ctrl Pts',(-1.18180835795257,-0.365742807077991,
6.21365128674509)) ;
#73303 = CARTESIAN_POINT('Ctrl Pts',(-1.17619838945325,-0.383234137286321,
6.22434464445792)) ;
#73304 = CARTESIAN_POINT('Ctrl Pts',(-1.17433885136118,-0.388879457581289,
6.22846304369811)) ;
#73305 = CARTESIAN_POINT('Ctrl Pts',(-1.17208930685934,-0.395590250986855,
6.23599150360299)) ;
#73306 = CARTESIAN_POINT('Ctrl Pts',(-1.17136121561512,-0.39773526410404,
6.23910049969088)) ;
#73307 = CARTESIAN_POINT('Ctrl Pts',(-1.17059733480713,-0.399976624072225,
6.24494531778126)) ;
#73308 = CARTESIAN_POINT('Ctrl Pts',(-1.17042655012746,-0.400474933454289,
6.24743652302402)) ;
#73309 = CARTESIAN_POINT('Ctrl Pts',(-1.17044238937348,-0.400428638657382,
6.25245242249197)) ;
#73310 = CARTESIAN_POINT('Ctrl Pts',(-1.17060894530179,-0.399942487518192,
6.25480649215178)) ;
#73311 = CARTESIAN_POINT('Ctrl Pts',(-1.17128204467748,-0.397967653749609,
6.2600343415439)) ;
#73312 = CARTESIAN_POINT('Ctrl Pts',(-1.17186577386847,-0.39624915385918,
6.26274945420801)) ;
#73313 = CARTESIAN_POINT('Ctrl Pts',(-1.17375333330537,-0.390635890342859,
6.26967799482782)) ;
#73314 = CARTESIAN_POINT('Ctrl Pts',(-1.17535164607556,-0.385813073064476,
6.27358482212547)) ;
#73315 = CARTESIAN_POINT('Ctrl Pts',(-1.17890754325678,-0.374831481607947,
6.28103038015207)) ;
#73316 = CARTESIAN_POINT('Ctrl Pts',(-1.1811438609383,-0.367736459238746,
6.28473131480161)) ;
#73317 = CARTESIAN_POINT('Ctrl Pts',(-1.1832560635873,-0.36080960203242,6.28787103703615)) ;
#73318 = CARTESIAN_POINT('Ctrl Pts',(-1.51494228338223E-16,-1.23704425180958,
5.65546875)) ;
#73319 = CARTESIAN_POINT('Ctrl Pts',(0.512400506355205,-1.23704425180958,
5.705078125)) ;
#73320 = CARTESIAN_POINT('Ctrl Pts',(0.874722379082391,-0.874722379082391,
5.7546875)) ;
#73321 = CARTESIAN_POINT('Ctrl Pts',(1.23704425180958,-0.512400506355206,
5.804296875)) ;
#73322 = CARTESIAN_POINT('Ctrl Pts',(1.23704425180958,-2.27241342507335E-16,
5.85390625)) ;
#73323 = CARTESIAN_POINT('Ctrl Pts',(1.23704425180958,0.512400506355206,5.903515625)) ;
#73324 = CARTESIAN_POINT('Ctrl Pts',(0.874722379082391,0.874722379082391,
5.953125)) ;
#73325 = CARTESIAN_POINT('Ctrl Pts',(0.512400506355206,1.23704425180958,6.002734375)) ;
#73326 = CARTESIAN_POINT('Ctrl Pts',(0.,1.23704425180958,6.05234375)) ;
#73327 = CARTESIAN_POINT('Ctrl Pts',(-0.512400506355205,1.23704425180958,
6.101953125)) ;
#73328 = CARTESIAN_POINT('Ctrl Pts',(-0.874722379082391,0.874722379082391,
6.1515625)) ;
#73329 = CARTESIAN_POINT('Ctrl Pts',(-1.23704425180958,0.512400506355205,
6.201171875)) ;
#73330 = CARTESIAN_POINT('Ctrl Pts',(-1.23704425180958,7.57471141691116E-17,
6.25078125)) ;
#73331 = CARTESIAN_POINT('Ctrl Pts',(-1.23704425180958,-0.183204766505095,
6.26851869141665)) ;
#73332 = CARTESIAN_POINT('Ctrl Pts',(-1.18394409959329,-0.358545464304532,
6.28762423629624)) ;
#73333 = CARTESIAN_POINT('Origin',(3.10601593664312E-15,-2.12330153459561E-14,
-0.34726562499997)) ;
#73334 = CARTESIAN_POINT('',(9.19078401434668E-13,-1.23704425180949,4.76250000000022)) ;
#73335 = CARTESIAN_POINT('',(4.35160472637051E-13,-1.23704425180949,4.86171875000003)) ;
#73336 = CARTESIAN_POINT('',(6.06053764494801E-15,-1.23704425180962,-0.347265624999939)) ;
#73337 = CARTESIAN_POINT('Ctrl Pts',(1.77843850757079E-12,-1.23704425180949,
4.76250000000022)) ;
#73338 = CARTESIAN_POINT('Ctrl Pts',(0.0421386522123601,-1.23704425180949,
4.76657976216588)) ;
#73339 = CARTESIAN_POINT('Ctrl Pts',(0.0843179104865776,-1.23489139653225,
4.77074979199699)) ;
#73340 = CARTESIAN_POINT('Ctrl Pts',(0.289955684198697,-1.21377252576669,
4.79150607610251)) ;
#73341 = CARTESIAN_POINT('Ctrl Pts',(0.448520280260818,-1.16452899411383,
4.80883273683123)) ;
#73342 = CARTESIAN_POINT('Ctrl Pts',(0.732438679409685,-1.00951739173385,
4.84253748205696)) ;
#73343 = CARTESIAN_POINT('Ctrl Pts',(0.85603735041666,-0.907074834681463,
4.85783713510419)) ;
#73344 = CARTESIAN_POINT('Ctrl Pts',(1.06111293017096,-0.656791531698224,
4.890293135197)) ;
#73345 = CARTESIAN_POINT('Ctrl Pts',(1.13892739263001,-0.510058436740854,
4.90762008307935)) ;
#73346 = CARTESIAN_POINT('Ctrl Pts',(1.23110405460236,-0.199936799080401,
4.94134188310875)) ;
#73347 = CARTESIAN_POINT('Ctrl Pts',(1.24658404004136,-0.0401507195947445,
4.95666762906366)) ;
#73348 = CARTESIAN_POINT('Ctrl Pts',(1.2156625882264,0.281988156101469,4.98909638188065)) ;
#73349 = CARTESIAN_POINT('Ctrl Pts',(1.16742238571045,0.440972297818764,5.00642342534077)) ;
#73350 = CARTESIAN_POINT('Ctrl Pts',(1.01418089980775,0.725968107940733,5.04016149563328)) ;
#73351 = CARTESIAN_POINT('Ctrl Pts',(0.912528610844644,0.850220582311041,
5.05551334297379)) ;
#73352 = CARTESIAN_POINT('Ctrl Pts',(0.663486603667513,1.05695544741248,5.08791570638977)) ;
#73353 = CARTESIAN_POINT('Ctrl Pts',(0.517153989968506,1.13573725453211,5.10524267421844)) ;
#73354 = CARTESIAN_POINT('Ctrl Pts',(0.207506710452891,1.22985149951979,5.13899625123036)) ;
#73355 = CARTESIAN_POINT('Ctrl Pts',(0.0478133168613316,1.24631356321518,
5.15437410194347)) ;
#73356 = CARTESIAN_POINT('Ctrl Pts',(-0.274606409922473,1.21736453792499,
5.18675094555916)) ;
#73357 = CARTESIAN_POINT('Ctrl Pts',(-0.433973118519662,1.17005549056148,
5.20407768595966)) ;
#73358 = CARTESIAN_POINT('Ctrl Pts',(-0.719961390303868,1.01845516294561,
5.23784602836267)) ;
#73359 = CARTESIAN_POINT('Ctrl Pts',(-0.844818078053866,0.917532851082596,
5.25324968710869)) ;
#73360 = CARTESIAN_POINT('Ctrl Pts',(-1.05308115417194,0.669641964324695,
5.28560188791629)) ;
#73361 = CARTESIAN_POINT('Ctrl Pts',(-1.13275399505154,0.523684505045508,
5.30292826746668)) ;
#73362 = CARTESIAN_POINT('Ctrl Pts',(-1.22865598812913,0.214480137870498,
5.33671065711472)) ;
#73363 = CARTESIAN_POINT('Ctrl Pts',(-1.24602329086207,0.0548719765320699,
5.35213984046059)) ;
#73364 = CARTESIAN_POINT('Ctrl Pts',(-1.2188919644099,-0.267800701702066,
5.38446827876781)) ;
#73365 = CARTESIAN_POINT('Ctrl Pts',(-1.172442762695,-0.427514916174963,5.4017941813232)) ;
#73366 = CARTESIAN_POINT('Ctrl Pts',(-1.02235660958171,-0.714413388720673,
5.43558992398581)) ;
#73367 = CARTESIAN_POINT('Ctrl Pts',(-0.922105525992712,-0.83982589633167,
5.45104426958003)) ;
#73368 = CARTESIAN_POINT('Ctrl Pts',(-0.67527687879584,-1.04949031574621,
5.48334982521286)) ;
#73369 = CARTESIAN_POINT('Ctrl Pts',(-0.52966876539888,-1.12998027012065,
5.50067515076929)) ;
#73370 = CARTESIAN_POINT('Ctrl Pts',(-0.251874491965004,-1.21773217371334,
5.53108964699106)) ;
#73371 = CARTESIAN_POINT('Ctrl Pts',(-0.126242819055568,-1.23704425180948,
5.54402747626354)) ;
#73372 = CARTESIAN_POINT('Ctrl Pts',(1.6324094853637E-12,-1.23704425180947,
5.55625000000022)) ;
#73373 = CARTESIAN_POINT('Ctrl Pts',(1.55431223447522E-12,-1.23704425180947,
5.65546875000009)) ;
#73374 = CARTESIAN_POINT('Ctrl Pts',(-0.152484622127137,-1.23704425180965,
5.64070555849834)) ;
#73375 = CARTESIAN_POINT('Ctrl Pts',(-0.303785698542382,-1.20885031199389,
5.62492628913784)) ;
#73376 = CARTESIAN_POINT('Ctrl Pts',(-0.589144297891564,-1.09848368938504,
5.5928725116777)) ;
#73377 = CARTESIAN_POINT('Ctrl Pts',(-0.720593565085903,-1.01711877777539,
5.57688292274652)) ;
#73378 = CARTESIAN_POINT('Ctrl Pts',(-0.951469283805133,-0.80643673920516,
5.54608108124321)) ;
#73379 = CARTESIAN_POINT('Ctrl Pts',(-1.04730480818369,-0.677363204564986,
5.53022106353388)) ;
#73380 = CARTESIAN_POINT('Ctrl Pts',(-1.18731261688945,-0.38453773123282,
5.49625565641034)) ;
#73381 = CARTESIAN_POINT('Ctrl Pts',(-1.22802379686505,-0.22264310855874,
5.47894876478225)) ;
#73382 = CARTESIAN_POINT('Ctrl Pts',(-1.24310775880187,0.101564705464852,
5.44695483565233)) ;
#73383 = CARTESIAN_POINT('Ctrl Pts',(-1.21973263319505,0.260611300944475,
5.43110524505445)) ;
#73384 = CARTESIAN_POINT('Ctrl Pts',(-1.1119278562886,0.566738642807326,5.3971434263766)) ;
#73385 = CARTESIAN_POINT('Ctrl Pts',(-1.02636294861819,0.71006129721331,5.37983585179094)) ;
#73386 = CARTESIAN_POINT('Ctrl Pts',(-0.807993422942662,0.950145843994516,
5.34783414140409)) ;
#73387 = CARTESIAN_POINT('Ctrl Pts',(-0.679088552550741,1.04618462062345,
5.33199553059705)) ;
#73388 = CARTESIAN_POINT('Ctrl Pts',(-0.386533477579363,1.18666069086128,
5.29803752402347)) ;
#73389 = CARTESIAN_POINT('Ctrl Pts',(-0.224735086010386,1.22763894321764,
5.28072923881316)) ;
#73390 = CARTESIAN_POINT('Ctrl Pts',(0.0994070490296592,1.24328068929504,
5.24871929966044)) ;
#73391 = CARTESIAN_POINT('Ctrl Pts',(0.258479555860714,1.22018413326961,5.23289224202295)) ;
#73392 = CARTESIAN_POINT('Ctrl Pts',(0.56475485011669,1.11293256584222,5.19893828439744)) ;
#73393 = CARTESIAN_POINT('Ctrl Pts',(0.708205206869946,1.0276398336734,5.18162926107586)) ;
#73394 = CARTESIAN_POINT('Ctrl Pts',(0.948658049494458,0.809737369586976,
5.14961062382056)) ;
#73395 = CARTESIAN_POINT('Ctrl Pts',(1.04492481020587,0.681021673583593,5.13379571305975)) ;
#73396 = CARTESIAN_POINT('Ctrl Pts',(1.18592563438713,0.388770188997297,5.09984605508362)) ;
#73397 = CARTESIAN_POINT('Ctrl Pts',(1.22720313449488,0.227080222725434,5.08253626656936)) ;
#73398 = CARTESIAN_POINT('Ctrl Pts',(1.24347018371378,-0.096987662505879,
5.05050843947551)) ;
#73399 = CARTESIAN_POINT('Ctrl Pts',(1.22068586068575,-0.256089223457063,
5.03470628906358)) ;
#73400 = CARTESIAN_POINT('Ctrl Pts',(1.11405421863357,-0.562529739913569,
5.0007611959873)) ;
#73401 = CARTESIAN_POINT('Ctrl Pts',(1.02906669016739,-0.706122595938415,
4.98345061586245)) ;
#73402 = CARTESIAN_POINT('Ctrl Pts',(0.811687924735941,-0.94698751559422,
4.95141308427514)) ;
#73403 = CARTESIAN_POINT('Ctrl Pts',(0.683184093978087,-1.04350962700163,
4.93562432666935)) ;
#73404 = CARTESIAN_POINT('Ctrl Pts',(0.391273003367663,-1.18509758235805,
4.90168407900147)) ;
#73405 = CARTESIAN_POINT('Ctrl Pts',(0.229705083936882,-1.22670984317707,
4.88437268180648)) ;
#73406 = CARTESIAN_POINT('Ctrl Pts',(0.0431281364359357,-1.2364808339211,
4.86591690646213)) ;
#73407 = CARTESIAN_POINT('Ctrl Pts',(0.0215559159419141,-1.23704425180949,
4.86380574153132)) ;
#73408 = CARTESIAN_POINT('Ctrl Pts',(8.09560751768692E-13,-1.23704425180949,
4.86171875000003)) ;
#73409 = CARTESIAN_POINT('Origin',(3.10601593664312E-15,-2.12330153459561E-14,
-0.34726562499997)) ;
#73410 = CARTESIAN_POINT('',(5.32647143441161E-13,-1.23704425180951,3.96875000000014)) ;
#73411 = CARTESIAN_POINT('',(6.23963519277181E-13,-1.23704425180951,4.06796875000008)) ;
#73412 = CARTESIAN_POINT('',(6.06053764494801E-15,-1.23704425180962,-0.347265624999939)) ;
#73413 = CARTESIAN_POINT('Ctrl Pts',(1.0139111772387E-12,-1.23704425180951,
3.96875000000014)) ;
#73414 = CARTESIAN_POINT('Ctrl Pts',(0.0551038756713428,-1.23704425180951,
3.97408502367433)) ;
#73415 = CARTESIAN_POINT('Ctrl Pts',(0.110249673505602,-1.23336321992724,
3.97957172713591)) ;
#73416 = CARTESIAN_POINT('Ctrl Pts',(0.327554666791744,-1.20410203287067,
4.00178413571668)) ;
#73417 = CARTESIAN_POINT('Ctrl Pts',(0.484045790880615,-1.15014797873887,
4.01909895471897)) ;
#73418 = CARTESIAN_POINT('Ctrl Pts',(0.762789740117514,-0.986797807279728,
4.05263712515903)) ;
#73419 = CARTESIAN_POINT('Ctrl Pts',(0.883277688017725,-0.880589329049968,
4.06774382098912)) ;
#73420 = CARTESIAN_POINT('Ctrl Pts',(1.08038014525501,-0.624463865032571,
4.1004456975994)) ;
#73421 = CARTESIAN_POINT('Ctrl Pts',(1.15354966053906,-0.475904993799031,
4.11776313568763)) ;
#73422 = CARTESIAN_POINT('Ctrl Pts',(1.2364656378473,-0.163597807609727,4.15132515257324)) ;
#73423 = CARTESIAN_POINT('Ctrl Pts',(1.24723638954917,-0.00336380386512913,
4.16645308780335)) ;
#73424 = CARTESIAN_POINT('Ctrl Pts',(1.20685407023023,0.317335284596847,4.19912185452807)) ;
#73425 = CARTESIAN_POINT('Ctrl Pts',(1.15417636174644,0.474405368821141,4.21644154156241)) ;
#73426 = CARTESIAN_POINT('Ctrl Pts',(0.993090564161647,0.754570831146914,
4.25002653092196)) ;
#73427 = CARTESIAN_POINT('Ctrl Pts',(0.887912031932113,0.875908694415663,
4.26517683476727)) ;
#73428 = CARTESIAN_POINT('Ctrl Pts',(0.633372016242751,1.07520220942914,4.29781308043887)) ;
#73429 = CARTESIAN_POINT('Ctrl Pts',(0.485298711297695,1.14964745804084,4.31513466810497)) ;
#73430 = CARTESIAN_POINT('Ctrl Pts',(0.173576773798556,1.23510024408959,4.34874175666028)) ;
#73431 = CARTESIAN_POINT('Ctrl Pts',(0.0134663297023445,1.24716370540185,
4.36391540060311)) ;
#73432 = CARTESIAN_POINT('Ctrl Pts',(-0.307643328469588,1.20937850104566,
4.39651976519306)) ;
#73433 = CARTESIAN_POINT('Ctrl Pts',(-0.465251840947688,1.15791401095084,
4.41384292766305)) ;
#73434 = CARTESIAN_POINT('Ctrl Pts',(-0.746754901463488,0.998977011960021,
4.44747124643818)) ;
#73435 = CARTESIAN_POINT('Ctrl Pts',(-0.868895668647008,0.894770740285789,
4.46266904680359)) ;
#73436 = CARTESIAN_POINT('Ctrl Pts',(-1.07025040888213,0.641736004836289,
4.49524221652169)) ;
#73437 = CARTESIAN_POINT('Ctrl Pts',(-1.14589635909296,0.494130644689081,
4.51256665082678)) ;
#73438 = CARTESIAN_POINT('Ctrl Pts',(-1.2337411814112,0.182969856561674,4.54621533845682)) ;
#73439 = CARTESIAN_POINT('Ctrl Pts',(-1.24702165966823,0.0229753121996063,
4.56143796044876)) ;
#73440 = CARTESIAN_POINT('Ctrl Pts',(-1.21168159833801,-0.298510265502198,
4.59398066271132)) ;
#73441 = CARTESIAN_POINT('Ctrl Pts',(-1.16136280242387,-0.456616720778517,
4.61130608884694)) ;
#73442 = CARTESIAN_POINT('Ctrl Pts',(-1.00445201492435,-0.739371046092404,
4.64497429457722)) ;
#73443 = CARTESIAN_POINT('Ctrl Pts',(-0.90115810133007,-0.862265756220849,
4.66022225759696)) ;
#73444 = CARTESIAN_POINT('Ctrl Pts',(-0.649543364335466,-1.06554826071117,
4.69273525593167)) ;
#73445 = CARTESIAN_POINT('Ctrl Pts',(-0.502385483457626,-1.14231757247314,
4.7100614167188)) ;
#73446 = CARTESIAN_POINT('Ctrl Pts',(-0.232372718583162,-1.22062577891459,
4.7393438041112)) ;
#73447 = CARTESIAN_POINT('Ctrl Pts',(-0.116404738713934,-1.2370442518095,
4.75122997535534)) ;
#73448 = CARTESIAN_POINT('Ctrl Pts',(1.7786640216233E-12,-1.23704425180949,
4.76250000000022)) ;
#73449 = CARTESIAN_POINT('Ctrl Pts',(8.09612793473136E-13,-1.23704425180949,
4.86171875000003)) ;
#73450 = CARTESIAN_POINT('Ctrl Pts',(-0.137336915342943,-1.23704425180949,
4.8484221227521)) ;
#73451 = CARTESIAN_POINT('Ctrl Pts',(-0.273837360267966,-1.21418534140677,
4.83428976615802)) ;
#73452 = CARTESIAN_POINT('Ctrl Pts',(-0.560037656867374,-1.11530384903455,
4.80261508754638)) ;
#73453 = CARTESIAN_POINT('Ctrl Pts',(-0.703789186902301,-1.03065804248177,
4.7853028491147)) ;
#73454 = CARTESIAN_POINT('Ctrl Pts',(-0.945114351967411,-0.813865590204942,
4.75324427068868)) ;
#73455 = CARTESIAN_POINT('Ctrl Pts',(-1.04192199729811,-0.685598645235772,
4.73748426662642)) ;
#73456 = CARTESIAN_POINT('Ctrl Pts',(-1.18416571355528,-0.39406863303059,
4.70355461596626)) ;
#73457 = CARTESIAN_POINT('Ctrl Pts',(-1.22615178933585,-0.232637942704037,
4.6862415138019)) ;
#73458 = CARTESIAN_POINT('Ctrl Pts',(-1.24390083882174,0.0912513448628287,
4.65417154521747)) ;
#73459 = CARTESIAN_POINT('Ctrl Pts',(-1.22185629281801,0.250421796258092,
4.63842693364645)) ;
#73460 = CARTESIAN_POINT('Ctrl Pts',(-1.11669285766411,0.557251204171017,
4.60450306876804)) ;
#73461 = CARTESIAN_POINT('Ctrl Pts',(-1.03242901230166,0.701179000912871,
4.58718908246915)) ;
#73462 = CARTESIAN_POINT('Ctrl Pts',(-0.816291860310908,0.943017192844111,
4.5551071136332)) ;
#73463 = CARTESIAN_POINT('Ctrl Pts',(-0.68828928793283,1.0401435395084,4.53937858989549)) ;
#73464 = CARTESIAN_POINT('Ctrl Pts',(-0.397185174831524,1.18311822243788,
4.50546085968587)) ;
#73465 = CARTESIAN_POINT('Ctrl Pts',(-0.23590859250982,1.22552088559737,4.48814597141756)) ;
#73466 = CARTESIAN_POINT('Ctrl Pts',(0.0878738572500918,1.24414215332276,
4.45605136790905)) ;
#73467 = CARTESIAN_POINT('Ctrl Pts',(0.247084876853158,1.22253285185974,4.44033963824566)) ;
#73468 = CARTESIAN_POINT('Ctrl Pts',(0.554141397167057,1.11823283162416,4.40642841055572)) ;
#73469 = CARTESIAN_POINT('Ctrl Pts',(0.69826448734219,1.03439511621537,4.38911260557476)) ;
#73470 = CARTESIAN_POINT('Ctrl Pts',(0.94067327944826,0.818988981154981,4.35700470869683)) ;
#73471 = CARTESIAN_POINT('Ctrl Pts',(1.03815462345547,0.691280851097263,4.34131048759468)) ;
#73472 = CARTESIAN_POINT('Ctrl Pts',(1.18194231219858,0.400651824203295,4.30740614998345)) ;
#73473 = CARTESIAN_POINT('Ctrl Pts',(1.22480819038543,0.23954806056204,4.29008941721771)) ;
#73474 = CARTESIAN_POINT('Ctrl Pts',(1.24440011555374,-0.0841139884145471,
4.25796754419715)) ;
#73475 = CARTESIAN_POINT('Ctrl Pts',(1.22327506160333,-0.243370178118099,
4.24229155132392)) ;
#73476 = CARTESIAN_POINT('Ctrl Pts',(1.11993530837595,-0.550677908791383,
4.20839451179072)) ;
#73477 = CARTESIAN_POINT('Ctrl Pts',(1.03657199420482,-0.695016737891022,
4.19107684447547)) ;
#73478 = CARTESIAN_POINT('Ctrl Pts',(0.821979619332609,-0.938058608442367,
4.15894028882639)) ;
#73479 = CARTESIAN_POINT('Ctrl Pts',(0.694598672019677,-1.03593448500254,
4.14328324552636)) ;
#73480 = CARTESIAN_POINT('Ctrl Pts',(0.404498475654644,-1.18062421707747,
4.10939393322327)) ;
#73481 = CARTESIAN_POINT('Ctrl Pts',(0.243588203023662,-1.22400387511481,
4.09207532959614)) ;
#73482 = CARTESIAN_POINT('Ctrl Pts',(0.052584724229101,-1.23620676325144,
4.07309346146815)) ;
#73483 = CARTESIAN_POINT('Ctrl Pts',(0.026281115687445,-1.23704425180951,
4.07051322391713)) ;
#73484 = CARTESIAN_POINT('Ctrl Pts',(1.19550203070388E-12,-1.23704425180951,
4.06796875000008)) ;
#73485 = CARTESIAN_POINT('Origin',(3.10601593664312E-15,-2.12330153459561E-14,
-0.34726562499997)) ;
#73486 = CARTESIAN_POINT('',(8.58475084835609E-14,-1.23704425180953,3.17500000000004)) ;
#73487 = CARTESIAN_POINT('',(8.50687621102125E-13,-1.23704425180953,3.27421875000013)) ;
#73488 = CARTESIAN_POINT('',(6.06053764494801E-15,-1.23704425180962,-0.347265624999939)) ;
#73489 = CARTESIAN_POINT('Ctrl Pts',(1.28647092978432E-13,-1.23704425180953,
3.17500000000004)) ;
#73490 = CARTESIAN_POINT('Ctrl Pts',(0.0708155775454666,-1.23704425180953,
3.18185619256565)) ;
#73491 = CARTESIAN_POINT('Ctrl Pts',(0.141641158011715,-1.23096580307423,
3.18895711854993)) ;
#73492 = CARTESIAN_POINT('Ctrl Pts',(0.37265237290927,-1.19083439746923,3.21293246032262)) ;
#73493 = CARTESIAN_POINT('Ctrl Pts',(0.526449006731497,-1.13128370789566,
3.23021084803643)) ;
#73494 = CARTESIAN_POINT('Ctrl Pts',(0.798776567960535,-0.9579519766928,3.26352809136088)) ;
#73495 = CARTESIAN_POINT('Ctrl Pts',(0.915468185958332,-0.847133187399626,
3.27852390399491)) ;
#73496 = CARTESIAN_POINT('Ctrl Pts',(1.10267389299613,-0.584031316057481,
3.31150432856375)) ;
#73497 = CARTESIAN_POINT('Ctrl Pts',(1.1700919079108,-0.433429567785851,3.32878889975524)) ;
#73498 = CARTESIAN_POINT('Ctrl Pts',(1.24162311102855,-0.118621376363251,
3.3621364925631)) ;
#73499 = CARTESIAN_POINT('Ctrl Pts',(1.24656360713669,0.0421759060016317,
3.37713911282345)) ;
#73500 = CARTESIAN_POINT('Ctrl Pts',(1.19447652746202,0.360879175517894,3.41008404699193)) ;
#73501 = CARTESIAN_POINT('Ctrl Pts',(1.136381222018,0.515401389867704,3.42737431816112)) ;
#73502 = CARTESIAN_POINT('Ctrl Pts',(0.965654131201204,0.789427315205592,
3.46075153868974)) ;
#73503 = CARTESIAN_POINT('Ctrl Pts',(0.856049877773158,0.907117744817803,
3.475763232627)) ;
#73504 = CARTESIAN_POINT('Ctrl Pts',(0.594766231382718,1.09694412949167,3.5086727184997)) ;
#73505 = CARTESIAN_POINT('Ctrl Pts',(0.444681672071364,1.16588309277448,3.52596821153494)) ;
#73506 = CARTESIAN_POINT('Ctrl Pts',(0.13051322723977,1.24041746774059,3.55937430228894)) ;
#73507 = CARTESIAN_POINT('Ctrl Pts',(-0.0301340284081215,1.24690081458028,
3.57439722434183)) ;
#73508 = CARTESIAN_POINT('Ctrl Pts',(-0.349388372826032,1.19790902522301,
3.6072713813451)) ;
#73509 = CARTESIAN_POINT('Ctrl Pts',(-0.504603592915391,1.14123807328055,
3.62457162658369)) ;
#73510 = CARTESIAN_POINT('Ctrl Pts',(-0.780270998401231,0.973053725356881,
3.65800579923392)) ;
#73511 = CARTESIAN_POINT('Ctrl Pts',(-0.898930809787884,0.864627154576215,
3.67304197956894)) ;
#73512 = CARTESIAN_POINT('Ctrl Pts',(-1.09128935018277,0.605120146751677,
3.70588100303067)) ;
#73513 = CARTESIAN_POINT('Ctrl Pts',(-1.16169940902439,0.455551501636983,
3.72318554207434)) ;
#73514 = CARTESIAN_POINT('Ctrl Pts',(-1.23914333848065,0.142016544828403,
3.75664698236262)) ;
#73515 = CARTESIAN_POINT('Ctrl Pts',(-1.24711798196723,-0.0184863590425373,
3.77169831613014)) ;
#73516 = CARTESIAN_POINT('Ctrl Pts',(-1.20111976828371,-0.338257695483038,
3.80450247522439)) ;
#73517 = CARTESIAN_POINT('Ctrl Pts',(-1.14583216279305,-0.494130023229818,
3.82181086347906)) ;
#73518 = CARTESIAN_POINT('Ctrl Pts',(-0.980111709808021,-0.771372658155629,
3.85529873606951)) ;
#73519 = CARTESIAN_POINT('Ctrl Pts',(-0.872819008504264,-0.890966611339828,
3.87036697465867)) ;
#73520 = CARTESIAN_POINT('Ctrl Pts',(-0.615034927641384,-1.08575441832947,
3.90313660975835)) ;
#73521 = CARTESIAN_POINT('Ctrl Pts',(-0.465976295817607,-1.15757703751633,
3.92044841867519)) ;
#73522 = CARTESIAN_POINT('Ctrl Pts',(-0.206659226669885,-1.2240756405299,
3.94822167239887)) ;
#73523 = CARTESIAN_POINT('Ctrl Pts',(-0.103453804072554,-1.23704425180952,
3.95873385345504)) ;
#73524 = CARTESIAN_POINT('Ctrl Pts',(1.01420608022984E-12,-1.23704425180951,
3.96875000000014)) ;
#73525 = CARTESIAN_POINT('Ctrl Pts',(1.19626530903361E-12,-1.23704425180951,
4.06796875000008)) ;
#73526 = CARTESIAN_POINT('Ctrl Pts',(-0.132492712536078,-1.23704425180951,
4.05514112672582)) ;
#73527 = CARTESIAN_POINT('Ctrl Pts',(-0.264250786478305,-1.2157711313891,
4.04153151017354)) ;
#73528 = CARTESIAN_POINT('Ctrl Pts',(-0.546829425379681,-1.1218114770952,
4.01040485290746)) ;
#73529 = CARTESIAN_POINT('Ctrl Pts',(-0.691405803061307,-1.03897506036924,
3.99308531696321)) ;
#73530 = CARTESIAN_POINT('Ctrl Pts',(-0.935148161467304,-0.825286427283299,
3.9609171846732)) ;
#73531 = CARTESIAN_POINT('Ctrl Pts',(-1.03346140934947,-0.698268122235989,
3.94530019093328)) ;
#73532 = CARTESIAN_POINT('Ctrl Pts',(-1.17914926345779,-0.408755192718701,
3.9114277085422)) ;
#73533 = CARTESIAN_POINT('Ctrl Pts',(-1.22309721265908,-0.248061163883425,
3.89410725084768)) ;
#73534 = CARTESIAN_POINT('Ctrl Pts',(-1.24496001774116,0.075313000626321,
3.8619221806586)) ;
#73535 = CARTESIAN_POINT('Ctrl Pts',(-1.22496742029096,0.234674977830744,
3.84632626845864)) ;
#73536 = CARTESIAN_POINT('Ctrl Pts',(-1.1238718134627,0.542564131407952,3.81246293431581)) ;
#73537 = CARTESIAN_POINT('Ctrl Pts',(-1.04161906937166,0.687401129125714,
3.79514157288443)) ;
#73538 = CARTESIAN_POINT('Ctrl Pts',(-0.828931494713476,0.931916231594316,
3.76293877098675)) ;
#73539 = CARTESIAN_POINT('Ctrl Pts',(-0.702314007776924,1.03071299719022,
3.74736462375802)) ;
#73540 = CARTESIAN_POINT('Ctrl Pts',(-0.41345153282745,1.17750198072219,3.71351095803971)) ;
#73541 = CARTESIAN_POINT('Ctrl Pts',(-0.252998681415089,1.22207659623042,
3.69618871926384)) ;
#73542 = CARTESIAN_POINT('Ctrl Pts',(0.0702044827112899,1.24525680135152,
3.66396737302194)) ;
#73543 = CARTESIAN_POINT('Ctrl Pts',(0.22962791148717,1.22592090736459,3.64841565102641)) ;
#73544 = CARTESIAN_POINT('Ctrl Pts',(0.537850340219543,1.12612564725782,3.61457219799452)) ;
#73545 = CARTESIAN_POINT('Ctrl Pts',(0.682972132674095,1.04451759575679,3.59724911763267)) ;
#73546 = CARTESIAN_POINT('Ctrl Pts',(0.928336862229866,0.83293567962328,3.5650083972929)) ;
#73547 = CARTESIAN_POINT('Ctrl Pts',(1.02766652798706,0.706759836179155,3.54947973110837)) ;
#73548 = CARTESIAN_POINT('Ctrl Pts',(1.17566627400191,0.418615717276284,3.51564705948802)) ;
#73549 = CARTESIAN_POINT('Ctrl Pts',(1.22092959963284,0.258431230748975,3.49832318370233)) ;
#73550 = CARTESIAN_POINT('Ctrl Pts',(1.24555959704839,-0.0645803549285124,
3.46606224437914)) ;
#73551 = CARTESIAN_POINT('Ctrl Pts',(1.22694620073508,-0.224071489051609,
3.45055722787517)) ;
#73552 = CARTESIAN_POINT('Ctrl Pts',(1.12858066702693,-0.532657284147546,
3.41673593112935)) ;
#73553 = CARTESIAN_POINT('Ctrl Pts',(1.04768242874002,-0.678088926833233,
3.39941131756716)) ;
#73554 = CARTESIAN_POINT('Ctrl Pts',(0.837317818847695,-0.924384412258899,
3.36712930151868)) ;
#73555 = CARTESIAN_POINT('Ctrl Pts',(0.711626949645792,-1.02429943344021,
3.35164848434463)) ;
#73556 = CARTESIAN_POINT('Ctrl Pts',(0.424273643956393,-1.17362567149252,
3.31783918082949)) ;
#73557 = CARTESIAN_POINT('Ctrl Pts',(0.264386998566793,-1.21964309144324,
3.30051389974086)) ;
#73558 = CARTESIAN_POINT('Ctrl Pts',(0.0667888724753224,-1.23569338185853,
3.28073926088402)) ;
#73559 = CARTESIAN_POINT('Ctrl Pts',(0.0333785908521117,-1.23704425180953,
3.27745038425878)) ;
#73560 = CARTESIAN_POINT('Ctrl Pts',(1.65728542000869E-12,-1.23704425180953,
3.27421875000013)) ;
#73561 = CARTESIAN_POINT('Origin',(3.10601593664312E-15,-2.12330153459561E-14,
-0.34726562499997)) ;
#73562 = CARTESIAN_POINT('',(-3.53216841023252E-15,-1.23704425180955,2.38125000000001)) ;
#73563 = CARTESIAN_POINT('',(9.61945429429848E-13,-1.23704425180955,2.48046875000017)) ;
#73564 = CARTESIAN_POINT('',(6.06053764494801E-15,-1.23704425180962,-0.347265624999939)) ;
#73565 = CARTESIAN_POINT('Ctrl Pts',(-4.17770751542265E-14,-1.23704425180955,
2.38125000000001)) ;
#73566 = CARTESIAN_POINT('Ctrl Pts',(0.087742059255656,-1.23704425180956,
2.38974497349614)) ;
#73567 = CARTESIAN_POINT('Ctrl Pts',(0.175397924138452,-1.22771444679764,
2.39860575646061)) ;
#73568 = CARTESIAN_POINT('Ctrl Pts',(0.421086846657427,-1.17456748660854,
2.42452412308534)) ;
#73569 = CARTESIAN_POINT('Ctrl Pts',(0.572236413054084,-1.1088156553442,2.44179491348184)) ;
#73570 = CARTESIAN_POINT('Ctrl Pts',(0.837308815849046,-0.924484441545288,
2.47485084388711)) ;
#73571 = CARTESIAN_POINT('Ctrl Pts',(0.949454964634233,-0.808883391388236,
2.48984013351775)) ;
#73572 = CARTESIAN_POINT('Ctrl Pts',(1.12561252818267,-0.538418100523992,
2.52309040112664)) ;
#73573 = CARTESIAN_POINT('Ctrl Pts',(1.18673778075662,-0.385426693580367,
2.54035397366693)) ;
#73574 = CARTESIAN_POINT('Ctrl Pts',(1.24545581479387,-0.06796089209204,2.57344502135837)) ;
#73575 = CARTESIAN_POINT('Ctrl Pts',(1.24382461226767,0.0931604792678681,
2.58843515795435)) ;
#73576 = CARTESIAN_POINT('Ctrl Pts',(1.17870954711358,0.409287181349732,2.6216530984053)) ;
#73577 = CARTESIAN_POINT('Ctrl Pts',(1.11454847343287,0.560941616284452,2.63890897455499)) ;
#73578 = CARTESIAN_POINT('Ctrl Pts',(0.93296551076449,0.827874944272307,2.67203486169088)) ;
#73579 = CARTESIAN_POINT('Ctrl Pts',(0.818402498915292,0.941285688546151,
2.68702840287109)) ;
#73580 = CARTESIAN_POINT('Ctrl Pts',(0.549717127143605,1.12011507343048,2.7202134914879)) ;
#73581 = CARTESIAN_POINT('Ctrl Pts',(0.397504367741431,1.18272460810127,2.73746120165276)) ;
#73582 = CARTESIAN_POINT('Ctrl Pts',(0.0806781569248627,1.24471548612111,
2.77062157708896)) ;
#73583 = CARTESIAN_POINT('Ctrl Pts',(-0.0806045211311646,1.24472025715767,
2.78562110233823)) ;
#73584 = CARTESIAN_POINT('Ctrl Pts',(-0.397356001307769,1.182763456008,2.81877287594506)) ;
#73585 = CARTESIAN_POINT('Ctrl Pts',(-0.549502376681443,1.12020880515138,
2.8360119579552)) ;
#73586 = CARTESIAN_POINT('Ctrl Pts',(-0.818295898471779,0.941404839217002,
2.86920649801463)) ;
#73587 = CARTESIAN_POINT('Ctrl Pts',(-0.932980086154937,0.827888629057569,
2.88421439790037)) ;
#73588 = CARTESIAN_POINT('Ctrl Pts',(-1.11448302604523,0.561002038877481,
2.9173325508293)) ;
#73589 = CARTESIAN_POINT('Ctrl Pts',(-1.1785728542988,0.409585276593328,2.93456255892281)) ;
#73590 = CARTESIAN_POINT('Ctrl Pts',(-1.2438453660056,0.0934176447806062,
2.96779077619432)) ;
#73591 = CARTESIAN_POINT('Ctrl Pts',(-1.24549236720236,-0.0680239283704382,
2.98280961579441)) ;
#73592 = CARTESIAN_POINT('Ctrl Pts',(-1.18669605779163,-0.385386507512381,
3.01589380883778)) ;
#73593 = CARTESIAN_POINT('Ctrl Pts',(-1.12575095674432,-0.538007783822041,
3.03311432158302)) ;
#73594 = CARTESIAN_POINT('Ctrl Pts',(-0.949994588684741,-0.808247851089063,
3.06632669438506)) ;
#73595 = CARTESIAN_POINT('Ctrl Pts',(-0.837932363556729,-0.923917822393809,
3.08131606252068)) ;
#73596 = CARTESIAN_POINT('Ctrl Pts',(-0.57298402990398,-1.1084310914558,3.11436728184243)) ;
#73597 = CARTESIAN_POINT('Ctrl Pts',(-0.421868558518369,-1.17428838114891,
3.13163900045812)) ;
#73598 = CARTESIAN_POINT('Ctrl Pts',(-0.175938483935532,-1.22765667322761,
3.1575895909478)) ;
#73599 = CARTESIAN_POINT('Ctrl Pts',(-0.0880134335085121,-1.23704425180953,
3.16647875270654)) ;
#73600 = CARTESIAN_POINT('Ctrl Pts',(1.28647092978432E-13,-1.23704425180953,
3.17500000000004)) ;
#73601 = CARTESIAN_POINT('Ctrl Pts',(1.65839564303383E-12,-1.23704425180953,
3.27421875000013)) ;
#73602 = CARTESIAN_POINT('Ctrl Pts',(-0.125259306880064,-1.23704425180953,
3.26209144752812)) ;
#73603 = CARTESIAN_POINT('Ctrl Pts',(-0.249926036900973,-1.21803207403063,
3.24925906863424)) ;
#73604 = CARTESIAN_POINT('Ctrl Pts',(-0.526956071082114,-1.1312423725868,
3.21895715154446)) ;
#73605 = CARTESIAN_POINT('Ctrl Pts',(-0.672723207759457,-1.05112289247697,
3.2016312869256)) ;
#73606 = CARTESIAN_POINT('Ctrl Pts',(-0.920034257456585,-0.842093826970192,
3.16930450594698)) ;
#73607 = CARTESIAN_POINT('Ctrl Pts',(-1.02058989133647,-0.716933533450121,
3.15387351926058)) ;
#73608 = CARTESIAN_POINT('Ctrl Pts',(-1.17136365853769,-0.430447751260752,
3.12009015678486)) ;
#73609 = CARTESIAN_POINT('Ctrl Pts',(-1.21820341668262,-0.270890696784831,
3.10276380753511)) ;
#73610 = CARTESIAN_POINT('Ctrl Pts',(-1.24615994228965,0.0516678432709414,
3.07041332672158)) ;
#73611 = CARTESIAN_POINT('Ctrl Pts',(-1.22920362688226,0.211314677528755,
3.05500784135146)) ;
#73612 = CARTESIAN_POINT('Ctrl Pts',(-1.13411349407752,0.520720804939624,
3.0212384759232)) ;
#73613 = CARTESIAN_POINT('Ctrl Pts',(-1.05484511114142,0.666849301455023,
3.00391175700099)) ;
#73614 = CARTESIAN_POINT('Ctrl Pts',(-0.847275704032822,0.915263631919053,
2.971536695957)) ;
#73615 = CARTESIAN_POINT('Ctrl Pts',(-0.722693521263278,1.01651754484435,
2.95615700125366)) ;
#73616 = CARTESIAN_POINT('Ctrl Pts',(-0.437155755641923,1.16886410870982,
2.92240234933873)) ;
#73617 = CARTESIAN_POINT('Ctrl Pts',(-0.277962236505721,1.21659665948755,
2.90507539289976)) ;
#73618 = CARTESIAN_POINT('Ctrl Pts',(0.0443306516715813,1.24644225330239,
2.87267487426566)) ;
#73619 = CARTESIAN_POINT('Ctrl Pts',(0.204066149164751,1.23042661911412,2.85732117214245)) ;
#73620 = CARTESIAN_POINT('Ctrl Pts',(0.513929854356582,1.13719340528694,2.82358197344859)) ;
#73621 = CARTESIAN_POINT('Ctrl Pts',(0.660445358989949,1.05885124898515,2.80625492994689)) ;
#73622 = CARTESIAN_POINT('Ctrl Pts',(0.912420921808995,0.850916104331233,
2.77352041178961)) ;
#73623 = CARTESIAN_POINT('Ctrl Pts',(1.0159735026812,0.724138380107633,2.75788120679066)) ;
#73624 = CARTESIAN_POINT('Ctrl Pts',(1.16792566570418,0.438487516909866,2.72413142175986)) ;
#73625 = CARTESIAN_POINT('Ctrl Pts',(1.21512293691003,0.282521136875137,2.70713837550492)) ;
#73626 = CARTESIAN_POINT('Ctrl Pts',(1.24699068652411,-0.0393940197984395,
2.67469333309582)) ;
#73627 = CARTESIAN_POINT('Ctrl Pts',(1.23111986905087,-0.202210012834243,
2.65909118027089)) ;
#73628 = CARTESIAN_POINT('Ctrl Pts',(1.13766332112956,-0.511919195941446,
2.62535798562932)) ;
#73629 = CARTESIAN_POINT('Ctrl Pts',(1.06121309629516,-0.655885259419098,
2.60835364525798)) ;
#73630 = CARTESIAN_POINT('Ctrl Pts',(0.85698298817807,-0.906688869553548,
2.57588117636637)) ;
#73631 = CARTESIAN_POINT('Ctrl Pts',(0.731074505423473,-1.01096042603533,
2.56031628581112)) ;
#73632 = CARTESIAN_POINT('Ctrl Pts',(0.446585037301406,-1.16486864609059,
2.5266005001818)) ;
#73633 = CARTESIAN_POINT('Ctrl Pts',(0.29084157916395,-1.21317239258132,2.50958466353687)) ;
#73634 = CARTESIAN_POINT('Ctrl Pts',(0.0868667757727215,-1.23475935950554,
2.48897061205492)) ;
#73635 = CARTESIAN_POINT('Ctrl Pts',(0.0434117617253601,-1.23704425180955,
2.484671771543)) ;
#73636 = CARTESIAN_POINT('Ctrl Pts',(1.88813622231907E-12,-1.23704425180955,
2.48046875000017)) ;
#73637 = CARTESIAN_POINT('Origin',(3.10601593664312E-15,-2.12330153459561E-14,
-0.34726562499997)) ;
#73638 = CARTESIAN_POINT('',(-4.44768360959499E-13,-1.23704425180957,1.58749999999992)) ;
#73639 = CARTESIAN_POINT('',(5.0368059013805E-13,-1.23704425180957,1.68671875000009)) ;
#73640 = CARTESIAN_POINT('',(6.06053764494801E-15,-1.23704425180962,-0.347265624999939)) ;
#73641 = CARTESIAN_POINT('Ctrl Pts',(-9.15951342550514E-13,-1.23704425180957,
1.58749999999992)) ;
#73642 = CARTESIAN_POINT('Ctrl Pts',(0.103213138457939,-1.23704425180965,
1.5974928458836)) ;
#73643 = CARTESIAN_POINT('Ctrl Pts',(0.20618093125318,-1.22413589226724,1.6079796039136)) ;
#73644 = CARTESIAN_POINT('Ctrl Pts',(0.465294526843657,-1.15784994931821,
1.63572462948155)) ;
#73645 = CARTESIAN_POINT('Ctrl Pts',(0.614386971854366,-1.08611976088681,
1.65303600534444)) ;
#73646 = CARTESIAN_POINT('Ctrl Pts',(0.872284307129058,-0.891490854380605,
1.68581023305133)) ;
#73647 = CARTESIAN_POINT('Ctrl Pts',(0.979651300418265,-0.771958131624264,
1.70087611594015)) ;
#73648 = CARTESIAN_POINT('Ctrl Pts',(1.1455336587961,-0.494818547234572,1.73436050434422)) ;
#73649 = CARTESIAN_POINT('Ctrl Pts',(1.20091225741019,-0.338988964280692,
1.75166840326281)) ;
#73650 = CARTESIAN_POINT('Ctrl Pts',(1.24710701030825,-0.019251089994797,
1.78447720447454)) ;
#73651 = CARTESIAN_POINT('Ctrl Pts',(1.23923025432837,0.141261268995484,1.79952640806237)) ;
#73652 = CARTESIAN_POINT('Ctrl Pts',(1.16197750256199,0.454838262952741,1.8329842514573)) ;
#73653 = CARTESIAN_POINT('Ctrl Pts',(1.09166402678993,0.604441255179057,1.85028824261942)) ;
#73654 = CARTESIAN_POINT('Ctrl Pts',(0.899471659306014,0.864065455998327,
1.88313194836513)) ;
#73655 = CARTESIAN_POINT('Ctrl Pts',(0.780875597126371,0.972569441935872,
1.89816624369074)) ;
#73656 = CARTESIAN_POINT('Ctrl Pts',(0.505315928503476,1.14092145152737,1.93159670928056)) ;
#73657 = CARTESIAN_POINT('Ctrl Pts',(0.350145937766151,1.19768642569191,1.94889634611048)) ;
#73658 = CARTESIAN_POINT('Ctrl Pts',(0.0309273791243574,1.24688212451289,
1.98177521583409)) ;
#73659 = CARTESIAN_POINT('Ctrl Pts',(-0.129729735598369,1.24050038649072,
1.996796516646)) ;
#73660 = CARTESIAN_POINT('Ctrl Pts',(-0.443940802185009,1.16616401538692,
2.03019879335581)) ;
#73661 = CARTESIAN_POINT('Ctrl Pts',(-0.594059940236127,1.09732525431576,
2.04749361579619)) ;
#73662 = CARTESIAN_POINT('Ctrl Pts',(-0.855463952527125,0.907671435081854,
2.08040783478537)) ;
#73663 = CARTESIAN_POINT('Ctrl Pts',(-0.965148313080044,0.7900469122298,2.09541818852656)) ;
#73664 = CARTESIAN_POINT('Ctrl Pts',(-1.13604775318347,0.516132835806172,
2.12879149186426)) ;
#73665 = CARTESIAN_POINT('Ctrl Pts',(-1.19423947770742,0.361658141632641,
2.14608102895431)) ;
#73666 = CARTESIAN_POINT('Ctrl Pts',(-1.24653657779848,0.0429928738521064,
2.17903070636778)) ;
#73667 = CARTESIAN_POINT('Ctrl Pts',(-1.24170080478482,-0.117814616829579,
2.1940322831697)) ;
#73668 = CARTESIAN_POINT('Ctrl Pts',(-1.17037318110268,-0.432665655153667,
2.22737586013345)) ;
#73669 = CARTESIAN_POINT('Ctrl Pts',(-1.10305835532869,-0.5833018986499,2.24465963285908)) ;
#73670 = CARTESIAN_POINT('Ctrl Pts',(-0.916030557171499,-0.846526450950797,
2.27764480039392)) ;
#73671 = CARTESIAN_POINT('Ctrl Pts',(-0.799406585624652,-0.957427536954876,
2.29263988016888)) ;
#73672 = CARTESIAN_POINT('Ctrl Pts',(-0.527194302150408,-1.13093510371108,
2.32595301414067)) ;
#73673 = CARTESIAN_POINT('Ctrl Pts',(-0.373447225065235,-1.19058390611551,
2.3432305385252)) ;
#73674 = CARTESIAN_POINT('Ctrl Pts',(-0.142197606895638,-1.23091787788555,
2.36723708546675)) ;
#73675 = CARTESIAN_POINT('Ctrl Pts',(-0.0710943025950748,-1.23704425180955,
2.3743668219507)) ;
#73676 = CARTESIAN_POINT('Ctrl Pts',(-4.17770751542265E-14,-1.23704425180955,
2.38125000000001)) ;
#73677 = CARTESIAN_POINT('Ctrl Pts',(1.88718832228041E-12,-1.23704425180955,
2.48046875000017)) ;
#73678 = CARTESIAN_POINT('Ctrl Pts',(-0.117854422562485,-1.23704425180955,
2.4690583704788)) ;
#73679 = CARTESIAN_POINT('Ctrl Pts',(-0.235259954172443,-1.22021429663736,
2.45701651722142)) ;
#73680 = CARTESIAN_POINT('Ctrl Pts',(-0.503742565535835,-1.14132347646503,
2.42785891093527)) ;
#73681 = CARTESIAN_POINT('Ctrl Pts',(-0.648352051565075,-1.06584880147738,
2.41083139857694)) ;
#73682 = CARTESIAN_POINT('Ctrl Pts',(-0.9005016509573,-0.863442817047236,
2.37830176737945)) ;
#73683 = CARTESIAN_POINT('Ctrl Pts',(-1.00554098541687,-0.738463663602721,
2.36281152285193)) ;
#73684 = CARTESIAN_POINT('Ctrl Pts',(-1.16153599988668,-0.45522443795177,
2.32913309563231)) ;
#73685 = CARTESIAN_POINT('Ctrl Pts',(-1.21102257045409,-0.299728136240724,
2.31209375309849)) ;
#73686 = CARTESIAN_POINT('Ctrl Pts',(-1.24737301964058,0.0215105103391086,
2.27953443836968)) ;
#73687 = CARTESIAN_POINT('Ctrl Pts',(-1.23390184302536,0.184098066882936,
2.26408130090388)) ;
#73688 = CARTESIAN_POINT('Ctrl Pts',(-1.14516389803635,0.494989647801575,
2.23042286022801)) ;
#73689 = CARTESIAN_POINT('Ctrl Pts',(-1.07073590685864,0.640278380071665,
2.21337156021615)) ;
#73690 = CARTESIAN_POINT('Ctrl Pts',(-0.870280527286828,0.893856283492051,
2.18078186949001)) ;
#73691 = CARTESIAN_POINT('Ctrl Pts',(-0.746289475136698,0.999711062990307,
2.16536549722697)) ;
#73692 = CARTESIAN_POINT('Ctrl Pts',(-0.464389285401086,1.15791979132683,
2.13172793531287)) ;
#73693 = CARTESIAN_POINT('Ctrl Pts',(-0.309165785841783,1.20866374621666,
2.11466457974615)) ;
#73694 = CARTESIAN_POINT('Ctrl Pts',(0.011687544531865,1.24747565459223,2.08204385812378)) ;
#73695 = CARTESIAN_POINT('Ctrl Pts',(0.174149188670792,1.2353163190968,2.06666375212741)) ;
#73696 = CARTESIAN_POINT('Ctrl Pts',(0.485671507308586,1.14916490674463,2.03304797306873)) ;
#73697 = CARTESIAN_POINT('Ctrl Pts',(0.631672625126814,1.0758538699623,2.01597249500797)) ;
#73698 = CARTESIAN_POINT('Ctrl Pts',(0.886757111752249,0.877472869550115,
1.98332012969277)) ;
#73699 = CARTESIAN_POINT('Ctrl Pts',(0.993472981931957,0.754526248933447,
1.96797562842022)) ;
#73700 = CARTESIAN_POINT('Ctrl Pts',(1.15401598399901,0.474052350699193,1.93438254485527)) ;
#73701 = CARTESIAN_POINT('Ctrl Pts',(1.2060886249513,0.319128439609208,1.91729491021741)) ;
#73702 = CARTESIAN_POINT('Ctrl Pts',(1.24750140441329,-0.00130710008280192,
1.8846103349448)) ;
#73703 = CARTESIAN_POINT('Ctrl Pts',(1.2367238774351,-0.163635493877063,1.86930061010034)) ;
#73704 = CARTESIAN_POINT('Ctrl Pts',(1.15330201587322,-0.47581012292618,1.83573113952197)) ;
#73705 = CARTESIAN_POINT('Ctrl Pts',(1.08117603828055,-0.622553229007982,
1.81863134856616)) ;
#73706 = CARTESIAN_POINT('Ctrl Pts',(0.884988109592906,-0.879216813977091,
1.78591404786803)) ;
#73707 = CARTESIAN_POINT('Ctrl Pts',(0.763138611287406,-0.986836462633585,
1.77063810181685)) ;
#73708 = CARTESIAN_POINT('Ctrl Pts',(0.484175066543603,-1.14982526943159,
1.73709316253432)) ;
#73709 = CARTESIAN_POINT('Ctrl Pts',(0.329578303643328,-1.20329307532079,
1.71998125107816)) ;
#73710 = CARTESIAN_POINT('Ctrl Pts',(0.112914723118742,-1.23318313648863,
1.6978057226914)) ;
#73711 = CARTESIAN_POINT('Ctrl Pts',(0.0564359310574075,-1.23704425180957,
1.69218274004799)) ;
#73712 = CARTESIAN_POINT('Ctrl Pts',(9.799417293904E-13,-1.23704425180957,
1.68671875000009)) ;
#73713 = CARTESIAN_POINT('Origin',(3.10601593664312E-15,-2.12330153459561E-14,
-0.34726562499997)) ;
#73714 = CARTESIAN_POINT('',(-8.39648792932172E-13,-1.23704425180959,0.793749999999827)) ;
#73715 = CARTESIAN_POINT('',(5.29840382873746E-14,-1.23704425180959,0.892968750000012)) ;
#73716 = CARTESIAN_POINT('',(6.06053764494801E-15,-1.23704425180962,-0.347265624999939)) ;
#73717 = CARTESIAN_POINT('Ctrl Pts',(-1.69756569912138E-12,-1.23704425180959,
0.793749999999827)) ;
#73718 = CARTESIAN_POINT('Ctrl Pts',(0.1162135096242,-1.23704425180975,0.805001510307853)) ;
#73719 = CARTESIAN_POINT('Ctrl Pts',(0.231993391524348,-1.22067968586107,
0.816867308523916)) ;
#73720 = CARTESIAN_POINT('Ctrl Pts',(0.501851918951939,-1.1425510323291,0.846127562382746)) ;
#73721 = CARTESIAN_POINT('Ctrl Pts',(0.64903902066643,-1.06585436358931,0.863453639046213)) ;
#73722 = CARTESIAN_POINT('Ctrl Pts',(0.900745927932724,-0.862696502043695,
0.895970562508104)) ;
#73723 = CARTESIAN_POINT('Ctrl Pts',(1.00409892292396,-0.739850629398905,
0.911215113226969)) ;
#73724 = CARTESIAN_POINT('Ctrl Pts',(1.16114120635477,-0.457177214677076,
0.944880758791297)) ;
#73725 = CARTESIAN_POINT('Ctrl Pts',(1.21153440255779,-0.299102787427825,
0.962206067737137)) ;
#73726 = CARTESIAN_POINT('Ctrl Pts',(1.24703303565389,0.0223587230185338,
0.994752799094146)) ;
#73727 = CARTESIAN_POINT('Ctrl Pts',(1.23383148384927,0.182360771507888,1.0099720699921)) ;
#73728 = CARTESIAN_POINT('Ctrl Pts',(1.14614189822723,0.493558250385675,1.04361808445064)) ;
#73729 = CARTESIAN_POINT('Ctrl Pts',(1.07057380233359,0.641194275551678,1.06094236546491)) ;
#73730 = CARTESIAN_POINT('Ctrl Pts',(0.869352688423176,0.894327003201699,
1.09351966371337)) ;
#73731 = CARTESIAN_POINT('Ctrl Pts',(0.747264072761988,0.998596405999818,
1.1087141933317)) ;
#73732 = CARTESIAN_POINT('Ctrl Pts',(0.465847736088978,1.15767326019276,1.14233972434915)) ;
#73733 = CARTESIAN_POINT('Ctrl Pts',(0.308273942622746,1.20921677031023,1.15966269436063)) ;
#73734 = CARTESIAN_POINT('Ctrl Pts',(-0.0128093674351517,1.24717088191047,
1.1922712817031)) ;
#73735 = CARTESIAN_POINT('Ctrl Pts',(-0.172927832847755,1.23519149091611,
1.20744175516426)) ;
#73736 = CARTESIAN_POINT('Ctrl Pts',(-0.484688169925139,1.14990381148094,
1.24104594017786)) ;
#73737 = CARTESIAN_POINT('Ctrl Pts',(-0.632793413025101,1.07554152064093,
1.25836729315049)) ;
#73738 = CARTESIAN_POINT('Ctrl Pts',(-0.887436959175382,0.876390450413255,
1.29100784990532)) ;
#73739 = CARTESIAN_POINT('Ctrl Pts',(-0.992682559954528,0.755107952134886,
1.30615510407062)) ;
#73740 = CARTESIAN_POINT('Ctrl Pts',(-1.15391618506924,0.475034915683939,
1.33973707333109)) ;
#73741 = CARTESIAN_POINT('Ctrl Pts',(-1.20667728664983,0.31800226565451,1.35705648040355)) ;
#73742 = CARTESIAN_POINT('Ctrl Pts',(-1.24723842912681,-0.00266812435902711,
1.38972963998657)) ;
#73743 = CARTESIAN_POINT('Ctrl Pts',(-1.23655669159541,-0.162910653688068,
1.4048546673072)) ;
#73744 = CARTESIAN_POINT('Ctrl Pts',(-1.15381523882729,-0.47525772953329,
1.43841354722827)) ;
#73745 = CARTESIAN_POINT('Ctrl Pts',(-1.08073357594365,-0.623849600619874,
1.45573065712404)) ;
#73746 = CARTESIAN_POINT('Ctrl Pts',(-0.883782048240159,-0.880083724520226,
1.48843700117062)) ;
#73747 = CARTESIAN_POINT('Ctrl Pts',(-0.763352513880301,-0.986363018669953,
1.50354095205518)) ;
#73748 = CARTESIAN_POINT('Ctrl Pts',(-0.484706471672932,-1.14986842699004,
1.53707586886158)) ;
#73749 = CARTESIAN_POINT('Ctrl Pts',(-0.328255474692753,-1.20390989906769,
1.55439030858974)) ;
#73750 = CARTESIAN_POINT('Ctrl Pts',(-0.11073495251392,-1.23333072827733,
1.57662998630918)) ;
#73751 = CARTESIAN_POINT('Ctrl Pts',(-0.0553466012557314,-1.23704425180953,
1.58214147622296)) ;
#73752 = CARTESIAN_POINT('Ctrl Pts',(-9.1591427459783E-13,-1.23704425180957,
1.58749999999992)) ;
#73753 = CARTESIAN_POINT('Ctrl Pts',(9.77854949790746E-13,-1.23704425180957,
1.68671875000009)) ;
#73754 = CARTESIAN_POINT('Ctrl Pts',(-0.10386256664325,-1.23704425180957,
1.67666302805362)) ;
#73755 = CARTESIAN_POINT('Ctrl Pts',(-0.207478531013762,-1.22397292284966,
1.66610698003369)) ;
#73756 = CARTESIAN_POINT('Ctrl Pts',(-0.465439188933171,-1.15754626523678,
1.63846793599463)) ;
#73757 = CARTESIAN_POINT('Ctrl Pts',(-0.612949519067283,-1.08666986668399,
1.6213439763253)) ;
#73758 = CARTESIAN_POINT('Ctrl Pts',(-0.871257204810473,-0.892786088060061,
1.58855990145816)) ;
#73759 = CARTESIAN_POINT('Ctrl Pts',(-0.979819407915098,-0.772081537314303,
1.57334784025726)) ;
#73760 = CARTESIAN_POINT('Ctrl Pts',(-1.14535382711181,-0.494707432630223,
1.53985469962491)) ;
#73761 = CARTESIAN_POINT('Ctrl Pts',(-1.20027685322434,-0.340465686100379,
1.52271880107381)) ;
#73762 = CARTESIAN_POINT('Ctrl Pts',(-1.24726986798919,-0.0209634197422772,
1.48990079803262)) ;
#73763 = CARTESIAN_POINT('Ctrl Pts',(-1.23944258399302,0.141078963361431,
1.47471850741457)) ;
#73764 = CARTESIAN_POINT('Ctrl Pts',(-1.16186482936867,0.454604495748239,
1.4412526127647)) ;
#73765 = CARTESIAN_POINT('Ctrl Pts',(-1.09229745619761,0.602902154226948,
1.42410492191876)) ;
#73766 = CARTESIAN_POINT('Ctrl Pts',(-0.900818692585104,0.862909739124637,
1.39125271562109)) ;
#73767 = CARTESIAN_POINT('Ctrl Pts',(-0.781300846944657,0.972448427893816,
1.37609853100886)) ;
#73768 = CARTESIAN_POINT('Ctrl Pts',(-0.505588448131426,1.14061394427051,
1.34266075741807)) ;
#73769 = CARTESIAN_POINT('Ctrl Pts',(-0.351729338343704,1.19704425540707,
1.32550145794681)) ;
#73770 = CARTESIAN_POINT('Ctrl Pts',(-0.0327411096781994,1.24698920659493,
1.29261484083076)) ;
#73771 = CARTESIAN_POINT('Ctrl Pts',(0.129150239315594,1.24071495015846,1.27748694345738)) ;
#73772 = CARTESIAN_POINT('Ctrl Pts',(0.443363792513356,1.16622189220983,1.24407814236331)) ;
#73773 = CARTESIAN_POINT('Ctrl Pts',(0.592463098666166,1.09801641980495,1.22690745444761)) ;
#73774 = CARTESIAN_POINT('Ctrl Pts',(0.854215627606005,0.909030767087041,
1.19398628850527)) ;
#73775 = CARTESIAN_POINT('Ctrl Pts',(0.964759018890449,0.790734196106168,
1.17888271455525)) ;
#73776 = CARTESIAN_POINT('Ctrl Pts',(1.13562442012412,0.516747116745544,1.14550370831607)) ;
#73777 = CARTESIAN_POINT('Ctrl Pts',(1.19360463581005,0.363297383936295,1.12832188767215)) ;
#73778 = CARTESIAN_POINT('Ctrl Pts',(1.2465863443891,0.04485264056338,1.09536610593822)) ;
#73779 = CARTESIAN_POINT('Ctrl Pts',(1.2419044748859,-0.116883762470755,1.0802847577046)) ;
#73780 = CARTESIAN_POINT('Ctrl Pts',(1.1705797531155,-0.431786062192727,1.0469363341123)) ;
#73781 = CARTESIAN_POINT('Ctrl Pts',(1.10378105038461,-0.581695050705877,
1.02974367061268)) ;
#73782 = CARTESIAN_POINT('Ctrl Pts',(0.917361446453772,-0.845225492784956,
0.996753278077057)) ;
#73783 = CARTESIAN_POINT('Ctrl Pts',(0.800312552818451,-0.956795325894941,
0.981691937034111)) ;
#73784 = CARTESIAN_POINT('Ctrl Pts',(0.528104024710194,-1.13041068455493,
0.948374843852459)) ;
#73785 = CARTESIAN_POINT('Ctrl Pts',(0.375088845060119,-1.18997271695152,
0.931171659754383)) ;
#73786 = CARTESIAN_POINT('Ctrl Pts',(0.143803632792016,-1.23077857977579,
0.907142742359252)) ;
#73787 = CARTESIAN_POINT('Ctrl Pts',(0.0718982454565328,-1.23704425180959,
0.899929763848464)) ;
#73788 = CARTESIAN_POINT('Ctrl Pts',(8.68838113439773E-14,-1.23704425180959,
0.892968750000012)) ;
#73789 = CARTESIAN_POINT('Origin',(3.10601593664312E-15,-2.12330153459561E-14,
-0.34726562499997)) ;
#73790 = CARTESIAN_POINT('',(1.05447087183509E-14,-1.23704425180961,0.079756751809301)) ;
#73791 = CARTESIAN_POINT('',(-7.25126625797582E-14,-1.23704425180961,0.0992187500000007)) ;
#73792 = CARTESIAN_POINT('',(6.06053764494801E-15,-1.23704425180962,-0.347265624999939)) ;
#73793 = CARTESIAN_POINT('',(0.726199640324295,-1.00145522282725,0.0797567518095777)) ;
#73794 = CARTESIAN_POINT('Origin',(-2.4980018054066E-14,3.26683124995952E-13,
0.0797567518098535)) ;
#73795 = CARTESIAN_POINT('Ctrl Pts',(0.726199640323043,-1.0014552228282,0.0797567518093963)) ;
#73796 = CARTESIAN_POINT('Ctrl Pts',(0.802662369413066,-0.946008703505574,
0.0893832681515186)) ;
#73797 = CARTESIAN_POINT('Ctrl Pts',(0.872471815530275,-0.882035343570336,
0.0984204718097368)) ;
#73798 = CARTESIAN_POINT('Ctrl Pts',(0.997224140199396,-0.738258844823923,
0.117343525487123)) ;
#73799 = CARTESIAN_POINT('Ctrl Pts',(1.05143921430174,-0.658747762510608,
0.127215791163134)) ;
#73800 = CARTESIAN_POINT('Ctrl Pts',(1.17229056528863,-0.427929940265304,
0.154409533454461)) ;
#73801 = CARTESIAN_POINT('Ctrl Pts',(1.21879504238397,-0.268237899717561,
0.171735505901204)) ;
#73802 = CARTESIAN_POINT('Ctrl Pts',(1.24604311601219,0.0544187008378128,
0.204067069536395)) ;
#73803 = CARTESIAN_POINT('Ctrl Pts',(1.22873396164754,0.214032331477905,0.21949286037181)) ;
#73804 = CARTESIAN_POINT('Ctrl Pts',(1.13294685474823,0.52326531264887,0.253273413059563)) ;
#73805 = CARTESIAN_POINT('Ctrl Pts',(1.05333123000921,0.669247043075862,0.270599847935997)) ;
#73806 = CARTESIAN_POINT('Ctrl Pts',(0.845166281544509,0.917212072143561,
0.302955291793988)) ;
#73807 = CARTESIAN_POINT('Ctrl Pts',(0.720348450836969,1.01818131913425,0.318355515374318)) ;
#73808 = CARTESIAN_POINT('Ctrl Pts',(0.434423910324296,1.16988734227459,0.352121926193887)) ;
#73809 = CARTESIAN_POINT('Ctrl Pts',(0.275081654562437,1.21725638444016,0.369448705110878)) ;
#73810 = CARTESIAN_POINT('Ctrl Pts',(-0.0473201945277858,1.24633236809541,
0.401828909282351)) ;
#73811 = CARTESIAN_POINT('Ctrl Pts',(-0.207019547606109,1.22993352367641,
0.417203293416204)) ;
#73812 = CARTESIAN_POINT('Ctrl Pts',(-0.516697555743524,1.13594406746541,
0.450954841075392)) ;
#73813 = CARTESIAN_POINT('Ctrl Pts',(-0.663056154002597,1.05722451103384,
0.468281828217318)) ;
#73814 = CARTESIAN_POINT('Ctrl Pts',(-0.912178303567051,0.850596417502907,
0.500687668948343)) ;
#73815 = CARTESIAN_POINT('Ctrl Pts',(-1.01388151658769,0.726386083539357,
0.51603603077116)) ;
#73816 = CARTESIAN_POINT('Ctrl Pts',(-1.16723727435572,0.441459608090348,
0.549771970910831)) ;
#73817 = CARTESIAN_POINT('Ctrl Pts',(-1.21554227974159,0.282502333661602,
0.567099011944622)) ;
#73818 = CARTESIAN_POINT('Ctrl Pts',(-1.24660115811779,-0.0396167266740036,
0.599531357524871)) ;
#73819 = CARTESIAN_POINT('Ctrl Pts',(-1.23118959083217,-0.19940927205464,
0.6148536127307)) ;
#73820 = CARTESIAN_POINT('Ctrl Pts',(-1.13914783753225,-0.509563718089096,
0.648573178924222)) ;
#73821 = CARTESIAN_POINT('Ctrl Pts',(-1.06140079033295,-0.656324460188585,
0.66590009997139)) ;
#73822 = CARTESIAN_POINT('Ctrl Pts',(-0.856440857683523,-0.906693947072086,
0.698359806366983)) ;
#73823 = CARTESIAN_POINT('Ctrl Pts',(-0.732887669291429,-1.00919149521601,
0.713655978353038)) ;
#73824 = CARTESIAN_POINT('Ctrl Pts',(-0.449044355490821,-1.16432601467632,
0.747358383359865)) ;
#73825 = CARTESIAN_POINT('Ctrl Pts',(-0.290509159749249,-1.21363917762656,
0.764684990055389)) ;
#73826 = CARTESIAN_POINT('Ctrl Pts',(-0.0846982434860556,-1.23487193179222,
0.785462604486457)) ;
#73827 = CARTESIAN_POINT('Ctrl Pts',(-0.042328748373072,-1.23704425180953,
0.789651833184625)) ;
#73828 = CARTESIAN_POINT('Ctrl Pts',(-1.69733995288825E-12,-1.23704425180959,
0.793749999999827)) ;
#73829 = CARTESIAN_POINT('Ctrl Pts',(8.68838113439773E-14,-1.23704425180959,
0.892968750000012)) ;
#73830 = CARTESIAN_POINT('Ctrl Pts',(-0.0875248041401834,-1.23704425180959,
0.884494810617548)) ;
#73831 = CARTESIAN_POINT('Ctrl Pts',(-0.174966896078172,-1.22776054683028,
0.87565657338642)) ;
#73832 = CARTESIAN_POINT('Ctrl Pts',(-0.41995018210912,-1.17490010146493,
0.849818014923812)) ;
#73833 = CARTESIAN_POINT('Ctrl Pts',(-0.570670292727075,-1.10954373360727,
0.832604662724326)) ;
#73834 = CARTESIAN_POINT('Ctrl Pts',(-0.835998524625215,-0.925745863761894,
0.799545352339523)) ;
#73835 = CARTESIAN_POINT('Ctrl Pts',(-0.948609445250275,-0.809962101861421,
0.784516962607178)) ;
#73836 = CARTESIAN_POINT('Ctrl Pts',(-1.12500457693874,-0.539573439929506,
0.75126458679419)) ;
#73837 = CARTESIAN_POINT('Ctrl Pts',(-1.18616863733828,-0.387015722853597,
0.734041446739443)) ;
#73838 = CARTESIAN_POINT('Ctrl Pts',(-1.24539471075493,-0.0697352935498187,
0.700947972352484)) ;
#73839 = CARTESIAN_POINT('Ctrl Pts',(-1.24397131491542,0.0916846098798968,
0.685932365379448)) ;
#73840 = CARTESIAN_POINT('Ctrl Pts',(-1.17914537419291,0.407942995498055,
0.652713270448955)) ;
#73841 = CARTESIAN_POINT('Ctrl Pts',(-1.11525651939214,0.55946897649527,0.635480747733497)) ;
#73842 = CARTESIAN_POINT('Ctrl Pts',(-0.934117137292666,0.826601135755457,
0.602353399215146)) ;
#73843 = CARTESIAN_POINT('Ctrl Pts',(-0.819606476545795,0.940260261763549,
0.587348036170277)) ;
#73844 = CARTESIAN_POINT('Ctrl Pts',(-0.551065827509422,1.1194437567851,0.554162758324779)) ;
#73845 = CARTESIAN_POINT('Ctrl Pts',(-0.398985533121644,1.1822176944358,0.536921280023609)) ;
#73846 = CARTESIAN_POINT('Ctrl Pts',(-0.0823183609100411,1.24460538594021,
0.503760388847658)) ;
#73847 = CARTESIAN_POINT('Ctrl Pts',(0.0789422497001507,1.24482410271381,
0.488762749285042)) ;
#73848 = CARTESIAN_POINT('Ctrl Pts',(0.39585691264359,1.18328008947396,0.455611730814931)) ;
#73849 = CARTESIAN_POINT('Ctrl Pts',(0.548176881593565,1.12087276457155,0.438361750130771)) ;
#73850 = CARTESIAN_POINT('Ctrl Pts',(0.817106163526264,0.942407848466602,
0.405167663070568)) ;
#73851 = CARTESIAN_POINT('Ctrl Pts',(0.931811182096248,0.829170170116615,
0.390175304535352)) ;
#73852 = CARTESIAN_POINT('Ctrl Pts',(1.11377079968785,0.562490560968091,0.357058876792354)) ;
#73853 = CARTESIAN_POINT('Ctrl Pts',(1.17814975251798,0.410904233082254,0.339800856961119)) ;
#73854 = CARTESIAN_POINT('Ctrl Pts',(1.2436934742221,0.0948635622913495,0.30657405537189)) ;
#73855 = CARTESIAN_POINT('Ctrl Pts',(1.24554635127363,-0.066236004955523,
0.291584401546679)) ;
#73856 = CARTESIAN_POINT('Ctrl Pts',(1.18727207947304,-0.383787057084025,
0.258502896359715)) ;
#73857 = CARTESIAN_POINT('Ctrl Pts',(1.12634866084976,-0.53688286891284,0.241237309769291)) ;
#73858 = CARTESIAN_POINT('Ctrl Pts',(0.950553801783562,-0.807588345240864,
0.207978333579274)) ;
#73859 = CARTESIAN_POINT('Ctrl Pts',(0.838578599221216,-0.923329787010875,
0.192988836521312)) ;
#73860 = CARTESIAN_POINT('Ctrl Pts',(0.573758990510375,-1.10803178977929,
0.159942511219614)) ;
#73861 = CARTESIAN_POINT('Ctrl Pts',(0.422678950448764,-1.1739984166373,0.142669838213727)) ;
#73862 = CARTESIAN_POINT('Ctrl Pts',(0.17651318645884,-1.22759348881469,0.116687334249879)) ;
#73863 = CARTESIAN_POINT('Ctrl Pts',(0.0883103353827004,-1.23704425180962,
0.107768742613292)) ;
#73864 = CARTESIAN_POINT('Ctrl Pts',(-1.55774404735361E-13,-1.23704425180961,
0.0992187500000006)) ;
#73865 = CARTESIAN_POINT('Origin',(0.,0.,0.)) ;
#73866 = CARTESIAN_POINT('',(-1.7526,3.24070050962596E-15,1.09140625)) ;
#73867 = CARTESIAN_POINT('',(-1.7526,1.70165690542032E-13,0.992187499999977)) ;
#73868 = CARTESIAN_POINT('',(-1.7526,-2.14631598018565E-16,0.)) ;
#73869 = CARTESIAN_POINT('',(1.23927534470755,-1.23927534470755,0.595312499999997)) ;
#73870 = CARTESIAN_POINT('Ctrl Pts',(-1.7526,5.55111512312578E-15,1.09140625)) ;
#73871 = CARTESIAN_POINT('Ctrl Pts',(-1.7526,0.104547657359432,1.08426176482362)) ;
#73872 = CARTESIAN_POINT('Ctrl Pts',(-1.74324717274818,0.209108727288083,
1.07685162045178)) ;
#73873 = CARTESIAN_POINT('Ctrl Pts',(-1.68340069519565,0.539420779786685,
1.05258502413979)) ;
#73874 = CARTESIAN_POINT('Ctrl Pts',(-1.59787269747691,0.75605024665108,1.03536022243484)) ;
#73875 = CARTESIAN_POINT('Ctrl Pts',(-1.35066052761109,1.13936681186793,1.00216784753972)) ;
#73876 = CARTESIAN_POINT('Ctrl Pts',(-1.19306628616519,1.30346997592726,0.987212602834704)) ;
#73877 = CARTESIAN_POINT('Ctrl Pts',(-0.819924420582547,1.56608123915945,
0.954279648356355)) ;
#73878 = CARTESIAN_POINT('Ctrl Pts',(-0.606768521826978,1.66033533629354,
0.937045217909976)) ;
#73879 = CARTESIAN_POINT('Ctrl Pts',(-0.161546082820598,1.75962805345187,
0.90380940587192)) ;
#73880 = CARTESIAN_POINT('Ctrl Pts',(0.0657712499739911,1.76580372195142,
0.888847879253041)) ;
#73881 = CARTESIAN_POINT('Ctrl Pts',(0.515896453846038,1.69080176141891,0.855964604443078)) ;
#73882 = CARTESIAN_POINT('Ctrl Pts',(0.733993601723274,1.60816871798398,0.838721450690954)) ;
#73883 = CARTESIAN_POINT('Ctrl Pts',(1.12071257887363,1.36614209500329,0.805443347700574)) ;
#73884 = CARTESIAN_POINT('Ctrl Pts',(1.28680628777948,1.21097938674294,0.790470917443707)) ;
#73885 = CARTESIAN_POINT('Ctrl Pts',(1.55465981560029,0.841466028666496,0.757637536319184)) ;
#73886 = CARTESIAN_POINT('Ctrl Pts',(1.65195907511392,0.629329368409463,0.740386560838467)) ;
#73887 = CARTESIAN_POINT('Ctrl Pts',(1.7572524398515,0.185372758680501,0.707067396633006)) ;
#73888 = CARTESIAN_POINT('Ctrl Pts',(1.76651236376204,-0.0416378121238857,
0.692079647673984)) ;
#73889 = CARTESIAN_POINT('Ctrl Pts',(1.70441589556448,-0.448830076054136,
0.662495590997371)) ;
#73890 = CARTESIAN_POINT('Ctrl Pts',(1.64693701205005,-0.627750772362418,
0.648641660541893)) ;
#73891 = CARTESIAN_POINT('Ctrl Pts',(1.47869800081274,-0.958703636471365,
0.621263096675404)) ;
#73892 = CARTESIAN_POINT('Ctrl Pts',(1.36965572949312,-1.10889495992211,0.607912887171705)) ;
#73893 = CARTESIAN_POINT('Ctrl Pts',(1.23927534470684,-1.23927534470824,0.595312499999933)) ;
#73894 = CARTESIAN_POINT('',(1.7526,0.,0.5953125)) ;
#73895 = CARTESIAN_POINT('Origin',(0.,0.,0.5953125)) ;
#73896 = CARTESIAN_POINT('Ctrl Pts',(1.7526,-2.15105711021124E-15,0.5953125)) ;
#73897 = CARTESIAN_POINT('Ctrl Pts',(1.7526,0.21481984001363,0.609992667890278)) ;
#73898 = CARTESIAN_POINT('Ctrl Pts',(1.71310447370405,0.427903785524575,0.625672176423836)) ;
#73899 = CARTESIAN_POINT('Ctrl Pts',(1.55856129077335,0.830122835430236,0.657533189451965)) ;
#73900 = CARTESIAN_POINT('Ctrl Pts',(1.44454049439502,1.01565121826221,0.673439154533952)) ;
#73901 = CARTESIAN_POINT('Ctrl Pts',(1.1487270417631,1.34262606689925,0.704157014779829)) ;
#73902 = CARTESIAN_POINT('Ctrl Pts',(0.967058618495535,1.47886687425541,0.71991567147517)) ;
#73903 = CARTESIAN_POINT('Ctrl Pts',(0.554468507663844,1.67889396301424,0.75377288756523)) ;
#73904 = CARTESIAN_POINT('Ctrl Pts',(0.326094855888817,1.73776089872563,0.771045580701419)) ;
#73905 = CARTESIAN_POINT('Ctrl Pts',(-0.131750544532228,1.76205786107286,
0.803021167700791)) ;
#73906 = CARTESIAN_POINT('Ctrl Pts',(-0.356611590657682,1.73062508679216,
0.818741832310748)) ;
#73907 = CARTESIAN_POINT('Ctrl Pts',(-0.790158210912439,1.58168779748694,
0.852584999765607)) ;
#73908 = CARTESIAN_POINT('Ctrl Pts',(-0.993577728078715,1.46250450419731,
0.869859723794248)) ;
#73909 = CARTESIAN_POINT('Ctrl Pts',(-1.33540783531321,1.15709975956045,0.901864242180511)) ;
#73910 = CARTESIAN_POINT('Ctrl Pts',(-1.4727465616134,0.9763392165215,0.917545719644801)) ;
#73911 = CARTESIAN_POINT('Ctrl Pts',(-1.67528581774019,0.56521487114132,0.951373879364155)) ;
#73912 = CARTESIAN_POINT('Ctrl Pts',(-1.73558543790577,0.337376226297066,
0.9686505654653)) ;
#73913 = CARTESIAN_POINT('Ctrl Pts',(-1.75156455156437,0.0695968375627338,
0.987402143410981)) ;
#73914 = CARTESIAN_POINT('Ctrl Pts',(-1.7526,0.0347828049418742,0.989810543494454)) ;
#73915 = CARTESIAN_POINT('Ctrl Pts',(-1.7526,3.40546012682082E-13,0.992187499999977)) ;
#73916 = CARTESIAN_POINT('Origin',(0.,0.,0.)) ;
#73917 = CARTESIAN_POINT('',(-1.7526,-7.2430388732916E-14,1.88515625000001)) ;
#73918 = CARTESIAN_POINT('',(-1.7526,2.85432335943383E-13,1.78593749999996)) ;
#73919 = CARTESIAN_POINT('',(-1.7526,-2.14631598018565E-16,0.)) ;
#73920 = CARTESIAN_POINT('Ctrl Pts',(-1.7526,-1.44155520853673E-13,1.88515625000001)) ;
#73921 = CARTESIAN_POINT('Ctrl Pts',(-1.75260000000001,0.137894910250373,
1.87573290980218)) ;
#73922 = CARTESIAN_POINT('Ctrl Pts',(-1.73633070266727,0.275582131070812,
1.86586324117668)) ;
#73923 = CARTESIAN_POINT('Ctrl Pts',(-1.65021735313446,0.633251880812449,
1.83898358452446)) ;
#73924 = CARTESIAN_POINT('Ctrl Pts',(-1.55325686201387,0.8435796286795,1.82186581412804)) ;
#73925 = CARTESIAN_POINT('Ctrl Pts',(-1.28533606284546,1.21283083755785,1.78904844332966)) ;
#73926 = CARTESIAN_POINT('Ctrl Pts',(-1.11779116886749,1.3687913098494,1.77396952247319)) ;
#73927 = CARTESIAN_POINT('Ctrl Pts',(-0.73020747915963,1.6096874188709,1.74066432803057)) ;
#73928 = CARTESIAN_POINT('Ctrl Pts',(-0.513326877073374,1.69138962506005,
1.72353065793429)) ;
#73929 = CARTESIAN_POINT('Ctrl Pts',(-0.0633186871198124,1.76605389040637,
1.69066493837158)) ;
#73930 = CARTESIAN_POINT('Ctrl Pts',(0.165276475839116,1.75944269119178,1.67561792294161)) ;
#73931 = CARTESIAN_POINT('Ctrl Pts',(0.610355197234708,1.65886568423244,1.64235557883846)) ;
#73932 = CARTESIAN_POINT('Ctrl Pts',(0.822287881901152,1.56467786568413,1.62520661540491)) ;
#73933 = CARTESIAN_POINT('Ctrl Pts',(1.19504792379624,1.30181724091056,1.59229269518788)) ;
#73934 = CARTESIAN_POINT('Ctrl Pts',(1.35302893168609,1.13674084899859,1.57727316131317)) ;
#73935 = CARTESIAN_POINT('Ctrl Pts',(1.59934964349609,0.752676972049826,1.5440549510449)) ;
#73936 = CARTESIAN_POINT('Ctrl Pts',(1.68417623655015,0.536652784648655,1.52689136646387)) ;
#73937 = CARTESIAN_POINT('Ctrl Pts',(1.76495892013688,0.0877725403261723,
1.49392953852819)) ;
#73938 = CARTESIAN_POINT('Ctrl Pts',(1.76154542959128,-0.140503534161234,
1.47893285472881)) ;
#73939 = CARTESIAN_POINT('Ctrl Pts',(1.6673469914036,-0.586915339414595,1.44575996430666)) ;
#73940 = CARTESIAN_POINT('Ctrl Pts',(1.57600910258148,-0.800445713521442,
1.4285824899529)) ;
#73941 = CARTESIAN_POINT('Ctrl Pts',(1.31832327386051,-1.17674495475663,1.39557318966923)) ;
#73942 = CARTESIAN_POINT('Ctrl Pts',(1.15574533167312,-1.33677126408857,1.38059456494248)) ;
#73943 = CARTESIAN_POINT('Ctrl Pts',(0.775287903995105,-1.5885585898706,1.34746807016247)) ;
#73944 = CARTESIAN_POINT('Ctrl Pts',(0.560176278440258,-1.67654203789935,
1.33027748898416)) ;
#73945 = CARTESIAN_POINT('Ctrl Pts',(0.112478485471377,-1.76351335068776,
1.29722129003663)) ;
#73946 = CARTESIAN_POINT('Ctrl Pts',(-0.11547683701007,-1.76331954554437,
1.28225582539335)) ;
#73947 = CARTESIAN_POINT('Ctrl Pts',(-0.563182482720134,-1.67555649639276,
1.24917667879644)) ;
#73948 = CARTESIAN_POINT('Ctrl Pts',(-0.77828442275198,-1.58711590168822,
1.23197381943213)) ;
#73949 = CARTESIAN_POINT('Ctrl Pts',(-1.15811524055575,-1.33466516746216,
1.19887136681734)) ;
#73950 = CARTESIAN_POINT('Ctrl Pts',(-1.3201894927846,-1.1745901086568,1.18391422887698)) ;
#73951 = CARTESIAN_POINT('Ctrl Pts',(-1.57742656628545,-0.797786875386106,
1.15088318976893)) ;
#73952 = CARTESIAN_POINT('Ctrl Pts',(-1.668564210659,-0.583635070404743,1.13366891677396)) ;
#73953 = CARTESIAN_POINT('Ctrl Pts',(-1.74027492516994,-0.239971504707985,
1.10815408560011)) ;
#73954 = CARTESIAN_POINT('Ctrl Pts',(-1.7526,-0.120018555030801,1.0996079716738)) ;
#73955 = CARTESIAN_POINT('Ctrl Pts',(-1.7526,5.44703171456717E-15,1.09140625)) ;
#73956 = CARTESIAN_POINT('Ctrl Pts',(-1.7526,3.37785355242204E-13,0.992187499999977)) ;
#73957 = CARTESIAN_POINT('Ctrl Pts',(-1.7526,-0.189598109227915,1.005144087599)) ;
#73958 = CARTESIAN_POINT('Ctrl Pts',(-1.7218412189295,-0.378150559501995,
1.01889988084353)) ;
#73959 = CARTESIAN_POINT('Ctrl Pts',(-1.58698346716713,-0.77942035652952,
1.05013880571663)) ;
#73960 = CARTESIAN_POINT('Ctrl Pts',(-1.46927136315343,-0.983505269936009,
1.06741735728579)) ;
#73961 = CARTESIAN_POINT('Ctrl Pts',(-1.16639091096922,-1.32729172587642,
1.09948411387195)) ;
#73962 = CARTESIAN_POINT('Ctrl Pts',(-0.986642304617752,-1.46585487001854,
1.11508405901835)) ;
#73963 = CARTESIAN_POINT('Ctrl Pts',(-0.577158522321734,-1.67118546774369,
1.14887911955152)) ;
#73964 = CARTESIAN_POINT('Ctrl Pts',(-0.349926086046935,-1.73307590322111,
1.16615940898039)) ;
#73965 = CARTESIAN_POINT('Ctrl Pts',(0.107114628641963,-1.76371403859573,
1.1982595003338)) ;
#73966 = CARTESIAN_POINT('Ctrl Pts',(0.332276422609993,-1.73544618249771,
1.21381737045474)) ;
#73967 = CARTESIAN_POINT('Ctrl Pts',(0.767450699788526,-1.59278072451589,
1.24759423582901)) ;
#73968 = CARTESIAN_POINT('Ctrl Pts',(0.972262664692636,-1.47670680677704,
1.26487610123737)) ;
#73969 = CARTESIAN_POINT('Ctrl Pts',(1.31821032672548,-1.17663629117846,1.29701100989763)) ;
#73970 = CARTESIAN_POINT('Ctrl Pts',(1.458131396676,-0.998009254994801,1.31252615256722)) ;
#73971 = CARTESIAN_POINT('Ctrl Pts',(1.66654482904563,-0.590351992356521,
1.34628365722728)) ;
#73972 = CARTESIAN_POINT('Ctrl Pts',(1.73019072282956,-0.363803485072845,
1.36356689920542)) ;
#73973 = CARTESIAN_POINT('Ctrl Pts',(1.7645229382863,0.0927476684014285,1.39573810057802)) ;
#73974 = CARTESIAN_POINT('Ctrl Pts',(1.73809700251126,0.318085361371882,1.41121005975164)) ;
#73975 = CARTESIAN_POINT('Ctrl Pts',(1.59907663088538,0.754185070479275,1.44494698807761)) ;
#73976 = CARTESIAN_POINT('Ctrl Pts',(1.48481611104004,0.95978494330198,1.46223136650934)) ;
#73977 = CARTESIAN_POINT('Ctrl Pts',(1.18785527375227,1.30810418333975,1.494440318916)) ;
#73978 = CARTESIAN_POINT('Ctrl Pts',(1.01046360803963,1.44952204637,1.50986886038149)) ;
#73979 = CARTESIAN_POINT('Ctrl Pts',(0.604827973964349,1.66131763116995,1.54358394852591)) ;
#73980 = CARTESIAN_POINT('Ctrl Pts',(0.379047263768518,1.72688742092612,1.56086917957305)) ;
#73981 = CARTESIAN_POINT('Ctrl Pts',(-0.0769481266801126,1.76527924233848,
1.59311731355779)) ;
#73982 = CARTESIAN_POINT('Ctrl Pts',(-0.302479780335044,1.74087622754771,
1.60850245019479)) ;
#73983 = CARTESIAN_POINT('Ctrl Pts',(-0.7395773828631,1.60585438572068,1.64219438865525)) ;
#73984 = CARTESIAN_POINT('Ctrl Pts',(-0.946023426504051,1.49358813022675,
1.65948014199397)) ;
#73985 = CARTESIAN_POINT('Ctrl Pts',(-1.29692605138797,1.20004656583408,1.69176884898162)) ;
#73986 = CARTESIAN_POINT('Ctrl Pts',(-1.4399827386388,1.02400637996451,1.70711086526757)) ;
#73987 = CARTESIAN_POINT('Ctrl Pts',(-1.65546189751001,0.620593827557374,
1.74077830226157)) ;
#73988 = CARTESIAN_POINT('Ctrl Pts',(-1.72312437828023,0.395670201913235,
1.75806419866947)) ;
#73989 = CARTESIAN_POINT('Ctrl Pts',(-1.75003962953136,0.109450542229317,
1.77838549156683)) ;
#73990 = CARTESIAN_POINT('Ctrl Pts',(-1.7526,0.0546965877173526,1.78219969305134)) ;
#73991 = CARTESIAN_POINT('Ctrl Pts',(-1.7526,5.71079303484785E-13,1.78593749999996)) ;
#73992 = CARTESIAN_POINT('Origin',(0.,0.,0.)) ;
#73993 = CARTESIAN_POINT('',(-1.7526,-3.02963679535642E-13,2.67890625000005)) ;
#73994 = CARTESIAN_POINT('',(-1.7526,1.12532367841355E-13,2.57968749999998)) ;
#73995 = CARTESIAN_POINT('',(-1.7526,-2.14631598018565E-16,0.)) ;
#73996 = CARTESIAN_POINT('Ctrl Pts',(-1.7526,-6.06112382506296E-13,2.67890625000005)) ;
#73997 = CARTESIAN_POINT('Ctrl Pts',(-1.75260000000006,0.167794841835216,
2.66743963476974)) ;
#73998 = CARTESIAN_POINT('Ctrl Pts',(-1.72851068177184,0.334990802640833,
2.65533206925858)) ;
#73999 = CARTESIAN_POINT('Ctrl Pts',(-1.61613829516608,0.715405367443283,
2.62615480509768)) ;
#74000 = CARTESIAN_POINT('Ctrl Pts',(-1.50932245410327,0.91960420272306,2.60917689979265)) ;
#74001 = CARTESIAN_POINT('Ctrl Pts',(-1.22317845929475,1.27581509594749,2.5767348378504)) ;
#74002 = CARTESIAN_POINT('Ctrl Pts',(-1.04652669095695,1.42430903244335,2.56127802021772)) ;
#74003 = CARTESIAN_POINT('Ctrl Pts',(-0.646337776712737,1.64499658772374,
2.52768344765317)) ;
#74004 = CARTESIAN_POINT('Ctrl Pts',(-0.426687637569999,1.71514464643388,
2.51068756892792)) ;
#74005 = CARTESIAN_POINT('Ctrl Pts',(0.0271348749003668,1.76720867163961,
2.47820091557302)) ;
#74006 = CARTESIAN_POINT('Ctrl Pts',(0.256915735402302,1.74864533134862,2.46279992862756)) ;
#74007 = CARTESIAN_POINT('Ctrl Pts',(0.696591814856775,1.62437266580848,2.42923605239312)) ;
#74008 = CARTESIAN_POINT('Ctrl Pts',(0.902246371267716,1.51980072118882,2.41222218339769)) ;
#74009 = CARTESIAN_POINT('Ctrl Pts',(1.26150882860939,1.23784150397511,2.3796900413523)) ;
#74010 = CARTESIAN_POINT('Ctrl Pts',(1.41174582860743,1.0633118822824,2.36434318780097)) ;
#74011 = CARTESIAN_POINT('Ctrl Pts',(1.63716968880939,0.666006325112866,2.33081158893528)) ;
#74012 = CARTESIAN_POINT('Ctrl Pts',(1.71001242012726,0.446946707454403,2.31377978891158)) ;
#74013 = CARTESIAN_POINT('Ctrl Pts',(1.76734651524038,-0.00603574739972152,
2.28120136723079)) ;
#74014 = CARTESIAN_POINT('Ctrl Pts',(1.75159138829553,-0.235540169200276,
2.26590656468891)) ;
#74015 = CARTESIAN_POINT('Ctrl Pts',(1.63286262308617,-0.676544727005498,
2.23240883060458)) ;
#74016 = CARTESIAN_POINT('Ctrl Pts',(1.53069027897643,-0.883715991510807,
2.21535923762982)) ;
#74017 = CARTESIAN_POINT('Ctrl Pts',(1.25318188960883,-1.24618637556307,2.18273386097376)) ;
#74018 = CARTESIAN_POINT('Ctrl Pts',(1.08088890457571,-1.39825791607344,2.16748864177913)) ;
#74019 = CARTESIAN_POINT('Ctrl Pts',(0.686657935676051,-1.62865582263718,
2.13402635525318)) ;
#74020 = CARTESIAN_POINT('Ctrl Pts',(0.468256765243388,-1.70433764044138,
2.1169591879779)) ;
#74021 = CARTESIAN_POINT('Ctrl Pts',(0.0161917720505629,-1.7672238142356,
2.08428630495496)) ;
#74022 = CARTESIAN_POINT('Ctrl Pts',(-0.21302102223957,-1.75441282183859,
2.06908782214896)) ;
#74023 = CARTESIAN_POINT('Ctrl Pts',(-0.655379533562164,-1.64151270301104,
2.0356625493825)) ;
#74024 = CARTESIAN_POINT('Ctrl Pts',(-0.864114072684682,-1.5418833009729,
2.01857810765572)) ;
#74025 = CARTESIAN_POINT('Ctrl Pts',(-1.22992400629464,-1.26906584175147,
1.98585729803748)) ;
#74026 = CARTESIAN_POINT('Ctrl Pts',(-1.38390861706332,-1.09910773855309,
1.97070233785842)) ;
#74027 = CARTESIAN_POINT('Ctrl Pts',(-1.61947947451139,-0.708125235589788,
1.93731561574699)) ;
#74028 = CARTESIAN_POINT('Ctrl Pts',(-1.69812325285362,-0.490450951286152,
1.92021428004477)) ;
#74029 = CARTESIAN_POINT('Ctrl Pts',(-1.74595470399728,-0.176304466427567,
1.89739249122397)) ;
#74030 = CARTESIAN_POINT('Ctrl Pts',(-1.75259999999999,-0.0881227360395467,
1.89117830345619)) ;
#74031 = CARTESIAN_POINT('Ctrl Pts',(-1.7526,-1.44646145867813E-13,1.88515625000001)) ;
#74032 = CARTESIAN_POINT('Ctrl Pts',(-1.7526,5.71079303484785E-13,1.78593749999996)) ;
#74033 = CARTESIAN_POINT('Ctrl Pts',(-1.7526,-0.169339024401733,1.79750964021027)) ;
#74034 = CARTESIAN_POINT('Ctrl Pts',(-1.72806515051229,-0.338033438283696,
1.80973221695903)) ;
#74035 = CARTESIAN_POINT('Ctrl Pts',(-1.61308143750617,-0.72360540841447,
1.83933583993703)) ;
#74036 = CARTESIAN_POINT('Ctrl Pts',(-1.50299263305593,-0.930951275487185,
1.85662144933578)) ;
#74037 = CARTESIAN_POINT('Ctrl Pts',(-1.21318427577553,-1.28464560245755,
1.88899526043142)) ;
#74038 = CARTESIAN_POINT('Ctrl Pts',(-1.03861168766202,-1.42948356470644,
1.90425308939975)) ;
#74039 = CARTESIAN_POINT('Ctrl Pts',(-0.637626366345578,-1.64894294060327,
1.93786732108372)) ;
#74040 = CARTESIAN_POINT('Ctrl Pts',(-0.413653382345688,-1.71886315472059,
1.95515216114529)) ;
#74041 = CARTESIAN_POINT('Ctrl Pts',(0.0410093244316962,-1.76648056906025,
1.98757036447825)) ;
#74042 = CARTESIAN_POINT('Ctrl Pts',(0.266984560954872,-1.74667118590977,
2.00278777632734)) ;
#74043 = CARTESIAN_POINT('Ctrl Pts',(0.706276495114559,-1.6207083130571,2.03637324445863)) ;
#74044 = CARTESIAN_POINT('Ctrl Pts',(0.914569087867585,-1.51297837596066,
2.05365677988273)) ;
#74045 = CARTESIAN_POINT('Ctrl Pts',(1.27125430488095,-1.22721474999631,2.08612048896267)) ;
#74046 = CARTESIAN_POINT('Ctrl Pts',(1.41801316077564,-1.054223186184,2.10129906156371)) ;
#74047 = CARTESIAN_POINT('Ctrl Pts',(1.64173675890614,-0.655867477843011,
2.13485429684043)) ;
#74048 = CARTESIAN_POINT('Ctrl Pts',(1.71407133525771,-0.432941345458989,
2.15213593940611)) ;
#74049 = CARTESIAN_POINT('Ctrl Pts',(1.76683813655813,0.0209350447270955,
2.18464616750078)) ;
#74050 = CARTESIAN_POINT('Ctrl Pts',(1.74959152333341,0.24715968621795,2.19978783806631)) ;
#74051 = CARTESIAN_POINT('Ctrl Pts',(1.62866847251747,0.687632694870889,2.23331135941382)) ;
#74052 = CARTESIAN_POINT('Ctrl Pts',(1.52347229531964,0.896910039075942,2.25059046889851)) ;
#74053 = CARTESIAN_POINT('Ctrl Pts',(1.24205467761495,1.25677007786189,2.28314811733312)) ;
#74054 = CARTESIAN_POINT('Ctrl Pts',(1.07075186180036,1.40558294859694,2.29825518800676)) ;
#74055 = CARTESIAN_POINT('Ctrl Pts',(0.675221204033864,1.63383361824712,2.33174551148854)) ;
#74056 = CARTESIAN_POINT('Ctrl Pts',(0.453438689242829,1.70872576533173,2.34902139753333)) ;
#74057 = CARTESIAN_POINT('Ctrl Pts',(0.000432766936031767,1.76697209320413,
2.38162724471802)) ;
#74058 = CARTESIAN_POINT('Ctrl Pts',(-0.226058764460174,1.75245236168843,
2.39670238262469)) ;
#74059 = CARTESIAN_POINT('Ctrl Pts',(-0.667754664436714,1.63687944061578,
2.43015803121053)) ;
#74060 = CARTESIAN_POINT('Ctrl Pts',(-0.878043964467795,1.5343801550739,2.44742995619069)) ;
#74061 = CARTESIAN_POINT('Ctrl Pts',(-1.24124121035046,1.25759093278454,2.48008464762852)) ;
#74062 = CARTESIAN_POINT('Ctrl Pts',(-1.39223079083935,1.08807569583888,2.49513087887956)) ;
#74063 = CARTESIAN_POINT('Ctrl Pts',(-1.62524149301606,0.695552885592716,
2.52855039298208)) ;
#74064 = CARTESIAN_POINT('Ctrl Pts',(-1.70281592843141,0.475008766544544,
2.54581757591695)) ;
#74065 = CARTESIAN_POINT('Ctrl Pts',(-1.7468382272959,0.164173644723157,2.5683052532728)) ;
#74066 = CARTESIAN_POINT('Ctrl Pts',(-1.7526,0.0820549291164976,2.57408010295708)) ;
#74067 = CARTESIAN_POINT('Ctrl Pts',(-1.7526,2.25279367280728E-13,2.57968749999998)) ;
#74068 = CARTESIAN_POINT('Origin',(0.,0.,0.)) ;
#74069 = CARTESIAN_POINT('',(-1.7526,-2.09103334841134E-13,3.47265625000003)) ;
#74070 = CARTESIAN_POINT('',(-1.7526,-5.06302198483948E-16,3.3734375)) ;
#74071 = CARTESIAN_POINT('',(-1.7526,-2.14631598018565E-16,0.)) ;
#74072 = CARTESIAN_POINT('Ctrl Pts',(-1.7526,-4.17513246198098E-13,3.47265625000003)) ;
#74073 = CARTESIAN_POINT('Ctrl Pts',(-1.75260000000004,0.185210600655636,
3.45999949207434)) ;
#74074 = CARTESIAN_POINT('Ctrl Pts',(-1.72324896284641,0.369470892755415,
3.44657686035593)) ;
#74075 = CARTESIAN_POINT('Ctrl Pts',(-1.59279484445025,0.767421264017481,
3.41568942540778)) ;
#74076 = CARTESIAN_POINT('Ctrl Pts',(-1.47672495305229,0.972234997958048,
3.39840755307882)) ;
#74077 = CARTESIAN_POINT('Ctrl Pts',(-1.17301360568729,1.32239354269544,3.36588182688286)) ;
#74078 = CARTESIAN_POINT('Ctrl Pts',(-0.989205491121332,1.4649837181463,3.34995951071369)) ;
#74079 = CARTESIAN_POINT('Ctrl Pts',(-0.579538199999467,1.6695782840237,3.31617274395179)) ;
#74080 = CARTESIAN_POINT('Ctrl Pts',(-0.358141571382955,1.73064028751114,
3.29931470650395)) ;
#74081 = CARTESIAN_POINT('Ctrl Pts',(0.0982952795497277,1.7649160237594,3.26715291494664)) ;
#74082 = CARTESIAN_POINT('Ctrl Pts',(0.328999802663575,1.73676904263517,3.25128773938596)) ;
#74083 = CARTESIAN_POINT('Ctrl Pts',(0.763872713205693,1.5937059475115,3.21752021295754)) ;
#74084 = CARTESIAN_POINT('Ctrl Pts',(0.964173820662061,1.48114590915186,3.20064607095859)) ;
#74085 = CARTESIAN_POINT('Ctrl Pts',(1.31233058947525,1.18417961761153,3.16844806697758)) ;
#74086 = CARTESIAN_POINT('Ctrl Pts',(1.45622838186895,1.00195149571405,3.15264086582667)) ;
#74087 = CARTESIAN_POINT('Ctrl Pts',(1.66439213815404,0.594344213342975,3.11889384404487)) ;
#74088 = CARTESIAN_POINT('Ctrl Pts',(1.72745943040643,0.373300780381277,3.10200318094529)) ;
#74089 = CARTESIAN_POINT('Ctrl Pts',(1.76566483314572,-0.0825878733541528,
3.06976761783615)) ;
#74090 = CARTESIAN_POINT('Ctrl Pts',(1.73964953909945,-0.313090227909846,
3.05401898960127)) ;
#74091 = CARTESIAN_POINT('Ctrl Pts',(1.60074750475764,-0.749067292774356,
3.02029379210293)) ;
#74092 = CARTESIAN_POINT('Ctrl Pts',(1.48993651937415,-0.950581907434876,
3.00338623149624)) ;
#74093 = CARTESIAN_POINT('Ctrl Pts',(1.19628310005053,-1.30122937743768,2.97111179487327)) ;
#74094 = CARTESIAN_POINT('Ctrl Pts',(1.01577567112777,-1.44654829596119,2.95542207613238)) ;
#74095 = CARTESIAN_POINT('Ctrl Pts',(0.610432930541322,-1.65858863601416,
2.92172007540247)) ;
#74096 = CARTESIAN_POINT('Ctrl Pts',(0.389794994609997,-1.72384046393432,
2.9047952869848)) ;
#74097 = CARTESIAN_POINT('Ctrl Pts',(-0.0654779456713953,-1.76632390737681,
2.872480705054)) ;
#74098 = CARTESIAN_POINT('Ctrl Pts',(-0.295758785991269,-1.74261971907228,
2.85684994471076)) ;
#74099 = CARTESIAN_POINT('Ctrl Pts',(-0.732909890444729,-1.60824129178231,
2.82317256267759)) ;
#74100 = CARTESIAN_POINT('Ctrl Pts',(-0.935725769901182,-1.49934475758604,
2.80623026815074)) ;
#74101 = CARTESIAN_POINT('Ctrl Pts',(-1.28906055399697,-1.2092995320789,2.77387432234772)) ;
#74102 = CARTESIAN_POINT('Ctrl Pts',(-1.43591283688306,-1.03065239366411,
2.75830225741605)) ;
#74103 = CARTESIAN_POINT('Ctrl Pts',(-1.65213207633461,-0.62778258377614,
2.72465096104054)) ;
#74104 = CARTESIAN_POINT('Ctrl Pts',(-1.71974616387183,-0.407607554591312,
2.70769093983665)) ;
#74105 = CARTESIAN_POINT('Ctrl Pts',(-1.74949550562248,-0.120523582461612,
2.68723036010368)) ;
#74106 = CARTESIAN_POINT('Ctrl Pts',(-1.75259999999998,-0.0602292128905996,
2.6830221405857)) ;
#74107 = CARTESIAN_POINT('Ctrl Pts',(-1.7526,-6.05712727473265E-13,2.67890625000005)) ;
#74108 = CARTESIAN_POINT('Ctrl Pts',(-1.7526,2.25279367280728E-13,2.57968749999998)) ;
#74109 = CARTESIAN_POINT('Ctrl Pts',(-1.7526,-0.142024538270848,2.58939304705851)) ;
#74110 = CARTESIAN_POINT('Ctrl Pts',(-1.73534182380825,-0.283790939099401,
2.59956946643582)) ;
#74111 = CARTESIAN_POINT('Ctrl Pts',(-1.64524534444182,-0.6467636811424,2.62692426138539)) ;
#74112 = CARTESIAN_POINT('Ctrl Pts',(-1.54558886698793,-0.858079736654223,
2.64418588289291)) ;
#74113 = CARTESIAN_POINT('Ctrl Pts',(-1.27368250679245,-1.22474897706124,
2.6769396253434)) ;
#74114 = CARTESIAN_POINT('Ctrl Pts',(-1.10604159088307,-1.37802354594454,
2.69193848892341)) ;
#74115 = CARTESIAN_POINT('Ctrl Pts',(-0.716690851871007,-1.61598895300862,
2.7252814814989)) ;
#74116 = CARTESIAN_POINT('Ctrl Pts',(-0.497475018079849,-1.69634711168952,
2.74253668976731)) ;
#74117 = CARTESIAN_POINT('Ctrl Pts',(-0.0464636891190264,-1.76639663606009,
2.77534033536094)) ;
#74118 = CARTESIAN_POINT('Ctrl Pts',(0.180608059176743,-1.75775315744277,
2.79032136742799)) ;
#74119 = CARTESIAN_POINT('Ctrl Pts',(0.624821194156055,-1.6536608113385,2.82362406560381)) ;
#74120 = CARTESIAN_POINT('Ctrl Pts',(0.837165348245854,-1.55697051100277,
2.84087198331866)) ;
#74121 = CARTESIAN_POINT('Ctrl Pts',(1.20740840408138,-1.29016467261973,2.87372557381785)) ;
#74122 = CARTESIAN_POINT('Ctrl Pts',(1.36305801487321,-1.12446972860818,2.8886930464671)) ;
#74123 = CARTESIAN_POINT('Ctrl Pts',(1.60612704091343,-0.73843090146846,2.92195417639586)) ;
#74124 = CARTESIAN_POINT('Ctrl Pts',(1.6893429308557,-0.520625246278682,2.93919390852514)) ;
#74125 = CARTESIAN_POINT('Ctrl Pts',(1.76561778142678,-0.0707325453436116,
2.97209732538375)) ;
#74126 = CARTESIAN_POINT('Ctrl Pts',(1.76007670662897,0.156648105524041,2.98705574259079)) ;
#74127 = CARTESIAN_POINT('Ctrl Pts',(1.66201597291323,0.602125530862736,3.02027410693917)) ;
#74128 = CARTESIAN_POINT('Ctrl Pts',(1.5683878464975,0.815485282051297,3.03750474924555)) ;
#74129 = CARTESIAN_POINT('Ctrl Pts',(1.30685524541685,1.18936675820036,3.07045771379264)) ;
#74130 = CARTESIAN_POINT('Ctrl Pts',(1.14316023010785,1.34745987301223,3.08541176804576)) ;
#74131 = CARTESIAN_POINT('Ctrl Pts',(0.76054348947215,1.59572971971315,3.11858625771782)) ;
#74132 = CARTESIAN_POINT('Ctrl Pts',(0.54421879935505,1.681846775671,3.13580690583587)) ;
#74133 = CARTESIAN_POINT('Ctrl Pts',(0.0955173731444148,1.76448303712047,
3.16880898152834)) ;
#74134 = CARTESIAN_POINT('Ctrl Pts',(-0.1321808781177,1.76211573038241,3.18376350595154)) ;
#74135 = CARTESIAN_POINT('Ctrl Pts',(-0.578905685979277,1.67020212412462,
3.21689311125174)) ;
#74136 = CARTESIAN_POINT('Ctrl Pts',(-0.793255034070076,1.57970086529386,
3.23410287014207)) ;
#74137 = CARTESIAN_POINT('Ctrl Pts',(-1.17079956001474,1.32356249944587,3.26715346685808)) ;
#74138 = CARTESIAN_POINT('Ctrl Pts',(-1.33138037898044,1.16190166375245,3.28211338383734)) ;
#74139 = CARTESIAN_POINT('Ctrl Pts',(-1.58489259402161,0.782783166642962,
3.31519720495683)) ;
#74140 = CARTESIAN_POINT('Ctrl Pts',(-1.67392181139128,0.567996248342534,
3.33239519829217)) ;
#74141 = CARTESIAN_POINT('Ctrl Pts',(-1.74135782360205,0.22921502874541,3.35745538361937)) ;
#74142 = CARTESIAN_POINT('Ctrl Pts',(-1.7526,0.114623761611832,3.36560444293893)) ;
#74143 = CARTESIAN_POINT('Ctrl Pts',(-1.7526,-5.55111512312578E-16,3.3734375)) ;
#74144 = CARTESIAN_POINT('Origin',(0.,0.,0.)) ;
#74145 = CARTESIAN_POINT('',(-1.7526,-6.97032678444217E-14,4.26640625000002)) ;
#74146 = CARTESIAN_POINT('',(-1.7526,-1.44575086878353E-13,4.16718750000002)) ;
#74147 = CARTESIAN_POINT('',(-1.7526,-2.14631598018565E-16,0.)) ;
#74148 = CARTESIAN_POINT('Ctrl Pts',(-1.7526,-1.3912482277334E-13,4.26640625000002)) ;
#74149 = CARTESIAN_POINT('Ctrl Pts',(-1.75260000000002,0.20021035250331,4.25272445232278)) ;
#74150 = CARTESIAN_POINT('Ctrl Pts',(-1.7182993432369,0.399124785467476,4.23816029418824)) ;
#74151 = CARTESIAN_POINT('Ctrl Pts',(-1.57256716668258,0.808235012859114,
4.20607776373)) ;
#74152 = CARTESIAN_POINT('Ctrl Pts',(-1.45090373646926,1.01050584252262,4.18881133453901)) ;
#74153 = CARTESIAN_POINT('Ctrl Pts',(-1.14124126899642,1.34900413359057,4.15691398307249)) ;
#74154 = CARTESIAN_POINT('Ctrl Pts',(-0.958764240846233,1.48426752674617,
4.14108339296375)) ;
#74155 = CARTESIAN_POINT('Ctrl Pts',(-0.544873581032442,1.68205096011171,
4.10720081037692)) ;
#74156 = CARTESIAN_POINT('Ctrl Pts',(-0.316030548027637,1.73963764710754,
4.08993228000637)) ;
#74157 = CARTESIAN_POINT('Ctrl Pts',(0.142141141021597,1.76125722862828,4.05801018175233)) ;
#74158 = CARTESIAN_POINT('Ctrl Pts',(0.366875607603623,1.72848677607019,4.04221497702927)) ;
#74159 = CARTESIAN_POINT('Ctrl Pts',(0.799720006941358,1.57689574068337,4.0083446799656)) ;
#74160 = CARTESIAN_POINT('Ctrl Pts',(1.00253640979324,1.45640111071015,3.99107405212338)) ;
#74161 = CARTESIAN_POINT('Ctrl Pts',(1.34261020733303,1.14874555256045,3.95912584298678)) ;
#74162 = CARTESIAN_POINT('Ctrl Pts',(1.47885343647802,0.967079132387764,3.94336736075693)) ;
#74163 = CARTESIAN_POINT('Ctrl Pts',(1.67888607605626,0.554492249112647,3.90951020810639)) ;
#74164 = CARTESIAN_POINT('Ctrl Pts',(1.73775617832987,0.326119768457322,3.89223750536792)) ;
#74165 = CARTESIAN_POINT('Ctrl Pts',(1.76205976840444,-0.131724814356606,
3.86026178663595)) ;
#74166 = CARTESIAN_POINT('Ctrl Pts',(1.73063030439237,-0.356586174100122,
3.8445413022737)) ;
#74167 = CARTESIAN_POINT('Ctrl Pts',(1.58169958013592,-0.790134521566633,
3.81069820261749)) ;
#74168 = CARTESIAN_POINT('Ctrl Pts',(1.46251953418115,-0.993555520508037,
3.7934234692482)) ;
#74169 = CARTESIAN_POINT('Ctrl Pts',(1.15712036235999,-1.33538996225157,3.76141881239911)) ;
#74170 = CARTESIAN_POINT('Ctrl Pts',(0.976362057983705,-1.47273139649564,
3.74573752054108)) ;
#74171 = CARTESIAN_POINT('Ctrl Pts',(0.565241334081197,-1.67527683800978,
3.7119094332185)) ;
#74172 = CARTESIAN_POINT('Ctrl Pts',(0.337404018862843,-1.73557998459742,
3.69463273816068)) ;
#74173 = CARTESIAN_POINT('Ctrl Pts',(-0.12006516187297,-1.76288584741123,
3.66259769051253)) ;
#74174 = CARTESIAN_POINT('Ctrl Pts',(-0.345068736274904,-1.73295537074502,
3.64695668443386)) ;
#74175 = CARTESIAN_POINT('Ctrl Pts',(-0.779393877244594,-1.58699641468622,
3.61314462029586)) ;
#74176 = CARTESIAN_POINT('Ctrl Pts',(-0.98348041604981,-1.4692879367239,3.59586606029122)) ;
#74177 = CARTESIAN_POINT('Ctrl Pts',(-1.32727167564188,-1.1664137051595,3.56379915151923)) ;
#74178 = CARTESIAN_POINT('Ctrl Pts',(-1.46583783176088,-0.986667587364208,
3.54819940101925)) ;
#74179 = CARTESIAN_POINT('Ctrl Pts',(-1.67117528248908,-0.577187848274536,
3.51440442280493)) ;
#74180 = CARTESIAN_POINT('Ctrl Pts',(-1.73306962205852,-0.349956915545484,
3.49712412561418)) ;
#74181 = CARTESIAN_POINT('Ctrl Pts',(-1.75129362080061,-0.0781760192814626,
3.47803555211733)) ;
#74182 = CARTESIAN_POINT('Ctrl Pts',(-1.75259999999999,-0.0390693720068885,
3.47532613812762)) ;
#74183 = CARTESIAN_POINT('Ctrl Pts',(-1.7526,-4.1799203808425E-13,3.47265625000003)) ;
#74184 = CARTESIAN_POINT('Ctrl Pts',(-1.7526,5.20417042793042E-16,3.3734375)) ;
#74185 = CARTESIAN_POINT('Ctrl Pts',(-1.7526,-0.110290712389861,3.38097444898255)) ;
#74186 = CARTESIAN_POINT('Ctrl Pts',(-1.74219157692512,-0.220571031733036,
3.38880531021715)) ;
#74187 = CARTESIAN_POINT('Ctrl Pts',(-1.6781174386689,-0.555412544065956,
3.41350110557992)) ;
#74188 = CARTESIAN_POINT('Ctrl Pts',(-1.59077377474029,-0.770712973034604,
3.4306864792079)) ;
#74189 = CARTESIAN_POINT('Ctrl Pts',(-1.34036001264139,-1.15149977671283,
3.46379660228058)) ;
#74190 = CARTESIAN_POINT('Ctrl Pts',(-1.18116471893329,-1.31429332825069,
3.47875083345804)) ;
#74191 = CARTESIAN_POINT('Ctrl Pts',(-0.805655132204611,-1.57343913115523,
3.51174749729369)) ;
#74192 = CARTESIAN_POINT('Ctrl Pts',(-0.591851390805269,-1.66568295798028,
3.5289692964048)) ;
#74193 = CARTESIAN_POINT('Ctrl Pts',(-0.145816340827931,-1.7610209202741,
3.56214869600973)) ;
#74194 = CARTESIAN_POINT('Ctrl Pts',(0.0817046468911821,-1.76515776908648,
3.57710299755285)) ;
#74195 = CARTESIAN_POINT('Ctrl Pts',(0.531076123027321,-1.68606731810649,
3.61005049424702)) ;
#74196 = CARTESIAN_POINT('Ctrl Pts',(0.748231261236104,-1.60156493198531,
3.62728218768916)) ;
#74197 = CARTESIAN_POINT('Ctrl Pts',(1.13276017984804,-1.35619220140093,3.66050534385486)) ;
#74198 = CARTESIAN_POINT('Ctrl Pts',(1.29757141623345,-1.19946318792092,3.67546453578996)) ;
#74199 = CARTESIAN_POINT('Ctrl Pts',(1.56205098033292,-0.827608010919695,
3.70836244610627)) ;
#74200 = CARTESIAN_POINT('Ctrl Pts',(1.65738980324903,-0.614809925134019,
3.72560312906785)) ;
#74201 = CARTESIAN_POINT('Ctrl Pts',(1.75881857792582,-0.170033544249094,
3.75886892236587)) ;
#74202 = CARTESIAN_POINT('Ctrl Pts',(1.76609340287348,0.0571742758199495,
3.77383767859007)) ;
#74203 = CARTESIAN_POINT('Ctrl Pts',(1.69329679860401,0.507697700798713,3.80668574151523)) ;
#74204 = CARTESIAN_POINT('Ctrl Pts',(1.6116753741927,0.726296042245817,3.82393451034011)) ;
#74205 = CARTESIAN_POINT('Ctrl Pts',(1.3714561522033,1.11418980751476,3.85724173437944)) ;
#74206 = CARTESIAN_POINT('Ctrl Pts',(1.21713546460311,1.28097332671082,3.8722245352361)) ;
#74207 = CARTESIAN_POINT('Ctrl Pts',(0.848887625573543,1.55063619792425,3.9050226500038)) ;
#74208 = CARTESIAN_POINT('Ctrl Pts',(0.637113785841988,1.64898751954791,3.92227861121472)) ;
#74209 = CARTESIAN_POINT('Ctrl Pts',(0.193604384633389,1.75635710844691,3.95562598441266)) ;
#74210 = CARTESIAN_POINT('Ctrl Pts',(-0.0333006902295665,1.7666817120298,
3.97062707387792)) ;
#74211 = CARTESIAN_POINT('Ctrl Pts',(-0.4848992414616,1.70000772939862,4.00337529992421)) ;
#74212 = CARTESIAN_POINT('Ctrl Pts',(-0.704863455468664,1.62120653484239,
4.02063757866201)) ;
#74213 = CARTESIAN_POINT('Ctrl Pts',(-1.09599481138453,1.38601427493407,4.05402375631231)) ;
#74214 = CARTESIAN_POINT('Ctrl Pts',(-1.26468653960243,1.23402108015127,4.06904710460958)) ;
#74215 = CARTESIAN_POINT('Ctrl Pts',(-1.53933410450875,0.869294862158893,
4.10174565949343)) ;
#74216 = CARTESIAN_POINT('Ctrl Pts',(-1.6405861752385,0.658550076098389,4.11901340721298)) ;
#74217 = CARTESIAN_POINT('Ctrl Pts',(-1.73431865952934,0.292042822720498,
4.14671266180152)) ;
#74218 = CARTESIAN_POINT('Ctrl Pts',(-1.75260000000002,0.146174356133978,
4.15719836636521)) ;
#74219 = CARTESIAN_POINT('Ctrl Pts',(-1.7526,-2.89004931097736E-13,4.16718750000002)) ;
#74220 = CARTESIAN_POINT('Origin',(0.,0.,0.)) ;
#74221 = CARTESIAN_POINT('',(-1.7526,-2.15134495268842E-14,5.06015625000001)) ;
#74222 = CARTESIAN_POINT('',(-1.7526,-2.79050850736062E-13,4.96093750000004)) ;
#74223 = CARTESIAN_POINT('',(-1.7526,-2.14631598018565E-16,0.)) ;
#74224 = CARTESIAN_POINT('Ctrl Pts',(-1.7526,-4.34374758384592E-14,5.06015625000001)) ;
#74225 = CARTESIAN_POINT('Ctrl Pts',(-1.75260000000001,0.209553021544105,
5.04583600128375)) ;
#74226 = CARTESIAN_POINT('Ctrl Pts',(-1.71502071246155,0.417566653426324,
5.03055722471029)) ;
#74227 = CARTESIAN_POINT('Ctrl Pts',(-1.55945751550078,0.833354407293773,
4.99774009293334)) ;
#74228 = CARTESIAN_POINT('Ctrl Pts',(-1.43434040293718,1.03396849796978,4.98048912002016)) ;
#74229 = CARTESIAN_POINT('Ctrl Pts',(-1.11874264416212,1.36775444830488,4.94874579101757)) ;
#74230 = CARTESIAN_POINT('Ctrl Pts',(-0.933851894800391,1.50010250410655,
4.93268272773915)) ;
#74231 = CARTESIAN_POINT('Ctrl Pts',(-0.516107355713871,1.69115436333346,
4.89872732717594)) ;
#74232 = CARTESIAN_POINT('Ctrl Pts',(-0.285903620642897,1.74489672691016,
4.88147462838478)) ;
#74233 = CARTESIAN_POINT('Ctrl Pts',(0.173197292714659,1.75850207685975,4.84971588173976)) ;
#74234 = CARTESIAN_POINT('Ctrl Pts',(0.39755401614597,1.72172171026321,4.83367701009703)) ;
#74235 = CARTESIAN_POINT('Ctrl Pts',(0.828242469633597,1.56216698635971,4.79972862271391)) ;
#74236 = CARTESIAN_POINT('Ctrl Pts',(1.02919949925927,1.43775341500248,4.78247412889219)) ;
#74237 = CARTESIAN_POINT('Ctrl Pts',(1.3639523869677,1.1233654135263,4.75069896576308)) ;
#74238 = CARTESIAN_POINT('Ctrl Pts',(1.49689684607618,0.938968663923053,4.7346856328411)) ;
#74239 = CARTESIAN_POINT('Ctrl Pts',(1.68933053643342,0.522009368276059,4.70074477921605)) ;
#74240 = CARTESIAN_POINT('Ctrl Pts',(1.74386238587,0.29207915162885,4.68348842457198)) ;
#74241 = CARTESIAN_POINT('Ctrl Pts',(1.75911059422777,-0.166837054428321,
4.65169579727879)) ;
#74242 = CARTESIAN_POINT('Ctrl Pts',(1.72315300195766,-0.391271092051124,
4.63570938136785)) ;
#74243 = CARTESIAN_POINT('Ctrl Pts',(1.56523325401132,-0.822408145766662,
4.60177661782992)) ;
#74244 = CARTESIAN_POINT('Ctrl Pts',(1.44162220607035,-1.023752946598,4.58451834119889)) ;
#74245 = CARTESIAN_POINT('Ctrl Pts',(1.12861370694019,-1.35960440722033,4.55270715318068)) ;
#74246 = CARTESIAN_POINT('Ctrl Pts',(0.944778996204964,-1.49322756830232,
4.53674905734208)) ;
#74247 = CARTESIAN_POINT('Ctrl Pts',(0.528715304794354,-1.68723084035202,
4.5028249778962)) ;
#74248 = CARTESIAN_POINT('Ctrl Pts',(0.299099398954512,-1.7426592494988,4.48556472418351)) ;
#74249 = CARTESIAN_POINT('Ctrl Pts',(-0.159603232089813,-1.75977495358756,
4.45373383035843)) ;
#74250 = CARTESIAN_POINT('Ctrl Pts',(-0.384125224424138,-1.72475213656398,
4.4378054746974)) ;
#74251 = CARTESIAN_POINT('Ctrl Pts',(-0.815768038173584,-1.56868936870932,
4.40389071295291)) ;
#74252 = CARTESIAN_POINT('Ctrl Pts',(-1.01754948783441,-1.44599111725407,
4.38662843476389)) ;
#74253 = CARTESIAN_POINT('Ctrl Pts',(-1.35464482158062,-1.13455112137733,
4.35477664234939)) ;
#74254 = CARTESIAN_POINT('Ctrl Pts',(-1.48903790883624,-0.95135381841529,
4.33887945488558)) ;
#74255 = CARTESIAN_POINT('Ctrl Pts',(-1.68481791220455,-0.536308650653891,
4.30497468596644)) ;
#74256 = CARTESIAN_POINT('Ctrl Pts',(-1.74126092919167,-0.307053205314894,
4.2877103454328)) ;
#74257 = CARTESIAN_POINT('Ctrl Pts',(-1.75208741637621,-0.0489626096197369,
4.26976672270769)) ;
#74258 = CARTESIAN_POINT('Ctrl Pts',(-1.7526,-0.0244726012247594,4.26807863693907)) ;
#74259 = CARTESIAN_POINT('Ctrl Pts',(-1.7526,-1.39191904090825E-13,4.26640625000002)) ;
#74260 = CARTESIAN_POINT('Ctrl Pts',(-1.7526,-2.88935542158687E-13,4.16718750000002)) ;
#74261 = CARTESIAN_POINT('Ctrl Pts',(-1.75259999999999,-0.0778592500677814,
4.17250817644559)) ;
#74262 = CARTESIAN_POINT('Ctrl Pts',(-1.74741231880974,-0.155785145504359,
4.17798025057415)) ;
#74263 = CARTESIAN_POINT('Ctrl Pts',(-1.70616780214948,-0.462906643552702,
4.20013552125307)) ;
#74264 = CARTESIAN_POINT('Ctrl Pts',(-1.63009713754219,-0.684150006894371,
4.21740792254869)) ;
#74265 = CARTESIAN_POINT('Ctrl Pts',(-1.39975666801596,-1.07836487569639,
4.2508674830185)) ;
#74266 = CARTESIAN_POINT('Ctrl Pts',(-1.24999034087451,-1.24888442921395,
4.26594601436367)) ;
#74267 = CARTESIAN_POINT('Ctrl Pts',(-0.888665008594113,-1.52827751968141,
4.29854649013608)) ;
#74268 = CARTESIAN_POINT('Ctrl Pts',(-0.678940366934257,-1.63229381110136,
4.31582276860299)) ;
#74269 = CARTESIAN_POINT('Ctrl Pts',(-0.237928042188737,-1.75087446783154,
4.34931684107538)) ;
#74270 = CARTESIAN_POINT('Ctrl Pts',(-0.0115868232081193,-1.76692803281445,
4.36442761836085)) ;
#74271 = CARTESIAN_POINT('Ctrl Pts',(0.441913018063719,-1.7117638375004,4.3969799752066)) ;
#74272 = CARTESIAN_POINT('Ctrl Pts',(0.664342551661163,-1.63830877582951,
4.41425939828048)) ;
#74273 = CARTESIAN_POINT('Ctrl Pts',(1.06146566052312,-1.41260316424873,4.44778650445482)) ;
#74274 = CARTESIAN_POINT('Ctrl Pts',(1.2337191956317,-1.26494693200175,4.46293215457177)) ;
#74275 = CARTESIAN_POINT('Ctrl Pts',(1.51758671909389,-0.906871654067533,
4.49543718502358)) ;
#74276 = CARTESIAN_POINT('Ctrl Pts',(1.62421107924902,-0.698145300472901,
4.51271906777459)) ;
#74277 = CARTESIAN_POINT('Ctrl Pts',(1.74797322130534,-0.25833414777866,4.54627772356529)) ;
#74278 = CARTESIAN_POINT('Ctrl Pts',(1.76666420047231,-0.0322502404855705,
4.56146050813967)) ;
#74279 = CARTESIAN_POINT('Ctrl Pts',(1.71679968828143,0.422073094209958,4.593919126474)) ;
#74280 = CARTESIAN_POINT('Ctrl Pts',(1.64582462485974,0.64559257787106,4.61120283436381)) ;
#74281 = CARTESIAN_POINT('Ctrl Pts',(1.42450323936098,1.04543338478737,4.64479155957741)) ;
#74282 = CARTESIAN_POINT('Ctrl Pts',(1.27882812276648,1.21931673326615,4.66001337566066)) ;
#74283 = CARTESIAN_POINT('Ctrl Pts',(0.923827775295789,1.50736471058222,4.69242660683217)) ;
#74284 = CARTESIAN_POINT('Ctrl Pts',(0.716066272743709,1.61642680955421,4.7097115574711)) ;
#74285 = CARTESIAN_POINT('Ctrl Pts',(0.277408009498461,1.74504501462892,4.74332888461807)) ;
#74286 = CARTESIAN_POINT('Ctrl Pts',(0.0515634108557028,1.76620249745117,
4.75859127085426)) ;
#74287 = CARTESIAN_POINT('Ctrl Pts',(-0.403500598482737,1.72129330343181,
4.79096023872994)) ;
#74288 = CARTESIAN_POINT('Ctrl Pts',(-0.628013288176575,1.65264694722788,
4.80824590269585)) ;
#74289 = CARTESIAN_POINT('Ctrl Pts',(-1.03037182335714,1.4354341131867,4.84189038488026)) ;
#74290 = CARTESIAN_POINT('Ctrl Pts',(-1.20577370834242,1.29160291027468,4.85719453252823)) ;
#74291 = CARTESIAN_POINT('Ctrl Pts',(-1.49769414797966,0.939484314067199,
4.88952044767104)) ;
#74292 = CARTESIAN_POINT('Ctrl Pts',(-1.60901484935553,0.732644451246718,
4.9068063484703)) ;
#74293 = CARTESIAN_POINT('Ctrl Pts',(-1.72711252303101,0.344486838563733,
4.93667481106522)) ;
#74294 = CARTESIAN_POINT('Ctrl Pts',(-1.75260000000006,0.172594590798071,
4.94914288377783)) ;
#74295 = CARTESIAN_POINT('Ctrl Pts',(-1.7526,-5.58962598429247E-13,4.96093750000004)) ;
#74296 = CARTESIAN_POINT('Origin',(0.,0.,0.)) ;
#74297 = CARTESIAN_POINT('',(-1.7526,-5.41548163298149E-15,5.85390625)) ;
#74298 = CARTESIAN_POINT('',(-1.7526,-1.50126202001478E-13,5.75468750000002)) ;
#74299 = CARTESIAN_POINT('',(-1.7526,-2.14631598018565E-16,0.)) ;
#74300 = CARTESIAN_POINT('Ctrl Pts',(-1.7526,-1.04083408558608E-14,5.85390625)) ;
#74301 = CARTESIAN_POINT('Ctrl Pts',(-1.7526,0.215063581698836,5.83920942550641)) ;
#74302 = CARTESIAN_POINT('Ctrl Pts',(-1.71301637555779,0.428433931657122,
5.82350785119934)) ;
#74303 = CARTESIAN_POINT('Ctrl Pts',(-1.55154324405163,0.848059638465521,
5.79026115724544)) ;
#74304 = CARTESIAN_POINT('Ctrl Pts',(-1.42440027697519,1.04767049607852,5.77302139822362)) ;
#74305 = CARTESIAN_POINT('Ctrl Pts',(-1.10531671400859,1.37865171095447,5.7413710670186)) ;
#74306 = CARTESIAN_POINT('Ctrl Pts',(-0.918996616265576,1.50927478176608,
5.72515792892315)) ;
#74307 = CARTESIAN_POINT('Ctrl Pts',(-0.498990396180971,1.69631661152442,
5.69116148014123)) ;
#74308 = CARTESIAN_POINT('Ctrl Pts',(-0.268009804098051,1.74776715638448,
5.67392056576987)) ;
#74309 = CARTESIAN_POINT('Ctrl Pts',(0.191609637137813,1.75661159116519,5.64226114764989)) ;
#74310 = CARTESIAN_POINT('Ctrl Pts',(0.415742569592707,1.71744437932947,5.62606298203586)) ;
#74311 = CARTESIAN_POINT('Ctrl Pts',(0.845111418224298,1.55314432567097,5.59207045057964)) ;
#74312 = CARTESIAN_POINT('Ctrl Pts',(1.0449254130281,1.4264077591063,5.57482831338614)) ;
#74313 = CARTESIAN_POINT('Ctrl Pts',(1.37647173126268,1.10802376181094,5.54315916666592)) ;
#74314 = CARTESIAN_POINT('Ctrl Pts',(1.50744177625706,0.921991233292156,5.52697695775436)) ;
#74315 = CARTESIAN_POINT('Ctrl Pts',(1.69529178381865,0.502438791650662,5.49298864247188)) ;
#74316 = CARTESIAN_POINT('Ctrl Pts',(1.74720429850968,0.271612750237907,5.4757452130556)) ;
#74317 = CARTESIAN_POINT('Ctrl Pts',(1.75700745513532,-0.187904271158755,
5.44406565627846)) ;
#74318 = CARTESIAN_POINT('Ctrl Pts',(1.71832120043968,-0.412082242742052,
5.42790043764716)) ;
#74319 = CARTESIAN_POINT('Ctrl Pts',(1.55497759964053,-0.841719178154872,
5.39391665942113)) ;
#74320 = CARTESIAN_POINT('Ctrl Pts',(1.42870848978082,-1.04176565822851,5.37667186675926)) ;
#74321 = CARTESIAN_POINT('Ctrl Pts',(1.11112897410725,-1.37396044897767,5.34498117708394)) ;
#74322 = CARTESIAN_POINT('Ctrl Pts',(0.925426697440239,-1.5053290123611,5.32883403169105)) ;
#74323 = CARTESIAN_POINT('Ctrl Pts',(0.506396164499377,-1.69410628171457,
5.29485513492282)) ;
#74324 = CARTESIAN_POINT('Ctrl Pts',(0.275748699203071,-1.7465487915919,5.27760890675472)) ;
#74325 = CARTESIAN_POINT('Ctrl Pts',(-0.18364951780585,-1.75745242646143,
5.24590631841395)) ;
#74326 = CARTESIAN_POINT('Ctrl Pts',(-0.407879202904414,-1.71931804669363,
5.22977837814854)) ;
#74327 = CARTESIAN_POINT('Ctrl Pts',(-0.837822397688919,-1.55707177860285,
5.1958047323155)) ;
#74328 = CARTESIAN_POINT('Ctrl Pts',(-1.03813430276736,-1.43133945442896,
5.17855699561603)) ;
#74329 = CARTESIAN_POINT('Ctrl Pts',(-1.37107173384084,-1.11468349854734,
5.14684169847491)) ;
#74330 = CARTESIAN_POINT('Ctrl Pts',(-1.50289716039955,-0.929359773570224,
5.1307341431521)) ;
#74331 = CARTESIAN_POINT('Ctrl Pts',(-1.69273615719116,-0.510928497408213,
5.09676614443656)) ;
#74332 = CARTESIAN_POINT('Ctrl Pts',(-1.74578545348992,-0.280487150192089,
5.07951682599002)) ;
#74333 = CARTESIAN_POINT('Ctrl Pts',(-1.75239538719435,-0.0309314004765573,
5.06227580444235)) ;
#74334 = CARTESIAN_POINT('Ctrl Pts',(-1.7526,-0.0154618997563056,5.06121287160586)) ;
#74335 = CARTESIAN_POINT('Ctrl Pts',(-1.7526,-4.28122674557499E-14,5.06015625000001)) ;
#74336 = CARTESIAN_POINT('Ctrl Pts',(-1.7526,-5.57887069874106E-13,4.96093750000004)) ;
#74337 = CARTESIAN_POINT('Ctrl Pts',(-1.75259999999998,-0.0514754444292417,
4.96445518331268)) ;
#74338 = CARTESIAN_POINT('Ctrl Pts',(-1.75033229848047,-0.103004617511181,
4.96804072820716)) ;
#74339 = CARTESIAN_POINT('Ctrl Pts',(-1.72527339535509,-0.386268440786449,
4.988107481689)) ;
#74340 = CARTESIAN_POINT('Ctrl Pts',(-1.65879384324703,-0.611679371540988,
5.00539319495447)) ;
#74341 = CARTESIAN_POINT('Ctrl Pts',(-1.44539751850817,-1.01635167457427,
5.03908776263559)) ;
#74342 = CARTESIAN_POINT('Ctrl Pts',(-1.30326860888275,-1.19315682040023,
5.05447769671142)) ;
#74343 = CARTESIAN_POINT('Ctrl Pts',(-0.953826774202952,-1.4886359567931,
5.08672142273433)) ;
#74344 = CARTESIAN_POINT('Ctrl Pts',(-0.747857632971182,-1.60203231349978,
5.10400657476385)) ;
#74345 = CARTESIAN_POINT('Ctrl Pts',(-0.311322981091731,-1.73931875691161,
5.13772414497515)) ;
#74346 = CARTESIAN_POINT('Ctrl Pts',(-0.0859013110107367,-1.76486779209003,
5.15315749824057)) ;
#74347 = CARTESIAN_POINT('Ctrl Pts',(0.370411258410795,-1.7287761040988,5.18536219937763)) ;
#74348 = CARTESIAN_POINT('Ctrl Pts',(0.596629075374267,-1.6642956856852,5.20264646512087)) ;
#74349 = CARTESIAN_POINT('Ctrl Pts',(1.00341199399925,-1.45441565979707,5.23638573326439)) ;
#74350 = CARTESIAN_POINT('Ctrl Pts',(1.18150397822415,-1.31384645521521,5.2518624900127)) ;
#74351 = CARTESIAN_POINT('Ctrl Pts',(1.48022953107292,-0.966870472196266,
5.28402960043137)) ;
#74352 = CARTESIAN_POINT('Ctrl Pts',(1.59551918713128,-0.761715580467981,
5.30131270103304)) ;
#74353 = CARTESIAN_POINT('Ctrl Pts',(1.73660710597921,-0.326138942781364,
5.33507240848899)) ;
#74354 = CARTESIAN_POINT('Ctrl Pts',(1.76407804995685,-0.100901126708342,
5.35059230869242)) ;
#74355 = CARTESIAN_POINT('Ctrl Pts',(1.73184195511883,0.355929701719502,5.38272328911981)) ;
#74356 = CARTESIAN_POINT('Ctrl Pts',(1.66919160755838,0.582868013518023,5.40000498912339)) ;
#74357 = CARTESIAN_POINT('Ctrl Pts',(1.46252684911046,0.991563221616929,5.43378392573789)) ;
#74358 = CARTESIAN_POINT('Ctrl Pts',(1.32337677146238,1.17082696103987,5.44934649035458)) ;
#74359 = CARTESIAN_POINT('Ctrl Pts',(0.978655074350586,1.47249420866847,5.4814428174617)) ;
#74360 = CARTESIAN_POINT('Ctrl Pts',(0.774254492279916,1.58949907634077,5.49872292177171)) ;
#74361 = CARTESIAN_POINT('Ctrl Pts',(0.339562078660178,1.73403937841308,5.53251992761676)) ;
#74362 = CARTESIAN_POINT('Ctrl Pts',(0.114490432682257,1.76325387278217,5.54812448403179)) ;
#74363 = CARTESIAN_POINT('Ctrl Pts',(-0.342795796134348,1.73451329405964,
5.58018764057103)) ;
#74364 = CARTESIAN_POINT('Ctrl Pts',(-0.570374083439141,1.67352630851254,
5.59746599126339)) ;
#74365 = CARTESIAN_POINT('Ctrl Pts',(-0.98079126107425,1.46978121726822,5.63127995774103)) ;
#74366 = CARTESIAN_POINT('Ctrl Pts',(-1.16111506906919,1.33191414004616,5.64692566486227)) ;
#74367 = CARTESIAN_POINT('Ctrl Pts',(-1.46543165464954,0.98923897254071,5.67895713062485)) ;
#74368 = CARTESIAN_POINT('Ctrl Pts',(-1.58398081695685,0.785531195556426,
5.69623360368484)) ;
#74369 = CARTESIAN_POINT('Ctrl Pts',(-1.72110925026966,0.382583025914159,
5.72765149797256)) ;
#74370 = CARTESIAN_POINT('Ctrl Pts',(-1.75260000000003,0.191839612966701,
5.74157773450451)) ;
#74371 = CARTESIAN_POINT('Ctrl Pts',(-1.7526,-2.99725522179273E-13,5.75468750000002)) ;
#74372 = CARTESIAN_POINT('Origin',(0.,0.,0.)) ;
#74373 = CARTESIAN_POINT('',(1.24732203685813,1.23117606229494,6.24999999831013)) ;
#74374 = CARTESIAN_POINT('Ctrl Pts',(-1.7526,-3.00037772404938E-13,5.75468750000002)) ;
#74375 = CARTESIAN_POINT('Ctrl Pts',(-1.75259999999999,-0.032598322299679,
5.75691517526626)) ;
#74376 = CARTESIAN_POINT('Ctrl Pts',(-1.75169052435328,-0.0652248173994592,
5.75917051954304)) ;
#74377 = CARTESIAN_POINT('Ctrl Pts',(-1.73683227675797,-0.330958761491049,
5.77775059029158)) ;
#74378 = CARTESIAN_POINT('Ctrl Pts',(-1.67734733744449,-0.559102898338026,
5.79502509234845)) ;
#74379 = CARTESIAN_POINT('Ctrl Pts',(-1.47623678512082,-0.971062086850928,
5.8288698617205)) ;
#74380 = CARTESIAN_POINT('Ctrl Pts',(-1.33952292301057,-1.15233928101824,
5.84459479373804)) ;
#74381 = CARTESIAN_POINT('Ctrl Pts',(-0.998693925502225,-1.45902877365591,
5.87656726545657)) ;
#74382 = CARTESIAN_POINT('Ctrl Pts',(-0.795617527723386,-1.57896062756801,
5.89383973057284)) ;
#74383 = CARTESIAN_POINT('Ctrl Pts',(-0.362470600691468,-1.72941212332175,
5.9276984455155)) ;
#74384 = CARTESIAN_POINT('Ctrl Pts',(-0.137681826299413,-1.76160826471163,
5.94346123196741)) ;
#74385 = CARTESIAN_POINT('Ctrl Pts',(0.320350778809865,-1.73883941048927,
5.97540635712271)) ;
#74386 = CARTESIAN_POINT('Ctrl Pts',(0.54899323602356,-1.68070291513661,5.99267674368556)) ;
#74387 = CARTESIAN_POINT('Ctrl Pts',(0.962326432463704,-1.48195606680838,
6.02654850141181)) ;
#74388 = CARTESIAN_POINT('Ctrl Pts',(1.14445650561047,-1.34627333654908,6.04234785886134)) ;
#74389 = CARTESIAN_POINT('Ctrl Pts',(1.45326081358979,-1.00710025443336,6.07426703240116)) ;
#74390 = CARTESIAN_POINT('Ctrl Pts',(1.57442451607132,-0.804595233816516,
6.09153532015318)) ;
#74391 = CARTESIAN_POINT('Ctrl Pts',(1.72737162339113,-0.372112789748117,
6.12541926742668)) ;
#74392 = CARTESIAN_POINT('Ctrl Pts',(1.76082533135169,-0.147442862085292,
6.14125385278895)) ;
#74393 = CARTESIAN_POINT('Ctrl Pts',(1.74137248937904,0.292789957304284,6.17188872838747)) ;
#74394 = CARTESIAN_POINT('Ctrl Pts',(1.69217994490562,0.504581831709392,6.18775442585301)) ;
#74395 = CARTESIAN_POINT('Ctrl Pts',(1.51977635982089,0.898901097711236,6.21958114983884)) ;
#74396 = CARTESIAN_POINT('Ctrl Pts',(1.3982679007908,1.07825065364772,6.23527681869574)) ;
#74397 = CARTESIAN_POINT('Ctrl Pts',(1.24732203681668,1.23117606233693,6.24999999746791)) ;
#74398 = CARTESIAN_POINT('',(1.57068438372304,-0.777603252442184,6.25000631418241)) ;
#74399 = CARTESIAN_POINT('Origin',(0.,0.,6.25)) ;
#74400 = CARTESIAN_POINT('',(1.35494872380545,-1.11162979288941,6.16356193246049)) ;
#74401 = CARTESIAN_POINT('Ctrl Pts',(1.3549489689189,-1.11162945787956,6.16355972756376)) ;
#74402 = CARTESIAN_POINT('Ctrl Pts',(1.44940645924245,-0.996496597542542,
6.17410130374198)) ;
#74403 = CARTESIAN_POINT('Ctrl Pts',(1.50897892716071,-0.894016315078257,
6.19049173038489)) ;
#74404 = CARTESIAN_POINT('Ctrl Pts',(1.54943011338412,-0.81923740960474,6.21567530064911)) ;
#74405 = CARTESIAN_POINT('Ctrl Pts',(1.5604493439252,-0.797983948328948,6.22382703793116)) ;
#74406 = CARTESIAN_POINT('Ctrl Pts',(1.5675598412834,-0.783817595875971,6.23657317890588)) ;
#74407 = CARTESIAN_POINT('Ctrl Pts',(1.56873001705364,-0.781470558754527,
6.23913690798495)) ;
#74408 = CARTESIAN_POINT('Ctrl Pts',(1.57003590014195,-0.77884225486478,6.24379691046241)) ;
#74409 = CARTESIAN_POINT('Ctrl Pts',(1.57040611261523,-0.778094809706397,
6.24570740151285)) ;
#74410 = CARTESIAN_POINT('Ctrl Pts',(1.57062599767995,-0.777650791220551,
6.24850359260972)) ;
#74411 = CARTESIAN_POINT('Ctrl Pts',(1.57065531335762,-0.777591567997932,
6.24925253303392)) ;
#74412 = CARTESIAN_POINT('Ctrl Pts',(1.57065531335762,-0.777591567997932,
6.25)) ;
#74413 = CARTESIAN_POINT('Ctrl Pts',(1.354948802545,-1.11162966067026,6.16355970899623)) ;
#74414 = CARTESIAN_POINT('Ctrl Pts',(1.2691105239076,-1.21625665738258,6.15398004999797)) ;
#74415 = CARTESIAN_POINT('Ctrl Pts',(1.17146411011478,-1.31057075856948,6.1449103765824)) ;
#74416 = CARTESIAN_POINT('Ctrl Pts',(0.953918635023722,-1.47675496499653,
6.12533991001694)) ;
#74417 = CARTESIAN_POINT('Ctrl Pts',(0.834365619456194,-1.54744734708524,
6.1151689721293)) ;
#74418 = CARTESIAN_POINT('Ctrl Pts',(0.493385532353786,-1.69796606169852,
6.0876067703235)) ;
#74419 = CARTESIAN_POINT('Ctrl Pts',(0.2621558383588,-1.74866546389136,6.07037009501047)) ;
#74420 = CARTESIAN_POINT('Ctrl Pts',(-0.197627883205035,-1.75595205213961,
6.03874354709929)) ;
#74421 = CARTESIAN_POINT('Ctrl Pts',(-0.421687652843615,-1.716002974801,6.02249091157781)) ;
#74422 = CARTESIAN_POINT('Ctrl Pts',(-0.850618335952917,-1.55014782434877,
5.98848430427106)) ;
#74423 = CARTESIAN_POINT('Ctrl Pts',(-1.05005207636958,-1.42265205221592,
5.97124666237111)) ;
#74424 = CARTESIAN_POINT('Ctrl Pts',(-1.38054170467941,-1.10296105685791,
5.93961273069518)) ;
#74425 = CARTESIAN_POINT('Ctrl Pts',(-1.51086317209616,-0.916390969524942,
5.92337240531497)) ;
#74426 = CARTESIAN_POINT('Ctrl Pts',(-1.69720186521872,-0.495990785382188,
5.88936893726401)) ;
#74427 = CARTESIAN_POINT('Ctrl Pts',(-1.74825045640576,-0.264876556215191,
5.87213026828475)) ;
#74428 = CARTESIAN_POINT('Ctrl Pts',(-1.75251138476543,-0.0203541928781188,
5.85529970515546)) ;
#74429 = CARTESIAN_POINT('Ctrl Pts',(-1.7526,-0.0101753703444853,5.85460160544293)) ;
#74430 = CARTESIAN_POINT('Ctrl Pts',(-1.7526,-1.06163316679444E-14,5.85390625)) ;
#74431 = CARTESIAN_POINT('Origin',(3.10601593664312E-15,-2.12330153459561E-14,
-0.34726562499997)) ;
#74432 = CARTESIAN_POINT('',(-0.194635088948059,-1.22163646928425,0.0797567518094987)) ;
#74433 = CARTESIAN_POINT('Ctrl Pts',(-1.55774404735361E-13,-1.23704425180961,
0.0992187500000006)) ;
#74434 = CARTESIAN_POINT('Ctrl Pts',(-0.0650557921671749,-1.2370442518096,
0.0929202058933744)) ;
#74435 = CARTESIAN_POINT('Ctrl Pts',(-0.130120178037894,-1.23191519437095,
0.0864151383895563)) ;
#74436 = CARTESIAN_POINT('Ctrl Pts',(-0.194635088950127,-1.22163646928396,
0.0797567518093028)) ;
#74437 = CARTESIAN_POINT('Origin',(-2.4980018054066E-14,3.26683124995952E-13,
0.0797567518098535)) ;
#74438 = CARTESIAN_POINT('Ctrl Pts',(-3.31205160669424,-0.887893661760288,
6.793484)) ;
#74439 = CARTESIAN_POINT('Ctrl Pts',(-3.31287790153464,-0.884811388204761,
6.79777468341573)) ;
#74440 = CARTESIAN_POINT('Ctrl Pts',(-3.31364139250918,-0.881705147287936,
6.80206837154771)) ;
#74441 = CARTESIAN_POINT('Ctrl Pts',(-3.3271818086533,-0.821152481751811,
6.88564197720954)) ;
#74442 = CARTESIAN_POINT('Ctrl Pts',(-3.31839899815499,-0.75612836629395,
6.96625435392858)) ;
#74443 = CARTESIAN_POINT('Ctrl Pts',(-3.2794239181545,-0.707077062047013,
7.03908289042949)) ;
#74444 = CARTESIAN_POINT('Ctrl Pts',(-3.31205160669424,-0.887893661760288,
6.793484)) ;
#74445 = CARTESIAN_POINT('Ctrl Pts',(-3.31274522369532,-0.885306307663954,
6.79809343284722)) ;
#74446 = CARTESIAN_POINT('Ctrl Pts',(-3.31334303732996,-0.882699040456771,
6.80271791145202)) ;
#74447 = CARTESIAN_POINT('Ctrl Pts',(-3.32434030414173,-0.831838892965903,
6.89249111240127)) ;
#74448 = CARTESIAN_POINT('Ctrl Pts',(-3.30868757227878,-0.775373519472582,
6.97904841531997)) ;
#74449 = CARTESIAN_POINT('Ctrl Pts',(-3.26540522272929,-0.738492188311658,
7.04973176535319)) ;
#74450 = CARTESIAN_POINT('Ctrl Pts',(-3.31205160669424,-0.887893661760288,
6.793484)) ;
#74451 = CARTESIAN_POINT('Ctrl Pts',(-3.31261121114413,-0.885806205911472,
6.79841624482425)) ;
#74452 = CARTESIAN_POINT('Ctrl Pts',(-3.31307594580977,-0.883698810455709,
6.8033633352161)) ;
#74453 = CARTESIAN_POINT('Ctrl Pts',(-3.32193595542266,-0.842609793416927,
6.89941056353899)) ;
#74454 = CARTESIAN_POINT('Ctrl Pts',(-3.30625449205529,-0.797119135192663,
6.99229450465509)) ;
#74455 = CARTESIAN_POINT('Ctrl Pts',(-3.26888725785268,-0.772941191040195,
7.07185431702686)) ;
#74456 = CARTESIAN_POINT('Ctrl Pts',(-3.31205160669424,-0.887893661760288,
6.793484)) ;
#74457 = CARTESIAN_POINT('Ctrl Pts',(-3.31247680269833,-0.886307580938716,
6.79874217767331)) ;
#74458 = CARTESIAN_POINT('Ctrl Pts',(-3.31286385709175,-0.884707693083396,
6.8040040381699)) ;
#74459 = CARTESIAN_POINT('Ctrl Pts',(-3.31959859765461,-0.853484701399462,
6.90642242752541)) ;
#74460 = CARTESIAN_POINT('Ctrl Pts',(-3.31286250738096,-0.819472008973412,
7.00521187075637)) ;
#74461 = CARTESIAN_POINT('Ctrl Pts',(-3.2881405032392,-0.793313315480957,
7.09446231571417)) ;
#74462 = CARTESIAN_POINT('',(-3.2881405032392,-0.793313315480957,7.09446231571417)) ;
#74463 = CARTESIAN_POINT('',(-3.27942391815471,-0.707077062047147,7.03908289042914)) ;
#74464 = CARTESIAN_POINT('Origin',(-3.36081883130047,-0.724626630961913,7.09446231571417)) ;
#74465 = CARTESIAN_POINT('',(-3.31205160669424,-0.887893661760289,6.793484)) ;
#74466 = CARTESIAN_POINT('Ctrl Pts',(-3.2794239181545,-0.707077062047013,
7.03908289042949)) ;
#74467 = CARTESIAN_POINT('Ctrl Pts',(-3.31839899815499,-0.75612836629395,
6.96625435392858)) ;
#74468 = CARTESIAN_POINT('Ctrl Pts',(-3.3271818086533,-0.821152481751811,
6.88564197720954)) ;
#74469 = CARTESIAN_POINT('Ctrl Pts',(-3.31364139250918,-0.881705147287936,
6.80206837154771)) ;
#74470 = CARTESIAN_POINT('Ctrl Pts',(-3.31287790153464,-0.884811388204761,
6.79777468341573)) ;
#74471 = CARTESIAN_POINT('Ctrl Pts',(-3.31205160669424,-0.887893661760288,
6.793484)) ;
#74472 = CARTESIAN_POINT('Ctrl Pts',(-3.31205160669424,-0.887893661760289,
6.793484)) ;
#74473 = CARTESIAN_POINT('Ctrl Pts',(-3.31247680269833,-0.886307580938716,
6.79874217767331)) ;
#74474 = CARTESIAN_POINT('Ctrl Pts',(-3.31286385709175,-0.884707693083396,
6.8040040381699)) ;
#74475 = CARTESIAN_POINT('Ctrl Pts',(-3.31959859765461,-0.853484701399462,
6.90642242752541)) ;
#74476 = CARTESIAN_POINT('Ctrl Pts',(-3.31286250738096,-0.819472008973412,
7.00521187075637)) ;
#74477 = CARTESIAN_POINT('Ctrl Pts',(-3.2881405032392,-0.793313315480957,
7.09446231571417)) ;
#74478 = CARTESIAN_POINT('Ctrl Pts',(-3.25930415002282,-0.772122965994088,
7.15495237069481)) ;
#74479 = CARTESIAN_POINT('Ctrl Pts',(-3.27166340593034,-0.778151805203039,
7.1395492738358)) ;
#74480 = CARTESIAN_POINT('Ctrl Pts',(-3.28134410254902,-0.786121950190065,
7.11899842460839)) ;
#74481 = CARTESIAN_POINT('Ctrl Pts',(-3.28814050323922,-0.793313315480977,
7.0944623157141)) ;
#74482 = CARTESIAN_POINT('Ctrl Pts',(-3.24720304082971,-0.766220050630805,
7.13091195407385)) ;
#74483 = CARTESIAN_POINT('Ctrl Pts',(-3.25869714385255,-0.769669020390238,
7.11948103534319)) ;
#74484 = CARTESIAN_POINT('Ctrl Pts',(-3.26931499881139,-0.775745323042673,
7.10257847346906)) ;
#74485 = CARTESIAN_POINT('Ctrl Pts',(-3.27713864873267,-0.781672101514855,
7.0815434593213)) ;
#74486 = CARTESIAN_POINT('Ctrl Pts',(-3.23542257587948,-0.737017859268681,
7.08914722322202)) ;
#74487 = CARTESIAN_POINT('Ctrl Pts',(-3.24613293999889,-0.741135418665641,
7.08437187855016)) ;
#74488 = CARTESIAN_POINT('Ctrl Pts',(-3.25765493730861,-0.747264169147483,
7.07395698641591)) ;
#74489 = CARTESIAN_POINT('Ctrl Pts',(-3.26627246770002,-0.753460431697837,
7.05898639091382)) ;
#74490 = CARTESIAN_POINT('Ctrl Pts',(-3.24626907090961,-0.691101901539863,
7.07061000050612)) ;
#74491 = CARTESIAN_POINT('Ctrl Pts',(-3.25699307007247,-0.701213312565526,
7.06492336370951)) ;
#74492 = CARTESIAN_POINT('Ctrl Pts',(-3.26646853336989,-0.711672429614719,
7.05583711304386)) ;
#74493 = CARTESIAN_POINT('Ctrl Pts',(-3.27341590582957,-0.720540687589137,
7.04364669396793)) ;
#74494 = CARTESIAN_POINT('Ctrl Pts',(-3.25413500684155,-0.672122965994088,
7.06837618534741)) ;
#74495 = CARTESIAN_POINT('Ctrl Pts',(-3.2651569253511,-0.68462662701825,7.0606746369179)) ;
#74496 = CARTESIAN_POINT('Ctrl Pts',(-3.27351027276397,-0.697039528212523,
7.05095544131491)) ;
#74497 = CARTESIAN_POINT('Ctrl Pts',(-3.27942391815468,-0.707077062047158,
7.03908289042919)) ;
#74498 = CARTESIAN_POINT('',(-3.25930415002282,-0.772122965994088,7.15495237069481)) ;
#74499 = CARTESIAN_POINT('Ctrl Pts',(-3.28814050323922,-0.793313315480977,
7.0944623157141)) ;
#74500 = CARTESIAN_POINT('Ctrl Pts',(-3.28134410254902,-0.786121950190065,
7.11899842460839)) ;
#74501 = CARTESIAN_POINT('Ctrl Pts',(-3.27166340593034,-0.778151805203039,
7.1395492738358)) ;
#74502 = CARTESIAN_POINT('Ctrl Pts',(-3.25930415002282,-0.772122965994088,
7.15495237069481)) ;
#74503 = CARTESIAN_POINT('',(-3.25413500684155,-0.672122965994088,7.06837618534741)) ;
#74504 = CARTESIAN_POINT('Origin',(-3.30314612486771,-0.682245931988176,7.15495237069481)) ;
#74505 = CARTESIAN_POINT('Ctrl Pts',(-3.25413500684155,-0.672122965994088,
7.06837618534741)) ;
#74506 = CARTESIAN_POINT('Ctrl Pts',(-3.25939413791001,-0.678089113548593,
7.06470137568647)) ;
#74507 = CARTESIAN_POINT('Ctrl Pts',(-3.26403592778485,-0.684033341438776,
7.06055993267684)) ;
#74508 = CARTESIAN_POINT('Ctrl Pts',(-3.27227350301816,-0.695529889843682,
7.05122867472026)) ;
#74509 = CARTESIAN_POINT('Ctrl Pts',(-3.27584190801,-0.701066725671648,7.04601233351152)) ;
#74510 = CARTESIAN_POINT('Ctrl Pts',(-3.27902209145488,-0.706397160161627,
7.03988142131546)) ;
#74511 = CARTESIAN_POINT('Ctrl Pts',(-3.27922442992735,-0.706738460440355,
7.03948339366763)) ;
#74512 = CARTESIAN_POINT('Ctrl Pts',(-3.27942391815467,-0.707077062047157,
7.03908289042919)) ;
#74513 = CARTESIAN_POINT('Ctrl Pts',(-3.25413500684155,-0.672122965994087,
7.06837618534741)) ;
#74514 = CARTESIAN_POINT('Ctrl Pts',(-3.24907828834912,-0.668116125762003,
7.07170731541641)) ;
#74515 = CARTESIAN_POINT('Ctrl Pts',(-3.23589756364382,-0.660507101185359,
7.07825767676847)) ;
#74516 = CARTESIAN_POINT('Ctrl Pts',(-3.21994984969872,-0.659191608936345,
7.08122103082289)) ;
#74517 = CARTESIAN_POINT('Ctrl Pts',(-3.2105035504766,-0.660979117346627,
7.08167176697949)) ;
#74518 = CARTESIAN_POINT('Ctrl Pts',(-3.24364709226562,-0.697428213388454,
7.07135460555903)) ;
#74519 = CARTESIAN_POINT('Ctrl Pts',(-3.23904198217673,-0.694613604341688,
7.07381433044803)) ;
#74520 = CARTESIAN_POINT('Ctrl Pts',(-3.22806793638566,-0.689730698218501,
7.07820430178644)) ;
#74521 = CARTESIAN_POINT('Ctrl Pts',(-3.21711227111321,-0.689553339863551,
7.08049944622424)) ;
#74522 = CARTESIAN_POINT('Ctrl Pts',(-3.21048830525436,-0.691091935293639,
7.08136471265295)) ;
#74523 = CARTESIAN_POINT('Ctrl Pts',(-3.23575890408185,-0.743524350516924,
7.09478029250273)) ;
#74524 = CARTESIAN_POINT('Ctrl Pts',(-3.23142097756856,-0.74257695355463,
7.09766695337376)) ;
#74525 = CARTESIAN_POINT('Ctrl Pts',(-3.22221828421189,-0.741823967860394,
7.10251922930311)) ;
#74526 = CARTESIAN_POINT('Ctrl Pts',(-3.21582930459776,-0.742834159269564,
7.10502824890571)) ;
#74527 = CARTESIAN_POINT('Ctrl Pts',(-3.21172314782629,-0.743501302288172,
7.10623570350962)) ;
#74528 = CARTESIAN_POINT('Ctrl Pts',(-3.25022831812798,-0.767695779471626,
7.13692205822909)) ;
#74529 = CARTESIAN_POINT('Ctrl Pts',(-3.24530748822128,-0.765971442670609,
7.14245586827297)) ;
#74530 = CARTESIAN_POINT('Ctrl Pts',(-3.23346592056584,-0.762891866825046,
7.15309078996572)) ;
#74531 = CARTESIAN_POINT('Ctrl Pts',(-3.22141912805696,-0.761902076472111,
7.15799343781877)) ;
#74532 = CARTESIAN_POINT('Ctrl Pts',(-3.21434217223136,-0.761999999999958,
7.15898553043246)) ;
#74533 = CARTESIAN_POINT('Ctrl Pts',(-3.25930415002282,-0.772122965994088,
7.15495237069481)) ;
#74534 = CARTESIAN_POINT('Ctrl Pts',(-3.253958434241,-0.769515328354208,7.16161463083283)) ;
#74535 = CARTESIAN_POINT('Ctrl Pts',(-3.24030166703836,-0.764233790350221,
7.17471535353693)) ;
#74536 = CARTESIAN_POINT('Ctrl Pts',(-3.22454046181232,-0.762000000000339,
7.18064206164579)) ;
#74537 = CARTESIAN_POINT('Ctrl Pts',(-3.21546217518166,-0.762,7.18154353395898)) ;
#74538 = CARTESIAN_POINT('',(-3.2154621751798,-0.762,7.18154353395898)) ;
#74539 = CARTESIAN_POINT('',(-3.2105035504766,-0.660979117346627,7.08167176697949)) ;
#74540 = CARTESIAN_POINT('Origin',(-3.2154621751854,-0.662,7.18154353395898)) ;
#74541 = CARTESIAN_POINT('Ctrl Pts',(-3.2105035504766,-0.660979117346627,
7.08167176697949)) ;
#74542 = CARTESIAN_POINT('Ctrl Pts',(-3.21994984969872,-0.659191608936345,
7.08122103082289)) ;
#74543 = CARTESIAN_POINT('Ctrl Pts',(-3.23589756364382,-0.660507101185359,
7.07825767676847)) ;
#74544 = CARTESIAN_POINT('Ctrl Pts',(-3.24907828834912,-0.668116125762003,
7.07170731541641)) ;
#74545 = CARTESIAN_POINT('Ctrl Pts',(-3.25413500684155,-0.672122965994087,
7.06837618534741)) ;
#74546 = CARTESIAN_POINT('Ctrl Pts',(-3.25930415002282,-0.772122965994088,
7.15495237069481)) ;
#74547 = CARTESIAN_POINT('Ctrl Pts',(-3.253958434241,-0.769515328354208,7.16161463083283)) ;
#74548 = CARTESIAN_POINT('Ctrl Pts',(-3.24030166703836,-0.764233790350221,
7.17471535353693)) ;
#74549 = CARTESIAN_POINT('Ctrl Pts',(-3.22454046181232,-0.762000000000339,
7.18064206164579)) ;
#74550 = CARTESIAN_POINT('Ctrl Pts',(-3.21546217518166,-0.762,7.18154353395898)) ;
#74551 = CARTESIAN_POINT('Ctrl Pts',(-3.2105035504766,-0.660979117346627,
7.08167176697949)) ;
#74552 = CARTESIAN_POINT('Ctrl Pts',(-3.20871214489261,-0.66131810222033,
7.08175724503273)) ;
#74553 = CARTESIAN_POINT('Ctrl Pts',(-3.20691819492506,-0.661658530855223,
7.0818)) ;
#74554 = CARTESIAN_POINT('Ctrl Pts',(-3.20512388881539,-0.662,7.0818)) ;
#74555 = CARTESIAN_POINT('Ctrl Pts',(-3.21048830525548,-0.691091935293675,
7.08136471265289)) ;
#74556 = CARTESIAN_POINT('Ctrl Pts',(-3.20871266627196,-0.691367100691539,
7.08155544690455)) ;
#74557 = CARTESIAN_POINT('Ctrl Pts',(-3.20691291140055,-0.691643821063274,
7.08169470978418)) ;
#74558 = CARTESIAN_POINT('Ctrl Pts',(-3.20512388881539,-0.691919930034189,
7.0818)) ;
#74559 = CARTESIAN_POINT('Ctrl Pts',(-3.21172314486594,-0.743501373347166,
7.10623564382334)) ;
#74560 = CARTESIAN_POINT('Ctrl Pts',(-3.2095315878856,-0.743584576017368,
7.1065058196023)) ;
#74561 = CARTESIAN_POINT('Ctrl Pts',(-3.20733490885682,-0.743666470692696,
7.10672585564236)) ;
#74562 = CARTESIAN_POINT('Ctrl Pts',(-3.20512388881539,-0.743749639050895,
7.1068882100183)) ;
#74563 = CARTESIAN_POINT('Ctrl Pts',(-3.2143421722351,-0.762,7.15898553043244)) ;
#74564 = CARTESIAN_POINT('Ctrl Pts',(-3.21127367849934,-0.761999102403065,
7.15918594173638)) ;
#74565 = CARTESIAN_POINT('Ctrl Pts',(-3.20820121468723,-0.762000880498864,
7.15931169382832)) ;
#74566 = CARTESIAN_POINT('Ctrl Pts',(-3.20512388881539,-0.762,7.15936005247436)) ;
#74567 = CARTESIAN_POINT('Ctrl Pts',(-3.2154621751854,-0.762,7.18154353395898)) ;
#74568 = CARTESIAN_POINT('Ctrl Pts',(-3.21201894456551,-0.762,7.18171449006546)) ;
#74569 = CARTESIAN_POINT('Ctrl Pts',(-3.20857144403868,-0.762,7.1818)) ;
#74570 = CARTESIAN_POINT('Ctrl Pts',(-3.20512388881539,-0.762,7.1818)) ;
#74571 = CARTESIAN_POINT('',(-3.20512388881539,-0.762,7.1818)) ;
#74572 = CARTESIAN_POINT('',(-3.2051238888154,-0.662,7.0818)) ;
#74573 = CARTESIAN_POINT('Origin',(-3.20512388881539,-0.662,7.1818)) ;
#74574 = CARTESIAN_POINT('Origin',(-3.2048792341882,-0.66383132792774,7.00284754580388)) ;
#74575 = CARTESIAN_POINT('Origin',(-3.20581132767206,-0.762,7.0244442135551)) ;
#74576 = CARTESIAN_POINT('Ctrl Pts',(-3.10768758242201,-0.761999999110866,
7.18178789612072)) ;
#74577 = CARTESIAN_POINT('Ctrl Pts',(-3.10820350632125,-0.762,7.1818)) ;
#74578 = CARTESIAN_POINT('Ctrl Pts',(-3.10871943022056,-0.762,7.1818)) ;
#74579 = CARTESIAN_POINT('Ctrl Pts',(-3.11460888995322,-0.762,7.18179999999999)) ;
#74580 = CARTESIAN_POINT('Ctrl Pts',(-3.12266919370325,-0.762,7.1818)) ;
#74581 = CARTESIAN_POINT('Ctrl Pts',(-3.1374980096349,-0.762,7.1818)) ;
#74582 = CARTESIAN_POINT('Ctrl Pts',(-3.1469532897332,-0.762,7.1818)) ;
#74583 = CARTESIAN_POINT('Ctrl Pts',(-3.15372180191481,-0.762,7.1818)) ;
#74584 = CARTESIAN_POINT('Ctrl Pts',(-3.10768758242201,-0.761999999110866,
7.18178789612072)) ;
#74585 = CARTESIAN_POINT('Ctrl Pts',(-3.10820350632198,-0.761999971546708,
7.18162961113284)) ;
#74586 = CARTESIAN_POINT('Ctrl Pts',(-3.10871943022056,-0.762,7.1814602658962)) ;
#74587 = CARTESIAN_POINT('Ctrl Pts',(-3.11460888995322,-0.762,7.17949782470739)) ;
#74588 = CARTESIAN_POINT('Ctrl Pts',(-3.12266919370325,-0.762,7.17631957154599)) ;
#74589 = CARTESIAN_POINT('Ctrl Pts',(-3.1374980096349,-0.762,7.16854333762089)) ;
#74590 = CARTESIAN_POINT('Ctrl Pts',(-3.1469532897332,-0.762,7.16306055736286)) ;
#74591 = CARTESIAN_POINT('Ctrl Pts',(-3.15372180191481,-0.762,7.16076336222311)) ;
#74592 = CARTESIAN_POINT('Ctrl Pts',(-3.10768758242201,-0.761999999110866,
7.18178789612072)) ;
#74593 = CARTESIAN_POINT('Ctrl Pts',(-3.10820350632112,-0.761999937262456,
7.18142430431638)) ;
#74594 = CARTESIAN_POINT('Ctrl Pts',(-3.10871943022057,-0.761997356649989,
7.18105351783653)) ;
#74595 = CARTESIAN_POINT('Ctrl Pts',(-3.11460888995317,-0.761976495217826,
7.17672655551623)) ;
#74596 = CARTESIAN_POINT('Ctrl Pts',(-3.12266919370324,-0.761694542972285,
7.16985111380514)) ;
#74597 = CARTESIAN_POINT('Ctrl Pts',(-3.13749800963488,-0.759216921298734,
7.15262801012254)) ;
#74598 = CARTESIAN_POINT('Ctrl Pts',(-3.14695328973321,-0.755825896474783,
7.14096328750365)) ;
#74599 = CARTESIAN_POINT('Ctrl Pts',(-3.15372180191481,-0.753693441915688,
7.13527073955965)) ;
#74600 = CARTESIAN_POINT('Ctrl Pts',(-3.10768758242201,-0.761999999110866,
7.18178789612072)) ;
#74601 = CARTESIAN_POINT('Ctrl Pts',(-3.10820350632311,-0.761999900310011,
7.18120301937144)) ;
#74602 = CARTESIAN_POINT('Ctrl Pts',(-3.10871943022057,-0.761994331607278,
7.18061138592162)) ;
#74603 = CARTESIAN_POINT('Ctrl Pts',(-3.11460888995315,-0.761878231569385,
7.17374285180056)) ;
#74604 = CARTESIAN_POINT('Ctrl Pts',(-3.12266919370323,-0.760928454763849,
7.16271105773673)) ;
#74605 = CARTESIAN_POINT('Ctrl Pts',(-3.13749800963488,-0.752712459225539,
7.13650432564738)) ;
#74606 = CARTESIAN_POINT('Ctrl Pts',(-3.14695328973321,-0.74201847270757,
7.1206541791479)) ;
#74607 = CARTESIAN_POINT('Ctrl Pts',(-3.15372180191481,-0.735935879405177,
7.11434234885099)) ;
#74608 = CARTESIAN_POINT('Ctrl Pts',(-3.10768758242201,-0.761999999110866,
7.18178789612072)) ;
#74609 = CARTESIAN_POINT('Ctrl Pts',(-3.10820350632367,-0.761999890371836,
7.18114350589661)) ;
#74610 = CARTESIAN_POINT('Ctrl Pts',(-3.10871943022057,-0.761993397983058,
7.18049224493129)) ;
#74611 = CARTESIAN_POINT('Ctrl Pts',(-3.11460888995315,-0.761848304054905,
7.17294119572008)) ;
#74612 = CARTESIAN_POINT('Ctrl Pts',(-3.12266919370323,-0.760692288773643,
7.1607896050519)) ;
#74613 = CARTESIAN_POINT('Ctrl Pts',(-3.13749800963488,-0.750735669662562,
7.13225210589726)) ;
#74614 = CARTESIAN_POINT('Ctrl Pts',(-3.14695328973321,-0.737874325756503,
7.11550492633058)) ;
#74615 = CARTESIAN_POINT('Ctrl Pts',(-3.15372180191481,-0.730681059791499,
7.1091778777056)) ;
#74616 = CARTESIAN_POINT('Ctrl Pts',(-3.10768758242201,-0.761999999110866,
7.18178789612072)) ;
#74617 = CARTESIAN_POINT('Ctrl Pts',(-3.10820350632406,-0.761999885411581,
7.18111380205138)) ;
#74618 = CARTESIAN_POINT('Ctrl Pts',(-3.10871943022057,-0.761992965550236,
7.18043260514312)) ;
#74619 = CARTESIAN_POINT('Ctrl Pts',(-3.11460888995315,-0.761831627738708,
7.17254121063549)) ;
#74620 = CARTESIAN_POINT('Ctrl Pts',(-3.12266919370323,-0.760566154944648,
7.1598249400892)) ;
#74621 = CARTESIAN_POINT('Ctrl Pts',(-3.13749800963487,-0.749690046465535,
7.13015050138915)) ;
#74622 = CARTESIAN_POINT('Ctrl Pts',(-3.14695328973321,-0.735691643270758,
7.11300325031031)) ;
#74623 = CARTESIAN_POINT('Ctrl Pts',(-3.15372180191481,-0.727929085659609,
7.10673826884187)) ;
#74624 = CARTESIAN_POINT('Ctrl Pts',(-3.10768758242201,-0.761999999110866,
7.18178789612072)) ;
#74625 = CARTESIAN_POINT('Ctrl Pts',(-3.10820350632437,-0.761999882300983,
7.18109517463631)) ;
#74626 = CARTESIAN_POINT('Ctrl Pts',(-3.10871943022057,-0.761992726760589,
7.18039509107439)) ;
#74627 = CARTESIAN_POINT('Ctrl Pts',(-3.11460888995315,-0.761820320860478,
7.17229047989692)) ;
#74628 = CARTESIAN_POINT('Ctrl Pts',(-3.12266919370323,-0.760484017917808,
7.15921737584589)) ;
#74629 = CARTESIAN_POINT('Ctrl Pts',(-3.13749800963488,-0.749015451777574,
7.12883825022165)) ;
#74630 = CARTESIAN_POINT('Ctrl Pts',(-3.14695328973321,-0.734287500072791,
7.11145355959439)) ;
#74631 = CARTESIAN_POINT('Ctrl Pts',(-3.15372180191481,-0.726166969088686,
7.10525117650479)) ;
#74632 = CARTESIAN_POINT('Ctrl Pts',(-3.10768758242201,-0.761999999110866,
7.18178789612072)) ;
#74633 = CARTESIAN_POINT('Ctrl Pts',(-3.10820350632452,-0.761999880603801,
7.18108501128053)) ;
#74634 = CARTESIAN_POINT('Ctrl Pts',(-3.10871943022057,-0.761992578089339,
7.18037464637613)) ;
#74635 = CARTESIAN_POINT('Ctrl Pts',(-3.11460888995315,-0.761814227722725,
7.1721536831723)) ;
#74636 = CARTESIAN_POINT('Ctrl Pts',(-3.12266919370323,-0.760438384835969,
7.15888643811152)) ;
#74637 = CARTESIAN_POINT('Ctrl Pts',(-3.13749800963488,-0.748640047873434,
7.12812617670508)) ;
#74638 = CARTESIAN_POINT('Ctrl Pts',(-3.14695328973321,-0.733507903613573,
7.11062229391851)) ;
#74639 = CARTESIAN_POINT('Ctrl Pts',(-3.15372180191481,-0.725190242268012,
7.10445781568441)) ;
#74640 = CARTESIAN_POINT('Ctrl Pts',(-3.10768758242201,-0.761999999110866,
7.18178789612072)) ;
#74641 = CARTESIAN_POINT('Ctrl Pts',(-3.10820350632465,-0.761999879617918,
7.18107910744813)) ;
#74642 = CARTESIAN_POINT('Ctrl Pts',(-3.10871943022057,-0.761992519832539,
7.18036270141455)) ;
#74643 = CARTESIAN_POINT('Ctrl Pts',(-3.11460888995315,-0.761810241967301,
7.17207425568446)) ;
#74644 = CARTESIAN_POINT('Ctrl Pts',(-3.12266919370323,-0.76041106646782,
7.15869248076817)) ;
#74645 = CARTESIAN_POINT('Ctrl Pts',(-3.13749800963488,-0.74841848455698,
7.12771246966564)) ;
#74646 = CARTESIAN_POINT('Ctrl Pts',(-3.14695328973321,-0.733048178705464,
7.11013808561189)) ;
#74647 = CARTESIAN_POINT('Ctrl Pts',(-3.15372180191481,-0.724616601445939,
7.10400482490522)) ;
#74648 = CARTESIAN_POINT('',(-3.14953687287002,-0.730523456132445,7.10896775467099)) ;
#74649 = CARTESIAN_POINT('',(-3.14953687287001,-0.762,7.1818)) ;
#74650 = CARTESIAN_POINT('Origin',(-3.14953687287001,-0.662,7.1818)) ;
#74651 = CARTESIAN_POINT('',(-3.10768474164716,-0.761999999558836,7.18179289868234)) ;
#74652 = CARTESIAN_POINT('',(-3.14953687287001,-0.762,7.1818)) ;
#74653 = CARTESIAN_POINT('Ctrl Pts',(-3.10768189955247,-0.761999999565641,
7.18179079992629)) ;
#74654 = CARTESIAN_POINT('Ctrl Pts',(-3.11550396931728,-0.7619989990746,7.17119510360894)) ;
#74655 = CARTESIAN_POINT('Ctrl Pts',(-3.12158404061982,-0.760269612060714,
7.1602507583022)) ;
#74656 = CARTESIAN_POINT('Ctrl Pts',(-3.13169750131939,-0.753543279843757,
7.14032498264226)) ;
#74657 = CARTESIAN_POINT('Ctrl Pts',(-3.13586387425679,-0.748880446529675,
7.13126215380791)) ;
#74658 = CARTESIAN_POINT('Ctrl Pts',(-3.14321743559729,-0.739229351300546,
7.11795970925599)) ;
#74659 = CARTESIAN_POINT('Ctrl Pts',(-3.1461798989977,-0.735037333748867,
7.11321458920752)) ;
#74660 = CARTESIAN_POINT('Ctrl Pts',(-3.14953687287001,-0.730523456132447,
7.10896775467099)) ;
#74661 = CARTESIAN_POINT('Ctrl Pts',(-3.14953687287001,-0.762,7.1818)) ;
#74662 = CARTESIAN_POINT('Ctrl Pts',(-3.15676355558523,-0.762,7.1818)) ;
#74663 = CARTESIAN_POINT('Ctrl Pts',(-3.16399023830045,-0.762,7.1818)) ;
#74664 = CARTESIAN_POINT('Ctrl Pts',(-3.17121692101567,-0.762,7.1818)) ;
#74665 = CARTESIAN_POINT('Ctrl Pts',(-3.14953687287001,-0.762,7.16625960724294)) ;
#74666 = CARTESIAN_POINT('Ctrl Pts',(-3.15676355558523,-0.762015837610647,
7.16371429760845)) ;
#74667 = CARTESIAN_POINT('Ctrl Pts',(-3.16399023830045,-0.761980537877959,
7.16173716654572)) ;
#74668 = CARTESIAN_POINT('Ctrl Pts',(-3.17121692101567,-0.762,7.16049051462243)) ;
#74669 = CARTESIAN_POINT('Ctrl Pts',(-3.14953687287001,-0.755540893518778,
7.1390837819811)) ;
#74670 = CARTESIAN_POINT('Ctrl Pts',(-3.15676355558523,-0.75338304373689,
7.13211431434399)) ;
#74671 = CARTESIAN_POINT('Ctrl Pts',(-3.16399023830045,-0.751152261593369,
7.1266719591844)) ;
#74672 = CARTESIAN_POINT('Ctrl Pts',(-3.17121692101567,-0.749661462765229,
7.12329552595192)) ;
#74673 = CARTESIAN_POINT('Ctrl Pts',(-3.14953687287002,-0.739012268865877,
7.11695436533126)) ;
#74674 = CARTESIAN_POINT('Ctrl Pts',(-3.15676355558523,-0.73174878770295,
7.10798226702609)) ;
#74675 = CARTESIAN_POINT('Ctrl Pts',(-3.16399023830045,-0.724623549182784,
7.10220324165009)) ;
#74676 = CARTESIAN_POINT('Ctrl Pts',(-3.17121692101567,-0.720057683295034,
7.09882570651471)) ;
#74677 = CARTESIAN_POINT('Ctrl Pts',(-3.14953687287002,-0.730523456132442,
7.10896775467099)) ;
#74678 = CARTESIAN_POINT('Ctrl Pts',(-3.15676355558523,-0.720806263628133,
7.09982543575316)) ;
#74679 = CARTESIAN_POINT('Ctrl Pts',(-3.16399023830045,-0.711535796534348,
7.09468761566807)) ;
#74680 = CARTESIAN_POINT('Ctrl Pts',(-3.17121692101567,-0.705680904617081,
7.09184457452808)) ;
#74681 = CARTESIAN_POINT('',(-3.17121692101567,-0.705680904617081,7.09184457452808)) ;
#74682 = CARTESIAN_POINT('',(-3.17121692101567,-0.762,7.1818)) ;
#74683 = CARTESIAN_POINT('Origin',(-3.17121692101567,-0.662,7.1818)) ;
#74684 = CARTESIAN_POINT('',(-3.17121692101567,-0.762,7.1818)) ;
#74685 = CARTESIAN_POINT('Ctrl Pts',(-3.14953687287002,-0.730523456132445,
7.10896775467099)) ;
#74686 = CARTESIAN_POINT('Ctrl Pts',(-3.15676355558523,-0.720806263628138,
7.09982543575316)) ;
#74687 = CARTESIAN_POINT('Ctrl Pts',(-3.16399023830045,-0.711535796534354,
7.09468761566807)) ;
#74688 = CARTESIAN_POINT('Ctrl Pts',(-3.17121692101566,-0.705680904617088,
7.09184457452809)) ;
#74689 = CARTESIAN_POINT('Ctrl Pts',(-3.20512388881539,-0.661999999999999,
7.0818)) ;
#74690 = CARTESIAN_POINT('Ctrl Pts',(-3.20472023443683,-0.662977161851642,
7.0818)) ;
#74691 = CARTESIAN_POINT('Ctrl Pts',(-3.20391292567969,-0.664831438935813,
7.0818281326209)) ;
#74692 = CARTESIAN_POINT('Ctrl Pts',(-3.20270196254399,-0.667381960953699,
7.08193509059619)) ;
#74693 = CARTESIAN_POINT('Ctrl Pts',(-3.20149099940828,-0.669755131272187,
7.08209149598161)) ;
#74694 = CARTESIAN_POINT('Ctrl Pts',(-3.1974544556226,-0.67713609635116,7.08275930201881)) ;
#74695 = CARTESIAN_POINT('Ctrl Pts',(-3.18736309615839,-0.691331994006399,
7.08558723772616)) ;
#74696 = CARTESIAN_POINT('Ctrl Pts',(-3.17767539107276,-0.700448400904756,
7.08930375506814)) ;
#74697 = CARTESIAN_POINT('Ctrl Pts',(-3.17121692101566,-0.705680904617081,
7.09184457452809)) ;
#74698 = CARTESIAN_POINT('Ctrl Pts',(-3.20512388881539,-0.691919930034188,
7.0818)) ;
#74699 = CARTESIAN_POINT('Ctrl Pts',(-3.20472023443683,-0.692710054581018,
7.08210130272039)) ;
#74700 = CARTESIAN_POINT('Ctrl Pts',(-3.20391292567969,-0.694201326478369,
7.08268816612552)) ;
#74701 = CARTESIAN_POINT('Ctrl Pts',(-3.20270196254399,-0.696232474572727,
7.08353635047393)) ;
#74702 = CARTESIAN_POINT('Ctrl Pts',(-3.20149099940828,-0.698105863873827,
7.08436153702967)) ;
#74703 = CARTESIAN_POINT('Ctrl Pts',(-3.1974544556226,-0.703886507865681,
7.0870216034983)) ;
#74704 = CARTESIAN_POINT('Ctrl Pts',(-3.18736309615839,-0.714604348638996,
7.09308139393355)) ;
#74705 = CARTESIAN_POINT('Ctrl Pts',(-3.17767539107276,-0.721164846104133,
7.09796452550531)) ;
#74706 = CARTESIAN_POINT('Ctrl Pts',(-3.17121692101566,-0.724849942854352,
7.10115275051025)) ;
#74707 = CARTESIAN_POINT('Ctrl Pts',(-3.20512388881539,-0.743749664724923,
7.10688818862076)) ;
#74708 = CARTESIAN_POINT('Ctrl Pts',(-3.20472023443683,-0.743987662646956,
7.10735278843905)) ;
#74709 = CARTESIAN_POINT('Ctrl Pts',(-3.20391292567969,-0.744433776876774,
7.10823521710843)) ;
#74710 = CARTESIAN_POINT('Ctrl Pts',(-3.20270196254399,-0.745035453736892,
7.10945017013558)) ;
#74711 = CARTESIAN_POINT('Ctrl Pts',(-3.20149099940828,-0.745586219467376,
7.11058176595391)) ;
#74712 = CARTESIAN_POINT('Ctrl Pts',(-3.1974544556226,-0.747266305413514,
7.11411357106582)) ;
#74713 = CARTESIAN_POINT('Ctrl Pts',(-3.18736309615839,-0.750270097373977,
7.12099360901837)) ;
#74714 = CARTESIAN_POINT('Ctrl Pts',(-3.17767539107276,-0.751952696995019,
7.1257288226096)) ;
#74715 = CARTESIAN_POINT('Ctrl Pts',(-3.17121692101566,-0.75291924171095,
7.12849905621401)) ;
#74716 = CARTESIAN_POINT('Ctrl Pts',(-3.20512388881539,-0.762,7.15936005247436)) ;
#74717 = CARTESIAN_POINT('Ctrl Pts',(-3.20472023443683,-0.761997480329003,
7.1594984375227)) ;
#74718 = CARTESIAN_POINT('Ctrl Pts',(-3.20391292567969,-0.761993348192325,
7.1597613592822)) ;
#74719 = CARTESIAN_POINT('Ctrl Pts',(-3.20270196254399,-0.76198811015298,
7.16012343058549)) ;
#74720 = CARTESIAN_POINT('Ctrl Pts',(-3.20149099940828,-0.761983122426318,
7.16046067089829)) ;
#74721 = CARTESIAN_POINT('Ctrl Pts',(-3.1974544556226,-0.761972743237157,
7.16151393713481)) ;
#74722 = CARTESIAN_POINT('Ctrl Pts',(-3.18736309615839,-0.761958192393428,
7.16356744125941)) ;
#74723 = CARTESIAN_POINT('Ctrl Pts',(-3.17767539107276,-0.762003840410888,
7.16498934960751)) ;
#74724 = CARTESIAN_POINT('Ctrl Pts',(-3.17121692101567,-0.762,7.16581788596682)) ;
#74725 = CARTESIAN_POINT('Ctrl Pts',(-3.20512388881539,-0.762,7.1818)) ;
#74726 = CARTESIAN_POINT('Ctrl Pts',(-3.20472023443683,-0.762,7.1818)) ;
#74727 = CARTESIAN_POINT('Ctrl Pts',(-3.20391292567969,-0.762,7.1818)) ;
#74728 = CARTESIAN_POINT('Ctrl Pts',(-3.20270196254399,-0.762,7.1818)) ;
#74729 = CARTESIAN_POINT('Ctrl Pts',(-3.20149099940828,-0.762,7.1818)) ;
#74730 = CARTESIAN_POINT('Ctrl Pts',(-3.1974544556226,-0.762,7.1818)) ;
#74731 = CARTESIAN_POINT('Ctrl Pts',(-3.18736309615839,-0.762,7.1818)) ;
#74732 = CARTESIAN_POINT('Ctrl Pts',(-3.17767539107276,-0.762,7.1818)) ;
#74733 = CARTESIAN_POINT('Ctrl Pts',(-3.17121692101567,-0.762,7.1818)) ;
#74734 = CARTESIAN_POINT('Ctrl Pts',(-3.17121692101567,-0.705680904617077,
7.09184457452808)) ;
#74735 = CARTESIAN_POINT('Ctrl Pts',(-3.17444615604422,-0.703064652760914,
7.09057416479811)) ;
#74736 = CARTESIAN_POINT('Ctrl Pts',(-3.17767539107276,-0.700235809090658,
7.0893360813593)) ;
#74737 = CARTESIAN_POINT('Ctrl Pts',(-3.18371137404519,-0.694285563440634,
7.08710907960385)) ;
#74738 = CARTESIAN_POINT('Ctrl Pts',(-3.18651812198907,-0.691250186366111,
7.08610870787848)) ;
#74739 = CARTESIAN_POINT('Ctrl Pts',(-3.18974735701762,-0.687336965752854,
7.08506159474165)) ;
#74740 = CARTESIAN_POINT('Ctrl Pts',(-3.19016984410228,-0.686816704289863,
7.08492674037565)) ;
#74741 = CARTESIAN_POINT('Ctrl Pts',(-3.19239331865279,-0.684033333884775,
7.08422985303717)) ;
#74742 = CARTESIAN_POINT('Ctrl Pts',(-3.19419430611863,-0.68162375111484,
7.08370642162001)) ;
#74743 = CARTESIAN_POINT('Ctrl Pts',(-3.19742354114718,-0.676803085814083,
7.082878067165)) ;
#74744 = CARTESIAN_POINT('Ctrl Pts',(-3.19885178870988,-0.674495257467968,
7.0825507746911)) ;
#74745 = CARTESIAN_POINT('Ctrl Pts',(-3.20068369065114,-0.67123138690268,
7.08222438102226)) ;
#74746 = CARTESIAN_POINT('Ctrl Pts',(-3.20108734502971,-0.670493217907312,
7.08215837537037)) ;
#74747 = CARTESIAN_POINT('Ctrl Pts',(-3.20189465378685,-0.66896403985744,
7.08203983631671)) ;
#74748 = CARTESIAN_POINT('Ctrl Pts',(-3.20229830816542,-0.668173012083411,
7.08198732917139)) ;
#74749 = CARTESIAN_POINT('Ctrl Pts',(-3.20310561692256,-0.666531791312407,
7.08189935834229)) ;
#74750 = CARTESIAN_POINT('Ctrl Pts',(-3.20350927130112,-0.665681610657713,
7.08186384002979)) ;
#74751 = CARTESIAN_POINT('Ctrl Pts',(-3.20431658005826,-0.663904297940051,
7.08181418112562)) ;
#74752 = CARTESIAN_POINT('Ctrl Pts',(-3.20472023443683,-0.662977161851642,
7.0818)) ;
#74753 = CARTESIAN_POINT('Ctrl Pts',(-3.20512388881539,-0.661999999999999,
7.0818)) ;
#74754 = CARTESIAN_POINT('',(-3.20512388881539,-0.762,7.1818)) ;
#74755 = CARTESIAN_POINT('Ctrl Pts',(-3.28702640935013,-0.678916496982596,
7.03662526114754)) ;
#74756 = CARTESIAN_POINT('Ctrl Pts',(-3.28505420805782,-0.68846506114502,
7.03662526114754)) ;
#74757 = CARTESIAN_POINT('Ctrl Pts',(-3.28250316889159,-0.697892264769899,
7.03746773980168)) ;
#74758 = CARTESIAN_POINT('Ctrl Pts',(-3.27942391815487,-0.707077062047443,
7.03908289042881)) ;
#74759 = CARTESIAN_POINT('Ctrl Pts',(-3.27867914825951,-0.677192417966096,
7.04962706151189)) ;
#74760 = CARTESIAN_POINT('Ctrl Pts',(-3.27680440972048,-0.685870309279993,
7.04975105769206)) ;
#74761 = CARTESIAN_POINT('Ctrl Pts',(-3.2743643275819,-0.694431071838909,
7.05063960533657)) ;
#74762 = CARTESIAN_POINT('Ctrl Pts',(-3.27140856314625,-0.702764080010726,
7.05223037429132)) ;
#74763 = CARTESIAN_POINT('Ctrl Pts',(-3.26731641278835,-0.674845509970385,
7.06059580486523)) ;
#74764 = CARTESIAN_POINT('Ctrl Pts',(-3.26548227953707,-0.682632591536585,
7.06080383849016)) ;
#74765 = CARTESIAN_POINT('Ctrl Pts',(-3.26310082825167,-0.69030704612225,
7.06169180427166)) ;
#74766 = CARTESIAN_POINT('Ctrl Pts',(-3.26021975085612,-0.697769125082816,
7.06320246322368)) ;
#74767 = CARTESIAN_POINT('Ctrl Pts',(-3.25413500684155,-0.672122965994088,
7.06837618534741)) ;
#74768 = CARTESIAN_POINT('Ctrl Pts',(-3.2523024532275,-0.679097662424487,
7.06859808108705)) ;
#74769 = CARTESIAN_POINT('Ctrl Pts',(-3.24994321022021,-0.685968760565752,
7.0694168668701)) ;
#74770 = CARTESIAN_POINT('Ctrl Pts',(-3.24710198979478,-0.692647775796551,
7.07077875440761)) ;
#74771 = CARTESIAN_POINT('',(-3.28702640935013,-0.678916496982596,7.03662526114754)) ;
#74772 = CARTESIAN_POINT('Origin',(-3.2051238888154,-0.662,6.9818)) ;
#74773 = CARTESIAN_POINT('Origin',(-3.18317729866126,-0.677221167011857,7.17900526082346)) ;
#74774 = CARTESIAN_POINT('Origin',(0.,-8.67361737988404E-16,6.793484)) ;
#74775 = CARTESIAN_POINT('',(3.31205160669424,0.887893661760288,6.793484)) ;
#74776 = CARTESIAN_POINT('',(-4.19931387427627E-16,3.429,6.793484)) ;
#74777 = CARTESIAN_POINT('Origin',(0.,-1.01919954906029E-15,6.793484)) ;
#74778 = CARTESIAN_POINT('',(3.27942391815471,0.707077062047146,7.03908289042914)) ;
#74779 = CARTESIAN_POINT('Ctrl Pts',(3.2794239181545,0.707077062047012,7.03908289042949)) ;
#74780 = CARTESIAN_POINT('Ctrl Pts',(3.31839899815499,0.756128366293949,6.96625435392858)) ;
#74781 = CARTESIAN_POINT('Ctrl Pts',(3.32718180865331,0.82115248175181,6.88564197720954)) ;
#74782 = CARTESIAN_POINT('Ctrl Pts',(3.31364139250919,0.881705147287931,6.80206837154771)) ;
#74783 = CARTESIAN_POINT('Ctrl Pts',(3.31287790153465,0.884811388204746,6.79777468341573)) ;
#74784 = CARTESIAN_POINT('Ctrl Pts',(3.31205160669424,0.887893661760288,6.793484)) ;
#74785 = CARTESIAN_POINT('',(3.28702640935013,0.678916496982597,7.03662526114754)) ;
#74786 = CARTESIAN_POINT('Origin',(3.18317729880794,0.677221167035773,7.17900526061628)) ;
#74787 = CARTESIAN_POINT('',(3.2870264093502,-0.678916496982227,7.03662526114754)) ;
#74788 = CARTESIAN_POINT('Origin',(0.,-7.50806669192421E-16,7.03662526114754)) ;
#74789 = CARTESIAN_POINT('',(3.27942391815471,-0.707077062047155,7.03908289042913)) ;
#74790 = CARTESIAN_POINT('Origin',(3.18706485416322,-0.677836112548214,7.17352010134439)) ;
#74791 = CARTESIAN_POINT('',(3.31205160669424,-0.887893661760288,6.793484)) ;
#74792 = CARTESIAN_POINT('Ctrl Pts',(3.31205160669424,-0.887893661760288,
6.793484)) ;
#74793 = CARTESIAN_POINT('Ctrl Pts',(3.31287790157776,-0.884811388043908,
6.79777468368237)) ;
#74794 = CARTESIAN_POINT('Ctrl Pts',(3.31364139250205,-0.881705147317766,
6.80206837149932)) ;
#74795 = CARTESIAN_POINT('Ctrl Pts',(3.32718180880554,-0.821152481073567,
6.88564197832078)) ;
#74796 = CARTESIAN_POINT('Ctrl Pts',(3.31839899815499,-0.756128366293962,
6.96625435392856)) ;
#74797 = CARTESIAN_POINT('Ctrl Pts',(3.27942391815451,-0.707077062047025,
7.03908289042947)) ;
#74798 = CARTESIAN_POINT('Origin',(0.,-1.01919954906029E-15,6.793484)) ;
#74799 = CARTESIAN_POINT('',(-3.2870264093502,0.678916496982226,7.03662526114754)) ;
#74800 = CARTESIAN_POINT('Origin',(0.,-7.50806669192421E-16,7.03662526114754)) ;
#74801 = CARTESIAN_POINT('',(-3.27942391815471,0.707077062047156,7.03908289042913)) ;
#74802 = CARTESIAN_POINT('Origin',(-3.18706485424506,0.677836112556869,7.17352010123012)) ;
#74803 = CARTESIAN_POINT('',(-3.31205160669424,0.887893661760289,6.793484)) ;
#74804 = CARTESIAN_POINT('Ctrl Pts',(-3.31205160669424,0.887893661760288,
6.793484)) ;
#74805 = CARTESIAN_POINT('Ctrl Pts',(-3.31287790157776,0.884811388043911,
6.79777468368234)) ;
#74806 = CARTESIAN_POINT('Ctrl Pts',(-3.31364139250206,0.881705147317757,
6.80206837149931)) ;
#74807 = CARTESIAN_POINT('Ctrl Pts',(-3.32718180880552,0.821152481073622,
6.88564197832082)) ;
#74808 = CARTESIAN_POINT('Ctrl Pts',(-3.31839899815499,0.756128366293961,
6.96625435392856)) ;
#74809 = CARTESIAN_POINT('Ctrl Pts',(-3.27942391815451,0.707077062047025,
7.03908289042948)) ;
#74810 = CARTESIAN_POINT('Origin',(0.,-1.01919954906029E-15,6.793484)) ;
#74811 = CARTESIAN_POINT('',(-3.65620261320321E-16,2.985516,6.35)) ;
#74812 = CARTESIAN_POINT('Origin',(-3.65620261320321E-16,2.985516,6.793484)) ;
#74813 = CARTESIAN_POINT('Origin',(0.,-1.23179328113998E-15,6.35)) ;
#74814 = CARTESIAN_POINT('Origin',(0.,-8.2222504619082E-16,6.9818)) ;
#74815 = CARTESIAN_POINT('',(-3.20512388881552,0.661999999999843,7.0818)) ;
#74816 = CARTESIAN_POINT('Origin',(0.,-8.2222504619082E-16,7.0818)) ;
#74817 = CARTESIAN_POINT('',(-3.2105035504766,0.660979117346627,7.08167176697949)) ;
#74818 = CARTESIAN_POINT('Origin',(-3.2048792375206,0.663831325381439,7.00284763048191)) ;
#74819 = CARTESIAN_POINT('',(-3.25413500684125,0.672122965993743,7.06837618534762)) ;
#74820 = CARTESIAN_POINT('Ctrl Pts',(-3.25413500684122,0.672122965993824,
7.06837618534763)) ;
#74821 = CARTESIAN_POINT('Ctrl Pts',(-3.24739271551801,0.666780512351139,
7.07281769210623)) ;
#74822 = CARTESIAN_POINT('Ctrl Pts',(-3.23371088749541,0.659801218122162,
7.07893541781973)) ;
#74823 = CARTESIAN_POINT('Ctrl Pts',(-3.21758827489312,0.659638486038928,
7.08133371486205)) ;
#74824 = CARTESIAN_POINT('Ctrl Pts',(-3.2105035504766,0.660979117346627,7.08167176697949)) ;
#74825 = CARTESIAN_POINT('Origin',(-3.20512388881547,0.661999999999639,6.9818)) ;
#74826 = CARTESIAN_POINT('Ctrl Pts',(-3.31205160669424,0.887893661760288,
6.793484)) ;
#74827 = CARTESIAN_POINT('Ctrl Pts',(-3.31247680274145,0.886307580777865,
6.79874217793992)) ;
#74828 = CARTESIAN_POINT('Ctrl Pts',(-3.31286385708463,0.884707693113234,
6.80400403812142)) ;
#74829 = CARTESIAN_POINT('Ctrl Pts',(-3.31959859780671,0.853484700721687,
6.90642242863739)) ;
#74830 = CARTESIAN_POINT('Ctrl Pts',(-3.31286250738096,0.819472008973418,
7.00521187075636)) ;
#74831 = CARTESIAN_POINT('Ctrl Pts',(-3.2881405032392,0.793313315480963,7.09446231571415)) ;
#74832 = CARTESIAN_POINT('Ctrl Pts',(-3.31205160669424,0.887893661760288,
6.793484)) ;
#74833 = CARTESIAN_POINT('Ctrl Pts',(-3.31261121118724,0.885806205750657,
6.79841624509089)) ;
#74834 = CARTESIAN_POINT('Ctrl Pts',(-3.31307594580264,0.883698810485547,
6.80336333516763)) ;
#74835 = CARTESIAN_POINT('Ctrl Pts',(-3.32193595557476,0.842609792739153,
6.89941056465096)) ;
#74836 = CARTESIAN_POINT('Ctrl Pts',(-3.30625449205529,0.797119135192672,
6.99229450465508)) ;
#74837 = CARTESIAN_POINT('Ctrl Pts',(-3.26888725785269,0.7729411910402,7.07185431702684)) ;
#74838 = CARTESIAN_POINT('Ctrl Pts',(-3.31205160669424,0.887893661760288,
6.793484)) ;
#74839 = CARTESIAN_POINT('Ctrl Pts',(-3.31274522373845,0.885306307503067,
6.79809343311381)) ;
#74840 = CARTESIAN_POINT('Ctrl Pts',(-3.31334303732283,0.8826990404866,6.8027179114036)) ;
#74841 = CARTESIAN_POINT('Ctrl Pts',(-3.32434030429394,0.831838892287706,
6.89249111351257)) ;
#74842 = CARTESIAN_POINT('Ctrl Pts',(-3.30868757227878,0.775373519472595,
6.97904841531995)) ;
#74843 = CARTESIAN_POINT('Ctrl Pts',(-3.2654052227293,0.738492188311667,7.04973176535317)) ;
#74844 = CARTESIAN_POINT('Ctrl Pts',(-3.31205160669424,0.887893661760288,
6.793484)) ;
#74845 = CARTESIAN_POINT('Ctrl Pts',(-3.31287790157776,0.884811388043911,
6.79777468368234)) ;
#74846 = CARTESIAN_POINT('Ctrl Pts',(-3.31364139250206,0.881705147317757,
6.80206837149931)) ;
#74847 = CARTESIAN_POINT('Ctrl Pts',(-3.32718180880552,0.821152481073622,
6.88564197832082)) ;
#74848 = CARTESIAN_POINT('Ctrl Pts',(-3.31839899815499,0.756128366293961,
6.96625435392856)) ;
#74849 = CARTESIAN_POINT('Ctrl Pts',(-3.27942391815451,0.707077062047025,
7.03908289042948)) ;
#74850 = CARTESIAN_POINT('',(-3.2881405032392,0.793313315480963,7.09446231571415)) ;
#74851 = CARTESIAN_POINT('Origin',(-3.36081883130048,0.724626630961926,7.09446231571415)) ;
#74852 = CARTESIAN_POINT('Ctrl Pts',(-3.2881405032392,0.793313315480963,7.09446231571415)) ;
#74853 = CARTESIAN_POINT('Ctrl Pts',(-3.31286250738096,0.819472008973418,
7.00521187075636)) ;
#74854 = CARTESIAN_POINT('Ctrl Pts',(-3.31959859780671,0.853484700721687,
6.90642242863739)) ;
#74855 = CARTESIAN_POINT('Ctrl Pts',(-3.31286385708463,0.884707693113234,
6.80400403812142)) ;
#74856 = CARTESIAN_POINT('Ctrl Pts',(-3.31247680274145,0.886307580777865,
6.79874217793992)) ;
#74857 = CARTESIAN_POINT('Ctrl Pts',(-3.31205160669424,0.887893661760288,
6.793484)) ;
#74858 = CARTESIAN_POINT('Ctrl Pts',(-3.28814050323922,0.793313315480982,
7.09446231571408)) ;
#74859 = CARTESIAN_POINT('Ctrl Pts',(-3.28134410252723,0.786121950167006,
7.11899842468707)) ;
#74860 = CARTESIAN_POINT('Ctrl Pts',(-3.27166340596969,0.778151805222174,
7.13954927378692)) ;
#74861 = CARTESIAN_POINT('Ctrl Pts',(-3.25930415002248,0.77212296599392,7.15495237069524)) ;
#74862 = CARTESIAN_POINT('Ctrl Pts',(-3.27713864873268,0.781672101514859,
7.08154345932128)) ;
#74863 = CARTESIAN_POINT('Ctrl Pts',(-3.2693149987863,0.775745323023668,7.10257847353651)) ;
#74864 = CARTESIAN_POINT('Ctrl Pts',(-3.2586971438891,0.76966902040116,7.11948103530695)) ;
#74865 = CARTESIAN_POINT('Ctrl Pts',(-3.24720304082939,0.766220050630706,
7.13091195407417)) ;
#74866 = CARTESIAN_POINT('Ctrl Pts',(-3.26627246770002,0.753460431697841,
7.05898639091381)) ;
#74867 = CARTESIAN_POINT('Ctrl Pts',(-3.25765493728098,0.747264169127614,
7.07395698646391)) ;
#74868 = CARTESIAN_POINT('Ctrl Pts',(-3.24613294003293,0.741135418678703,
7.08437187853508)) ;
#74869 = CARTESIAN_POINT('Ctrl Pts',(-3.23542257587918,0.737017859268566,
7.08914722322215)) ;
#74870 = CARTESIAN_POINT('Ctrl Pts',(-3.27341590582958,0.720540687589143,
7.04364669396792)) ;
#74871 = CARTESIAN_POINT('Ctrl Pts',(-3.26646853334762,0.711672429586283,
7.05583711308295)) ;
#74872 = CARTESIAN_POINT('Ctrl Pts',(-3.25699307010659,0.701213312597674,
7.06492336369149)) ;
#74873 = CARTESIAN_POINT('Ctrl Pts',(-3.24626907090931,0.691101901539582,
7.07061000050628)) ;
#74874 = CARTESIAN_POINT('Ctrl Pts',(-3.27942391815468,0.707077062047165,
7.03908289042918)) ;
#74875 = CARTESIAN_POINT('Ctrl Pts',(-3.27351027274501,0.697039528180337,
7.05095544135298)) ;
#74876 = CARTESIAN_POINT('Ctrl Pts',(-3.26515692538619,0.684626627058011,
7.06067463689345)) ;
#74877 = CARTESIAN_POINT('Ctrl Pts',(-3.25413500684125,0.67212296599374,7.06837618534762)) ;
#74878 = CARTESIAN_POINT('',(-3.25930415002248,0.77212296599392,7.15495237069524)) ;
#74879 = CARTESIAN_POINT('Origin',(-3.30314612486703,0.68224593198784,7.15495237069524)) ;
#74880 = CARTESIAN_POINT('Ctrl Pts',(-3.25930415002248,0.77212296599392,7.15495237069524)) ;
#74881 = CARTESIAN_POINT('Ctrl Pts',(-3.27166340596969,0.778151805222174,
7.13954927378692)) ;
#74882 = CARTESIAN_POINT('Ctrl Pts',(-3.28134410252723,0.786121950167006,
7.11899842468707)) ;
#74883 = CARTESIAN_POINT('Ctrl Pts',(-3.28814050323922,0.793313315480982,
7.09446231571408)) ;
#74884 = CARTESIAN_POINT('Ctrl Pts',(-3.27942391815468,0.707077062047165,
7.03908289042918)) ;
#74885 = CARTESIAN_POINT('Ctrl Pts',(-3.2764538639168,0.702035836553619,7.04504573022475)) ;
#74886 = CARTESIAN_POINT('Ctrl Pts',(-3.27285683396428,0.696395529148052,
7.05045952339999)) ;
#74887 = CARTESIAN_POINT('Ctrl Pts',(-3.26443586616697,0.684547202106127,
7.0602016814902)) ;
#74888 = CARTESIAN_POINT('Ctrl Pts',(-3.25962130503425,0.678346820109796,
7.06454264301149)) ;
#74889 = CARTESIAN_POINT('Ctrl Pts',(-3.25413500684125,0.672122965993741,
7.06837618534762)) ;
#74890 = CARTESIAN_POINT('Ctrl Pts',(-3.25930415002247,0.772122965993916,
7.15495237069525)) ;
#74891 = CARTESIAN_POINT('Ctrl Pts',(-3.25217652898008,0.768646115807462,
7.16383538421246)) ;
#74892 = CARTESIAN_POINT('Ctrl Pts',(-3.23808903446775,0.763655482586567,
7.17607083563947)) ;
#74893 = CARTESIAN_POINT('Ctrl Pts',(-3.22227089015459,0.762000000000254,
7.18086742972409)) ;
#74894 = CARTESIAN_POINT('Ctrl Pts',(-3.21546217518166,0.762,7.18154353395898)) ;
#74895 = CARTESIAN_POINT('Ctrl Pts',(-3.24720304082939,0.766220050630709,
7.13091195407419)) ;
#74896 = CARTESIAN_POINT('Ctrl Pts',(-3.24082772074753,0.764341685381236,
7.13776252021244)) ;
#74897 = CARTESIAN_POINT('Ctrl Pts',(-3.22957572127668,0.76230454784959,7.14681577983074)) ;
#74898 = CARTESIAN_POINT('Ctrl Pts',(-3.21874824269101,0.761905886466605,
7.15069418882242)) ;
#74899 = CARTESIAN_POINT('Ctrl Pts',(-3.2139688379146,0.761999999999944,7.15146619592362)) ;
#74900 = CARTESIAN_POINT('Ctrl Pts',(-3.23542257429462,0.737017860463239,
7.08914722161447)) ;
#74901 = CARTESIAN_POINT('Ctrl Pts',(-3.22965611967589,0.735483547844239,
7.09257680559161)) ;
#74902 = CARTESIAN_POINT('Ctrl Pts',(-3.22096836281863,0.734845466512303,
7.09620345120675)) ;
#74903 = CARTESIAN_POINT('Ctrl Pts',(-3.21447987532315,0.735942196903049,
7.09846645621959)) ;
#74904 = CARTESIAN_POINT('Ctrl Pts',(-3.21138266038764,0.736564632620709,
7.0993779386748)) ;
#74905 = CARTESIAN_POINT('Ctrl Pts',(-3.2462690709093,0.691101901539657,7.0706100005063)) ;
#74906 = CARTESIAN_POINT('Ctrl Pts',(-3.23998072705782,0.686932534379085,
7.07420186243876)) ;
#74907 = CARTESIAN_POINT('Ctrl Pts',(-3.22834802048836,0.681963529037854,
7.07871480715488)) ;
#74908 = CARTESIAN_POINT('Ctrl Pts',(-3.2160102402617,0.68236088570503,7.08087457454952)) ;
#74909 = CARTESIAN_POINT('Ctrl Pts',(-3.21049211655992,0.683563730806886,
7.08144147623458)) ;
#74910 = CARTESIAN_POINT('Ctrl Pts',(-3.25413500684122,0.672122965993824,
7.06837618534763)) ;
#74911 = CARTESIAN_POINT('Ctrl Pts',(-3.24739271551801,0.666780512351139,
7.07281769210623)) ;
#74912 = CARTESIAN_POINT('Ctrl Pts',(-3.23371088749541,0.659801218122162,
7.07893541781973)) ;
#74913 = CARTESIAN_POINT('Ctrl Pts',(-3.21758827489312,0.659638486038928,
7.08133371486205)) ;
#74914 = CARTESIAN_POINT('Ctrl Pts',(-3.2105035504766,0.660979117346627,7.08167176697949)) ;
#74915 = CARTESIAN_POINT('',(-3.2154621751798,0.762,7.18154353395898)) ;
#74916 = CARTESIAN_POINT('Origin',(-3.2154621751854,0.662,7.18154353395898)) ;
#74917 = CARTESIAN_POINT('Ctrl Pts',(-3.21546217518166,0.762,7.18154353395898)) ;
#74918 = CARTESIAN_POINT('Ctrl Pts',(-3.22227089015459,0.762000000000254,
7.18086742972409)) ;
#74919 = CARTESIAN_POINT('Ctrl Pts',(-3.23808903446775,0.763655482586567,
7.17607083563947)) ;
#74920 = CARTESIAN_POINT('Ctrl Pts',(-3.25217652898008,0.768646115807462,
7.16383538421246)) ;
#74921 = CARTESIAN_POINT('Ctrl Pts',(-3.25930415002247,0.772122965993916,
7.15495237069525)) ;
#74922 = CARTESIAN_POINT('Ctrl Pts',(-3.2154621751854,0.762,7.18154353395898)) ;
#74923 = CARTESIAN_POINT('Ctrl Pts',(-3.21201894456566,0.762,7.18171449006545)) ;
#74924 = CARTESIAN_POINT('Ctrl Pts',(-3.20857144403885,0.762,7.1818)) ;
#74925 = CARTESIAN_POINT('Ctrl Pts',(-3.20512388881564,0.762,7.1818)) ;
#74926 = CARTESIAN_POINT('Ctrl Pts',(-3.21396883791834,0.762,7.15146619592359)) ;
#74927 = CARTESIAN_POINT('Ctrl Pts',(-3.21102860740559,0.761997290973651,
7.15167826758758)) ;
#74928 = CARTESIAN_POINT('Ctrl Pts',(-3.20807464984533,0.762002680217736,
7.15181361851019)) ;
#74929 = CARTESIAN_POINT('Ctrl Pts',(-3.20512388881561,0.762,7.15188006996581)) ;
#74930 = CARTESIAN_POINT('Ctrl Pts',(-3.21138265683666,0.736564691651965,
7.0993778670976)) ;
#74931 = CARTESIAN_POINT('Ctrl Pts',(-3.20930558735074,0.736681278140644,
7.09965201966661)) ;
#74932 = CARTESIAN_POINT('Ctrl Pts',(-3.20722130366678,0.7367952805891,7.09987813004075)) ;
#74933 = CARTESIAN_POINT('Ctrl Pts',(-3.20512388881555,0.736911789981695,
7.10005036094909)) ;
#74934 = CARTESIAN_POINT('Ctrl Pts',(-3.21049211656076,0.683563730806912,
7.08144147623454)) ;
#74935 = CARTESIAN_POINT('Ctrl Pts',(-3.20870975639603,0.683855790193559,
7.08160438817637)) ;
#74936 = CARTESIAN_POINT('Ctrl Pts',(-3.20691685125597,0.684146559499709,
7.08172265074698)) ;
#74937 = CARTESIAN_POINT('Ctrl Pts',(-3.20512388881552,0.68443994752562,7.08179999999999)) ;
#74938 = CARTESIAN_POINT('Ctrl Pts',(-3.2105035504766,0.660979117346626,7.08167176697949)) ;
#74939 = CARTESIAN_POINT('Ctrl Pts',(-3.20871214489269,0.661318102220315,
7.08175724503272)) ;
#74940 = CARTESIAN_POINT('Ctrl Pts',(-3.20691819492514,0.661658530855206,
7.0818)) ;
#74941 = CARTESIAN_POINT('Ctrl Pts',(-3.20512388881552,0.661999999999975,
7.0818)) ;
#74942 = CARTESIAN_POINT('',(-3.20512388881569,0.762,7.1818)) ;
#74943 = CARTESIAN_POINT('Origin',(-3.20512388881569,0.662,7.1818)) ;
#74944 = CARTESIAN_POINT('Origin',(-3.20581132625523,0.762,7.02444416805792)) ;
#74945 = CARTESIAN_POINT('Ctrl Pts',(-3.14953687287001,0.762,7.1818)) ;
#74946 = CARTESIAN_POINT('Ctrl Pts',(-3.14687049250718,0.762,7.1818)) ;
#74947 = CARTESIAN_POINT('Ctrl Pts',(-3.14153773178152,0.762,7.1818)) ;
#74948 = CARTESIAN_POINT('Ctrl Pts',(-3.13353859069304,0.762,7.1818)) ;
#74949 = CARTESIAN_POINT('Ctrl Pts',(-3.12287306924172,0.762,7.1818)) ;
#74950 = CARTESIAN_POINT('Ctrl Pts',(-3.11487392815324,0.762,7.18180000000001)) ;
#74951 = CARTESIAN_POINT('Ctrl Pts',(-3.10892316710968,0.762,7.18179999999999)) ;
#74952 = CARTESIAN_POINT('Ctrl Pts',(-3.10830516679178,0.762,7.18179999999999)) ;
#74953 = CARTESIAN_POINT('Ctrl Pts',(-3.10768716647391,0.761999999491749,
7.18179159914902)) ;
#74954 = CARTESIAN_POINT('Ctrl Pts',(-3.14953687287001,0.762,7.16625960724294)) ;
#74955 = CARTESIAN_POINT('Ctrl Pts',(-3.14687049250718,0.762,7.16719533415406)) ;
#74956 = CARTESIAN_POINT('Ctrl Pts',(-3.14153773178152,0.762,7.16928720207077)) ;
#74957 = CARTESIAN_POINT('Ctrl Pts',(-3.13353859069304,0.762,7.17285503844875)) ;
#74958 = CARTESIAN_POINT('Ctrl Pts',(-3.12287306924172,0.762,7.17733421919101)) ;
#74959 = CARTESIAN_POINT('Ctrl Pts',(-3.11487392815324,0.762,7.17988076927801)) ;
#74960 = CARTESIAN_POINT('Ctrl Pts',(-3.10892316710968,0.762,7.18147435116188)) ;
#74961 = CARTESIAN_POINT('Ctrl Pts',(-3.10830516679238,0.76199997373953,7.18163768471162)) ;
#74962 = CARTESIAN_POINT('Ctrl Pts',(-3.10768716647391,0.761999999491749,
7.18179159914902)) ;
#74963 = CARTESIAN_POINT('Ctrl Pts',(-3.14953687287001,0.755540898601867,
7.13908377950685)) ;
#74964 = CARTESIAN_POINT('Ctrl Pts',(-3.14687049250718,0.756336720061584,
7.1416558838152)) ;
#74965 = CARTESIAN_POINT('Ctrl Pts',(-3.14153773178152,0.757950944898512,
7.14739328800637)) ;
#74966 = CARTESIAN_POINT('Ctrl Pts',(-3.13353859069303,0.760010135132571,
7.157199311821)) ;
#74967 = CARTESIAN_POINT('Ctrl Pts',(-3.12287306924172,0.761680931524669,
7.16950958658713)) ;
#74968 = CARTESIAN_POINT('Ctrl Pts',(-3.11487392815321,0.761961216462268,
7.17650146046705)) ;
#74969 = CARTESIAN_POINT('Ctrl Pts',(-3.10892316710969,0.761997489103582,
7.18090629058231)) ;
#74970 = CARTESIAN_POINT('Ctrl Pts',(-3.10830516679297,0.761999927581,7.18135238002238)) ;
#74971 = CARTESIAN_POINT('Ctrl Pts',(-3.10768716647391,0.761999999491749,
7.18179159914902)) ;
#74972 = CARTESIAN_POINT('Ctrl Pts',(-3.14953687287001,0.739012268865883,
7.11695436533127)) ;
#74973 = CARTESIAN_POINT('Ctrl Pts',(-3.14687049250718,0.74169687311928,7.12026196117322)) ;
#74974 = CARTESIAN_POINT('Ctrl Pts',(-3.14153773178152,0.747258461785075,
7.12796089840982)) ;
#74975 = CARTESIAN_POINT('Ctrl Pts',(-3.13353859069302,0.754625778458326,
7.1423590326318)) ;
#74976 = CARTESIAN_POINT('Ctrl Pts',(-3.12287306924171,0.760786688710496,
7.16164067071631)) ;
#74977 = CARTESIAN_POINT('Ctrl Pts',(-3.11487392815318,0.761845223762039,
7.17312655610409)) ;
#74978 = CARTESIAN_POINT('Ctrl Pts',(-3.10892316710969,0.761991474599831,
7.18033804412795)) ;
#74979 = CARTESIAN_POINT('Ctrl Pts',(-3.10830516679363,0.761999881429747,
7.18106712031758)) ;
#74980 = CARTESIAN_POINT('Ctrl Pts',(-3.10768716647391,0.761999999491749,
7.18179159914902)) ;
#74981 = CARTESIAN_POINT('Ctrl Pts',(-3.14953687287001,0.73052345613245,7.10896775467099)) ;
#74982 = CARTESIAN_POINT('Ctrl Pts',(-3.14687049250718,0.734108743088629,
7.11234093439866)) ;
#74983 = CARTESIAN_POINT('Ctrl Pts',(-3.14153773178152,0.741620611344294,
7.12039126654701)) ;
#74984 = CARTESIAN_POINT('Ctrl Pts',(-3.13353859069302,0.751722671586531,
7.13626512385343)) ;
#74985 = CARTESIAN_POINT('Ctrl Pts',(-3.12287306924171,0.760294668457555,
7.15825743742988)) ;
#74986 = CARTESIAN_POINT('Ctrl Pts',(-3.11487392815318,0.761768784399304,
7.17170556226768)) ;
#74987 = CARTESIAN_POINT('Ctrl Pts',(-3.10892316710969,0.761989461278184,
7.18009224570766)) ;
#74988 = CARTESIAN_POINT('Ctrl Pts',(-3.10830516679515,0.761999861904407,
7.18094643469176)) ;
#74989 = CARTESIAN_POINT('Ctrl Pts',(-3.10768716647391,0.761999999491749,
7.18179159914902)) ;
#74990 = CARTESIAN_POINT('',(-3.14953687287002,0.730523456132444,7.10896775467099)) ;
#74991 = CARTESIAN_POINT('',(-3.10768716647391,0.761999999491749,7.18179159914902)) ;
#74992 = CARTESIAN_POINT('Ctrl Pts',(-3.14953687287001,0.73052345613245,7.10896775467099)) ;
#74993 = CARTESIAN_POINT('Ctrl Pts',(-3.14797942941845,0.732617636606373,
7.11093804246303)) ;
#74994 = CARTESIAN_POINT('Ctrl Pts',(-3.14650618411119,0.734653311026188,
7.11301988346854)) ;
#74995 = CARTESIAN_POINT('Ctrl Pts',(-3.14387449159256,0.738267786921109,
7.11706119147952)) ;
#74996 = CARTESIAN_POINT('Ctrl Pts',(-3.14270349733143,0.739869138198676,
7.11898770799634)) ;
#74997 = CARTESIAN_POINT('Ctrl Pts',(-3.14003428427703,0.743434565765228,
7.12365088269313)) ;
#74998 = CARTESIAN_POINT('Ctrl Pts',(-3.13853953335781,0.745372225194674,
7.12646045464107)) ;
#74999 = CARTESIAN_POINT('Ctrl Pts',(-3.13653045010517,0.747788501075358,
7.13038308945641)) ;
#75000 = CARTESIAN_POINT('Ctrl Pts',(-3.13605623456106,0.748345478006875,
7.13131931951466)) ;
#75001 = CARTESIAN_POINT('Ctrl Pts',(-3.13490030581321,0.749663361810016,
7.13362028111691)) ;
#75002 = CARTESIAN_POINT('Ctrl Pts',(-3.13422095933187,0.750405401569636,
7.1349879362403)) ;
#75003 = CARTESIAN_POINT('Ctrl Pts',(-3.13116301782668,0.753565178819733,
7.14117483383158)) ;
#75004 = CARTESIAN_POINT('Ctrl Pts',(-3.12875081675081,0.755569874503869,
7.14614156555835)) ;
#75005 = CARTESIAN_POINT('Ctrl Pts',(-3.12605506967943,0.757288027552031,
7.15141997627083)) ;
#75006 = CARTESIAN_POINT('Ctrl Pts',(-3.12579739926236,0.75744707015426,7.15192175274669)) ;
#75007 = CARTESIAN_POINT('Ctrl Pts',(-3.12252089822597,0.759403912638519,
7.15826199813988)) ;
#75008 = CARTESIAN_POINT('Ctrl Pts',(-3.1194641078908,0.760518751613542,7.16374160917873)) ;
#75009 = CARTESIAN_POINT('Ctrl Pts',(-3.11411372865795,0.761651857385016,
7.17250963958096)) ;
#75010 = CARTESIAN_POINT('Ctrl Pts',(-3.11182852612461,0.761881719502846,
7.17599758854373)) ;
#75011 = CARTESIAN_POINT('Ctrl Pts',(-3.10892327200399,0.761989457388304,
7.18009209787526)) ;
#75012 = CARTESIAN_POINT('Ctrl Pts',(-3.1083052192423,0.761999861892731,7.18094636296612)) ;
#75013 = CARTESIAN_POINT('Ctrl Pts',(-3.10768716647391,0.761999999491749,
7.18179159914902)) ;
#75014 = CARTESIAN_POINT('',(-3.14953687287001,0.762,7.1818)) ;
#75015 = CARTESIAN_POINT('',(-3.10768716647391,0.761999999491749,7.18179159914902)) ;
#75016 = CARTESIAN_POINT('Origin',(-3.14953687287001,0.661999999999999,7.1818)) ;
#75017 = CARTESIAN_POINT('Ctrl Pts',(-3.17121692101567,0.762,7.1818)) ;
#75018 = CARTESIAN_POINT('Ctrl Pts',(-3.16399023830045,0.762,7.1818)) ;
#75019 = CARTESIAN_POINT('Ctrl Pts',(-3.15676355558523,0.762,7.1818)) ;
#75020 = CARTESIAN_POINT('Ctrl Pts',(-3.14953687287001,0.762,7.1818)) ;
#75021 = CARTESIAN_POINT('Ctrl Pts',(-3.17121692101567,0.762,7.16049051462243)) ;
#75022 = CARTESIAN_POINT('Ctrl Pts',(-3.16399023830045,0.761980537877959,
7.16173716654572)) ;
#75023 = CARTESIAN_POINT('Ctrl Pts',(-3.15676355558523,0.762015837610647,
7.16371429760845)) ;
#75024 = CARTESIAN_POINT('Ctrl Pts',(-3.14953687287001,0.762,7.16625960724294)) ;
#75025 = CARTESIAN_POINT('Ctrl Pts',(-3.17121692101567,0.749661462765229,
7.12329552595192)) ;
#75026 = CARTESIAN_POINT('Ctrl Pts',(-3.16399023830045,0.751152261593369,
7.1266719591844)) ;
#75027 = CARTESIAN_POINT('Ctrl Pts',(-3.15676355558523,0.75338304373689,7.13211431434399)) ;
#75028 = CARTESIAN_POINT('Ctrl Pts',(-3.14953687287001,0.755540893518778,
7.1390837819811)) ;
#75029 = CARTESIAN_POINT('Ctrl Pts',(-3.17121692101567,0.720057683295033,
7.09882570651471)) ;
#75030 = CARTESIAN_POINT('Ctrl Pts',(-3.16399023830045,0.724623549182785,
7.10220324165009)) ;
#75031 = CARTESIAN_POINT('Ctrl Pts',(-3.15676355558523,0.731748787702952,
7.10798226702609)) ;
#75032 = CARTESIAN_POINT('Ctrl Pts',(-3.14953687287002,0.739012268865877,
7.11695436533126)) ;
#75033 = CARTESIAN_POINT('Ctrl Pts',(-3.17121692101567,0.70568090461708,7.09184457452808)) ;
#75034 = CARTESIAN_POINT('Ctrl Pts',(-3.16399023830045,0.711535796534348,
7.09468761566807)) ;
#75035 = CARTESIAN_POINT('Ctrl Pts',(-3.15676355558523,0.720806263628136,
7.09982543575316)) ;
#75036 = CARTESIAN_POINT('Ctrl Pts',(-3.14953687287002,0.730523456132442,
7.10896775467099)) ;
#75037 = CARTESIAN_POINT('',(-3.17121692101567,0.762,7.1818)) ;
#75038 = CARTESIAN_POINT('',(-3.14953687287001,0.762,7.1818)) ;
#75039 = CARTESIAN_POINT('',(-3.17121692101567,0.70568090461708,7.09184457452808)) ;
#75040 = CARTESIAN_POINT('Origin',(-3.17121692101567,0.662,7.1818)) ;
#75041 = CARTESIAN_POINT('Ctrl Pts',(-3.17121692101567,0.70568090461708,7.09184457452808)) ;
#75042 = CARTESIAN_POINT('Ctrl Pts',(-3.16399023830045,0.711535796534348,
7.09468761566807)) ;
#75043 = CARTESIAN_POINT('Ctrl Pts',(-3.15676355558523,0.720806263628136,
7.09982543575316)) ;
#75044 = CARTESIAN_POINT('Ctrl Pts',(-3.14953687287002,0.730523456132442,
7.10896775467099)) ;
#75045 = CARTESIAN_POINT('Ctrl Pts',(-3.20512388881547,0.762,7.1818)) ;
#75046 = CARTESIAN_POINT('Ctrl Pts',(-3.2047202344369,0.762,7.1818)) ;
#75047 = CARTESIAN_POINT('Ctrl Pts',(-3.20391292567976,0.762,7.1818)) ;
#75048 = CARTESIAN_POINT('Ctrl Pts',(-3.20270196254405,0.762,7.1818)) ;
#75049 = CARTESIAN_POINT('Ctrl Pts',(-3.20149099940835,0.762,7.1818)) ;
#75050 = CARTESIAN_POINT('Ctrl Pts',(-3.19745445562265,0.762,7.1818)) ;
#75051 = CARTESIAN_POINT('Ctrl Pts',(-3.18736309615843,0.762,7.1818)) ;
#75052 = CARTESIAN_POINT('Ctrl Pts',(-3.17767539107277,0.762,7.1818)) ;
#75053 = CARTESIAN_POINT('Ctrl Pts',(-3.17121692101567,0.762,7.1818)) ;
#75054 = CARTESIAN_POINT('Ctrl Pts',(-3.20512388881547,0.762,7.15188006996578)) ;
#75055 = CARTESIAN_POINT('Ctrl Pts',(-3.2047202344369,0.761992330181026,7.1520702301264)) ;
#75056 = CARTESIAN_POINT('Ctrl Pts',(-3.20391292567976,0.76197980992607,7.15243005278884)) ;
#75057 = CARTESIAN_POINT('Ctrl Pts',(-3.20270196254405,0.761963555547577,
7.15292464422255)) ;
#75058 = CARTESIAN_POINT('Ctrl Pts',(-3.20149099940835,0.761947562028465,
7.15338566691011)) ;
#75059 = CARTESIAN_POINT('Ctrl Pts',(-3.19745445562265,0.76191470846392,7.15481366906456)) ;
#75060 = CARTESIAN_POINT('Ctrl Pts',(-3.18736309615843,0.761861071074269,
7.15758629528363)) ;
#75061 = CARTESIAN_POINT('Ctrl Pts',(-3.17767539107277,0.76201739325461,7.15937638460794)) ;
#75062 = CARTESIAN_POINT('Ctrl Pts',(-3.17121692101567,0.762,7.16049051462243)) ;
#75063 = CARTESIAN_POINT('Ctrl Pts',(-3.20512388881547,0.736911811379183,
7.10005033527499)) ;
#75064 = CARTESIAN_POINT('Ctrl Pts',(-3.2047202344369,0.737245219347505,7.10054319817603)) ;
#75065 = CARTESIAN_POINT('Ctrl Pts',(-3.20391292567976,0.737869883520249,
7.10148033026224)) ;
#75066 = CARTESIAN_POINT('Ctrl Pts',(-3.20270196254405,0.738711770607014,
7.10277348618571)) ;
#75067 = CARTESIAN_POINT('Ctrl Pts',(-3.20149099940835,0.73948195346955,7.1039804248426)) ;
#75068 = CARTESIAN_POINT('Ctrl Pts',(-3.19745445562265,0.741829197217652,
7.10775251408813)) ;
#75069 = CARTESIAN_POINT('Ctrl Pts',(-3.18736309615843,0.746011102788114,
7.11515718689346)) ;
#75070 = CARTESIAN_POINT('Ctrl Pts',(-3.17767539107277,0.748329114460406,
7.12027803292724)) ;
#75071 = CARTESIAN_POINT('Ctrl Pts',(-3.17121692101567,0.749661438013567,
7.12329554369824)) ;
#75072 = CARTESIAN_POINT('Ctrl Pts',(-3.20512388881547,0.684439947525491,
7.08179999999996)) ;
#75073 = CARTESIAN_POINT('Ctrl Pts',(-3.2047202344369,0.685279518511752,7.08202134573632)) ;
#75074 = CARTESIAN_POINT('Ctrl Pts',(-3.20391292567976,0.686865903002586,
7.08246093200816)) ;
#75075 = CARTESIAN_POINT('Ctrl Pts',(-3.20270196254405,0.689032722166199,
7.08311409360665)) ;
#75076 = CARTESIAN_POINT('Ctrl Pts',(-3.20149099940835,0.691037008739264,
7.08376272980254)) ;
#75077 = CARTESIAN_POINT('Ctrl Pts',(-3.19745445562265,0.697229783074605,
7.08590527875505)) ;
#75078 = CARTESIAN_POINT('Ctrl Pts',(-3.18736309615843,0.708839952636613,
7.09112838260725)) ;
#75079 = CARTESIAN_POINT('Ctrl Pts',(-3.17767539107277,0.715977179240427,
7.09580721097557)) ;
#75080 = CARTESIAN_POINT('Ctrl Pts',(-3.17121692101567,0.720057683295033,
7.09882570651471)) ;
#75081 = CARTESIAN_POINT('Ctrl Pts',(-3.20512388881547,0.661999999999825,
7.0818)) ;
#75082 = CARTESIAN_POINT('Ctrl Pts',(-3.2047202344369,0.662977161851475,7.0818)) ;
#75083 = CARTESIAN_POINT('Ctrl Pts',(-3.20391292567976,0.664831438935661,
7.08182813262089)) ;
#75084 = CARTESIAN_POINT('Ctrl Pts',(-3.20270196254405,0.667381960953565,
7.08193509059619)) ;
#75085 = CARTESIAN_POINT('Ctrl Pts',(-3.20149099940835,0.669755131272068,
7.08209149598161)) ;
#75086 = CARTESIAN_POINT('Ctrl Pts',(-3.19745445562265,0.677136096351085,
7.08275930201879)) ;
#75087 = CARTESIAN_POINT('Ctrl Pts',(-3.18736309615843,0.691331994006365,
7.08558723772615)) ;
#75088 = CARTESIAN_POINT('Ctrl Pts',(-3.17767539107277,0.700448400904743,
7.08930375506813)) ;
#75089 = CARTESIAN_POINT('Ctrl Pts',(-3.17121692101567,0.705680904617079,
7.09184457452808)) ;
#75090 = CARTESIAN_POINT('',(-3.17121692101567,0.762,7.1818)) ;
#75091 = CARTESIAN_POINT('Ctrl Pts',(-3.20512388881547,0.661999999999825,
7.0818)) ;
#75092 = CARTESIAN_POINT('Ctrl Pts',(-3.2047202344369,0.662977161851475,7.0818)) ;
#75093 = CARTESIAN_POINT('Ctrl Pts',(-3.20431658005833,0.663904297939892,
7.08181418112561)) ;
#75094 = CARTESIAN_POINT('Ctrl Pts',(-3.20350927130119,0.665681610657567,
7.08186384002979)) ;
#75095 = CARTESIAN_POINT('Ctrl Pts',(-3.20310561692262,0.666531791312267,
7.08189935834228)) ;
#75096 = CARTESIAN_POINT('Ctrl Pts',(-3.20229830816548,0.668173012083282,
7.08198732917139)) ;
#75097 = CARTESIAN_POINT('Ctrl Pts',(-3.20189465378691,0.668964039857316,
7.0820398363167)) ;
#75098 = CARTESIAN_POINT('Ctrl Pts',(-3.20108734502978,0.670493217907198,
7.08215837537036)) ;
#75099 = CARTESIAN_POINT('Ctrl Pts',(-3.20068369065121,0.67123138690257,7.08222438102225)) ;
#75100 = CARTESIAN_POINT('Ctrl Pts',(-3.19847904880683,0.675159362227489,
7.08261718651246)) ;
#75101 = CARTESIAN_POINT('Ctrl Pts',(-3.19667806134099,0.677991390732854,
7.08305203429455)) ;
#75102 = CARTESIAN_POINT('Ctrl Pts',(-3.19344882631242,0.682614461197415,
7.08392572248012)) ;
#75103 = CARTESIAN_POINT('Ctrl Pts',(-3.19202057874969,0.684499933880174,
7.08434667817418)) ;
#75104 = CARTESIAN_POINT('Ctrl Pts',(-3.18778558324305,0.689801348801302,
7.08567402178888)) ;
#75105 = CARTESIAN_POINT('Ctrl Pts',(-3.18497883529916,0.692934482334903,
7.08665681146921)) ;
#75106 = CARTESIAN_POINT('Ctrl Pts',(-3.17911128623287,0.698892281462533,
7.0887953603999)) ;
#75107 = CARTESIAN_POINT('Ctrl Pts',(-3.17605048511049,0.70166412270943,7.08995925874849)) ;
#75108 = CARTESIAN_POINT('Ctrl Pts',(-3.17239876299729,0.704716249384997,
7.09138087098938)) ;
#75109 = CARTESIAN_POINT('Ctrl Pts',(-3.17180784200648,0.705202154038262,
7.09161210096399)) ;
#75110 = CARTESIAN_POINT('Ctrl Pts',(-3.17121692101567,0.705680904617079,
7.09184457452808)) ;
#75111 = CARTESIAN_POINT('Origin',(-3.21546217517793,0.862,0.)) ;
#75112 = CARTESIAN_POINT('',(-3.21546217517793,0.762,7.36730649953872)) ;
#75113 = CARTESIAN_POINT('',(-3.21546217517793,0.762,0.)) ;
#75114 = CARTESIAN_POINT('',(-3.31205160669424,0.887893661760289,7.36730649953872)) ;
#75115 = CARTESIAN_POINT('Origin',(-3.21546217517793,0.862,7.36730649953872)) ;
#75116 = CARTESIAN_POINT('',(-3.31205160669424,0.887893661760288,0.)) ;
#75117 = CARTESIAN_POINT('Origin',(-9.525,0.762,8.72161438184689)) ;
#75118 = CARTESIAN_POINT('',(-0.598228027472806,0.762,7.1818)) ;
#75119 = CARTESIAN_POINT('',(0.,0.762,7.1818)) ;
#75120 = CARTESIAN_POINT('',(-0.731723284002018,0.762,8.59150875795967)) ;
#75121 = CARTESIAN_POINT('',(-0.787882878836553,0.762,9.1845535952074)) ;
#75122 = CARTESIAN_POINT('',(-3.07434158440252,0.762,7.64111756647598)) ;
#75123 = CARTESIAN_POINT('Origin',(0.,0.762,3.42553041237115)) ;
#75124 = CARTESIAN_POINT('Ctrl Pts',(-3.21546217517793,0.762,7.36730649953872)) ;
#75125 = CARTESIAN_POINT('Ctrl Pts',(-3.21546217517793,0.762,7.41298218019493)) ;
#75126 = CARTESIAN_POINT('Ctrl Pts',(-3.19308177554602,0.762,7.51957930543031)) ;
#75127 = CARTESIAN_POINT('Ctrl Pts',(-3.12354733145101,0.762,7.60523282045775)) ;
#75128 = CARTESIAN_POINT('Ctrl Pts',(-3.07434158440252,0.762,7.64111756647598)) ;
#75129 = CARTESIAN_POINT('Ctrl Pts',(3.31205160669424,0.887893661760288,6.793484)) ;
#75130 = CARTESIAN_POINT('Ctrl Pts',(3.31287790153465,0.884811388204746,6.79777468341573)) ;
#75131 = CARTESIAN_POINT('Ctrl Pts',(3.31364139250919,0.881705147287931,6.80206837154771)) ;
#75132 = CARTESIAN_POINT('Ctrl Pts',(3.32718180865331,0.82115248175181,6.88564197720954)) ;
#75133 = CARTESIAN_POINT('Ctrl Pts',(3.31839899815499,0.756128366293949,6.96625435392858)) ;
#75134 = CARTESIAN_POINT('Ctrl Pts',(3.2794239181545,0.707077062047012,7.03908289042949)) ;
#75135 = CARTESIAN_POINT('Ctrl Pts',(3.31205160669424,0.887893661760288,6.793484)) ;
#75136 = CARTESIAN_POINT('Ctrl Pts',(3.31274522369532,0.885306307663944,6.79809343284722)) ;
#75137 = CARTESIAN_POINT('Ctrl Pts',(3.31334303732996,0.882699040456766,6.80271791145202)) ;
#75138 = CARTESIAN_POINT('Ctrl Pts',(3.32434030414173,0.831838892965902,6.89249111240128)) ;
#75139 = CARTESIAN_POINT('Ctrl Pts',(3.30868757227878,0.775373519472581,6.97904841531997)) ;
#75140 = CARTESIAN_POINT('Ctrl Pts',(3.26540522272929,0.738492188311657,7.04973176535319)) ;
#75141 = CARTESIAN_POINT('Ctrl Pts',(3.31205160669424,0.887893661760288,6.793484)) ;
#75142 = CARTESIAN_POINT('Ctrl Pts',(3.31261121114413,0.88580620591146,6.79841624482426)) ;
#75143 = CARTESIAN_POINT('Ctrl Pts',(3.31307594580977,0.883698810455707,6.8033633352161)) ;
#75144 = CARTESIAN_POINT('Ctrl Pts',(3.32193595542266,0.842609793416925,6.899410563539)) ;
#75145 = CARTESIAN_POINT('Ctrl Pts',(3.30625449205529,0.797119135192663,6.99229450465509)) ;
#75146 = CARTESIAN_POINT('Ctrl Pts',(3.26888725785268,0.772941191040193,7.07185431702686)) ;
#75147 = CARTESIAN_POINT('Ctrl Pts',(3.31205160669424,0.887893661760288,6.793484)) ;
#75148 = CARTESIAN_POINT('Ctrl Pts',(3.31247680269833,0.886307580938705,6.79874217767332)) ;
#75149 = CARTESIAN_POINT('Ctrl Pts',(3.31286385709175,0.884707693083394,6.8040040381699)) ;
#75150 = CARTESIAN_POINT('Ctrl Pts',(3.31959859765461,0.85348470139946,6.90642242752542)) ;
#75151 = CARTESIAN_POINT('Ctrl Pts',(3.31286250738096,0.819472008973411,7.00521187075637)) ;
#75152 = CARTESIAN_POINT('Ctrl Pts',(3.2881405032392,0.793313315480956,7.09446231571417)) ;
#75153 = CARTESIAN_POINT('',(3.2881405032392,0.793313315480956,7.09446231571417)) ;
#75154 = CARTESIAN_POINT('Origin',(3.36081883130047,0.724626630961912,7.09446231571417)) ;
#75155 = CARTESIAN_POINT('Ctrl Pts',(3.31205160669424,0.887893661760288,6.793484)) ;
#75156 = CARTESIAN_POINT('Ctrl Pts',(3.31247680269833,0.886307580938705,6.79874217767332)) ;
#75157 = CARTESIAN_POINT('Ctrl Pts',(3.31286385709175,0.884707693083394,6.8040040381699)) ;
#75158 = CARTESIAN_POINT('Ctrl Pts',(3.31959859765461,0.85348470139946,6.90642242752542)) ;
#75159 = CARTESIAN_POINT('Ctrl Pts',(3.31286250738096,0.819472008973411,7.00521187075637)) ;
#75160 = CARTESIAN_POINT('Ctrl Pts',(3.2881405032392,0.793313315480956,7.09446231571417)) ;
#75161 = CARTESIAN_POINT('Ctrl Pts',(3.25930415002282,0.772122965994088,7.15495237069481)) ;
#75162 = CARTESIAN_POINT('Ctrl Pts',(3.27166340593034,0.77815180520304,7.13954927383579)) ;
#75163 = CARTESIAN_POINT('Ctrl Pts',(3.28134410254902,0.786121950190065,7.11899842460839)) ;
#75164 = CARTESIAN_POINT('Ctrl Pts',(3.28814050323922,0.793313315480976,7.0944623157141)) ;
#75165 = CARTESIAN_POINT('Ctrl Pts',(3.24720304082971,0.766220050630804,7.13091195407385)) ;
#75166 = CARTESIAN_POINT('Ctrl Pts',(3.25869714385255,0.769669020390238,7.11948103534318)) ;
#75167 = CARTESIAN_POINT('Ctrl Pts',(3.26931499881139,0.775745323042673,7.10257847346906)) ;
#75168 = CARTESIAN_POINT('Ctrl Pts',(3.27713864873267,0.781672101514854,7.0815434593213)) ;
#75169 = CARTESIAN_POINT('Ctrl Pts',(3.23542257587948,0.73701785926868,7.08914722322202)) ;
#75170 = CARTESIAN_POINT('Ctrl Pts',(3.24613293999889,0.741135418665641,7.08437187855016)) ;
#75171 = CARTESIAN_POINT('Ctrl Pts',(3.25765493730861,0.747264169147483,7.07395698641591)) ;
#75172 = CARTESIAN_POINT('Ctrl Pts',(3.26627246770002,0.753460431697836,7.05898639091382)) ;
#75173 = CARTESIAN_POINT('Ctrl Pts',(3.24626907090961,0.691101901539863,7.07061000050612)) ;
#75174 = CARTESIAN_POINT('Ctrl Pts',(3.25699307007247,0.701213312565527,7.06492336370951)) ;
#75175 = CARTESIAN_POINT('Ctrl Pts',(3.26646853336989,0.711672429614719,7.05583711304386)) ;
#75176 = CARTESIAN_POINT('Ctrl Pts',(3.27341590582957,0.720540687589136,7.04364669396793)) ;
#75177 = CARTESIAN_POINT('Ctrl Pts',(3.25413500684156,0.672122965994088,7.0683761853474)) ;
#75178 = CARTESIAN_POINT('Ctrl Pts',(3.2651569253511,0.684626627018251,7.0606746369179)) ;
#75179 = CARTESIAN_POINT('Ctrl Pts',(3.27351027276397,0.697039528212523,7.05095544131491)) ;
#75180 = CARTESIAN_POINT('Ctrl Pts',(3.27942391815468,0.707077062047157,7.03908289042919)) ;
#75181 = CARTESIAN_POINT('',(3.25930415002282,0.772122965994088,7.15495237069481)) ;
#75182 = CARTESIAN_POINT('Ctrl Pts',(3.28814050323922,0.793313315480976,7.0944623157141)) ;
#75183 = CARTESIAN_POINT('Ctrl Pts',(3.28134410254902,0.786121950190065,7.11899842460839)) ;
#75184 = CARTESIAN_POINT('Ctrl Pts',(3.27166340593034,0.77815180520304,7.13954927383579)) ;
#75185 = CARTESIAN_POINT('Ctrl Pts',(3.25930415002282,0.772122965994088,7.15495237069481)) ;
#75186 = CARTESIAN_POINT('',(3.25413500684156,0.672122965994089,7.0683761853474)) ;
#75187 = CARTESIAN_POINT('Origin',(3.30314612486772,0.682245931988177,7.15495237069481)) ;
#75188 = CARTESIAN_POINT('Ctrl Pts',(3.25413500684156,0.672122965994088,7.0683761853474)) ;
#75189 = CARTESIAN_POINT('Ctrl Pts',(3.25939413790927,0.678089113547748,7.06470137568699)) ;
#75190 = CARTESIAN_POINT('Ctrl Pts',(3.26403592778354,0.684033341437091,7.06055993267801)) ;
#75191 = CARTESIAN_POINT('Ctrl Pts',(3.27227350301661,0.69552988984136,7.05122867472234)) ;
#75192 = CARTESIAN_POINT('Ctrl Pts',(3.27584190800862,0.701066725669454,7.04601233351373)) ;
#75193 = CARTESIAN_POINT('Ctrl Pts',(3.27902209145408,0.706397160160282,7.03988142131703)) ;
#75194 = CARTESIAN_POINT('Ctrl Pts',(3.27922442992696,0.706738460439687,7.03948339366842)) ;
#75195 = CARTESIAN_POINT('Ctrl Pts',(3.27942391815467,0.707077062047156,7.03908289042919)) ;
#75196 = CARTESIAN_POINT('Ctrl Pts',(3.25413500684156,0.672122965994089,7.0683761853474)) ;
#75197 = CARTESIAN_POINT('Ctrl Pts',(3.24907828834913,0.668116125762004,7.07170731541641)) ;
#75198 = CARTESIAN_POINT('Ctrl Pts',(3.23589756364382,0.660507101185358,7.07825767676846)) ;
#75199 = CARTESIAN_POINT('Ctrl Pts',(3.21994984969872,0.659191608936344,7.08122103082289)) ;
#75200 = CARTESIAN_POINT('Ctrl Pts',(3.2105035504766,0.660979117346626,7.08167176697949)) ;
#75201 = CARTESIAN_POINT('Ctrl Pts',(3.24364709226563,0.697428213388455,7.07135460555903)) ;
#75202 = CARTESIAN_POINT('Ctrl Pts',(3.23904198217673,0.694613604341688,7.07381433044803)) ;
#75203 = CARTESIAN_POINT('Ctrl Pts',(3.22806793638566,0.6897306982185,7.07820430178644)) ;
#75204 = CARTESIAN_POINT('Ctrl Pts',(3.21711227111321,0.689553339863549,7.08049944622424)) ;
#75205 = CARTESIAN_POINT('Ctrl Pts',(3.21048830525436,0.691091935293638,7.08136471265295)) ;
#75206 = CARTESIAN_POINT('Ctrl Pts',(3.23575890408185,0.743524350516923,7.09478029250273)) ;
#75207 = CARTESIAN_POINT('Ctrl Pts',(3.23142097756856,0.742576953554628,7.09766695337376)) ;
#75208 = CARTESIAN_POINT('Ctrl Pts',(3.2222182842119,0.741823967860392,7.10251922930311)) ;
#75209 = CARTESIAN_POINT('Ctrl Pts',(3.21582930459776,0.742834159269563,7.10502824890571)) ;
#75210 = CARTESIAN_POINT('Ctrl Pts',(3.21172314782629,0.74350130228817,7.10623570350962)) ;
#75211 = CARTESIAN_POINT('Ctrl Pts',(3.25022831812799,0.767695779471625,7.13692205822909)) ;
#75212 = CARTESIAN_POINT('Ctrl Pts',(3.24530748822129,0.765971442670608,7.14245586827297)) ;
#75213 = CARTESIAN_POINT('Ctrl Pts',(3.23346592056584,0.762891866825044,7.15309078996572)) ;
#75214 = CARTESIAN_POINT('Ctrl Pts',(3.22141912805696,0.76190207647211,7.15799343781877)) ;
#75215 = CARTESIAN_POINT('Ctrl Pts',(3.21434217223136,0.761999999999958,7.15898553043246)) ;
#75216 = CARTESIAN_POINT('Ctrl Pts',(3.25930415002282,0.772122965994088,7.15495237069481)) ;
#75217 = CARTESIAN_POINT('Ctrl Pts',(3.253958434241,0.769515328354208,7.16161463083282)) ;
#75218 = CARTESIAN_POINT('Ctrl Pts',(3.24030166703836,0.76423379035022,7.17471535353693)) ;
#75219 = CARTESIAN_POINT('Ctrl Pts',(3.22454046181232,0.762000000000338,7.18064206164579)) ;
#75220 = CARTESIAN_POINT('Ctrl Pts',(3.21546217518166,0.761999999999999,7.18154353395898)) ;
#75221 = CARTESIAN_POINT('',(3.2154621751798,0.761999999999999,7.18154353395898)) ;
#75222 = CARTESIAN_POINT('',(3.2105035504766,0.660979117346626,7.08167176697949)) ;
#75223 = CARTESIAN_POINT('Origin',(3.2154621751854,0.661999999999999,7.18154353395898)) ;
#75224 = CARTESIAN_POINT('Ctrl Pts',(3.2105035504766,0.660979117346626,7.08167176697949)) ;
#75225 = CARTESIAN_POINT('Ctrl Pts',(3.21994984969872,0.659191608936344,7.08122103082289)) ;
#75226 = CARTESIAN_POINT('Ctrl Pts',(3.23589756364382,0.660507101185358,7.07825767676846)) ;
#75227 = CARTESIAN_POINT('Ctrl Pts',(3.24907828834913,0.668116125762004,7.07170731541641)) ;
#75228 = CARTESIAN_POINT('Ctrl Pts',(3.25413500684156,0.672122965994089,7.0683761853474)) ;
#75229 = CARTESIAN_POINT('Ctrl Pts',(3.25930415002282,0.772122965994088,7.15495237069481)) ;
#75230 = CARTESIAN_POINT('Ctrl Pts',(3.253958434241,0.769515328354208,7.16161463083282)) ;
#75231 = CARTESIAN_POINT('Ctrl Pts',(3.24030166703836,0.76423379035022,7.17471535353693)) ;
#75232 = CARTESIAN_POINT('Ctrl Pts',(3.22454046181232,0.762000000000338,7.18064206164579)) ;
#75233 = CARTESIAN_POINT('Ctrl Pts',(3.21546217518166,0.761999999999999,7.18154353395898)) ;
#75234 = CARTESIAN_POINT('Ctrl Pts',(3.2105035504766,0.660979117346627,7.08167176697949)) ;
#75235 = CARTESIAN_POINT('Ctrl Pts',(3.20871214489261,0.66131810222033,7.08175724503273)) ;
#75236 = CARTESIAN_POINT('Ctrl Pts',(3.20691819492506,0.661658530855223,7.0818)) ;
#75237 = CARTESIAN_POINT('Ctrl Pts',(3.20512388881539,0.662,7.0818)) ;
#75238 = CARTESIAN_POINT('Ctrl Pts',(3.21048830525548,0.691091935293674,7.08136471265289)) ;
#75239 = CARTESIAN_POINT('Ctrl Pts',(3.20871266627196,0.691367100691539,7.08155544690455)) ;
#75240 = CARTESIAN_POINT('Ctrl Pts',(3.20691291140055,0.691643821063274,7.08169470978418)) ;
#75241 = CARTESIAN_POINT('Ctrl Pts',(3.20512388881539,0.691919930034189,7.0818)) ;
#75242 = CARTESIAN_POINT('Ctrl Pts',(3.21172314486594,0.743501373347166,7.10623564382333)) ;
#75243 = CARTESIAN_POINT('Ctrl Pts',(3.2095315878856,0.743584576017367,7.1065058196023)) ;
#75244 = CARTESIAN_POINT('Ctrl Pts',(3.20733490885682,0.743666470692696,7.10672585564236)) ;
#75245 = CARTESIAN_POINT('Ctrl Pts',(3.20512388881539,0.743749639050895,7.1068882100183)) ;
#75246 = CARTESIAN_POINT('Ctrl Pts',(3.21434217223511,0.762,7.15898553043244)) ;
#75247 = CARTESIAN_POINT('Ctrl Pts',(3.21127367849935,0.761999102403065,7.15918594173638)) ;
#75248 = CARTESIAN_POINT('Ctrl Pts',(3.20820121468723,0.762000880498864,7.15931169382832)) ;
#75249 = CARTESIAN_POINT('Ctrl Pts',(3.20512388881539,0.762,7.15936005247436)) ;
#75250 = CARTESIAN_POINT('Ctrl Pts',(3.2154621751854,0.762,7.18154353395898)) ;
#75251 = CARTESIAN_POINT('Ctrl Pts',(3.21201894456551,0.762,7.18171449006546)) ;
#75252 = CARTESIAN_POINT('Ctrl Pts',(3.20857144403868,0.762,7.1818)) ;
#75253 = CARTESIAN_POINT('Ctrl Pts',(3.20512388881539,0.762,7.1818)) ;
#75254 = CARTESIAN_POINT('',(3.2051238888154,0.762,7.1818)) ;
#75255 = CARTESIAN_POINT('',(3.20512388881539,0.662,7.0818)) ;
#75256 = CARTESIAN_POINT('Origin',(3.20512388881539,0.662,7.1818)) ;
#75257 = CARTESIAN_POINT('Origin',(3.20487923750922,0.663831325042322,7.00284764547056)) ;
#75258 = CARTESIAN_POINT('Origin',(3.20581132727714,0.76199999999966,7.02444419421177)) ;
#75259 = CARTESIAN_POINT('Ctrl Pts',(3.10768744607367,0.761999999467905,7.18179140434587)) ;
#75260 = CARTESIAN_POINT('Ctrl Pts',(3.10820341545623,0.762,7.18179999999999)) ;
#75261 = CARTESIAN_POINT('Ctrl Pts',(3.10871938483883,0.762,7.18179999999999)) ;
#75262 = CARTESIAN_POINT('Ctrl Pts',(3.11460889004124,0.762,7.18180000000001)) ;
#75263 = CARTESIAN_POINT('Ctrl Pts',(3.12266919377095,0.762,7.1818)) ;
#75264 = CARTESIAN_POINT('Ctrl Pts',(3.13341626541058,0.762,7.1818)) ;
#75265 = CARTESIAN_POINT('Ctrl Pts',(3.14287155003351,0.762,7.1818)) ;
#75266 = CARTESIAN_POINT('Ctrl Pts',(3.14964006674653,0.762,7.1818)) ;
#75267 = CARTESIAN_POINT('Ctrl Pts',(3.15372181554966,0.761999999999999,7.1818)) ;
#75268 = CARTESIAN_POINT('Ctrl Pts',(3.10768744607367,0.761999999467905,7.18179140434587)) ;
#75269 = CARTESIAN_POINT('Ctrl Pts',(3.10820341545672,0.76199997751292,7.18166386825364)) ;
#75270 = CARTESIAN_POINT('Ctrl Pts',(3.10871938483883,0.762,7.1815280060974)) ;
#75271 = CARTESIAN_POINT('Ctrl Pts',(3.11460889004124,0.762,7.1799608805651)) ;
#75272 = CARTESIAN_POINT('Ctrl Pts',(3.12266919377095,0.762,7.17741226428925)) ;
#75273 = CARTESIAN_POINT('Ctrl Pts',(3.13341626541058,0.762,7.17291023642561)) ;
#75274 = CARTESIAN_POINT('Ctrl Pts',(3.14287155003351,0.762,7.16868971481193)) ;
#75275 = CARTESIAN_POINT('Ctrl Pts',(3.14964006674653,0.762,7.1661262931308)) ;
#75276 = CARTESIAN_POINT('Ctrl Pts',(3.15372181554966,0.761999999999999,7.16488752501317)) ;
#75277 = CARTESIAN_POINT('Ctrl Pts',(3.10768744607367,0.761999999467905,7.18179140434587)) ;
#75278 = CARTESIAN_POINT('Ctrl Pts',(3.10820341545704,0.761999937929388,7.18142423841737)) ;
#75279 = CARTESIAN_POINT('Ctrl Pts',(3.10871938483883,0.761998151108146,7.18105256832397)) ;
#75280 = CARTESIAN_POINT('Ctrl Pts',(3.1146088900412,0.761969548435925,7.17671715413705)) ;
#75281 = CARTESIAN_POINT('Ctrl Pts',(3.12266919377094,0.761700099488059,7.16971001224105)) ;
#75282 = CARTESIAN_POINT('Ctrl Pts',(3.13341626541057,0.760034666415805,7.15732329778495)) ;
#75283 = CARTESIAN_POINT('Ctrl Pts',(3.1428715500335,0.75760394642085,7.14570932205733)) ;
#75284 = CARTESIAN_POINT('Ctrl Pts',(3.14964006674653,0.755469629013722,7.13867554654612)) ;
#75285 = CARTESIAN_POINT('Ctrl Pts',(3.15372181554965,0.754297293609929,7.13525111814463)) ;
#75286 = CARTESIAN_POINT('Ctrl Pts',(3.10768744607367,0.761999999467905,7.18179140434587)) ;
#75287 = CARTESIAN_POINT('Ctrl Pts',(3.10820341545741,0.761999898346827,7.18118461445737)) ;
#75288 = CARTESIAN_POINT('Ctrl Pts',(3.10871938483883,0.761993843816192,7.18057701642878)) ;
#75289 = CARTESIAN_POINT('Ctrl Pts',(3.11460889004116,0.761875850635945,7.17347680246517)) ;
#75290 = CARTESIAN_POINT('Ctrl Pts',(3.12266919377094,0.760857575245186,7.16195813475203)) ;
#75291 = CARTESIAN_POINT('Ctrl Pts',(3.13341626541056,0.75470827730496,7.14253521372758)) ;
#75292 = CARTESIAN_POINT('Ctrl Pts',(3.1428715500335,0.746000976828155,7.12546626554375)) ;
#75293 = CARTESIAN_POINT('Ctrl Pts',(3.14964006674653,0.738700687509333,7.11630258534313)) ;
#75294 = CARTESIAN_POINT('Ctrl Pts',(3.15372181554965,0.734844333349612,7.11213480673515)) ;
#75295 = CARTESIAN_POINT('Ctrl Pts',(3.10768744607367,0.761999999467905,7.18179140434587)) ;
#75296 = CARTESIAN_POINT('Ctrl Pts',(3.10820341545899,0.761999881560119,7.18108299149052)) ;
#75297 = CARTESIAN_POINT('Ctrl Pts',(3.10871938483884,0.76199264020277,7.18037081204062)) ;
#75298 = CARTESIAN_POINT('Ctrl Pts',(3.11460889004116,0.761810225860248,7.17211020648586)) ;
#75299 = CARTESIAN_POINT('Ctrl Pts',(3.12266919377094,0.760392329518759,7.15861536359771)) ;
#75300 = CARTESIAN_POINT('Ctrl Pts',(3.13341626541056,0.751826307912168,7.13644513645035)) ;
#75301 = CARTESIAN_POINT('Ctrl Pts',(3.1428715500335,0.739875257225671,7.11761639275596)) ;
#75302 = CARTESIAN_POINT('Ctrl Pts',(3.14964006674653,0.730040128626012,7.10821938255966)) ;
#75303 = CARTESIAN_POINT('Ctrl Pts',(3.15372181554966,0.724964736792743,7.10411096076474)) ;
#75304 = CARTESIAN_POINT('',(3.14953687287002,0.730523456132444,7.10896775467099)) ;
#75305 = CARTESIAN_POINT('',(3.14953687287002,0.762,7.1818)) ;
#75306 = CARTESIAN_POINT('Origin',(3.14953687287002,0.662,7.1818)) ;
#75307 = CARTESIAN_POINT('',(3.10768744685834,0.761999999467905,7.18179140434604)) ;
#75308 = CARTESIAN_POINT('',(3.14953687287002,0.762,7.1818)) ;
#75309 = CARTESIAN_POINT('Ctrl Pts',(3.10768744607367,0.761999999467905,7.18179140434587)) ;
#75310 = CARTESIAN_POINT('Ctrl Pts',(3.10814686764283,0.761999895879657,7.181169089747)) ;
#75311 = CARTESIAN_POINT('Ctrl Pts',(3.108595512336,0.761994276012473,7.18054760409202)) ;
#75312 = CARTESIAN_POINT('Ctrl Pts',(3.10904173751006,0.761982320202708,7.179922051077)) ;
#75313 = CARTESIAN_POINT('Ctrl Pts',(3.10910631864829,0.76198058986599,7.17983151623477)) ;
#75314 = CARTESIAN_POINT('Ctrl Pts',(3.10917084910702,0.761978727878474,7.17974098537151)) ;
#75315 = CARTESIAN_POINT('Ctrl Pts',(3.10923535422143,0.761976735136791,7.17965053196769)) ;
#75316 = CARTESIAN_POINT('Ctrl Pts',(3.10924577422062,0.761976413234149,7.17963592034497)) ;
#75317 = CARTESIAN_POINT('Ctrl Pts',(3.10925619355847,0.761976088548957,7.17962131002028)) ;
#75318 = CARTESIAN_POINT('Ctrl Pts',(3.10926661234177,0.761975761093632,7.17960670141875)) ;
#75319 = CARTESIAN_POINT('Ctrl Pts',(3.10934097866288,0.761973423810371,7.17950242936298)) ;
#75320 = CARTESIAN_POINT('Ctrl Pts',(3.10941518403546,0.761970942676249,7.17939812937458)) ;
#75321 = CARTESIAN_POINT('Ctrl Pts',(3.10948922921177,0.761968316107535,7.17929380201451)) ;
#75322 = CARTESIAN_POINT('Ctrl Pts',(3.10968668301525,0.761961311924298,7.179015595721)) ;
#75323 = CARTESIAN_POINT('Ctrl Pts',(3.10988299752596,0.761953273432761,7.17873719465478)) ;
#75324 = CARTESIAN_POINT('Ctrl Pts',(3.11007818909737,0.761944170760676,7.17845861140893)) ;
#75325 = CARTESIAN_POINT('Ctrl Pts',(3.11085895538299,0.761907760072338,7.17734427842554)) ;
#75326 = CARTESIAN_POINT('Ctrl Pts',(3.1116217541577,0.761854272437308,7.17622702027995)) ;
#75327 = CARTESIAN_POINT('Ctrl Pts',(3.11236770729956,0.761782159002747,7.17510778320945)) ;
#75328 = CARTESIAN_POINT('Ctrl Pts',(3.11385961358327,0.761637932133624,7.17286930906843)) ;
#75329 = CARTESIAN_POINT('Ctrl Pts',(3.11528416322639,0.761418774233399,7.17062291210547)) ;
#75330 = CARTESIAN_POINT('Ctrl Pts',(3.11665012530342,0.761118711339838,7.16837696163586)) ;
#75331 = CARTESIAN_POINT('Ctrl Pts',(3.11756076668811,0.760918669410798,7.16687966132279)) ;
#75332 = CARTESIAN_POINT('Ctrl Pts',(3.11844535991553,0.760682843534042,7.16538258060634)) ;
#75333 = CARTESIAN_POINT('Ctrl Pts',(3.11930647503948,0.76041094654234,7.16388813921314)) ;
#75334 = CARTESIAN_POINT('Ctrl Pts',(3.12067324691137,0.759979388496298,7.16151614457083)) ;
#75335 = CARTESIAN_POINT('Ctrl Pts',(3.12198086249394,0.759456809631881,7.15915107368702)) ;
#75336 = CARTESIAN_POINT('Ctrl Pts',(3.12323968895681,0.75884638944459,7.15680228300592)) ;
#75337 = CARTESIAN_POINT('Ctrl Pts',(3.12396045061273,0.758496883394329,7.15545744453084)) ;
#75338 = CARTESIAN_POINT('Ctrl Pts',(3.12466522294237,0.758118966837494,7.15411895662314)) ;
#75339 = CARTESIAN_POINT('Ctrl Pts',(3.12535596168084,0.757713132778189,7.15278604121403)) ;
#75340 = CARTESIAN_POINT('Ctrl Pts',(3.12587161370382,0.757410168513958,7.15179098984526)) ;
#75341 = CARTESIAN_POINT('Ctrl Pts',(3.12637944486437,0.757091653201126,7.1507990565287)) ;
#75342 = CARTESIAN_POINT('Ctrl Pts',(3.12688026881464,0.756758303828418,7.14981225466973)) ;
#75343 = CARTESIAN_POINT('Ctrl Pts',(3.12777798358105,0.756160783174511,7.14804343630581)) ;
#75344 = CARTESIAN_POINT('Ctrl Pts',(3.12865309125015,0.755514942557349,7.14628870169546)) ;
#75345 = CARTESIAN_POINT('Ctrl Pts',(3.12951212930122,0.754820486702849,7.14455120781842)) ;
#75346 = CARTESIAN_POINT('Ctrl Pts',(3.13037116735229,0.754126030848349,7.14281371394138)) ;
#75347 = CARTESIAN_POINT('Ctrl Pts',(3.13121414087768,0.753382918701887,7.14109344755347)) ;
#75348 = CARTESIAN_POINT('Ctrl Pts',(3.13204762512955,0.752589632180928,7.13939455997675)) ;
#75349 = CARTESIAN_POINT('Ctrl Pts',(3.13250636720713,0.752153014565273,7.13845950785698)) ;
#75350 = CARTESIAN_POINT('Ctrl Pts',(3.13296221766801,0.75170146888399,7.13753154269046)) ;
#75351 = CARTESIAN_POINT('Ctrl Pts',(3.13341626541056,0.751234198256885,7.1366105887522)) ;
#75352 = CARTESIAN_POINT('Ctrl Pts',(3.13461212798369,0.750003509494208,7.13418499724911)) ;
#75353 = CARTESIAN_POINT('Ctrl Pts',(3.13579548545068,0.748664969355334,7.13180786305741)) ;
#75354 = CARTESIAN_POINT('Ctrl Pts',(3.13698623201723,0.74723540828036,7.12948562600539)) ;
#75355 = CARTESIAN_POINT('Ctrl Pts',(3.13810837514584,0.745888209655321,7.12729718186106)) ;
#75356 = CARTESIAN_POINT('Ctrl Pts',(3.13923713344721,0.744459227164416,7.12515591598396)) ;
#75357 = CARTESIAN_POINT('Ctrl Pts',(3.1403891636022,0.742949052380492,7.1230703090154)) ;
#75358 = CARTESIAN_POINT('Ctrl Pts',(3.1407492773333,0.74247698602555,7.1224183680017)) ;
#75359 = CARTESIAN_POINT('Ctrl Pts',(3.14111156676817,0.741997237039512,7.12177239451161)) ;
#75360 = CARTESIAN_POINT('Ctrl Pts',(3.14147656914029,0.741510000116974,7.12113329701046)) ;
#75361 = CARTESIAN_POINT('Ctrl Pts',(3.14287298364461,0.739645944544631,7.11868825805063)) ;
#75362 = CARTESIAN_POINT('Ctrl Pts',(3.14430910606337,0.737670456610344,7.11634112949919)) ;
#75363 = CARTESIAN_POINT('Ctrl Pts',(3.14581501925236,0.735599221670195,7.11409458620081)) ;
#75364 = CARTESIAN_POINT('Ctrl Pts',(3.14662638563887,0.734483267296939,7.11288417797046)) ;
#75365 = CARTESIAN_POINT('Ctrl Pts',(3.14745801168483,0.73333986361788,7.11170358448786)) ;
#75366 = CARTESIAN_POINT('Ctrl Pts',(3.1483146025057,0.732175957104253,7.11055799739402)) ;
#75367 = CARTESIAN_POINT('Ctrl Pts',(3.14871637138839,0.73163004719238,7.11002067988431)) ;
#75368 = CARTESIAN_POINT('Ctrl Pts',(3.14912363306523,0.731079109520277,7.10949053534834)) ;
#75369 = CARTESIAN_POINT('Ctrl Pts',(3.14953687287001,0.730523456132444,7.10896775467099)) ;
#75370 = CARTESIAN_POINT('Ctrl Pts',(3.14953687287002,0.762,7.1818)) ;
#75371 = CARTESIAN_POINT('Ctrl Pts',(3.15676355558524,0.762,7.1818)) ;
#75372 = CARTESIAN_POINT('Ctrl Pts',(3.16399023830045,0.762,7.1818)) ;
#75373 = CARTESIAN_POINT('Ctrl Pts',(3.17121692101567,0.762,7.1818)) ;
#75374 = CARTESIAN_POINT('Ctrl Pts',(3.14953687287002,0.762,7.16625960724294)) ;
#75375 = CARTESIAN_POINT('Ctrl Pts',(3.15676355558524,0.762015837610647,7.16371429760845)) ;
#75376 = CARTESIAN_POINT('Ctrl Pts',(3.16399023830045,0.761980537877959,7.16173716654572)) ;
#75377 = CARTESIAN_POINT('Ctrl Pts',(3.17121692101567,0.762,7.16049051462243)) ;
#75378 = CARTESIAN_POINT('Ctrl Pts',(3.14953687287002,0.75554089351878,7.1390837819811)) ;
#75379 = CARTESIAN_POINT('Ctrl Pts',(3.15676355558524,0.75338304373689,7.13211431434399)) ;
#75380 = CARTESIAN_POINT('Ctrl Pts',(3.16399023830045,0.751152261593367,7.12667195918439)) ;
#75381 = CARTESIAN_POINT('Ctrl Pts',(3.17121692101567,0.749661462765228,7.12329552595192)) ;
#75382 = CARTESIAN_POINT('Ctrl Pts',(3.14953687287002,0.739012268865881,7.11695436533126)) ;
#75383 = CARTESIAN_POINT('Ctrl Pts',(3.15676355558524,0.731748787702952,7.10798226702609)) ;
#75384 = CARTESIAN_POINT('Ctrl Pts',(3.16399023830045,0.724623549182781,7.10220324165008)) ;
#75385 = CARTESIAN_POINT('Ctrl Pts',(3.17121692101567,0.720057683295031,7.09882570651471)) ;
#75386 = CARTESIAN_POINT('Ctrl Pts',(3.14953687287002,0.730523456132446,7.10896775467099)) ;
#75387 = CARTESIAN_POINT('Ctrl Pts',(3.15676355558524,0.720806263628135,7.09982543575316)) ;
#75388 = CARTESIAN_POINT('Ctrl Pts',(3.16399023830045,0.711535796534343,7.09468761566807)) ;
#75389 = CARTESIAN_POINT('Ctrl Pts',(3.17121692101567,0.705680904617078,7.09184457452808)) ;
#75390 = CARTESIAN_POINT('',(3.17121692101567,0.70568090461708,7.09184457452808)) ;
#75391 = CARTESIAN_POINT('',(3.17121692101567,0.762,7.1818)) ;
#75392 = CARTESIAN_POINT('Origin',(3.17121692101567,0.662,7.1818)) ;
#75393 = CARTESIAN_POINT('',(3.17121692101567,0.762,7.1818)) ;
#75394 = CARTESIAN_POINT('Ctrl Pts',(3.14953687287002,0.730523456132446,7.10896775467099)) ;
#75395 = CARTESIAN_POINT('Ctrl Pts',(3.15676355558524,0.720806263628135,7.09982543575316)) ;
#75396 = CARTESIAN_POINT('Ctrl Pts',(3.16399023830045,0.711535796534345,7.09468761566807)) ;
#75397 = CARTESIAN_POINT('Ctrl Pts',(3.17121692101567,0.705680904617079,7.09184457452808)) ;
#75398 = CARTESIAN_POINT('Ctrl Pts',(3.20512388881539,0.662000000000007,7.0818)) ;
#75399 = CARTESIAN_POINT('Ctrl Pts',(3.20472023443682,0.662977161851648,7.0818)) ;
#75400 = CARTESIAN_POINT('Ctrl Pts',(3.20391292567969,0.664831055223105,7.08182824388547)) ;
#75401 = CARTESIAN_POINT('Ctrl Pts',(3.20229830816541,0.668233044916084,7.08197050745125)) ;
#75402 = CARTESIAN_POINT('Ctrl Pts',(3.19947272751544,0.673555722181198,7.0823952931706)) ;
#75403 = CARTESIAN_POINT('Ctrl Pts',(3.19382156621548,0.682473494394306,7.08371679048587)) ;
#75404 = CARTESIAN_POINT('Ctrl Pts',(3.18413386112985,0.694361345054536,7.08684227892487)) ;
#75405 = CARTESIAN_POINT('Ctrl Pts',(3.17606077355848,0.701756526832837,7.08993895993313)) ;
#75406 = CARTESIAN_POINT('Ctrl Pts',(3.17121692101566,0.705680904617081,7.09184457452808)) ;
#75407 = CARTESIAN_POINT('Ctrl Pts',(3.20512388881539,0.691919930034194,7.0818)) ;
#75408 = CARTESIAN_POINT('Ctrl Pts',(3.20472023443682,0.692710054581024,7.08210130272039)) ;
#75409 = CARTESIAN_POINT('Ctrl Pts',(3.20391292567969,0.694201036499879,7.08268790815876)) ;
#75410 = CARTESIAN_POINT('Ctrl Pts',(3.20229830816541,0.696910532566344,7.08381855754183)) ;
#75411 = CARTESIAN_POINT('Ctrl Pts',(3.19947272751544,0.70109258926873,7.0857091269066)) ;
#75412 = CARTESIAN_POINT('Ctrl Pts',(3.19382156621548,0.707949082694699,7.08920850079664)) ;
#75413 = CARTESIAN_POINT('Ctrl Pts',(3.18413386112985,0.716769011824387,7.09473686068323)) ;
#75414 = CARTESIAN_POINT('Ctrl Pts',(3.17606077355848,0.722086120291688,7.09876158175655)) ;
#75415 = CARTESIAN_POINT('Ctrl Pts',(3.17121692101566,0.724849942854352,7.10115275051025)) ;
#75416 = CARTESIAN_POINT('Ctrl Pts',(3.20512388881539,0.743749664724925,7.10688818862076)) ;
#75417 = CARTESIAN_POINT('Ctrl Pts',(3.20472023443682,0.743987662646958,7.10735278843905)) ;
#75418 = CARTESIAN_POINT('Ctrl Pts',(3.20391292567969,0.744433617144009,7.10823510700091)) ;
#75419 = CARTESIAN_POINT('Ctrl Pts',(3.20229830816541,0.745236150925325,7.10985584551939)) ;
#75420 = CARTESIAN_POINT('Ctrl Pts',(3.19947272751544,0.746458040208068,7.11239771899758)) ;
#75421 = CARTESIAN_POINT('Ctrl Pts',(3.19382156621548,0.748404219152807,7.11670187166256)) ;
#75422 = CARTESIAN_POINT('Ctrl Pts',(3.18413386112984,0.75082846283691,7.12255514112684)) ;
#75423 = CARTESIAN_POINT('Ctrl Pts',(3.17606077355848,0.752194333174002,7.1264213810107)) ;
#75424 = CARTESIAN_POINT('Ctrl Pts',(3.17121692101566,0.75291924171095,7.12849905621401)) ;
#75425 = CARTESIAN_POINT('Ctrl Pts',(3.20512388881539,0.762000000000001,7.15936005247436)) ;
#75426 = CARTESIAN_POINT('Ctrl Pts',(3.20472023443682,0.761997480329004,7.1594984375227)) ;
#75427 = CARTESIAN_POINT('Ctrl Pts',(3.20391292567969,0.761993403439479,7.15976133310581)) ;
#75428 = CARTESIAN_POINT('Ctrl Pts',(3.20229830816542,0.76198653040893,7.16024434777636)) ;
#75429 = CARTESIAN_POINT('Ctrl Pts',(3.19947272751544,0.761977017261511,7.16100211541313)) ;
#75430 = CARTESIAN_POINT('Ctrl Pts',(3.19382156621548,0.761973864307133,7.16228718255731)) ;
#75431 = CARTESIAN_POINT('Ctrl Pts',(3.18413386112985,0.761967804257152,7.16403570034217)) ;
#75432 = CARTESIAN_POINT('Ctrl Pts',(3.17606077355848,0.762002880308166,7.16519648369734)) ;
#75433 = CARTESIAN_POINT('Ctrl Pts',(3.17121692101567,0.762,7.16581788596682)) ;
#75434 = CARTESIAN_POINT('Ctrl Pts',(3.20512388881539,0.762000000000001,7.1818)) ;
#75435 = CARTESIAN_POINT('Ctrl Pts',(3.20472023443682,0.762000000000001,7.1818)) ;
#75436 = CARTESIAN_POINT('Ctrl Pts',(3.20391292567969,0.762,7.1818)) ;
#75437 = CARTESIAN_POINT('Ctrl Pts',(3.20229830816542,0.762000000000001,7.1818)) ;
#75438 = CARTESIAN_POINT('Ctrl Pts',(3.19947272751544,0.762,7.1818)) ;
#75439 = CARTESIAN_POINT('Ctrl Pts',(3.19382156621548,0.762,7.1818)) ;
#75440 = CARTESIAN_POINT('Ctrl Pts',(3.18413386112985,0.762,7.1818)) ;
#75441 = CARTESIAN_POINT('Ctrl Pts',(3.17606077355848,0.762,7.1818)) ;
#75442 = CARTESIAN_POINT('Ctrl Pts',(3.17121692101567,0.762,7.1818)) ;
#75443 = CARTESIAN_POINT('Ctrl Pts',(3.17121692101566,0.70568090461708,7.09184457452808)) ;
#75444 = CARTESIAN_POINT('Ctrl Pts',(3.17436786852518,0.703128079505998,7.09060496380315)) ;
#75445 = CARTESIAN_POINT('Ctrl Pts',(3.17751881603471,0.700358139827596,7.0893901166366)) ;
#75446 = CARTESIAN_POINT('Ctrl Pts',(3.18236266857753,0.695601589255923,7.08759761564935)) ;
#75447 = CARTESIAN_POINT('Ctrl Pts',(3.18405557361082,0.693845452611266,7.08698598747326)) ;
#75448 = CARTESIAN_POINT('Ctrl Pts',(3.18797743406931,0.689520310025353,7.08562686578412)) ;
#75449 = CARTESIAN_POINT('Ctrl Pts',(3.19020638949449,0.68687117977675,7.08489484854452)) ;
#75450 = CARTESIAN_POINT('Ctrl Pts',(3.19343562452304,0.682587407723472,7.08393270101539)) ;
#75451 = CARTESIAN_POINT('Ctrl Pts',(3.1944359041264,0.681198456542271,7.08364897009716)) ;
#75452 = CARTESIAN_POINT('Ctrl Pts',(3.19705080124403,0.677377816432161,7.08296038741939)) ;
#75453 = CARTESIAN_POINT('Ctrl Pts',(3.1986654187583,0.674829666389823,7.08258427785979)) ;
#75454 = CARTESIAN_POINT('Ctrl Pts',(3.20108734502971,0.670514186935405,7.08215262880689)) ;
#75455 = CARTESIAN_POINT('Ctrl Pts',(3.20189465378685,0.668993420670207,7.08203130550947)) ;
#75456 = CARTESIAN_POINT('Ctrl Pts',(3.20310561692255,0.666532050590563,7.08189937136985)) ;
#75457 = CARTESIAN_POINT('Ctrl Pts',(3.20350927130112,0.665681551511474,7.08186383726635)) ;
#75458 = CARTESIAN_POINT('Ctrl Pts',(3.20431658005825,0.663904107368423,7.08181417691199)) ;
#75459 = CARTESIAN_POINT('Ctrl Pts',(3.20472023443682,0.662977161851648,7.0818)) ;
#75460 = CARTESIAN_POINT('Ctrl Pts',(3.20512388881539,0.662000000000007,7.0818)) ;
#75461 = CARTESIAN_POINT('',(3.20512388881539,0.762000000000001,7.1818)) ;
#75462 = CARTESIAN_POINT('Ctrl Pts',(3.28702640935013,0.678916496982596,7.03662526114754)) ;
#75463 = CARTESIAN_POINT('Ctrl Pts',(3.28505420805782,0.68846506114502,7.03662526114754)) ;
#75464 = CARTESIAN_POINT('Ctrl Pts',(3.28250316889159,0.697892264769897,7.03746773980168)) ;
#75465 = CARTESIAN_POINT('Ctrl Pts',(3.27942391815487,0.70707706204744,7.03908289042881)) ;
#75466 = CARTESIAN_POINT('Ctrl Pts',(3.27867914825951,0.677192417966096,7.04962706151189)) ;
#75467 = CARTESIAN_POINT('Ctrl Pts',(3.27680440972048,0.685870309279993,7.04975105769206)) ;
#75468 = CARTESIAN_POINT('Ctrl Pts',(3.2743643275819,0.694431071838907,7.05063960533657)) ;
#75469 = CARTESIAN_POINT('Ctrl Pts',(3.27140856314625,0.702764080010723,7.05223037429132)) ;
#75470 = CARTESIAN_POINT('Ctrl Pts',(3.26731641278835,0.674845509970385,7.06059580486522)) ;
#75471 = CARTESIAN_POINT('Ctrl Pts',(3.26548227953707,0.682632591536585,7.06080383849015)) ;
#75472 = CARTESIAN_POINT('Ctrl Pts',(3.26310082825167,0.690307046122249,7.06169180427166)) ;
#75473 = CARTESIAN_POINT('Ctrl Pts',(3.26021975085612,0.697769125082814,7.06320246322368)) ;
#75474 = CARTESIAN_POINT('Ctrl Pts',(3.25413500684156,0.672122965994088,7.0683761853474)) ;
#75475 = CARTESIAN_POINT('Ctrl Pts',(3.2523024532275,0.679097662424488,7.06859808108705)) ;
#75476 = CARTESIAN_POINT('Ctrl Pts',(3.24994321022021,0.685968760565752,7.0694168668701)) ;
#75477 = CARTESIAN_POINT('Ctrl Pts',(3.24710198979478,0.69264777579655,7.07077875440761)) ;
#75478 = CARTESIAN_POINT('Origin',(3.20512388881539,0.662,6.9818)) ;
#75479 = CARTESIAN_POINT('Origin',(0.,-8.2222504619082E-16,6.9818)) ;
#75480 = CARTESIAN_POINT('',(3.20512388881552,-0.661999999999843,7.0818)) ;
#75481 = CARTESIAN_POINT('Origin',(0.,-8.2222504619082E-16,7.0818)) ;
#75482 = CARTESIAN_POINT('',(3.2105035504766,-0.660979117346626,7.08167176697949)) ;
#75483 = CARTESIAN_POINT('Origin',(3.20487923730672,-0.663831325588436,7.00284762309432)) ;
#75484 = CARTESIAN_POINT('',(3.25413500684125,-0.672122965993743,7.06837618534762)) ;
#75485 = CARTESIAN_POINT('Ctrl Pts',(3.25413500684122,-0.672122965993823,
7.06837618534763)) ;
#75486 = CARTESIAN_POINT('Ctrl Pts',(3.24907828834881,-0.66811612576181,7.07170731541658)) ;
#75487 = CARTESIAN_POINT('Ctrl Pts',(3.23589756364359,-0.660507101185318,
7.07825767676852)) ;
#75488 = CARTESIAN_POINT('Ctrl Pts',(3.21994984969863,-0.659191608936361,
7.0812210308229)) ;
#75489 = CARTESIAN_POINT('Ctrl Pts',(3.2105035504766,-0.660979117346626,7.08167176697949)) ;
#75490 = CARTESIAN_POINT('Origin',(3.20512388881547,-0.66199999999964,6.9818)) ;
#75491 = CARTESIAN_POINT('Ctrl Pts',(3.31205160669424,-0.887893661760288,
6.793484)) ;
#75492 = CARTESIAN_POINT('Ctrl Pts',(3.31247680274145,-0.886307580777865,
6.79874217793995)) ;
#75493 = CARTESIAN_POINT('Ctrl Pts',(3.31286385708463,-0.884707693113238,
6.80400403812143)) ;
#75494 = CARTESIAN_POINT('Ctrl Pts',(3.31959859780673,-0.853484700721658,
6.90642242863736)) ;
#75495 = CARTESIAN_POINT('Ctrl Pts',(3.31286250738096,-0.819472008973418,
7.00521187075635)) ;
#75496 = CARTESIAN_POINT('Ctrl Pts',(3.28814050323921,-0.793313315480963,
7.09446231571415)) ;
#75497 = CARTESIAN_POINT('Ctrl Pts',(3.31205160669424,-0.887893661760288,
6.793484)) ;
#75498 = CARTESIAN_POINT('Ctrl Pts',(3.31261121118724,-0.885806205750656,
6.79841624509091)) ;
#75499 = CARTESIAN_POINT('Ctrl Pts',(3.31307594580264,-0.883698810485554,
6.80336333516764)) ;
#75500 = CARTESIAN_POINT('Ctrl Pts',(3.32193595557477,-0.842609792739121,
6.89941056465093)) ;
#75501 = CARTESIAN_POINT('Ctrl Pts',(3.30625449205529,-0.797119135192673,
6.99229450465508)) ;
#75502 = CARTESIAN_POINT('Ctrl Pts',(3.26888725785269,-0.7729411910402,7.07185431702684)) ;
#75503 = CARTESIAN_POINT('Ctrl Pts',(3.31205160669424,-0.887893661760288,
6.793484)) ;
#75504 = CARTESIAN_POINT('Ctrl Pts',(3.31274522373845,-0.885306307503065,
6.79809343311384)) ;
#75505 = CARTESIAN_POINT('Ctrl Pts',(3.31334303732283,-0.882699040486607,
6.80271791140361)) ;
#75506 = CARTESIAN_POINT('Ctrl Pts',(3.32434030429396,-0.831838892287652,
6.89249111351254)) ;
#75507 = CARTESIAN_POINT('Ctrl Pts',(3.30868757227878,-0.775373519472595,
6.97904841531995)) ;
#75508 = CARTESIAN_POINT('Ctrl Pts',(3.26540522272931,-0.738492188311667,
7.04973176535317)) ;
#75509 = CARTESIAN_POINT('Ctrl Pts',(3.31205160669424,-0.887893661760288,
6.793484)) ;
#75510 = CARTESIAN_POINT('Ctrl Pts',(3.31287790157776,-0.884811388043908,
6.79777468368237)) ;
#75511 = CARTESIAN_POINT('Ctrl Pts',(3.31364139250205,-0.881705147317766,
6.80206837149932)) ;
#75512 = CARTESIAN_POINT('Ctrl Pts',(3.32718180880554,-0.821152481073567,
6.88564197832078)) ;
#75513 = CARTESIAN_POINT('Ctrl Pts',(3.31839899815499,-0.756128366293962,
6.96625435392856)) ;
#75514 = CARTESIAN_POINT('Ctrl Pts',(3.27942391815451,-0.707077062047025,
7.03908289042947)) ;
#75515 = CARTESIAN_POINT('',(3.28814050323921,-0.793313315480963,7.09446231571415)) ;
#75516 = CARTESIAN_POINT('Origin',(3.36081883130048,-0.724626630961926,7.09446231571415)) ;
#75517 = CARTESIAN_POINT('Ctrl Pts',(3.28814050323921,-0.793313315480963,
7.09446231571415)) ;
#75518 = CARTESIAN_POINT('Ctrl Pts',(3.31286250738096,-0.819472008973418,
7.00521187075635)) ;
#75519 = CARTESIAN_POINT('Ctrl Pts',(3.31959859780673,-0.853484700721658,
6.90642242863736)) ;
#75520 = CARTESIAN_POINT('Ctrl Pts',(3.31286385708463,-0.884707693113238,
6.80400403812143)) ;
#75521 = CARTESIAN_POINT('Ctrl Pts',(3.31247680274145,-0.886307580777865,
6.79874217793995)) ;
#75522 = CARTESIAN_POINT('Ctrl Pts',(3.31205160669424,-0.887893661760288,
6.793484)) ;
#75523 = CARTESIAN_POINT('Ctrl Pts',(3.28814050323922,-0.793313315480982,
7.09446231571408)) ;
#75524 = CARTESIAN_POINT('Ctrl Pts',(3.28134410252723,-0.786121950167006,
7.11899842468707)) ;
#75525 = CARTESIAN_POINT('Ctrl Pts',(3.27166340596969,-0.778151805222174,
7.13954927378692)) ;
#75526 = CARTESIAN_POINT('Ctrl Pts',(3.25930415002248,-0.77212296599392,7.15495237069524)) ;
#75527 = CARTESIAN_POINT('Ctrl Pts',(3.27713864873268,-0.781672101514859,
7.08154345932128)) ;
#75528 = CARTESIAN_POINT('Ctrl Pts',(3.2693149987863,-0.775745323023668,7.10257847353651)) ;
#75529 = CARTESIAN_POINT('Ctrl Pts',(3.25869714388911,-0.76966902040116,7.11948103530695)) ;
#75530 = CARTESIAN_POINT('Ctrl Pts',(3.24720304082939,-0.766220050630705,
7.13091195407417)) ;
#75531 = CARTESIAN_POINT('Ctrl Pts',(3.26627246770002,-0.753460431697841,
7.05898639091381)) ;
#75532 = CARTESIAN_POINT('Ctrl Pts',(3.25765493728098,-0.747264169127614,
7.07395698646391)) ;
#75533 = CARTESIAN_POINT('Ctrl Pts',(3.24613294003293,-0.741135418678703,
7.08437187853508)) ;
#75534 = CARTESIAN_POINT('Ctrl Pts',(3.23542257587918,-0.737017859268566,
7.08914722322215)) ;
#75535 = CARTESIAN_POINT('Ctrl Pts',(3.27341590582958,-0.720540687589143,
7.04364669396792)) ;
#75536 = CARTESIAN_POINT('Ctrl Pts',(3.26646853334762,-0.711672429586283,
7.05583711308295)) ;
#75537 = CARTESIAN_POINT('Ctrl Pts',(3.25699307010659,-0.701213312597675,
7.06492336369149)) ;
#75538 = CARTESIAN_POINT('Ctrl Pts',(3.24626907090931,-0.691101901539582,
7.07061000050628)) ;
#75539 = CARTESIAN_POINT('Ctrl Pts',(3.27942391815468,-0.707077062047165,
7.03908289042918)) ;
#75540 = CARTESIAN_POINT('Ctrl Pts',(3.27351027274501,-0.697039528180338,
7.05095544135298)) ;
#75541 = CARTESIAN_POINT('Ctrl Pts',(3.26515692538619,-0.684626627058012,
7.06067463689345)) ;
#75542 = CARTESIAN_POINT('Ctrl Pts',(3.25413500684125,-0.67212296599374,7.06837618534762)) ;
#75543 = CARTESIAN_POINT('',(3.25930415002248,-0.77212296599392,7.15495237069524)) ;
#75544 = CARTESIAN_POINT('Origin',(3.30314612486703,-0.682245931987841,7.15495237069524)) ;
#75545 = CARTESIAN_POINT('Ctrl Pts',(3.25930415002248,-0.77212296599392,7.15495237069524)) ;
#75546 = CARTESIAN_POINT('Ctrl Pts',(3.27166340596969,-0.778151805222174,
7.13954927378692)) ;
#75547 = CARTESIAN_POINT('Ctrl Pts',(3.28134410252723,-0.786121950167006,
7.11899842468707)) ;
#75548 = CARTESIAN_POINT('Ctrl Pts',(3.28814050323922,-0.793313315480982,
7.09446231571408)) ;
#75549 = CARTESIAN_POINT('Ctrl Pts',(3.27942391815468,-0.707077062047165,
7.03908289042918)) ;
#75550 = CARTESIAN_POINT('Ctrl Pts',(3.27645386391631,-0.702035836552783,
7.04504573022574)) ;
#75551 = CARTESIAN_POINT('Ctrl Pts',(3.27285683396309,-0.696395529146179,
7.05045952340178)) ;
#75552 = CARTESIAN_POINT('Ctrl Pts',(3.26443586616536,-0.684547202104048,
7.06020168149165)) ;
#75553 = CARTESIAN_POINT('Ctrl Pts',(3.25962130503333,-0.678346820108753,
7.06454264301213)) ;
#75554 = CARTESIAN_POINT('Ctrl Pts',(3.25413500684125,-0.67212296599374,7.06837618534762)) ;
#75555 = CARTESIAN_POINT('Ctrl Pts',(3.25930415002247,-0.772122965993915,
7.15495237069525)) ;
#75556 = CARTESIAN_POINT('Ctrl Pts',(3.25395843424068,-0.769515328354075,
7.16161463083315)) ;
#75557 = CARTESIAN_POINT('Ctrl Pts',(3.24030166703813,-0.764233790350177,
7.17471535353703)) ;
#75558 = CARTESIAN_POINT('Ctrl Pts',(3.22454046181224,-0.762000000000338,
7.1806420616458)) ;
#75559 = CARTESIAN_POINT('Ctrl Pts',(3.21546217518166,-0.761999999999999,
7.18154353395898)) ;
#75560 = CARTESIAN_POINT('Ctrl Pts',(3.24720304082939,-0.766220050630709,
7.13091195407419)) ;
#75561 = CARTESIAN_POINT('Ctrl Pts',(3.242421550768,-0.764811276693603,7.13604987867788)) ;
#75562 = CARTESIAN_POINT('Ctrl Pts',(3.2311564898124,-0.762486695804742,7.14584148266612)) ;
#75563 = CARTESIAN_POINT('Ctrl Pts',(3.22034137761648,-0.761874515288824,
7.15043685312202)) ;
#75564 = CARTESIAN_POINT('Ctrl Pts',(3.2139688379146,-0.761999999999944,7.15146619592362)) ;
#75565 = CARTESIAN_POINT('Ctrl Pts',(3.23542257429462,-0.737017860463238,
7.08914722161447)) ;
#75566 = CARTESIAN_POINT('Ctrl Pts',(3.23109773333057,-0.735867125998988,
7.09171940959733)) ;
#75567 = CARTESIAN_POINT('Ctrl Pts',(3.22191662758841,-0.734718108963128,
7.09591659196459)) ;
#75568 = CARTESIAN_POINT('Ctrl Pts',(3.21551228030165,-0.735734718330495,
7.09816262873452)) ;
#75569 = CARTESIAN_POINT('Ctrl Pts',(3.21138266038765,-0.736564632620707,
7.0993779386748)) ;
#75570 = CARTESIAN_POINT('Ctrl Pts',(3.2462690709093,-0.691101901539656,7.0706100005063)) ;
#75571 = CARTESIAN_POINT('Ctrl Pts',(3.24155281302069,-0.687974876169227,
7.07330389695565)) ;
#75572 = CARTESIAN_POINT('Ctrl Pts',(3.23004851902068,-0.682396466707053,
7.07825157589535)) ;
#75573 = CARTESIAN_POINT('Ctrl Pts',(3.21784961482896,-0.681959937337743,
7.08068560732117)) ;
#75574 = CARTESIAN_POINT('Ctrl Pts',(3.21049211655992,-0.683563730806885,
7.08144147623458)) ;
#75575 = CARTESIAN_POINT('Ctrl Pts',(3.25413500684122,-0.672122965993823,
7.06837618534763)) ;
#75576 = CARTESIAN_POINT('Ctrl Pts',(3.24907828834881,-0.66811612576181,7.07170731541658)) ;
#75577 = CARTESIAN_POINT('Ctrl Pts',(3.23589756364359,-0.660507101185318,
7.07825767676852)) ;
#75578 = CARTESIAN_POINT('Ctrl Pts',(3.21994984969863,-0.659191608936361,
7.0812210308229)) ;
#75579 = CARTESIAN_POINT('Ctrl Pts',(3.2105035504766,-0.660979117346626,7.08167176697949)) ;
#75580 = CARTESIAN_POINT('',(3.2154621751798,-0.761999999999999,7.18154353395898)) ;
#75581 = CARTESIAN_POINT('Origin',(3.2154621751854,-0.661999999999999,7.18154353395898)) ;
#75582 = CARTESIAN_POINT('Ctrl Pts',(3.21546217518166,-0.761999999999999,
7.18154353395898)) ;
#75583 = CARTESIAN_POINT('Ctrl Pts',(3.22454046181224,-0.762000000000338,
7.1806420616458)) ;
#75584 = CARTESIAN_POINT('Ctrl Pts',(3.24030166703813,-0.764233790350177,
7.17471535353703)) ;
#75585 = CARTESIAN_POINT('Ctrl Pts',(3.25395843424068,-0.769515328354075,
7.16161463083315)) ;
#75586 = CARTESIAN_POINT('Ctrl Pts',(3.25930415002247,-0.772122965993915,
7.15495237069525)) ;
#75587 = CARTESIAN_POINT('Ctrl Pts',(3.2154621751854,-0.762,7.18154353395898)) ;
#75588 = CARTESIAN_POINT('Ctrl Pts',(3.21201894456566,-0.762,7.18171449006545)) ;
#75589 = CARTESIAN_POINT('Ctrl Pts',(3.20857144403885,-0.762,7.1818)) ;
#75590 = CARTESIAN_POINT('Ctrl Pts',(3.20512388881564,-0.762,7.1818)) ;
#75591 = CARTESIAN_POINT('Ctrl Pts',(3.21396883791835,-0.762,7.15146619592359)) ;
#75592 = CARTESIAN_POINT('Ctrl Pts',(3.21102860740559,-0.761997290973651,
7.15167826758758)) ;
#75593 = CARTESIAN_POINT('Ctrl Pts',(3.20807464984533,-0.762002680217736,
7.15181361851019)) ;
#75594 = CARTESIAN_POINT('Ctrl Pts',(3.20512388881561,-0.762,7.15188006996581)) ;
#75595 = CARTESIAN_POINT('Ctrl Pts',(3.21138265683666,-0.736564691651965,
7.0993778670976)) ;
#75596 = CARTESIAN_POINT('Ctrl Pts',(3.20930558735075,-0.736681278140644,
7.09965201966661)) ;
#75597 = CARTESIAN_POINT('Ctrl Pts',(3.20722130366678,-0.7367952805891,7.09987813004075)) ;
#75598 = CARTESIAN_POINT('Ctrl Pts',(3.20512388881554,-0.736911789981695,
7.1000503609491)) ;
#75599 = CARTESIAN_POINT('Ctrl Pts',(3.21049211656076,-0.683563730806912,
7.08144147623454)) ;
#75600 = CARTESIAN_POINT('Ctrl Pts',(3.20870975639604,-0.683855790193559,
7.08160438817637)) ;
#75601 = CARTESIAN_POINT('Ctrl Pts',(3.20691685125597,-0.684146559499709,
7.08172265074698)) ;
#75602 = CARTESIAN_POINT('Ctrl Pts',(3.20512388881552,-0.68443994752562,7.08179999999999)) ;
#75603 = CARTESIAN_POINT('Ctrl Pts',(3.2105035504766,-0.660979117346626,7.08167176697949)) ;
#75604 = CARTESIAN_POINT('Ctrl Pts',(3.20871214489269,-0.661318102220315,
7.08175724503272)) ;
#75605 = CARTESIAN_POINT('Ctrl Pts',(3.20691819492514,-0.661658530855206,
7.0818)) ;
#75606 = CARTESIAN_POINT('Ctrl Pts',(3.20512388881552,-0.661999999999975,
7.0818)) ;
#75607 = CARTESIAN_POINT('',(3.20512388881569,-0.762,7.1818)) ;
#75608 = CARTESIAN_POINT('Origin',(3.20512388881569,-0.662,7.1818)) ;
#75609 = CARTESIAN_POINT('Origin',(3.20581132625523,-0.762,7.02444416805792)) ;
#75610 = CARTESIAN_POINT('Ctrl Pts',(3.14953687287001,-0.762,7.1818)) ;
#75611 = CARTESIAN_POINT('Ctrl Pts',(3.14687049251069,-0.762,7.1818)) ;
#75612 = CARTESIAN_POINT('Ctrl Pts',(3.14153773179204,-0.762,7.1818)) ;
#75613 = CARTESIAN_POINT('Ctrl Pts',(3.13353859071408,-0.762,7.1818)) ;
#75614 = CARTESIAN_POINT('Ctrl Pts',(3.12287306927679,-0.762,7.1818)) ;
#75615 = CARTESIAN_POINT('Ctrl Pts',(3.11487392819883,-0.762,7.18180000000002)) ;
#75616 = CARTESIAN_POINT('Ctrl Pts',(3.10892329344282,-0.762,7.18179999999999)) ;
#75617 = CARTESIAN_POINT('Ctrl Pts',(3.10830541940544,-0.762,7.18179999999999)) ;
#75618 = CARTESIAN_POINT('Ctrl Pts',(3.1076875453681,-0.761999999459305,7.181791335163)) ;
#75619 = CARTESIAN_POINT('Ctrl Pts',(3.14953687287001,-0.762,7.16625960724294)) ;
#75620 = CARTESIAN_POINT('Ctrl Pts',(3.14687049251069,-0.762,7.16719533415535)) ;
#75621 = CARTESIAN_POINT('Ctrl Pts',(3.14153773179204,-0.762,7.16928720206195)) ;
#75622 = CARTESIAN_POINT('Ctrl Pts',(3.13353859071408,-0.762,7.17285503844539)) ;
#75623 = CARTESIAN_POINT('Ctrl Pts',(3.12287306927679,-0.762,7.1773342191656)) ;
#75624 = CARTESIAN_POINT('Ctrl Pts',(3.11487392819883,-0.762,7.17988076928538)) ;
#75625 = CARTESIAN_POINT('Ctrl Pts',(3.10892329344282,-0.762,7.18147431730214)) ;
#75626 = CARTESIAN_POINT('Ctrl Pts',(3.10830541940608,-0.761999972911341,
7.18163761817159)) ;
#75627 = CARTESIAN_POINT('Ctrl Pts',(3.1076875453681,-0.761999999459305,7.181791335163)) ;
#75628 = CARTESIAN_POINT('Ctrl Pts',(3.14953687287001,-0.755540898601866,
7.13908377950685)) ;
#75629 = CARTESIAN_POINT('Ctrl Pts',(3.14687049251069,-0.756336720063884,
7.14165588380709)) ;
#75630 = CARTESIAN_POINT('Ctrl Pts',(3.14153773179204,-0.757950944893126,
7.1473932880007)) ;
#75631 = CARTESIAN_POINT('Ctrl Pts',(3.13353859071408,-0.760010135143031,
7.15719931177908)) ;
#75632 = CARTESIAN_POINT('Ctrl Pts',(3.12287306927679,-0.761680931514211,
7.16950958656739)) ;
#75633 = CARTESIAN_POINT('Ctrl Pts',(3.11487392819882,-0.761961216508624,
7.17650146037765)) ;
#75634 = CARTESIAN_POINT('Ctrl Pts',(3.10892329344283,-0.761997488316066,
7.1809061971102)) ;
#75635 = CARTESIAN_POINT('Ctrl Pts',(3.10830541940668,-0.761999925297214,
7.18135219728602)) ;
#75636 = CARTESIAN_POINT('Ctrl Pts',(3.1076875453681,-0.761999999459305,7.181791335163)) ;
#75637 = CARTESIAN_POINT('Ctrl Pts',(3.14953687287001,-0.739012268865882,
7.11695436533127)) ;
#75638 = CARTESIAN_POINT('Ctrl Pts',(3.14687049251069,-0.741696873122348,
7.12026196115736)) ;
#75639 = CARTESIAN_POINT('Ctrl Pts',(3.14153773179204,-0.747258461773346,
7.12796089840492)) ;
#75640 = CARTESIAN_POINT('Ctrl Pts',(3.13353859071408,-0.754625778477829,
7.14235903254706)) ;
#75641 = CARTESIAN_POINT('Ctrl Pts',(3.12287306927679,-0.760786688692489,
7.16164067068996)) ;
#75642 = CARTESIAN_POINT('Ctrl Pts',(3.11487392819881,-0.761845223870069,
7.17312655589753)) ;
#75643 = CARTESIAN_POINT('Ctrl Pts',(3.10892329344283,-0.761991471478693,
7.18033789111251)) ;
#75644 = CARTESIAN_POINT('Ctrl Pts',(3.10830541940737,-0.761999877690589,
7.18106682137182)) ;
#75645 = CARTESIAN_POINT('Ctrl Pts',(3.1076875453681,-0.761999999459305,7.181791335163)) ;
#75646 = CARTESIAN_POINT('Ctrl Pts',(3.14953687287001,-0.730523456132448,
7.10896775467099)) ;
#75647 = CARTESIAN_POINT('Ctrl Pts',(3.14687049251069,-0.73410874308391,7.11234093439422)) ;
#75648 = CARTESIAN_POINT('Ctrl Pts',(3.14153773179204,-0.741620611340461,
7.12039126652058)) ;
#75649 = CARTESIAN_POINT('Ctrl Pts',(3.13353859071408,-0.751722671583157,
7.13626512379224)) ;
#75650 = CARTESIAN_POINT('Ctrl Pts',(3.12287306927679,-0.760294668466002,
7.15825743733922)) ;
#75651 = CARTESIAN_POINT('Ctrl Pts',(3.11487392819881,-0.761768784449911,
7.17170556214749)) ;
#75652 = CARTESIAN_POINT('Ctrl Pts',(3.10892329344284,-0.761989456647343,
7.18009206761753)) ;
#75653 = CARTESIAN_POINT('Ctrl Pts',(3.10830541940898,-0.761999857549363,
7.18094608564176)) ;
#75654 = CARTESIAN_POINT('Ctrl Pts',(3.1076875453681,-0.761999999459305,7.181791335163)) ;
#75655 = CARTESIAN_POINT('',(3.14953687287002,-0.730523456132445,7.10896775467099)) ;
#75656 = CARTESIAN_POINT('',(3.1076875453681,-0.761999999459305,7.181791335163)) ;
#75657 = CARTESIAN_POINT('Ctrl Pts',(3.14953687287001,-0.730523456132448,
7.10896775467099)) ;
#75658 = CARTESIAN_POINT('Ctrl Pts',(3.14797942264904,-0.732617645708692,
7.11093805102685)) ;
#75659 = CARTESIAN_POINT('Ctrl Pts',(3.1465061713264,-0.734653328663648,7.11301990160851)) ;
#75660 = CARTESIAN_POINT('Ctrl Pts',(3.14387447911892,-0.738267803994675,
7.117061211881)) ;
#75661 = CARTESIAN_POINT('Ctrl Pts',(3.1427034903174,-0.739869147575639,7.11898772024392)) ;
#75662 = CARTESIAN_POINT('Ctrl Pts',(3.14003426783858,-0.743434587735941,
7.12365091140022)) ;
#75663 = CARTESIAN_POINT('Ctrl Pts',(3.13853950336846,-0.745372263846278,
7.12646051120024)) ;
#75664 = CARTESIAN_POINT('Ctrl Pts',(3.13653043645198,-0.74778851672796,7.13038311670479)) ;
#75665 = CARTESIAN_POINT('Ctrl Pts',(3.13605624929057,-0.748345460226584,
7.13131929065347)) ;
#75666 = CARTESIAN_POINT('Ctrl Pts',(3.13490033520594,-0.749663329733279,
7.13362022192598)) ;
#75667 = CARTESIAN_POINT('Ctrl Pts',(3.13422097401358,-0.750405386417455,
7.13498790652006)) ;
#75668 = CARTESIAN_POINT('Ctrl Pts',(3.13116298082121,-0.753565217081952,
7.14117490868328)) ;
#75669 = CARTESIAN_POINT('Ctrl Pts',(3.12875074376133,-0.755569934781551,
7.14614171575595)) ;
#75670 = CARTESIAN_POINT('Ctrl Pts',(3.1260549976317,-0.757288072049574,7.15142011655119)) ;
#75671 = CARTESIAN_POINT('Ctrl Pts',(3.12579736320653,-0.757447091715282,
7.15192182249422)) ;
#75672 = CARTESIAN_POINT('Ctrl Pts',(3.12252085545441,-0.759403938221167,
7.15826208088107)) ;
#75673 = CARTESIAN_POINT('Ctrl Pts',(3.11946402361198,-0.760518781992785,
7.16374175989977)) ;
#75674 = CARTESIAN_POINT('Ctrl Pts',(3.11411364459364,-0.761651866001623,
7.17250976794735)) ;
#75675 = CARTESIAN_POINT('Ctrl Pts',(3.11182848381899,-0.761881721124906,
7.17599764811772)) ;
#75676 = CARTESIAN_POINT('Ctrl Pts',(3.10892339826902,-0.761989452759989,
7.18009191988114)) ;
#75677 = CARTESIAN_POINT('Ctrl Pts',(3.10830547182207,-0.761999857537325,
7.18094601394084)) ;
#75678 = CARTESIAN_POINT('Ctrl Pts',(3.1076875453681,-0.761999999459305,7.181791335163)) ;
#75679 = CARTESIAN_POINT('',(3.14953687287001,-0.762,7.1818)) ;
#75680 = CARTESIAN_POINT('',(3.1076875453681,-0.761999999459305,7.181791335163)) ;
#75681 = CARTESIAN_POINT('Origin',(3.14953687287001,-0.661999999999999,7.1818)) ;
#75682 = CARTESIAN_POINT('Ctrl Pts',(3.17121692101567,-0.762,7.1818)) ;
#75683 = CARTESIAN_POINT('Ctrl Pts',(3.16399023830045,-0.762,7.1818)) ;
#75684 = CARTESIAN_POINT('Ctrl Pts',(3.15676355558524,-0.762,7.1818)) ;
#75685 = CARTESIAN_POINT('Ctrl Pts',(3.14953687287003,-0.762,7.1818)) ;
#75686 = CARTESIAN_POINT('Ctrl Pts',(3.17121692101567,-0.762,7.16049051462243)) ;
#75687 = CARTESIAN_POINT('Ctrl Pts',(3.16399023830045,-0.761980537877959,
7.16173716654572)) ;
#75688 = CARTESIAN_POINT('Ctrl Pts',(3.15676355558524,-0.762015837610647,
7.16371429760845)) ;
#75689 = CARTESIAN_POINT('Ctrl Pts',(3.14953687287003,-0.762,7.16625960724294)) ;
#75690 = CARTESIAN_POINT('Ctrl Pts',(3.17121692101567,-0.749661462765229,
7.12329552595192)) ;
#75691 = CARTESIAN_POINT('Ctrl Pts',(3.16399023830045,-0.751152261593368,
7.12667195918439)) ;
#75692 = CARTESIAN_POINT('Ctrl Pts',(3.15676355558524,-0.753383043736888,
7.13211431434399)) ;
#75693 = CARTESIAN_POINT('Ctrl Pts',(3.14953687287003,-0.755540893518777,
7.1390837819811)) ;
#75694 = CARTESIAN_POINT('Ctrl Pts',(3.17121692101567,-0.720057683295034,
7.09882570651471)) ;
#75695 = CARTESIAN_POINT('Ctrl Pts',(3.16399023830045,-0.724623549182783,
7.10220324165009)) ;
#75696 = CARTESIAN_POINT('Ctrl Pts',(3.15676355558524,-0.731748787702946,
7.10798226702609)) ;
#75697 = CARTESIAN_POINT('Ctrl Pts',(3.14953687287003,-0.739012268865874,
7.11695436533126)) ;
#75698 = CARTESIAN_POINT('Ctrl Pts',(3.17121692101567,-0.705680904617081,
7.09184457452808)) ;
#75699 = CARTESIAN_POINT('Ctrl Pts',(3.16399023830045,-0.711535796534346,
7.09468761566807)) ;
#75700 = CARTESIAN_POINT('Ctrl Pts',(3.15676355558524,-0.720806263628127,
7.09982543575315)) ;
#75701 = CARTESIAN_POINT('Ctrl Pts',(3.14953687287002,-0.730523456132438,
7.10896775467099)) ;
#75702 = CARTESIAN_POINT('',(3.17121692101567,-0.762,7.1818)) ;
#75703 = CARTESIAN_POINT('',(3.14953687287003,-0.762,7.1818)) ;
#75704 = CARTESIAN_POINT('',(3.17121692101567,-0.70568090461708,7.09184457452808)) ;
#75705 = CARTESIAN_POINT('Origin',(3.17121692101567,-0.662000000000001,7.1818)) ;
#75706 = CARTESIAN_POINT('Ctrl Pts',(3.17121692101567,-0.705680904617081,
7.09184457452808)) ;
#75707 = CARTESIAN_POINT('Ctrl Pts',(3.16399023830045,-0.711535796534346,
7.09468761566807)) ;
#75708 = CARTESIAN_POINT('Ctrl Pts',(3.15676355558524,-0.720806263628127,
7.09982543575315)) ;
#75709 = CARTESIAN_POINT('Ctrl Pts',(3.14953687287002,-0.730523456132438,
7.10896775467099)) ;
#75710 = CARTESIAN_POINT('Ctrl Pts',(3.20512388881546,-0.762,7.1818)) ;
#75711 = CARTESIAN_POINT('Ctrl Pts',(3.2047202344369,-0.762,7.1818)) ;
#75712 = CARTESIAN_POINT('Ctrl Pts',(3.20391292567976,-0.762,7.1818)) ;
#75713 = CARTESIAN_POINT('Ctrl Pts',(3.20270196254405,-0.762,7.1818)) ;
#75714 = CARTESIAN_POINT('Ctrl Pts',(3.20149099940834,-0.762,7.1818)) ;
#75715 = CARTESIAN_POINT('Ctrl Pts',(3.19745445562265,-0.762,7.1818)) ;
#75716 = CARTESIAN_POINT('Ctrl Pts',(3.18736309615843,-0.762,7.1818)) ;
#75717 = CARTESIAN_POINT('Ctrl Pts',(3.17767539107277,-0.762,7.1818)) ;
#75718 = CARTESIAN_POINT('Ctrl Pts',(3.17121692101566,-0.762,7.1818)) ;
#75719 = CARTESIAN_POINT('Ctrl Pts',(3.20512388881546,-0.762,7.15188006996578)) ;
#75720 = CARTESIAN_POINT('Ctrl Pts',(3.2047202344369,-0.761992330181026,7.1520702301264)) ;
#75721 = CARTESIAN_POINT('Ctrl Pts',(3.20391292567976,-0.76197980992607,7.15243005278884)) ;
#75722 = CARTESIAN_POINT('Ctrl Pts',(3.20270196254405,-0.761963555547577,
7.15292464422255)) ;
#75723 = CARTESIAN_POINT('Ctrl Pts',(3.20149099940834,-0.761947562028464,
7.15338566691011)) ;
#75724 = CARTESIAN_POINT('Ctrl Pts',(3.19745445562265,-0.76191470846392,7.15481366906456)) ;
#75725 = CARTESIAN_POINT('Ctrl Pts',(3.18736309615843,-0.761861071074269,
7.15758629528363)) ;
#75726 = CARTESIAN_POINT('Ctrl Pts',(3.17767539107277,-0.76201739325461,7.15937638460794)) ;
#75727 = CARTESIAN_POINT('Ctrl Pts',(3.17121692101566,-0.762,7.16049051462243)) ;
#75728 = CARTESIAN_POINT('Ctrl Pts',(3.20512388881546,-0.736911811379185,
7.100050335275)) ;
#75729 = CARTESIAN_POINT('Ctrl Pts',(3.2047202344369,-0.737245219347507,7.10054319817604)) ;
#75730 = CARTESIAN_POINT('Ctrl Pts',(3.20391292567976,-0.737869883520251,
7.10148033026225)) ;
#75731 = CARTESIAN_POINT('Ctrl Pts',(3.20270196254405,-0.738711770607015,
7.10277348618571)) ;
#75732 = CARTESIAN_POINT('Ctrl Pts',(3.20149099940834,-0.73948195346955,7.10398042484261)) ;
#75733 = CARTESIAN_POINT('Ctrl Pts',(3.19745445562265,-0.74182919721765,7.10775251408813)) ;
#75734 = CARTESIAN_POINT('Ctrl Pts',(3.18736309615843,-0.746011102788114,
7.11515718689346)) ;
#75735 = CARTESIAN_POINT('Ctrl Pts',(3.17767539107277,-0.748329114460406,
7.12027803292724)) ;
#75736 = CARTESIAN_POINT('Ctrl Pts',(3.17121692101566,-0.749661438013567,
7.12329554369824)) ;
#75737 = CARTESIAN_POINT('Ctrl Pts',(3.20512388881546,-0.684439947525498,
7.08179999999996)) ;
#75738 = CARTESIAN_POINT('Ctrl Pts',(3.20472023443689,-0.685279518511759,
7.08202134573632)) ;
#75739 = CARTESIAN_POINT('Ctrl Pts',(3.20391292567976,-0.686865903002592,
7.08246093200817)) ;
#75740 = CARTESIAN_POINT('Ctrl Pts',(3.20270196254405,-0.689032722166202,
7.08311409360665)) ;
#75741 = CARTESIAN_POINT('Ctrl Pts',(3.20149099940834,-0.691037008739266,
7.08376272980254)) ;
#75742 = CARTESIAN_POINT('Ctrl Pts',(3.19745445562265,-0.697229783074603,
7.08590527875505)) ;
#75743 = CARTESIAN_POINT('Ctrl Pts',(3.18736309615843,-0.708839952636616,
7.09112838260725)) ;
#75744 = CARTESIAN_POINT('Ctrl Pts',(3.17767539107277,-0.715977179240427,
7.09580721097557)) ;
#75745 = CARTESIAN_POINT('Ctrl Pts',(3.17121692101566,-0.720057683295033,
7.09882570651471)) ;
#75746 = CARTESIAN_POINT('Ctrl Pts',(3.20512388881546,-0.661999999999833,
7.0818)) ;
#75747 = CARTESIAN_POINT('Ctrl Pts',(3.20472023443689,-0.662977161851482,
7.0818)) ;
#75748 = CARTESIAN_POINT('Ctrl Pts',(3.20391292567976,-0.664831438935667,
7.0818281326209)) ;
#75749 = CARTESIAN_POINT('Ctrl Pts',(3.20270196254405,-0.667381960953569,
7.08193509059619)) ;
#75750 = CARTESIAN_POINT('Ctrl Pts',(3.20149099940834,-0.669755131272071,
7.08209149598161)) ;
#75751 = CARTESIAN_POINT('Ctrl Pts',(3.19745445562265,-0.677136096351082,
7.08275930201879)) ;
#75752 = CARTESIAN_POINT('Ctrl Pts',(3.18736309615843,-0.691331994006369,
7.08558723772615)) ;
#75753 = CARTESIAN_POINT('Ctrl Pts',(3.17767539107277,-0.700448400904743,
7.08930375506814)) ;
#75754 = CARTESIAN_POINT('Ctrl Pts',(3.17121692101566,-0.70568090461708,7.09184457452808)) ;
#75755 = CARTESIAN_POINT('',(3.17121692101566,-0.762,7.1818)) ;
#75756 = CARTESIAN_POINT('Ctrl Pts',(3.20512388881546,-0.661999999999834,
7.0818)) ;
#75757 = CARTESIAN_POINT('Ctrl Pts',(3.20472023443689,-0.662977161851484,
7.0818)) ;
#75758 = CARTESIAN_POINT('Ctrl Pts',(3.20431658005833,-0.6639042979399,7.08181418112561)) ;
#75759 = CARTESIAN_POINT('Ctrl Pts',(3.2035092713012,-0.665681610657573,7.08186384002979)) ;
#75760 = CARTESIAN_POINT('Ctrl Pts',(3.20310561692262,-0.666531791312273,
7.08189935834228)) ;
#75761 = CARTESIAN_POINT('Ctrl Pts',(3.20229830816548,-0.668173012083287,
7.08198732917139)) ;
#75762 = CARTESIAN_POINT('Ctrl Pts',(3.20189465378691,-0.66896403985732,7.0820398363167)) ;
#75763 = CARTESIAN_POINT('Ctrl Pts',(3.20108734502978,-0.670493217907201,
7.08215837537036)) ;
#75764 = CARTESIAN_POINT('Ctrl Pts',(3.20068369065121,-0.671231386902573,
7.08222438102225)) ;
#75765 = CARTESIAN_POINT('Ctrl Pts',(3.1984790488068,-0.67515936222752,7.08261718651246)) ;
#75766 = CARTESIAN_POINT('Ctrl Pts',(3.19667806134095,-0.677991390732913,
7.08305203429456)) ;
#75767 = CARTESIAN_POINT('Ctrl Pts',(3.19344882631238,-0.682614461197469,
7.08392572248013)) ;
#75768 = CARTESIAN_POINT('Ctrl Pts',(3.19202057874967,-0.684499933880204,
7.08434667817419)) ;
#75769 = CARTESIAN_POINT('Ctrl Pts',(3.18778558324308,-0.689801348801288,
7.08567402178887)) ;
#75770 = CARTESIAN_POINT('Ctrl Pts',(3.1849788352992,-0.692934482334868,7.0866568114692)) ;
#75771 = CARTESIAN_POINT('Ctrl Pts',(3.17911128623295,-0.698892281462462,
7.08879536039987)) ;
#75772 = CARTESIAN_POINT('Ctrl Pts',(3.17605048511059,-0.701664122709342,
7.08995925874846)) ;
#75773 = CARTESIAN_POINT('Ctrl Pts',(3.17239876299736,-0.704716249384931,
7.09138087098935)) ;
#75774 = CARTESIAN_POINT('Ctrl Pts',(3.17180784200651,-0.70520215403823,7.09161210096398)) ;
#75775 = CARTESIAN_POINT('Ctrl Pts',(3.17121692101566,-0.70568090461708,7.09184457452808)) ;
#75776 = CARTESIAN_POINT('Origin',(3.21546217517793,-0.861999999999999,0.)) ;
#75777 = CARTESIAN_POINT('',(3.21546217517793,-0.762,7.36730649953872)) ;
#75778 = CARTESIAN_POINT('',(3.21546217517793,-0.762,0.)) ;
#75779 = CARTESIAN_POINT('',(3.31205160669424,-0.887893661760288,7.36730649953872)) ;
#75780 = CARTESIAN_POINT('Origin',(3.21546217517793,-0.862,7.36730649953872)) ;
#75781 = CARTESIAN_POINT('',(3.31205160669424,-0.887893661760288,0.)) ;
#75782 = CARTESIAN_POINT('Origin',(-9.525,-0.762,8.72161438184689)) ;
#75783 = CARTESIAN_POINT('',(0.598228027472807,-0.762,7.1818)) ;
#75784 = CARTESIAN_POINT('',(0.,-0.762,7.1818)) ;
#75785 = CARTESIAN_POINT('',(0.731723284002018,-0.762,8.59150875795967)) ;
#75786 = CARTESIAN_POINT('',(0.703226309181215,-0.762,8.29058094955136)) ;
#75787 = CARTESIAN_POINT('',(3.07434158440252,-0.762,7.64111756647598)) ;
#75788 = CARTESIAN_POINT('Origin',(0.,-0.762,3.42553041237115)) ;
#75789 = CARTESIAN_POINT('Origin',(2.94523160007116,-0.762,7.40850915739415)) ;
#75790 = CARTESIAN_POINT('Ctrl Pts',(0.233145498782351,-1.13595304047784,
6.71957)) ;
#75791 = CARTESIAN_POINT('Ctrl Pts',(0.282596494255523,-1.15562586963554,
6.71957)) ;
#75792 = CARTESIAN_POINT('Ctrl Pts',(0.32845503035145,-1.17386952959435,6.7615916062195)) ;
#75793 = CARTESIAN_POINT('Ctrl Pts',(0.332764968591525,-1.17558412963154,
6.81085442572523)) ;
#75794 = CARTESIAN_POINT('Ctrl Pts',(0.233145498782351,-1.13595304047784,
6.71957)) ;
#75795 = CARTESIAN_POINT('Ctrl Pts',(0.283851238553257,-1.14931784407503,
6.71957)) ;
#75796 = CARTESIAN_POINT('Ctrl Pts',(0.328698029275161,-1.16142573132119,
6.76307285057327)) ;
#75797 = CARTESIAN_POINT('Ctrl Pts',(0.332784667850019,-1.16254657695484,
6.81107958928014)) ;
#75798 = CARTESIAN_POINT('Ctrl Pts',(0.233145498782351,-1.13595304047784,
6.71957)) ;
#75799 = CARTESIAN_POINT('Ctrl Pts',(0.28510598285099,-1.14300981851451,6.71957)) ;
#75800 = CARTESIAN_POINT('Ctrl Pts',(0.331172502747825,-1.14898571310985,
6.76307285057327)) ;
#75801 = CARTESIAN_POINT('Ctrl Pts',(0.335376993538143,-1.14951407564648,
6.81107958928014)) ;
#75802 = CARTESIAN_POINT('Ctrl Pts',(0.233145498782351,-1.13595304047784,
6.71957)) ;
#75803 = CARTESIAN_POINT('Ctrl Pts',(0.286360727148723,-1.136701792954,6.71957)) ;
#75804 = CARTESIAN_POINT('Ctrl Pts',(0.33571003645062,-1.13739615091638,6.7615916062195)) ;
#75805 = CARTESIAN_POINT('Ctrl Pts',(0.340348049204377,-1.13746140899458,
6.81085442572523)) ;
#75806 = CARTESIAN_POINT('',(0.332764968591525,-1.17558412963154,6.81085442572523)) ;
#75807 = CARTESIAN_POINT('',(0.340348049204377,-1.13746140899458,6.81085442572523)) ;
#75808 = CARTESIAN_POINT('Origin',(0.4323844384007,-1.17558412963154,6.80213885145047)) ;
#75809 = CARTESIAN_POINT('',(0.233145498782351,-1.13595304047784,6.71957)) ;
#75810 = CARTESIAN_POINT('Origin',(0.233145498782351,-1.13595304047784,6.81957)) ;
#75811 = CARTESIAN_POINT('Origin',(0.233145498782351,-1.13595304047784,6.81957)) ;
#75812 = CARTESIAN_POINT('Origin',(0.607374264964752,-1.21039177030075,8.80228172152873)) ;
#75813 = CARTESIAN_POINT('',(0.484912864018598,-1.20584822770277,8.54991282821175)) ;
#75814 = CARTESIAN_POINT('',(0.507754795155577,-1.21039177030075,8.81099729580349)) ;
#75815 = CARTESIAN_POINT('',(0.49249594463145,-1.16772550706581,8.54991282821175)) ;
#75816 = CARTESIAN_POINT('Origin',(0.584532333827773,-1.20584822770277,8.54119725393698)) ;
#75817 = CARTESIAN_POINT('',(0.515337875768429,-1.17226904966379,8.81099729580349)) ;
#75818 = CARTESIAN_POINT('Origin',(0.584532333827771,-1.20584822770278,8.54119725393698)) ;
#75819 = CARTESIAN_POINT('',(0.595585710062509,-1.22865054909962,8.63793337445424)) ;
#75820 = CARTESIAN_POINT('Origin',(0.584532333827771,-1.20584822770278,8.54119725393698)) ;
#75821 = CARTESIAN_POINT('Origin',(0.584532333827771,-1.20584822770278,8.54119725393698)) ;
#75822 = CARTESIAN_POINT('Origin',(0.135929041739323,-4.80294522256305E-16,
3.41363816217501)) ;
#75823 = CARTESIAN_POINT('',(0.459053285493802,-2.10247651427315,8.254336493146)) ;
#75824 = CARTESIAN_POINT('Origin',(0.0363095719301483,-1.2829700173246E-16,
3.42235373644978)) ;
#75825 = CARTESIAN_POINT('',(0.563402527094027,-2.29049913469776,8.27007790985519)) ;
#75826 = CARTESIAN_POINT('Ctrl Pts',(0.563402527094027,-2.29049913469776,
8.27007790985519)) ;
#75827 = CARTESIAN_POINT('Ctrl Pts',(0.563094639607243,-2.29005173251521,
8.27032524748595)) ;
#75828 = CARTESIAN_POINT('Ctrl Pts',(0.562783526294646,-2.28959637341817,
8.27056977508129)) ;
#75829 = CARTESIAN_POINT('Ctrl Pts',(0.518363588386159,-2.22542344757913,
8.30657277835385)) ;
#75830 = CARTESIAN_POINT('Ctrl Pts',(0.463831241820141,-2.12754376098305,
8.30894878385637)) ;
#75831 = CARTESIAN_POINT('Ctrl Pts',(0.459053285493802,-2.10247651427315,
8.254336493146)) ;
#75832 = CARTESIAN_POINT('Origin',(0.138499429641961,-4.89376784692015E-16,
3.41341328237267)) ;
#75833 = CARTESIAN_POINT('Origin',(0.507999999999992,2.45141482417775E-15,
8.8138)) ;
#75834 = CARTESIAN_POINT('',(0.33276496859165,-1.72771014821123,6.81085442572668)) ;
#75835 = CARTESIAN_POINT('',(0.332764968591529,9.47397622833151E-16,6.81085442572523)) ;
#75836 = CARTESIAN_POINT('',(0.456330681975393,-2.09161206695506,8.2232169925309)) ;
#75837 = CARTESIAN_POINT('Ctrl Pts',(0.456330681975393,-2.09161206695506,
8.2232169925309)) ;
#75838 = CARTESIAN_POINT('Ctrl Pts',(0.415134631297314,-1.97064606309627,
7.75234397861325)) ;
#75839 = CARTESIAN_POINT('Ctrl Pts',(0.373944470214011,-1.84941569039825,
7.28153828307192)) ;
#75840 = CARTESIAN_POINT('Ctrl Pts',(0.332764968591776,-1.72771014821123,
6.81085442572812)) ;
#75841 = CARTESIAN_POINT('Origin',(0.453427128991176,-2.23537208573896,8.19002923005734)) ;
#75842 = CARTESIAN_POINT('Origin',(0.233145498782355,1.299395143357E-15,6.81957)) ;
#75843 = CARTESIAN_POINT('',(0.233145498782349,-1.72771014821048,6.71957)) ;
#75844 = CARTESIAN_POINT('',(0.233145498782355,1.299395143357E-15,6.71957)) ;
#75845 = CARTESIAN_POINT('Origin',(0.233145498782349,-1.72771014821048,6.81957)) ;
#75846 = CARTESIAN_POINT('Ctrl Pts',(0.459053285493802,-2.10247651427315,
8.254336493146)) ;
#75847 = CARTESIAN_POINT('Ctrl Pts',(0.463831241820141,-2.12754376098305,
8.30894878385637)) ;
#75848 = CARTESIAN_POINT('Ctrl Pts',(0.518363588386159,-2.22542344757913,
8.30657277835385)) ;
#75849 = CARTESIAN_POINT('Ctrl Pts',(0.562783526294646,-2.28959637341817,
8.27056977508129)) ;
#75850 = CARTESIAN_POINT('Ctrl Pts',(0.563094639607243,-2.29005173251521,
8.27032524748595)) ;
#75851 = CARTESIAN_POINT('Ctrl Pts',(0.563402527094027,-2.29049913469776,
8.27007790985519)) ;
#75852 = CARTESIAN_POINT('Ctrl Pts',(0.458120821927424,-2.12650219752326,
8.24367838581188)) ;
#75853 = CARTESIAN_POINT('Ctrl Pts',(0.461688966624489,-2.14596370314819,
8.28635124743027)) ;
#75854 = CARTESIAN_POINT('Ctrl Pts',(0.509788465353625,-2.2323671087866,8.30425543138927)) ;
#75855 = CARTESIAN_POINT('Ctrl Pts',(0.562697273737575,-2.28970714738724,
8.27052649306718)) ;
#75856 = CARTESIAN_POINT('Ctrl Pts',(0.563047685007142,-2.29010501322995,
8.27030551703833)) ;
#75857 = CARTESIAN_POINT('Ctrl Pts',(0.563402527094027,-2.29049913469776,
8.27007790985519)) ;
#75858 = CARTESIAN_POINT('Ctrl Pts',(0.437455203934562,-2.16829359261983,
8.22680527958952)) ;
#75859 = CARTESIAN_POINT('Ctrl Pts',(0.440261201157157,-2.18279718179887,
8.25963785655292)) ;
#75860 = CARTESIAN_POINT('Ctrl Pts',(0.497044842085689,-2.24468622633794,
8.30004865938944)) ;
#75861 = CARTESIAN_POINT('Ctrl Pts',(0.562535491219473,-2.28990061909155,
8.27045236517641)) ;
#75862 = CARTESIAN_POINT('Ctrl Pts',(0.562965514456966,-2.29019825448075,
8.27027098875499)) ;
#75863 = CARTESIAN_POINT('Ctrl Pts',(0.563402527094027,-2.29049913469776,
8.27007790985519)) ;
#75864 = CARTESIAN_POINT('Ctrl Pts',(0.394198333198201,-2.18878000295551,
8.22143216354669)) ;
#75865 = CARTESIAN_POINT('Ctrl Pts',(0.398660306869003,-2.20910331550188,
8.2673898581129)) ;
#75866 = CARTESIAN_POINT('Ctrl Pts',(0.486848771498274,-2.25930922281487,
8.29418858273012)) ;
#75867 = CARTESIAN_POINT('Ctrl Pts',(0.562361505034938,-2.29008362295378,
8.27038779969869)) ;
#75868 = CARTESIAN_POINT('Ctrl Pts',(0.56288334390679,-2.29029149573155,8.27023646047164)) ;
#75869 = CARTESIAN_POINT('Ctrl Pts',(0.563402527094027,-2.29049913469776,
8.27007790985519)) ;
#75870 = CARTESIAN_POINT('Ctrl Pts',(0.374769931517255,-2.19218377594761,
8.22161041260296)) ;
#75871 = CARTESIAN_POINT('Ctrl Pts',(0.38020887226914,-2.21659247451535,8.27645980857715)) ;
#75872 = CARTESIAN_POINT('Ctrl Pts',(0.482581338415516,-2.266212758132,8.29146057868529)) ;
#75873 = CARTESIAN_POINT('Ctrl Pts',(0.562286478119671,-2.29015910661772,
8.27036146369334)) ;
#75874 = CARTESIAN_POINT('Ctrl Pts',(0.562848127956715,-2.2903314562676,8.27022166263593)) ;
#75875 = CARTESIAN_POINT('Ctrl Pts',(0.563402527094027,-2.29049913469776,
8.27007790985519)) ;
#75876 = CARTESIAN_POINT('',(0.374769931517255,-2.19218377594761,8.22161041260296)) ;
#75877 = CARTESIAN_POINT('Ctrl Pts',(0.374769931517255,-2.19218377594761,
8.22161041260296)) ;
#75878 = CARTESIAN_POINT('Ctrl Pts',(0.38020887226914,-2.21659247451535,8.27645980857715)) ;
#75879 = CARTESIAN_POINT('Ctrl Pts',(0.482581338415516,-2.266212758132,8.29146057868529)) ;
#75880 = CARTESIAN_POINT('Ctrl Pts',(0.562286478119671,-2.29015910661772,
8.27036146369334)) ;
#75881 = CARTESIAN_POINT('Ctrl Pts',(0.562848127956715,-2.2903314562676,8.27022166263593)) ;
#75882 = CARTESIAN_POINT('Ctrl Pts',(0.563402527094027,-2.29049913469776,
8.27007790985519)) ;
#75883 = CARTESIAN_POINT('Origin',(0.359433815684627,-2.10247651427315,8.26305206742076)) ;
#75884 = CARTESIAN_POINT('Ctrl Pts',(0.374769931517254,-2.19218377594761,
8.22161041260296)) ;
#75885 = CARTESIAN_POINT('Ctrl Pts',(0.374271909287347,-2.18994876824218,
8.21658807098568)) ;
#75886 = CARTESIAN_POINT('Ctrl Pts',(0.373662616506299,-2.18815607354194,
8.21137680913461)) ;
#75887 = CARTESIAN_POINT('Ctrl Pts',(0.37295000513728,-2.18682986267501,8.20605066229541)) ;
#75888 = CARTESIAN_POINT('Ctrl Pts',(0.400674467091849,-2.18764541195813,
8.2213727471946)) ;
#75889 = CARTESIAN_POINT('Ctrl Pts',(0.400168655131402,-2.18531329532944,
8.21609868976098)) ;
#75890 = CARTESIAN_POINT('Ctrl Pts',(0.399569847844621,-2.18345309008412,
8.21059040433855)) ;
#75891 = CARTESIAN_POINT('Ctrl Pts',(0.398892978130845,-2.18211755991818,
8.20499152409472)) ;
#75892 = CARTESIAN_POINT('Ctrl Pts',(0.442802799136141,-2.16260269917149,
8.22888130401443)) ;
#75893 = CARTESIAN_POINT('Ctrl Pts',(0.442204751807135,-2.15964157072195,
8.22218874465404)) ;
#75894 = CARTESIAN_POINT('Ctrl Pts',(0.441564708190408,-2.15729533880903,
8.21524061522765)) ;
#75895 = CARTESIAN_POINT('Ctrl Pts',(0.440889933449587,-2.15559078214374,
8.20813192407365)) ;
#75896 = CARTESIAN_POINT('Ctrl Pts',(0.458353937819018,-2.12049577671073,
8.2463429126454)) ;
#75897 = CARTESIAN_POINT('Ctrl Pts',(0.457563066882837,-2.11646373803811,
8.23730217497138)) ;
#75898 = CARTESIAN_POINT('Ctrl Pts',(0.456741824116299,-2.11321321015441,
8.22792080639222)) ;
#75899 = CARTESIAN_POINT('Ctrl Pts',(0.455903016748525,-2.11078568946555,
8.21832875661974)) ;
#75900 = CARTESIAN_POINT('Ctrl Pts',(0.459053285493801,-2.10247651427315,
8.25433649314599)) ;
#75901 = CARTESIAN_POINT('Ctrl Pts',(0.458174489582068,-2.09798645436108,
8.24429180991142)) ;
#75902 = CARTESIAN_POINT('Ctrl Pts',(0.4572626369128,-2.09434861239325,8.23386928620929)) ;
#75903 = CARTESIAN_POINT('Ctrl Pts',(0.456330681975393,-2.09161206695506,
8.2232169925309)) ;
#75904 = CARTESIAN_POINT('',(0.37295000513728,-2.18682986267501,8.20605066229541)) ;
#75905 = CARTESIAN_POINT('Origin',(0.356711212166218,-2.09161206695506,8.23193256680567)) ;
#75906 = CARTESIAN_POINT('Origin',(0.356848236200114,-2.26130448598471,8.18949965412146)) ;
#75907 = CARTESIAN_POINT('Ctrl Pts',(0.332575554792171,-1.7271503343366,6.80868941609177)) ;
#75908 = CARTESIAN_POINT('Ctrl Pts',(0.373881299532484,-1.84923054559942,
7.28081623887807)) ;
#75909 = CARTESIAN_POINT('Ctrl Pts',(0.415197776566303,-1.97083234352155,
7.75306573234047)) ;
#75910 = CARTESIAN_POINT('Ctrl Pts',(0.456520172012611,-2.09216847395032,
8.22538287356716)) ;
#75911 = CARTESIAN_POINT('Ctrl Pts',(0.331987953017615,-1.75332513240999,
6.80197267219288)) ;
#75912 = CARTESIAN_POINT('Ctrl Pts',(0.373292933712475,-1.87515504373648,
7.27418379019747)) ;
#75913 = CARTESIAN_POINT('Ctrl Pts',(0.414627967367415,-1.99656668249708,
7.74649382983075)) ;
#75914 = CARTESIAN_POINT('Ctrl Pts',(0.455949949949699,-2.11773252293444,
8.21886547566713)) ;
#75915 = CARTESIAN_POINT('Ctrl Pts',(0.310793595327402,-1.79883340137849,
6.79205963153165)) ;
#75916 = CARTESIAN_POINT('Ctrl Pts',(0.352528666728234,-1.92025230099924,
7.26437312176635)) ;
#75917 = CARTESIAN_POINT('Ctrl Pts',(0.394171753364285,-2.04132212887046,
7.73676749348942)) ;
#75918 = CARTESIAN_POINT('Ctrl Pts',(0.435777022314021,-2.16220666599519,
8.20920517618971)) ;
#75919 = CARTESIAN_POINT('Ctrl Pts',(0.265876600167924,-1.81991774820283,
6.79053747107829)) ;
#75920 = CARTESIAN_POINT('Ctrl Pts',(0.308308238839946,-1.94157711521186,
7.26274358539733)) ;
#75921 = CARTESIAN_POINT('Ctrl Pts',(0.350504776847073,-2.06283206919883,
7.73505295857787)) ;
#75922 = CARTESIAN_POINT('Ctrl Pts',(0.392580797820033,-2.18386034844095,
8.20742162540622)) ;
#75923 = CARTESIAN_POINT('Ctrl Pts',(0.245836003043331,-1.82288076242879,
6.79152463448741)) ;
#75924 = CARTESIAN_POINT('Ctrl Pts',(0.28849419488381,-1.94477897268376,7.26365133260709)) ;
#75925 = CARTESIAN_POINT('Ctrl Pts',(0.330878372341273,-2.06621032168341,
7.73590073192183)) ;
#75926 = CARTESIAN_POINT('Ctrl Pts',(0.373113112727488,-2.18739110458305,
8.20821779213733)) ;
#75927 = CARTESIAN_POINT('',(0.246063080839075,-1.82343508275148,6.79368809549119)) ;
#75928 = CARTESIAN_POINT('Origin',(0.233145498782601,-1.72771014821123,6.81957000000289)) ;
#75929 = CARTESIAN_POINT('Ctrl Pts',(0.246063080839076,-1.82343508275148,
6.79368809549264)) ;
#75930 = CARTESIAN_POINT('Ctrl Pts',(0.263106778000548,-1.87213905946258,
6.98232754964158)) ;
#75931 = CARTESIAN_POINT('Ctrl Pts',(0.280128754030394,-1.92076304376671,
7.17098657374969)) ;
#75932 = CARTESIAN_POINT('Ctrl Pts',(0.314082706993329,-2.0179348788448,7.54848217854548)) ;
#75933 = CARTESIAN_POINT('Ctrl Pts',(0.331014637616594,-2.06648276270083,
7.73731878400216)) ;
#75934 = CARTESIAN_POINT('Ctrl Pts',(0.356264911138867,-2.13894444267106,
8.01945926643602)) ;
#75935 = CARTESIAN_POINT('Ctrl Pts',(0.364607313003592,-2.16289285302724,
8.11275364297402)) ;
#75936 = CARTESIAN_POINT('Ctrl Pts',(0.372950005137279,-2.18682986267501,
8.20605066229541)) ;
#75937 = CARTESIAN_POINT('Origin',(0.233145498782349,-1.72771014821048,6.81957)) ;
#75938 = CARTESIAN_POINT('Origin',(0.233145498782349,-1.72771014821048,6.81957)) ;
#75939 = CARTESIAN_POINT('Origin',(-0.233145498782373,-1.72771014821048,6.81957)) ;
#75940 = CARTESIAN_POINT('',(-0.332764968591548,-1.72771014821048,6.81085442572523)) ;
#75941 = CARTESIAN_POINT('',(-0.246063080838839,-1.82343508275073,6.79368809548975)) ;
#75942 = CARTESIAN_POINT('Origin',(-0.233145498782373,-1.72771014821048,6.81957)) ;
#75943 = CARTESIAN_POINT('',(-0.233145498782373,-1.72771014821048,6.71957)) ;
#75944 = CARTESIAN_POINT('Origin',(-0.233145498782373,-1.72771014821048,6.81957)) ;
#75945 = CARTESIAN_POINT('Origin',(-0.233145498782373,-1.72771014821048,6.81957)) ;
#75946 = CARTESIAN_POINT('Ctrl Pts',(-0.245836001151034,-1.8228807580253,
6.79152461794378)) ;
#75947 = CARTESIAN_POINT('Ctrl Pts',(-0.288494198953793,-1.9447789779916,
7.26365132481474)) ;
#75948 = CARTESIAN_POINT('Ctrl Pts',(-0.330878369254937,-2.06621031878769,
7.73590073893123)) ;
#75949 = CARTESIAN_POINT('Ctrl Pts',(-0.373113113874326,-2.18739110879812,
8.20821780878249)) ;
#75950 = CARTESIAN_POINT('Ctrl Pts',(-0.272553537556922,-1.8189308194855,
6.79020849164427)) ;
#75951 = CARTESIAN_POINT('Ctrl Pts',(-0.314905492765294,-1.94050480823612,
7.26244303990738)) ;
#75952 = CARTESIAN_POINT('Ctrl Pts',(-0.357046431870861,-2.06171037042116,
7.7347692407966)) ;
#75953 = CARTESIAN_POINT('Ctrl Pts',(-0.399066819643649,-2.18268421515255,
8.20715633330629)) ;
#75954 = CARTESIAN_POINT('Ctrl Pts',(-0.316376716060902,-1.79267106091927,
6.79316458204583)) ;
#75955 = CARTESIAN_POINT('Ctrl Pts',(-0.357994391162648,-1.91413489045563,
7.26547214219855)) ;
#75956 = CARTESIAN_POINT('Ctrl Pts',(-0.399548971339301,-2.03523918647868,
7.73786227286182)) ;
#75957 = CARTESIAN_POINT('Ctrl Pts',(-0.44107705424413,-2.15615536078617,
8.21029605360252)) ;
#75958 = CARTESIAN_POINT('Ctrl Pts',(-0.332134835417109,-1.74678141058242,
6.80365184795983)) ;
#75959 = CARTESIAN_POINT('Ctrl Pts',(-0.373443640775722,-1.86867784543941,
7.27584050139373)) ;
#75960 = CARTESIAN_POINT('Ctrl Pts',(-0.414768073581027,-1.99013064875018,
7.74813767788189)) ;
#75961 = CARTESIAN_POINT('Ctrl Pts',(-0.456092517669814,-2.11134152617596,
8.22049483777629)) ;
#75962 = CARTESIAN_POINT('Ctrl Pts',(-0.332575553339162,-1.72715033004212,
6.80868939948353)) ;
#75963 = CARTESIAN_POINT('Ctrl Pts',(-0.373881299047604,-1.84923054417823,
7.28081623333557)) ;
#75964 = CARTESIAN_POINT('Ctrl Pts',(-0.415197777050109,-1.97083234494871,
7.75306573787008)) ;
#75965 = CARTESIAN_POINT('Ctrl Pts',(-0.456520173465327,-2.09216847821589,
8.22538289017144)) ;
#75966 = CARTESIAN_POINT('',(-0.456330681975422,-2.09161206695506,8.2232169925309)) ;
#75967 = CARTESIAN_POINT('',(-0.37295000513731,-2.186829862675,8.20605066229541)) ;
#75968 = CARTESIAN_POINT('Origin',(-0.356711212166247,-2.09161206695506,8.23193256680567)) ;
#75969 = CARTESIAN_POINT('Ctrl Pts',(-0.37295000513731,-2.186829862675,8.20605066229541)) ;
#75970 = CARTESIAN_POINT('Ctrl Pts',(-0.356060675112372,-2.13837067836461,
8.01717588130003)) ;
#75971 = CARTESIAN_POINT('Ctrl Pts',(-0.33916937336606,-2.08986565451448,
7.82831193143985)) ;
#75972 = CARTESIAN_POINT('Ctrl Pts',(-0.305304200525196,-1.99279235652918,
7.45075381522733)) ;
#75973 = CARTESIAN_POINT('Ctrl Pts',(-0.288330373027804,-1.94422406244455,
7.26205962744251)) ;
#75974 = CARTESIAN_POINT('Ctrl Pts',(-0.262904814260684,-1.87155513860969,
6.98014705352749)) ;
#75975 = CARTESIAN_POINT('Ctrl Pts',(-0.254486208871171,-1.84750496780177,
6.88691518461202)) ;
#75976 = CARTESIAN_POINT('Ctrl Pts',(-0.246063080838839,-1.82343508275073,
6.79368809548975)) ;
#75977 = CARTESIAN_POINT('Ctrl Pts',(-0.332764968590868,-1.72771014820847,
6.81085442571747)) ;
#75978 = CARTESIAN_POINT('Ctrl Pts',(-0.373944470213416,-1.84941569039642,
7.28153828306482)) ;
#75979 = CARTESIAN_POINT('Ctrl Pts',(-0.41513463129703,-1.97064606309535,
7.75234397860969)) ;
#75980 = CARTESIAN_POINT('Ctrl Pts',(-0.456330681975422,-2.09161206695506,
8.2232169925309)) ;
#75981 = CARTESIAN_POINT('Ctrl Pts',(-0.37295000513731,-2.186829862675,8.20605066229541)) ;
#75982 = CARTESIAN_POINT('Ctrl Pts',(-0.373662616506329,-2.18815607354194,
8.21137680913461)) ;
#75983 = CARTESIAN_POINT('Ctrl Pts',(-0.374271909287377,-2.18994876824218,
8.21658807098568)) ;
#75984 = CARTESIAN_POINT('Ctrl Pts',(-0.374769931517285,-2.19218377594761,
8.22161041260296)) ;
#75985 = CARTESIAN_POINT('Ctrl Pts',(-0.398892978130875,-2.18211755991818,
8.20499152409472)) ;
#75986 = CARTESIAN_POINT('Ctrl Pts',(-0.399569847844652,-2.18345309008412,
8.21059040433855)) ;
#75987 = CARTESIAN_POINT('Ctrl Pts',(-0.400168655131432,-2.18531329532943,
8.21609868976098)) ;
#75988 = CARTESIAN_POINT('Ctrl Pts',(-0.400674467091879,-2.18764541195813,
8.2213727471946)) ;
#75989 = CARTESIAN_POINT('Ctrl Pts',(-0.440889933449617,-2.15559078214374,
8.20813192407365)) ;
#75990 = CARTESIAN_POINT('Ctrl Pts',(-0.441564708190438,-2.15729533880902,
8.21524061522766)) ;
#75991 = CARTESIAN_POINT('Ctrl Pts',(-0.442204751807165,-2.15964157072194,
8.22218874465405)) ;
#75992 = CARTESIAN_POINT('Ctrl Pts',(-0.442802799136171,-2.16260269917149,
8.22888130401443)) ;
#75993 = CARTESIAN_POINT('Ctrl Pts',(-0.455903016748555,-2.11078568946554,
8.21832875661974)) ;
#75994 = CARTESIAN_POINT('Ctrl Pts',(-0.456741824116329,-2.11321321015441,
8.22792080639222)) ;
#75995 = CARTESIAN_POINT('Ctrl Pts',(-0.457563066882866,-2.11646373803811,
8.23730217497138)) ;
#75996 = CARTESIAN_POINT('Ctrl Pts',(-0.458353937819047,-2.12049577671073,
8.24634291264541)) ;
#75997 = CARTESIAN_POINT('Ctrl Pts',(-0.456330681975422,-2.09161206695506,
8.2232169925309)) ;
#75998 = CARTESIAN_POINT('Ctrl Pts',(-0.45726263691283,-2.09434861239325,
8.23386928620929)) ;
#75999 = CARTESIAN_POINT('Ctrl Pts',(-0.458174489582097,-2.09798645436108,
8.24429180991143)) ;
#76000 = CARTESIAN_POINT('Ctrl Pts',(-0.459053285493831,-2.10247651427315,
8.254336493146)) ;
#76001 = CARTESIAN_POINT('',(-0.459053285493831,-2.10247651427315,8.254336493146)) ;
#76002 = CARTESIAN_POINT('',(-0.374769931517285,-2.19218377594761,8.22161041260296)) ;
#76003 = CARTESIAN_POINT('Origin',(-0.359433815684656,-2.10247651427315,8.26305206742076)) ;
#76004 = CARTESIAN_POINT('Origin',(-0.356848236064802,-2.26130448655063,8.18949965392306)) ;
#76005 = CARTESIAN_POINT('Origin',(-0.453427128997611,-2.2353720855235,8.19002923013049)) ;
#76006 = CARTESIAN_POINT('Ctrl Pts',(-0.374769931517285,-2.19218377594761,
8.22161041260296)) ;
#76007 = CARTESIAN_POINT('Ctrl Pts',(-0.380213170855601,-2.21661176556948,
8.27650315798654)) ;
#76008 = CARTESIAN_POINT('Ctrl Pts',(-0.482714730389439,-2.26627787671364,
8.29148068543043)) ;
#76009 = CARTESIAN_POINT('Ctrl Pts',(-0.562407667359032,-2.29019609072325,
8.27033080756506)) ;
#76010 = CARTESIAN_POINT('Ctrl Pts',(-0.56290832709327,-2.29034966353957,
8.27020605331712)) ;
#76011 = CARTESIAN_POINT('Ctrl Pts',(-0.563402527094058,-2.29049913469776,
8.27007790985519)) ;
#76012 = CARTESIAN_POINT('Ctrl Pts',(-0.40067446709188,-2.18764541195813,
8.2213727471946)) ;
#76013 = CARTESIAN_POINT('Ctrl Pts',(-0.404799111719599,-2.2065637149284,
8.26428096643201)) ;
#76014 = CARTESIAN_POINT('Ctrl Pts',(-0.488360100298001,-2.25706718969874,
8.29516164779624)) ;
#76015 = CARTESIAN_POINT('Ctrl Pts',(-0.562496982169543,-2.29010647931439,
8.2703619964159)) ;
#76016 = CARTESIAN_POINT('Ctrl Pts',(-0.56295018315296,-2.29030216828318,
8.27022364134446)) ;
#76017 = CARTESIAN_POINT('Ctrl Pts',(-0.563402527094058,-2.29049913469776,
8.27007790985519)) ;
#76018 = CARTESIAN_POINT('Ctrl Pts',(-0.442802313774365,-2.16260237888701,
8.22888148964801)) ;
#76019 = CARTESIAN_POINT('Ctrl Pts',(-0.445542573614775,-2.17718689461036,
8.26171487422345)) ;
#76020 = CARTESIAN_POINT('Ctrl Pts',(-0.498696522006183,-2.24300782595838,
8.3007470146104)) ;
#76021 = CARTESIAN_POINT('Ctrl Pts',(-0.562651405462978,-2.28994112152854,
8.2704209692529)) ;
#76022 = CARTESIAN_POINT('Ctrl Pts',(-0.563023431257417,-2.29021905158449,
8.27025442039232)) ;
#76023 = CARTESIAN_POINT('Ctrl Pts',(-0.563402527094058,-2.29049913469776,
8.27007790985519)) ;
#76024 = CARTESIAN_POINT('Ctrl Pts',(-0.458353937819048,-2.12049577671072,
8.24634291264541)) ;
#76025 = CARTESIAN_POINT('Ctrl Pts',(-0.462239142304945,-2.1414184975613,
8.2921265128678)) ;
#76026 = CARTESIAN_POINT('Ctrl Pts',(-0.512038168824972,-2.2307677807854,
8.30482405986502)) ;
#76027 = CARTESIAN_POINT('Ctrl Pts',(-0.562792975700759,-2.28976846564434,
8.27048768141226)) ;
#76028 = CARTESIAN_POINT('Ctrl Pts',(-0.563096679361875,-2.29013593488581,
8.27028519944017)) ;
#76029 = CARTESIAN_POINT('Ctrl Pts',(-0.563402527094058,-2.29049913469776,
8.27007790985519)) ;
#76030 = CARTESIAN_POINT('Ctrl Pts',(-0.459053285493832,-2.10247651427314,
8.254336493146)) ;
#76031 = CARTESIAN_POINT('Ctrl Pts',(-0.463835018007331,-2.12756357251097,
8.30899194587312)) ;
#76032 = CARTESIAN_POINT('Ctrl Pts',(-0.518436488407001,-2.22555128588009,
8.30657023215015)) ;
#76033 = CARTESIAN_POINT('Ctrl Pts',(-0.562850741456301,-2.28969445189011,
8.27051650453023)) ;
#76034 = CARTESIAN_POINT('Ctrl Pts',(-0.563128071406643,-2.29010031344351,
8.27029839046068)) ;
#76035 = CARTESIAN_POINT('Ctrl Pts',(-0.563402527094058,-2.29049913469776,
8.27007790985519)) ;
#76036 = CARTESIAN_POINT('',(-0.563402527094058,-2.29049913469776,8.27007790985519)) ;
#76037 = CARTESIAN_POINT('Ctrl Pts',(-0.459053285493832,-2.10247651427314,
8.254336493146)) ;
#76038 = CARTESIAN_POINT('Ctrl Pts',(-0.463835018007331,-2.12756357251097,
8.30899194587312)) ;
#76039 = CARTESIAN_POINT('Ctrl Pts',(-0.518436488407001,-2.22555128588009,
8.30657023215015)) ;
#76040 = CARTESIAN_POINT('Ctrl Pts',(-0.562850741456301,-2.28969445189011,
8.27051650453023)) ;
#76041 = CARTESIAN_POINT('Ctrl Pts',(-0.563128071406643,-2.29010031344351,
8.27029839046068)) ;
#76042 = CARTESIAN_POINT('Ctrl Pts',(-0.563402527094058,-2.29049913469776,
8.27007790985519)) ;
#76043 = CARTESIAN_POINT('Ctrl Pts',(-0.563402527094058,-2.29049913469776,
8.27007790985519)) ;
#76044 = CARTESIAN_POINT('Ctrl Pts',(-0.56290832709327,-2.29034966353957,
8.27020605331712)) ;
#76045 = CARTESIAN_POINT('Ctrl Pts',(-0.562407667359032,-2.29019609072325,
8.27033080756506)) ;
#76046 = CARTESIAN_POINT('Ctrl Pts',(-0.482714730389439,-2.26627787671364,
8.29148068543043)) ;
#76047 = CARTESIAN_POINT('Ctrl Pts',(-0.380213170855601,-2.21661176556948,
8.27650315798654)) ;
#76048 = CARTESIAN_POINT('Ctrl Pts',(-0.374769931517285,-2.19218377594761,
8.22161041260296)) ;
#76049 = CARTESIAN_POINT('Origin',(-0.135929041739328,8.98859866704575E-16,
3.41363816217501)) ;
#76050 = CARTESIAN_POINT('',(-0.484912864018618,-1.20584822770276,8.54991282821175)) ;
#76051 = CARTESIAN_POINT('Origin',(-0.0363095719301537,2.4010481180193E-16,
3.42235373644978)) ;
#76052 = CARTESIAN_POINT('',(-0.59558571006253,-1.2286505490996,8.63793337445424)) ;
#76053 = CARTESIAN_POINT('Origin',(-0.584532333827793,-1.20584822770276,8.54119725393699)) ;
#76054 = CARTESIAN_POINT('Origin',(-0.138499429641967,9.15857106573119E-16,
3.41341328237267)) ;
#76055 = CARTESIAN_POINT('Origin',(-0.508,1.1852043994395E-14,8.8138)) ;
#76056 = CARTESIAN_POINT('',(-0.332764968591544,-1.17558412963153,6.81085442572523)) ;
#76057 = CARTESIAN_POINT('',(-0.332764968591536,6.44687220156331E-15,6.81085442572523)) ;
#76058 = CARTESIAN_POINT('',(-0.507754795155597,-1.21039177030074,8.81099729580349)) ;
#76059 = CARTESIAN_POINT('Origin',(-0.233145498782362,5.78811714666067E-15,
6.81957)) ;
#76060 = CARTESIAN_POINT('',(-0.233145498782369,-1.13595304047784,6.71957)) ;
#76061 = CARTESIAN_POINT('',(-0.233145498782362,5.78811714666067E-15,6.71957)) ;
#76062 = CARTESIAN_POINT('Origin',(-0.233145498782369,-1.13595304047784,6.81957)) ;
#76063 = CARTESIAN_POINT('Ctrl Pts',(-0.233145498782369,-1.13595304047784,
6.71957)) ;
#76064 = CARTESIAN_POINT('Ctrl Pts',(-0.286360727148742,-1.13670179295399,
6.71957)) ;
#76065 = CARTESIAN_POINT('Ctrl Pts',(-0.335710036450638,-1.13739615091637,
6.7615916062195)) ;
#76066 = CARTESIAN_POINT('Ctrl Pts',(-0.340348049204396,-1.13746140899457,
6.81085442572523)) ;
#76067 = CARTESIAN_POINT('Ctrl Pts',(-0.233145498782369,-1.13595304047784,
6.71957)) ;
#76068 = CARTESIAN_POINT('Ctrl Pts',(-0.285105982851009,-1.14300981851451,
6.71957)) ;
#76069 = CARTESIAN_POINT('Ctrl Pts',(-0.331172502747844,-1.14898571310984,
6.76307285057327)) ;
#76070 = CARTESIAN_POINT('Ctrl Pts',(-0.335376993538162,-1.14951407564647,
6.81107958928014)) ;
#76071 = CARTESIAN_POINT('Ctrl Pts',(-0.233145498782369,-1.13595304047784,
6.71957)) ;
#76072 = CARTESIAN_POINT('Ctrl Pts',(-0.283851238553276,-1.14931784407502,
6.71957)) ;
#76073 = CARTESIAN_POINT('Ctrl Pts',(-0.328698029275179,-1.16142573132118,
6.76307285057327)) ;
#76074 = CARTESIAN_POINT('Ctrl Pts',(-0.332784667850038,-1.16254657695483,
6.81107958928014)) ;
#76075 = CARTESIAN_POINT('Ctrl Pts',(-0.233145498782369,-1.13595304047784,
6.71957)) ;
#76076 = CARTESIAN_POINT('Ctrl Pts',(-0.282596494255542,-1.15562586963553,
6.71957)) ;
#76077 = CARTESIAN_POINT('Ctrl Pts',(-0.328455030351469,-1.17386952959435,
6.7615916062195)) ;
#76078 = CARTESIAN_POINT('Ctrl Pts',(-0.332764968591544,-1.17558412963153,
6.81085442572523)) ;
#76079 = CARTESIAN_POINT('',(-0.340348049204396,-1.13746140899457,6.81085442572523)) ;
#76080 = CARTESIAN_POINT('Origin',(-0.432384438400719,-1.17558412963153,6.80213885145047)) ;
#76081 = CARTESIAN_POINT('Origin',(-0.23314549878237,-1.13595304047784,6.81957)) ;
#76082 = CARTESIAN_POINT('Origin',(-0.607374264964772,-1.21039177030074,8.80228172152873)) ;
#76083 = CARTESIAN_POINT('',(-0.49249594463147,-1.1677255070658,8.54991282821175)) ;
#76084 = CARTESIAN_POINT('',(-0.515337875768449,-1.17226904966378,8.81099729580349)) ;
#76085 = CARTESIAN_POINT('Origin',(-0.584532333827793,-1.20584822770276,8.54119725393698)) ;
#76086 = CARTESIAN_POINT('Origin',(-0.584532333827793,-1.20584822770276,8.54119725393699)) ;
#76087 = CARTESIAN_POINT('Origin',(-0.584532333827793,-1.20584822770276,8.54119725393699)) ;
#76088 = CARTESIAN_POINT('Origin',(-0.854554628096497,-0.353968116746241,
8.8138)) ;
#76089 = CARTESIAN_POINT('',(-0.558026198990151,-0.611939867549493,6.81085442572523)) ;
#76090 = CARTESIAN_POINT('',(-0.692658569199243,-0.286908573456252,6.81085442572523)) ;
#76091 = CARTESIAN_POINT('',(-0.570056476111077,-0.623970147580643,6.99051559579716)) ;
#76092 = CARTESIAN_POINT('',(-0.691124600663692,-0.74503826922303,8.7985570068643)) ;
#76093 = CARTESIAN_POINT('',(-0.506191638276494,-0.823877279363036,7.19051557427477)) ;
#76094 = CARTESIAN_POINT('Origin',(-0.589034350751109,-0.623877279363036,
7.19051557427477)) ;
#76095 = CARTESIAN_POINT('',(-0.639686894805704,-0.823877279363037,8.60022433223444)) ;
#76096 = CARTESIAN_POINT('',(-0.695846489640238,-0.823877279363037,9.19326916948217)) ;
#76097 = CARTESIAN_POINT('Origin',(-0.415843288169372,-0.172247929781569,
3.38615128096072)) ;
#76098 = CARTESIAN_POINT('Origin',(-0.60062218000292,-0.248785852819288,6.81957)) ;
#76099 = CARTESIAN_POINT('',(-0.497571705638611,-0.497571705638596,6.71957)) ;
#76100 = CARTESIAN_POINT('',(-0.60062218000292,-0.248785852819288,6.71957)) ;
#76101 = CARTESIAN_POINT('Origin',(-0.497571705638611,-0.497571705638596,
6.81957)) ;
#76102 = CARTESIAN_POINT('Origin',(-0.233145498782337,1.72771014821048,6.81957)) ;
#76103 = CARTESIAN_POINT('',(-0.246063080838801,1.82343508275074,6.79368809548975)) ;
#76104 = CARTESIAN_POINT('',(-0.332764968591511,1.72771014821048,6.81085442572523)) ;
#76105 = CARTESIAN_POINT('Origin',(-0.233145498782337,1.72771014821048,6.81957)) ;
#76106 = CARTESIAN_POINT('',(-0.233145498782337,1.72771014821048,6.71957)) ;
#76107 = CARTESIAN_POINT('Origin',(-0.233145498782337,1.72771014821048,6.81957)) ;
#76108 = CARTESIAN_POINT('Origin',(-0.233145498782337,1.72771014821048,6.81957)) ;
#76109 = CARTESIAN_POINT('Ctrl Pts',(-0.332575554791901,1.72715033433584,
6.80868941608882)) ;
#76110 = CARTESIAN_POINT('Ctrl Pts',(-0.373881299532302,1.84923054559893,
7.28081623887613)) ;
#76111 = CARTESIAN_POINT('Ctrl Pts',(-0.415197776566207,1.97083234352132,
7.75306573233952)) ;
#76112 = CARTESIAN_POINT('Ctrl Pts',(-0.456520172012602,2.09216847395034,
8.22538287356722)) ;
#76113 = CARTESIAN_POINT('Ctrl Pts',(-0.331987953017345,1.75332513240923,
6.80197267218993)) ;
#76114 = CARTESIAN_POINT('Ctrl Pts',(-0.373292933712292,1.87515504373599,
7.27418379019553)) ;
#76115 = CARTESIAN_POINT('Ctrl Pts',(-0.414627967367319,1.99656668249683,
7.74649382982981)) ;
#76116 = CARTESIAN_POINT('Ctrl Pts',(-0.455949949949689,2.11773252293446,
8.21886547566719)) ;
#76117 = CARTESIAN_POINT('Ctrl Pts',(-0.310793595327128,1.79883340137775,
6.7920596315287)) ;
#76118 = CARTESIAN_POINT('Ctrl Pts',(-0.352528666728049,1.92025230099876,
7.26437312176441)) ;
#76119 = CARTESIAN_POINT('Ctrl Pts',(-0.394171753364188,2.04132212887022,
7.73676749348846)) ;
#76120 = CARTESIAN_POINT('Ctrl Pts',(-0.435777022314011,2.16220666599522,
8.20920517618977)) ;
#76121 = CARTESIAN_POINT('Ctrl Pts',(-0.265876600167646,1.81991774820208,
6.79053747107535)) ;
#76122 = CARTESIAN_POINT('Ctrl Pts',(-0.308308238839758,1.94157711521136,
7.26274358539539)) ;
#76123 = CARTESIAN_POINT('Ctrl Pts',(-0.350504776846974,2.0628320691986,7.73505295857692)) ;
#76124 = CARTESIAN_POINT('Ctrl Pts',(-0.392580797820023,2.18386034844097,
8.20742162540629)) ;
#76125 = CARTESIAN_POINT('Ctrl Pts',(-0.245836003043051,1.82288076242804,
6.79152463448446)) ;
#76126 = CARTESIAN_POINT('Ctrl Pts',(-0.288494194883621,1.94477897268327,
7.26365133260514)) ;
#76127 = CARTESIAN_POINT('Ctrl Pts',(-0.330878372341174,2.06621032168316,
7.73590073192088)) ;
#76128 = CARTESIAN_POINT('Ctrl Pts',(-0.373113112727478,2.18739110458306,
8.20821779213739)) ;
#76129 = CARTESIAN_POINT('',(-0.372950005137265,2.18682986267501,8.20605066229541)) ;
#76130 = CARTESIAN_POINT('',(-0.456330681975378,2.09161206695507,8.2232169925309)) ;
#76131 = CARTESIAN_POINT('Origin',(-0.356711212166204,2.09161206695507,8.23193256680567)) ;
#76132 = CARTESIAN_POINT('Ctrl Pts',(-0.456330681975378,2.09161206695507,
8.2232169925309)) ;
#76133 = CARTESIAN_POINT('Ctrl Pts',(-0.415134631297216,1.97064606309603,
7.75234397861228)) ;
#76134 = CARTESIAN_POINT('Ctrl Pts',(-0.37394447021383,1.84941569039776,7.28153828307)) ;
#76135 = CARTESIAN_POINT('Ctrl Pts',(-0.332764968591511,1.72771014821048,
6.81085442572523)) ;
#76136 = CARTESIAN_POINT('Ctrl Pts',(-0.246063080838802,1.82343508275074,
6.79368809548975)) ;
#76137 = CARTESIAN_POINT('Ctrl Pts',(-0.263106778000196,1.87213905946162,
6.98232754963782)) ;
#76138 = CARTESIAN_POINT('Ctrl Pts',(-0.280128754029967,1.92076304376552,
7.17098657374507)) ;
#76139 = CARTESIAN_POINT('Ctrl Pts',(-0.314082706992799,2.01793487884333,
7.54848217853971)) ;
#76140 = CARTESIAN_POINT('Ctrl Pts',(-0.331014637616039,2.06648276269927,
7.7373187839961)) ;
#76141 = CARTESIAN_POINT('Ctrl Pts',(-0.356264911138476,2.13894444266998,
8.01945926643178)) ;
#76142 = CARTESIAN_POINT('Ctrl Pts',(-0.36460731300339,2.1628928530267,8.1127536429719)) ;
#76143 = CARTESIAN_POINT('Ctrl Pts',(-0.372950005137265,2.18682986267501,
8.20605066229541)) ;
#76144 = CARTESIAN_POINT('Ctrl Pts',(-0.37476993151724,2.19218377594762,8.22161041260296)) ;
#76145 = CARTESIAN_POINT('Ctrl Pts',(-0.374271909287332,2.18994876824219,
8.21658807098568)) ;
#76146 = CARTESIAN_POINT('Ctrl Pts',(-0.373662616506283,2.18815607354195,
8.21137680913461)) ;
#76147 = CARTESIAN_POINT('Ctrl Pts',(-0.372950005137264,2.18682986267501,
8.20605066229541)) ;
#76148 = CARTESIAN_POINT('Ctrl Pts',(-0.400674467091834,2.18764541195814,
8.2213727471946)) ;
#76149 = CARTESIAN_POINT('Ctrl Pts',(-0.400168655131387,2.18531329532944,
8.21609868976098)) ;
#76150 = CARTESIAN_POINT('Ctrl Pts',(-0.399569847844606,2.18345309008413,
8.21059040433855)) ;
#76151 = CARTESIAN_POINT('Ctrl Pts',(-0.39889297813083,2.18211755991819,8.20499152409472)) ;
#76152 = CARTESIAN_POINT('Ctrl Pts',(-0.442802799136127,2.1626026991715,8.22888130401443)) ;
#76153 = CARTESIAN_POINT('Ctrl Pts',(-0.44220475180712,2.15964157072196,8.22218874465405)) ;
#76154 = CARTESIAN_POINT('Ctrl Pts',(-0.441564708190393,2.15729533880903,
8.21524061522765)) ;
#76155 = CARTESIAN_POINT('Ctrl Pts',(-0.440889933449573,2.15559078214375,
8.20813192407365)) ;
#76156 = CARTESIAN_POINT('Ctrl Pts',(-0.458353937819003,2.12049577671074,
8.24634291264541)) ;
#76157 = CARTESIAN_POINT('Ctrl Pts',(-0.457563066882822,2.11646373803812,
8.23730217497138)) ;
#76158 = CARTESIAN_POINT('Ctrl Pts',(-0.456741824116285,2.11321321015442,
8.22792080639222)) ;
#76159 = CARTESIAN_POINT('Ctrl Pts',(-0.455903016748511,2.11078568946555,
8.21832875661974)) ;
#76160 = CARTESIAN_POINT('Ctrl Pts',(-0.459053285493787,2.10247651427316,
8.254336493146)) ;
#76161 = CARTESIAN_POINT('Ctrl Pts',(-0.458174489582053,2.09798645436109,
8.24429180991143)) ;
#76162 = CARTESIAN_POINT('Ctrl Pts',(-0.457262636912786,2.09434861239326,
8.23386928620929)) ;
#76163 = CARTESIAN_POINT('Ctrl Pts',(-0.456330681975378,2.09161206695507,
8.2232169925309)) ;
#76164 = CARTESIAN_POINT('',(-0.37476993151724,2.19218377594762,8.22161041260296)) ;
#76165 = CARTESIAN_POINT('Origin',(-0.356848236134331,2.26130448626201,8.18949965402755)) ;
#76166 = CARTESIAN_POINT('',(-0.459053285493787,2.10247651427316,8.254336493146)) ;
#76167 = CARTESIAN_POINT('Origin',(-0.359433815684613,2.10247651427315,8.26305206742076)) ;
#76168 = CARTESIAN_POINT('Origin',(-0.453427128997903,2.23537208552098,8.19002923013433)) ;
#76169 = CARTESIAN_POINT('Ctrl Pts',(-0.459053285493787,2.10247651427316,
8.254336493146)) ;
#76170 = CARTESIAN_POINT('Ctrl Pts',(-0.463831274313048,2.12754393145512,
8.30894915525216)) ;
#76171 = CARTESIAN_POINT('Ctrl Pts',(-0.518364204358841,2.22542453008761,
8.30657276282558)) ;
#76172 = CARTESIAN_POINT('Ctrl Pts',(-0.562784097682946,2.28959720721989,
8.27056932236647)) ;
#76173 = CARTESIAN_POINT('Ctrl Pts',(-0.563094923804728,2.29005214549267,
8.27032501917936)) ;
#76174 = CARTESIAN_POINT('Ctrl Pts',(-0.563402527094011,2.29049913469777,
8.27007790985519)) ;
#76175 = CARTESIAN_POINT('Ctrl Pts',(-0.458120821927409,2.12650219752326,
8.24367838581188)) ;
#76176 = CARTESIAN_POINT('Ctrl Pts',(-0.461688990889963,2.14596383549791,
8.2863515376309)) ;
#76177 = CARTESIAN_POINT('Ctrl Pts',(-0.509789157873014,2.23236813286337,
8.30425558488427)) ;
#76178 = CARTESIAN_POINT('Ctrl Pts',(-0.562697924855537,2.28970787909533,
8.27052608050501)) ;
#76179 = CARTESIAN_POINT('Ctrl Pts',(-0.563048012546372,2.29010537702631,
8.27030530694405)) ;
#76180 = CARTESIAN_POINT('Ctrl Pts',(-0.563402527094011,2.29049913469777,
8.27007790985519)) ;
#76181 = CARTESIAN_POINT('Ctrl Pts',(-0.437455203934548,2.16829359261983,
8.22680527958952)) ;
#76182 = CARTESIAN_POINT('Ctrl Pts',(-0.440261220239578,2.18279728043183,
8.2596380798338)) ;
#76183 = CARTESIAN_POINT('Ctrl Pts',(-0.497045700566893,2.24468709263695,
8.30004898389791)) ;
#76184 = CARTESIAN_POINT('Ctrl Pts',(-0.562536291712692,2.28990117236503,
8.27045202116462)) ;
#76185 = CARTESIAN_POINT('Ctrl Pts',(-0.562965917844249,2.29019853221018,
8.27027081053226)) ;
#76186 = CARTESIAN_POINT('Ctrl Pts',(-0.563402527094011,2.29049913469777,
8.27007790985519)) ;
#76187 = CARTESIAN_POINT('Ctrl Pts',(-0.394198333198186,2.18878000295551,
8.22143216354669)) ;
#76188 = CARTESIAN_POINT('Ctrl Pts',(-0.398660337213041,2.2091034537124,8.26739017065233)) ;
#76189 = CARTESIAN_POINT('Ctrl Pts',(-0.486849819185561,2.25930987312264,
8.29418883400901)) ;
#76190 = CARTESIAN_POINT('Ctrl Pts',(-0.562362466050226,2.2900840072024,8.27038751506786)) ;
#76191 = CARTESIAN_POINT('Ctrl Pts',(-0.562883823142126,2.29029168739404,
8.27023631412047)) ;
#76192 = CARTESIAN_POINT('Ctrl Pts',(-0.563402527094011,2.29049913469777,
8.27007790985519)) ;
#76193 = CARTESIAN_POINT('Ctrl Pts',(-0.37476993151724,2.19218377594762,8.22161041260296)) ;
#76194 = CARTESIAN_POINT('Ctrl Pts',(-0.38020890925713,2.2165926405089,8.27646018158539)) ;
#76195 = CARTESIAN_POINT('Ctrl Pts',(-0.482582465715569,2.26621331095889,
8.29146075442296)) ;
#76196 = CARTESIAN_POINT('Ctrl Pts',(-0.562287508336611,2.29015942107408,
8.27036120321575)) ;
#76197 = CARTESIAN_POINT('Ctrl Pts',(-0.562848639698359,2.29033161104427,
8.27022152994399)) ;
#76198 = CARTESIAN_POINT('Ctrl Pts',(-0.563402527094011,2.29049913469777,
8.27007790985519)) ;
#76199 = CARTESIAN_POINT('',(-0.563402527094011,2.29049913469777,8.27007790985519)) ;
#76200 = CARTESIAN_POINT('Ctrl Pts',(-0.37476993151724,2.19218377594762,8.22161041260296)) ;
#76201 = CARTESIAN_POINT('Ctrl Pts',(-0.38020890925713,2.2165926405089,8.27646018158539)) ;
#76202 = CARTESIAN_POINT('Ctrl Pts',(-0.482582465715569,2.26621331095889,
8.29146075442296)) ;
#76203 = CARTESIAN_POINT('Ctrl Pts',(-0.562287508336611,2.29015942107408,
8.27036120321575)) ;
#76204 = CARTESIAN_POINT('Ctrl Pts',(-0.562848639698359,2.29033161104427,
8.27022152994399)) ;
#76205 = CARTESIAN_POINT('Ctrl Pts',(-0.563402527094011,2.29049913469777,
8.27007790985519)) ;
#76206 = CARTESIAN_POINT('Ctrl Pts',(-0.563402527094011,2.29049913469777,
8.27007790985519)) ;
#76207 = CARTESIAN_POINT('Ctrl Pts',(-0.563094923804728,2.29005214549267,
8.27032501917936)) ;
#76208 = CARTESIAN_POINT('Ctrl Pts',(-0.562784097682946,2.28959720721989,
8.27056932236647)) ;
#76209 = CARTESIAN_POINT('Ctrl Pts',(-0.518364204358841,2.22542453008761,
8.30657276282558)) ;
#76210 = CARTESIAN_POINT('Ctrl Pts',(-0.463831274313048,2.12754393145512,
8.30894915525216)) ;
#76211 = CARTESIAN_POINT('Ctrl Pts',(-0.459053285493787,2.10247651427316,
8.254336493146)) ;
#76212 = CARTESIAN_POINT('Origin',(0.,0.,8.18016875778516)) ;
#76213 = CARTESIAN_POINT('',(0.372950005137295,2.18682986267501,8.20605066229541)) ;
#76214 = CARTESIAN_POINT('Origin',(-1.10454254757634E-16,0.,8.20605066229541)) ;
#76215 = CARTESIAN_POINT('',(0.374769931517269,2.19218377594761,8.22161041260296)) ;
#76216 = CARTESIAN_POINT('Origin',(0.356848236098008,2.26130448641591,8.18949965397682)) ;
#76217 = CARTESIAN_POINT('',(0.563402527094043,2.29049913469776,8.27007790985519)) ;
#76218 = CARTESIAN_POINT('Ctrl Pts',(0.563402527094042,2.29049913469776,8.27007790985519)) ;
#76219 = CARTESIAN_POINT('Ctrl Pts',(0.562908327135226,2.29034966355222,8.27020605330626)) ;
#76220 = CARTESIAN_POINT('Ctrl Pts',(0.562407667443435,2.29019609074898,8.27033080754371)) ;
#76221 = CARTESIAN_POINT('Ctrl Pts',(0.482714730480227,2.26627787676058,8.29148068544431)) ;
#76222 = CARTESIAN_POINT('Ctrl Pts',(0.380213170858573,2.21661176558288,8.27650315801665)) ;
#76223 = CARTESIAN_POINT('Ctrl Pts',(0.374769931517269,2.19218377594761,8.22161041260296)) ;
#76224 = CARTESIAN_POINT('Origin',(0.,0.,8.27007790985519)) ;
#76225 = CARTESIAN_POINT('Origin',(0.,0.,8.8138)) ;
#76226 = CARTESIAN_POINT('',(0.246063080838827,1.82343508275074,6.79368809548975)) ;
#76227 = CARTESIAN_POINT('Origin',(-9.16116711833935E-17,0.,6.79368809548975)) ;
#76228 = CARTESIAN_POINT('Ctrl Pts',(0.372950005137295,2.18682986267501,8.20605066229541)) ;
#76229 = CARTESIAN_POINT('Ctrl Pts',(0.356060675112335,2.13837067836455,8.01717588129979)) ;
#76230 = CARTESIAN_POINT('Ctrl Pts',(0.339169373366003,2.08986565451436,7.82831193143937)) ;
#76231 = CARTESIAN_POINT('Ctrl Pts',(0.305304200525137,1.99279235652906,7.45075381522683)) ;
#76232 = CARTESIAN_POINT('Ctrl Pts',(0.288330373027766,1.94422406244447,7.26205962744222)) ;
#76233 = CARTESIAN_POINT('Ctrl Pts',(0.262904814260669,1.87155513860968,6.98014705352744)) ;
#76234 = CARTESIAN_POINT('Ctrl Pts',(0.254486208871158,1.84750496780177,6.886915184612)) ;
#76235 = CARTESIAN_POINT('Ctrl Pts',(0.246063080838828,1.82343508275074,6.79368809548975)) ;
#76236 = CARTESIAN_POINT('Origin',(0.,0.,6.81957)) ;
#76237 = CARTESIAN_POINT('',(0.233145498782361,1.72771014821048,6.71957)) ;
#76238 = CARTESIAN_POINT('Origin',(0.,0.,6.71957)) ;
#76239 = CARTESIAN_POINT('Origin',(0.233145498782361,1.72771014821048,6.81957)) ;
#76240 = CARTESIAN_POINT('Origin',(-0.233145498782355,4.55548777629246E-15,
6.81957)) ;
#76241 = CARTESIAN_POINT('',(-0.332764968591517,1.17558412963155,6.81085442572523)) ;
#76242 = CARTESIAN_POINT('',(-0.332764968591529,5.59476833506534E-15,6.81085442572523)) ;
#76243 = CARTESIAN_POINT('',(-0.233145498782343,1.13595304047785,6.71957)) ;
#76244 = CARTESIAN_POINT('Origin',(-0.233145498782343,1.13595304047785,6.81957)) ;
#76245 = CARTESIAN_POINT('',(-0.233145498782355,4.55548777629246E-15,6.71957)) ;
#76246 = CARTESIAN_POINT('Origin',(0.233145498782361,1.72771014821048,6.81957)) ;
#76247 = CARTESIAN_POINT('',(0.332764968591536,1.72771014821048,6.81085442572523)) ;
#76248 = CARTESIAN_POINT('Origin',(0.233145498782361,1.72771014821048,6.81957)) ;
#76249 = CARTESIAN_POINT('Origin',(0.233145498782361,1.72771014821048,6.81957)) ;
#76250 = CARTESIAN_POINT('Ctrl Pts',(0.245836001151724,1.82288075802732,6.79152461795156)) ;
#76251 = CARTESIAN_POINT('Ctrl Pts',(0.288494198954246,1.94477897799293,7.26365132481993)) ;
#76252 = CARTESIAN_POINT('Ctrl Pts',(0.330878369255154,2.06621031878836,7.73590073893382)) ;
#76253 = CARTESIAN_POINT('Ctrl Pts',(0.373113113874311,2.18739110879813,8.20821780878248)) ;
#76254 = CARTESIAN_POINT('Ctrl Pts',(0.272553537557606,1.81893081948751,6.79020849165203)) ;
#76255 = CARTESIAN_POINT('Ctrl Pts',(0.314905492765744,1.94050480823746,7.26244303991256)) ;
#76256 = CARTESIAN_POINT('Ctrl Pts',(0.357046431871077,2.06171037042182,7.73476924079919)) ;
#76257 = CARTESIAN_POINT('Ctrl Pts',(0.399066819643634,2.18268421515255,8.20715633330628)) ;
#76258 = CARTESIAN_POINT('Ctrl Pts',(0.316376716061575,1.79267106092127,6.7931645820536)) ;
#76259 = CARTESIAN_POINT('Ctrl Pts',(0.35799439116309,1.91413489045696,7.26547214220374)) ;
#76260 = CARTESIAN_POINT('Ctrl Pts',(0.399548971339515,2.03523918647934,7.73786227286442)) ;
#76261 = CARTESIAN_POINT('Ctrl Pts',(0.441077054244115,2.15615536078618,8.21029605360251)) ;
#76262 = CARTESIAN_POINT('Ctrl Pts',(0.332134835417778,1.74678141058443,6.80365184796761)) ;
#76263 = CARTESIAN_POINT('Ctrl Pts',(0.373443640776162,1.86867784544074,7.2758405013989)) ;
#76264 = CARTESIAN_POINT('Ctrl Pts',(0.414768073581239,1.99013064875085,7.74813767788448)) ;
#76265 = CARTESIAN_POINT('Ctrl Pts',(0.4560925176698,2.11134152617597,8.22049483777628)) ;
#76266 = CARTESIAN_POINT('Ctrl Pts',(0.33257555333983,1.72715033004413,6.80868939949129)) ;
#76267 = CARTESIAN_POINT('Ctrl Pts',(0.373881299048044,1.84923054417957,7.28081623334075)) ;
#76268 = CARTESIAN_POINT('Ctrl Pts',(0.415197777050322,1.97083234494938,7.75306573787267)) ;
#76269 = CARTESIAN_POINT('Ctrl Pts',(0.456520173465311,2.09216847821588,8.22538289017143)) ;
#76270 = CARTESIAN_POINT('',(0.456330681975407,2.09161206695506,8.2232169925309)) ;
#76271 = CARTESIAN_POINT('Origin',(0.356711212166233,2.09161206695506,8.23193256680567)) ;
#76272 = CARTESIAN_POINT('Ctrl Pts',(0.332764968591536,1.72771014821048,6.81085442572523)) ;
#76273 = CARTESIAN_POINT('Ctrl Pts',(0.373944470213856,1.84941569039776,7.28153828307)) ;
#76274 = CARTESIAN_POINT('Ctrl Pts',(0.415134631297243,1.97064606309602,7.75234397861228)) ;
#76275 = CARTESIAN_POINT('Ctrl Pts',(0.456330681975407,2.09161206695506,8.2232169925309)) ;
#76276 = CARTESIAN_POINT('Ctrl Pts',(0.372950005137295,2.18682986267501,8.20605066229542)) ;
#76277 = CARTESIAN_POINT('Ctrl Pts',(0.373662616506314,2.18815607354194,8.21137680913461)) ;
#76278 = CARTESIAN_POINT('Ctrl Pts',(0.374271909287362,2.18994876824218,8.21658807098568)) ;
#76279 = CARTESIAN_POINT('Ctrl Pts',(0.374769931517269,2.19218377594761,8.22161041260296)) ;
#76280 = CARTESIAN_POINT('Ctrl Pts',(0.39889297813086,2.18211755991818,8.20499152409472)) ;
#76281 = CARTESIAN_POINT('Ctrl Pts',(0.399569847844636,2.18345309008412,8.21059040433856)) ;
#76282 = CARTESIAN_POINT('Ctrl Pts',(0.400168655131417,2.18531329532944,8.21609868976098)) ;
#76283 = CARTESIAN_POINT('Ctrl Pts',(0.400674467091864,2.18764541195814,8.2213727471946)) ;
#76284 = CARTESIAN_POINT('Ctrl Pts',(0.440889933449603,2.15559078214375,8.20813192407366)) ;
#76285 = CARTESIAN_POINT('Ctrl Pts',(0.441564708190423,2.15729533880903,8.21524061522766)) ;
#76286 = CARTESIAN_POINT('Ctrl Pts',(0.44220475180715,2.15964157072195,8.22218874465405)) ;
#76287 = CARTESIAN_POINT('Ctrl Pts',(0.442802799136157,2.16260269917149,8.22888130401443)) ;
#76288 = CARTESIAN_POINT('Ctrl Pts',(0.45590301674854,2.11078568946555,8.21832875661974)) ;
#76289 = CARTESIAN_POINT('Ctrl Pts',(0.456741824116314,2.11321321015441,8.22792080639223)) ;
#76290 = CARTESIAN_POINT('Ctrl Pts',(0.457563066882852,2.11646373803811,8.23730217497138)) ;
#76291 = CARTESIAN_POINT('Ctrl Pts',(0.458353937819032,2.12049577671073,8.2463429126454)) ;
#76292 = CARTESIAN_POINT('Ctrl Pts',(0.456330681975408,2.09161206695506,8.22321699253091)) ;
#76293 = CARTESIAN_POINT('Ctrl Pts',(0.457262636912815,2.09434861239326,8.23386928620929)) ;
#76294 = CARTESIAN_POINT('Ctrl Pts',(0.458174489582082,2.09798645436109,8.24429180991143)) ;
#76295 = CARTESIAN_POINT('Ctrl Pts',(0.459053285493816,2.10247651427315,8.254336493146)) ;
#76296 = CARTESIAN_POINT('',(0.459053285493816,2.10247651427315,8.254336493146)) ;
#76297 = CARTESIAN_POINT('Origin',(0.359433815684642,2.10247651427315,8.26305206742076)) ;
#76298 = CARTESIAN_POINT('Origin',(0.45342712900337,2.23537208534447,8.19002923019672)) ;
#76299 = CARTESIAN_POINT('Ctrl Pts',(0.374769931517269,2.19218377594761,8.22161041260296)) ;
#76300 = CARTESIAN_POINT('Ctrl Pts',(0.380213170858573,2.21661176558288,8.27650315801665)) ;
#76301 = CARTESIAN_POINT('Ctrl Pts',(0.482714730480227,2.26627787676058,8.29148068544431)) ;
#76302 = CARTESIAN_POINT('Ctrl Pts',(0.562407667443435,2.29019609074898,8.27033080754371)) ;
#76303 = CARTESIAN_POINT('Ctrl Pts',(0.562908327135226,2.29034966355222,8.27020605330626)) ;
#76304 = CARTESIAN_POINT('Ctrl Pts',(0.563402527094042,2.29049913469776,8.27007790985519)) ;
#76305 = CARTESIAN_POINT('Ctrl Pts',(0.400674467091864,2.18764541195814,8.2213727471946)) ;
#76306 = CARTESIAN_POINT('Ctrl Pts',(0.404799111721846,2.20656371493878,8.26428096645554)) ;
#76307 = CARTESIAN_POINT('Ctrl Pts',(0.488360100380293,2.25706718975662,8.29516164781817)) ;
#76308 = CARTESIAN_POINT('Ctrl Pts',(0.562496982246372,2.29010647934773,8.27036199639192)) ;
#76309 = CARTESIAN_POINT('Ctrl Pts',(0.562950183191371,2.29030216829986,8.27022364133211)) ;
#76310 = CARTESIAN_POINT('Ctrl Pts',(0.563402527094042,2.29049913469776,8.27007790985519)) ;
#76311 = CARTESIAN_POINT('Ctrl Pts',(0.442802313774349,2.16260237888702,8.22888148964801)) ;
#76312 = CARTESIAN_POINT('Ctrl Pts',(0.445542573616263,2.17718689461836,8.26171487424146)) ;
#76313 = CARTESIAN_POINT('Ctrl Pts',(0.498696522073216,2.24300782603398,8.30074701463518)) ;
#76314 = CARTESIAN_POINT('Ctrl Pts',(0.562651405526709,2.28994112157589,8.27042096922394)) ;
#76315 = CARTESIAN_POINT('Ctrl Pts',(0.563023431289625,2.29021905160823,8.27025442037735)) ;
#76316 = CARTESIAN_POINT('Ctrl Pts',(0.563402527094042,2.29049913469776,8.27007790985519)) ;
#76317 = CARTESIAN_POINT('Ctrl Pts',(0.458353937819032,2.12049577671073,8.2463429126454)) ;
#76318 = CARTESIAN_POINT('Ctrl Pts',(0.462239142307061,2.14141849757278,8.29212651289291)) ;
#76319 = CARTESIAN_POINT('Ctrl Pts',(0.512038168879329,2.23076778087308,8.30482405987301)) ;
#76320 = CARTESIAN_POINT('Ctrl Pts',(0.56279297575247,2.28976846570632,8.27048768137762)) ;
#76321 = CARTESIAN_POINT('Ctrl Pts',(0.56309667938788,2.2901359349166,8.27028519942259)) ;
#76322 = CARTESIAN_POINT('Ctrl Pts',(0.563402527094042,2.29049913469776,8.27007790985519)) ;
#76323 = CARTESIAN_POINT('Ctrl Pts',(0.459053285493816,2.10247651427315,8.254336493146)) ;
#76324 = CARTESIAN_POINT('Ctrl Pts',(0.463835018009939,2.12756357252473,8.3089919459031)) ;
#76325 = CARTESIAN_POINT('Ctrl Pts',(0.518436488456744,2.22555128597153,8.30657023214747)) ;
#76326 = CARTESIAN_POINT('Ctrl Pts',(0.562850741503104,2.28969445195835,8.27051650449314)) ;
#76327 = CARTESIAN_POINT('Ctrl Pts',(0.563128071429989,2.29010031347733,8.27029839044198)) ;
#76328 = CARTESIAN_POINT('Ctrl Pts',(0.563402527094042,2.29049913469776,8.27007790985519)) ;
#76329 = CARTESIAN_POINT('Ctrl Pts',(0.459053285493816,2.10247651427315,8.254336493146)) ;
#76330 = CARTESIAN_POINT('Ctrl Pts',(0.463835018009939,2.12756357252473,8.3089919459031)) ;
#76331 = CARTESIAN_POINT('Ctrl Pts',(0.518436488456744,2.22555128597153,8.30657023214747)) ;
#76332 = CARTESIAN_POINT('Ctrl Pts',(0.562850741503104,2.28969445195835,8.27051650449314)) ;
#76333 = CARTESIAN_POINT('Ctrl Pts',(0.563128071429989,2.29010031347733,8.27029839044198)) ;
#76334 = CARTESIAN_POINT('Ctrl Pts',(0.563402527094042,2.29049913469776,8.27007790985519)) ;
#76335 = CARTESIAN_POINT('Origin',(0.135929041739328,3.89259393415546E-17,
3.41363816217501)) ;
#76336 = CARTESIAN_POINT('',(0.48491286401861,1.20584822770277,8.54991282821175)) ;
#76337 = CARTESIAN_POINT('Origin',(0.0363095719301537,1.03979559951686E-17,
3.42235373644978)) ;
#76338 = CARTESIAN_POINT('',(0.595585710062521,1.22865054909962,8.63793337445424)) ;
#76339 = CARTESIAN_POINT('Origin',(0.584532333827785,1.20584822770277,8.54119725393698)) ;
#76340 = CARTESIAN_POINT('Origin',(0.138499429641967,3.9662020184192E-17,
3.41341328237267)) ;
#76341 = CARTESIAN_POINT('Origin',(0.508,1.45475734489699E-16,8.8138)) ;
#76342 = CARTESIAN_POINT('',(0.332764968591536,1.17558412963154,6.81085442572523)) ;
#76343 = CARTESIAN_POINT('',(0.332764968591536,9.52937563352271E-17,6.81085442572523)) ;
#76344 = CARTESIAN_POINT('',(0.507754795155589,1.21039177030075,8.81099729580349)) ;
#76345 = CARTESIAN_POINT('Origin',(0.233145498782362,6.67657729888411E-17,
6.81957)) ;
#76346 = CARTESIAN_POINT('',(0.233145498782361,1.13595304047785,6.71957)) ;
#76347 = CARTESIAN_POINT('',(0.233145498782362,6.67657729888411E-17,6.71957)) ;
#76348 = CARTESIAN_POINT('Origin',(0.233145498782361,1.13595304047784,6.81957)) ;
#76349 = CARTESIAN_POINT('Ctrl Pts',(0.233145498782362,1.13595304047784,6.71957)) ;
#76350 = CARTESIAN_POINT('Ctrl Pts',(0.286360727148734,1.136701792954,6.71957)) ;
#76351 = CARTESIAN_POINT('Ctrl Pts',(0.33571003645063,1.13739615091638,6.7615916062195)) ;
#76352 = CARTESIAN_POINT('Ctrl Pts',(0.340348049204388,1.13746140899458,6.81085442572523)) ;
#76353 = CARTESIAN_POINT('Ctrl Pts',(0.233145498782362,1.13595304047784,6.71957)) ;
#76354 = CARTESIAN_POINT('Ctrl Pts',(0.285105982851001,1.14300981851451,6.71957)) ;
#76355 = CARTESIAN_POINT('Ctrl Pts',(0.331172502747836,1.14898571310985,6.76307285057327)) ;
#76356 = CARTESIAN_POINT('Ctrl Pts',(0.335376993538154,1.14951407564648,6.81107958928014)) ;
#76357 = CARTESIAN_POINT('Ctrl Pts',(0.233145498782362,1.13595304047784,6.71957)) ;
#76358 = CARTESIAN_POINT('Ctrl Pts',(0.283851238553268,1.14931784407503,6.71957)) ;
#76359 = CARTESIAN_POINT('Ctrl Pts',(0.328698029275171,1.16142573132119,6.76307285057327)) ;
#76360 = CARTESIAN_POINT('Ctrl Pts',(0.33278466785003,1.16254657695484,6.81107958928014)) ;
#76361 = CARTESIAN_POINT('Ctrl Pts',(0.233145498782362,1.13595304047784,6.71957)) ;
#76362 = CARTESIAN_POINT('Ctrl Pts',(0.282596494255534,1.15562586963554,6.71957)) ;
#76363 = CARTESIAN_POINT('Ctrl Pts',(0.328455030351461,1.17386952959435,6.7615916062195)) ;
#76364 = CARTESIAN_POINT('Ctrl Pts',(0.332764968591536,1.17558412963154,6.81085442572523)) ;
#76365 = CARTESIAN_POINT('',(0.340348049204388,1.13746140899458,6.81085442572523)) ;
#76366 = CARTESIAN_POINT('Origin',(0.432384438400711,1.17558412963154,6.80213885145047)) ;
#76367 = CARTESIAN_POINT('Origin',(0.233145498782362,1.13595304047784,6.81957)) ;
#76368 = CARTESIAN_POINT('Origin',(0.607374264964764,1.21039177030075,8.80228172152873)) ;
#76369 = CARTESIAN_POINT('',(0.492495944631461,1.16772550706581,8.54991282821175)) ;
#76370 = CARTESIAN_POINT('',(0.515337875768441,1.17226904966379,8.81099729580349)) ;
#76371 = CARTESIAN_POINT('Origin',(0.584532333827784,1.20584822770277,8.54119725393698)) ;
#76372 = CARTESIAN_POINT('Origin',(0.584532333827785,1.20584822770277,8.54119725393698)) ;
#76373 = CARTESIAN_POINT('Origin',(0.584532333827785,1.20584822770277,8.54119725393698)) ;
#76374 = CARTESIAN_POINT('Origin',(0.854554628096495,0.353968116746256,8.8138)) ;
#76375 = CARTESIAN_POINT('',(0.558026198990147,0.611939867549503,6.81085442572523)) ;
#76376 = CARTESIAN_POINT('',(0.692658569199242,0.286908573456262,6.81085442572523)) ;
#76377 = CARTESIAN_POINT('',(0.570056476111073,0.623970147580653,6.99051559579716)) ;
#76378 = CARTESIAN_POINT('',(0.691124600663687,0.745038269223043,8.7985570068643)) ;
#76379 = CARTESIAN_POINT('',(0.506191638276493,0.823877279363036,7.19051557427477)) ;
#76380 = CARTESIAN_POINT('Origin',(0.58903435075111,0.623877279363035,7.19051557427477)) ;
#76381 = CARTESIAN_POINT('',(0.639686894805704,0.823877279363036,8.60022433223443)) ;
#76382 = CARTESIAN_POINT('',(0.611189919984901,0.823877279363036,8.29929652382612)) ;
#76383 = CARTESIAN_POINT('Origin',(0.415843288169372,0.172247929781573,3.38615128096072)) ;
#76384 = CARTESIAN_POINT('Origin',(0.600622180002919,0.248785852819297,6.81957)) ;
#76385 = CARTESIAN_POINT('',(0.497571705638608,0.497571705638606,6.71957)) ;
#76386 = CARTESIAN_POINT('',(0.600622180002919,0.248785852819297,6.71957)) ;
#76387 = CARTESIAN_POINT('Origin',(0.497571705638608,0.497571705638606,6.81957)) ;
#76388 = CARTESIAN_POINT('Ctrl Pts',(-0.233145498782343,1.13595304047785,
6.71957)) ;
#76389 = CARTESIAN_POINT('Ctrl Pts',(-0.282596494255515,1.15562586963555,
6.71957)) ;
#76390 = CARTESIAN_POINT('Ctrl Pts',(-0.328455030351442,1.17386952959436,
6.7615916062195)) ;
#76391 = CARTESIAN_POINT('Ctrl Pts',(-0.332764968591517,1.17558412963155,
6.81085442572523)) ;
#76392 = CARTESIAN_POINT('Ctrl Pts',(-0.233145498782343,1.13595304047785,
6.71957)) ;
#76393 = CARTESIAN_POINT('Ctrl Pts',(-0.283851238553249,1.14931784407504,
6.71957)) ;
#76394 = CARTESIAN_POINT('Ctrl Pts',(-0.328698029275152,1.1614257313212,6.76307285057327)) ;
#76395 = CARTESIAN_POINT('Ctrl Pts',(-0.332784667850011,1.16254657695485,
6.81107958928014)) ;
#76396 = CARTESIAN_POINT('Ctrl Pts',(-0.233145498782343,1.13595304047785,
6.71957)) ;
#76397 = CARTESIAN_POINT('Ctrl Pts',(-0.285105982850982,1.14300981851452,
6.71957)) ;
#76398 = CARTESIAN_POINT('Ctrl Pts',(-0.331172502747817,1.14898571310986,
6.76307285057327)) ;
#76399 = CARTESIAN_POINT('Ctrl Pts',(-0.335376993538135,1.14951407564649,
6.81107958928014)) ;
#76400 = CARTESIAN_POINT('Ctrl Pts',(-0.233145498782343,1.13595304047785,
6.71957)) ;
#76401 = CARTESIAN_POINT('Ctrl Pts',(-0.286360727148716,1.13670179295401,
6.71957)) ;
#76402 = CARTESIAN_POINT('Ctrl Pts',(-0.335710036450612,1.13739615091639,
6.7615916062195)) ;
#76403 = CARTESIAN_POINT('Ctrl Pts',(-0.340348049204369,1.13746140899459,
6.81085442572523)) ;
#76404 = CARTESIAN_POINT('',(-0.340348049204369,1.13746140899459,6.81085442572523)) ;
#76405 = CARTESIAN_POINT('Origin',(-0.432384438400691,1.17558412963155,6.80213885145047)) ;
#76406 = CARTESIAN_POINT('Origin',(-0.233145498782343,1.13595304047785,6.81957)) ;
#76407 = CARTESIAN_POINT('Origin',(-0.607374264964743,1.21039177030077,8.80228172152873)) ;
#76408 = CARTESIAN_POINT('',(-0.48491286401859,1.20584822770278,8.54991282821175)) ;
#76409 = CARTESIAN_POINT('',(-0.507754795155569,1.21039177030076,8.81099729580349)) ;
#76410 = CARTESIAN_POINT('',(-0.492495944631442,1.16772550706582,8.54991282821175)) ;
#76411 = CARTESIAN_POINT('Origin',(-0.584532333827764,1.20584822770279,8.54119725393698)) ;
#76412 = CARTESIAN_POINT('',(-0.515337875768421,1.1722690496638,8.81099729580349)) ;
#76413 = CARTESIAN_POINT('Origin',(-0.584532333827764,1.20584822770279,8.54119725393698)) ;
#76414 = CARTESIAN_POINT('',(-0.5955857100625,1.22865054909963,8.63793337445423)) ;
#76415 = CARTESIAN_POINT('Origin',(-0.584532333827764,1.20584822770279,8.54119725393698)) ;
#76416 = CARTESIAN_POINT('Origin',(-0.584532333827764,1.20584822770279,8.54119725393698)) ;
#76417 = CARTESIAN_POINT('Origin',(-0.507999999999992,9.54610490470689E-15,
8.8138)) ;
#76418 = CARTESIAN_POINT('Origin',(-0.0363095719301483,3.78799769529521E-16,
3.42235373644978)) ;
#76419 = CARTESIAN_POINT('Origin',(-0.600622180002913,0.248785852819307,6.81957)) ;
#76420 = CARTESIAN_POINT('',(-0.558026198990135,0.611939867549514,6.81085442572523)) ;
#76421 = CARTESIAN_POINT('',(-0.692658569199236,0.286908573456273,6.81085442572523)) ;
#76422 = CARTESIAN_POINT('',(-0.497571705638597,0.497571705638616,6.71957)) ;
#76423 = CARTESIAN_POINT('Origin',(-0.497571705638597,0.497571705638616,6.81957)) ;
#76424 = CARTESIAN_POINT('',(-0.600622180002913,0.248785852819307,6.71957)) ;
#76425 = CARTESIAN_POINT('Ctrl Pts',(-1.19897656428781,-0.496373153556905,
6.33534590600784)) ;
#76426 = CARTESIAN_POINT('Ctrl Pts',(-1.29413398678263,-0.345965287843427,
6.33536184533624)) ;
#76427 = CARTESIAN_POINT('Ctrl Pts',(-1.35715515810585,-0.175923801053208,
6.33539451712114)) ;
#76428 = CARTESIAN_POINT('Ctrl Pts',(-1.44171628055285,0.383734652831137,
6.33548203852068)) ;
#76429 = CARTESIAN_POINT('Ctrl Pts',(-1.33636524997174,0.791226364481497,
6.33543138977132)) ;
#76430 = CARTESIAN_POINT('Ctrl Pts',(-0.836647006099026,1.44451988146956,
6.33553163726836)) ;
#76431 = CARTESIAN_POINT('Ctrl Pts',(-0.429590154010006,1.67667510461985,
6.3354782063715)) ;
#76432 = CARTESIAN_POINT('Ctrl Pts',(0.198582828796795,1.75115739905097,6.33553659953948)) ;
#76433 = CARTESIAN_POINT('Ctrl Pts',(0.401406734790799,1.74183016014963,6.33550804006764)) ;
#76434 = CARTESIAN_POINT('Ctrl Pts',(0.596911211671376,1.69935525494279,6.33551075406924)) ;
#76435 = CARTESIAN_POINT('Ctrl Pts',(-1.21215577023931,-0.504706728862282,
6.34487726987667)) ;
#76436 = CARTESIAN_POINT('Ctrl Pts',(-1.30846683220268,-0.352463959114778,
6.34488305795696)) ;
#76437 = CARTESIAN_POINT('Ctrl Pts',(-1.37224255462146,-0.180350962994336,
6.34489495668493)) ;
#76438 = CARTESIAN_POINT('Ctrl Pts',(-1.45778550015873,0.385929272949004,
6.34492679187801)) ;
#76439 = CARTESIAN_POINT('Ctrl Pts',(-1.3512559606378,0.797418860642494,6.34490852424714)) ;
#76440 = CARTESIAN_POINT('Ctrl Pts',(-0.846299872573819,1.45757218278905,
6.34494501369235)) ;
#76441 = CARTESIAN_POINT('Ctrl Pts',(-0.435532263532225,1.69162660148109,
6.34492573960143)) ;
#76442 = CARTESIAN_POINT('Ctrl Pts',(0.198561637302729,1.76680713847606,6.34494698214462)) ;
#76443 = CARTESIAN_POINT('Ctrl Pts',(0.403018497435118,1.75737616029807,6.34493664202809)) ;
#76444 = CARTESIAN_POINT('Ctrl Pts',(0.600209236713373,1.71453384471607,6.34493762678056)) ;
#76445 = CARTESIAN_POINT('Ctrl Pts',(-1.22757973634767,-0.514459810923294,
6.35000000399322)) ;
#76446 = CARTESIAN_POINT('Ctrl Pts',(-1.3252389028925,-0.360066440752681,
6.34999995101887)) ;
#76447 = CARTESIAN_POINT('Ctrl Pts',(-1.38989146862233,-0.185526310309135,
6.34999987913905)) ;
#76448 = CARTESIAN_POINT('Ctrl Pts',(-1.47656546565633,0.388502446092232,
6.34999966194095)) ;
#76449 = CARTESIAN_POINT('Ctrl Pts',(-1.36866779698095,0.804666226495404,
6.34999994431863)) ;
#76450 = CARTESIAN_POINT('Ctrl Pts',(-0.857572260759232,1.47282532997322,
6.34999973263467)) ;
#76451 = CARTESIAN_POINT('Ctrl Pts',(-0.442476950791247,1.70910146559139,
6.35000002494746)) ;
#76452 = CARTESIAN_POINT('Ctrl Pts',(0.198536630827523,1.78508389827109,6.34999989493859)) ;
#76453 = CARTESIAN_POINT('Ctrl Pts',(0.404900148830056,1.7755363105867,6.35000001032902)) ;
#76454 = CARTESIAN_POINT('Ctrl Pts',(0.604061670832201,1.73226400636545,6.35000000159026)) ;
#76455 = CARTESIAN_POINT('Ctrl Pts',(-1.24302441939919,-0.524226019081257,
6.35)) ;
#76456 = CARTESIAN_POINT('Ctrl Pts',(-1.34203370677612,-0.367678700862383,
6.35000000000002)) ;
#76457 = CARTESIAN_POINT('Ctrl Pts',(-1.40756443263931,-0.190707970016344,
6.35000000000006)) ;
#76458 = CARTESIAN_POINT('Ctrl Pts',(-1.49537112857496,0.391080480273729,
6.35000000000016)) ;
#76459 = CARTESIAN_POINT('Ctrl Pts',(-1.38610400991126,0.81192437938103,6.35000000000003)) ;
#76460 = CARTESIAN_POINT('Ctrl Pts',(-0.868860233572473,1.48809999932316,
6.35000000000013)) ;
#76461 = CARTESIAN_POINT('Ctrl Pts',(-0.449431916290035,1.72660012548333,
6.34999999999999)) ;
#76462 = CARTESIAN_POINT('Ctrl Pts',(0.198511164967717,1.80338490120432,6.35000000000006)) ;
#76463 = CARTESIAN_POINT('Ctrl Pts',(0.406783902157189,1.7937204004824,6.35)) ;
#76464 = CARTESIAN_POINT('Ctrl Pts',(0.607919164074007,1.75001745175322,6.35)) ;
#76465 = CARTESIAN_POINT('',(-1.25119325853947,-0.511138653598631,6.35000000000021)) ;
#76466 = CARTESIAN_POINT('',(-1.20400491191847,-0.491561463064185,6.33635925836751)) ;
#76467 = CARTESIAN_POINT('Ctrl Pts',(-1.25036088004395,-0.512489623160576,
6.35000000000042)) ;
#76468 = CARTESIAN_POINT('Ctrl Pts',(-1.24997941519213,-0.512351401822971,
6.35000000000042)) ;
#76469 = CARTESIAN_POINT('Ctrl Pts',(-1.2495980855261,-0.512212821605165,
6.34999757998896)) ;
#76470 = CARTESIAN_POINT('Ctrl Pts',(-1.24126534039648,-0.509175370306275,
6.34989186587608)) ;
#76471 = CARTESIAN_POINT('Ctrl Pts',(-1.23339061866593,-0.506113476122858,
6.34874097096721)) ;
#76472 = CARTESIAN_POINT('Ctrl Pts',(-1.2169454739642,-0.499124478633754,
6.34401101135452)) ;
#76473 = CARTESIAN_POINT('Ctrl Pts',(-1.20962851798745,-0.495529127664985,
6.34035540742519)) ;
#76474 = CARTESIAN_POINT('Ctrl Pts',(-1.20344341232604,-0.492722585888641,
6.33644055435381)) ;
#76475 = CARTESIAN_POINT('',(0.607919162256355,1.75001744338779,6.35)) ;
#76476 = CARTESIAN_POINT('Ctrl Pts',(-1.25202563703499,-0.509787684036685,
6.35)) ;
#76477 = CARTESIAN_POINT('Ctrl Pts',(-1.3460115207624,-0.356834498649399,
6.35)) ;
#76478 = CARTESIAN_POINT('Ctrl Pts',(-1.4084112566866,-0.185097036772204,
6.35)) ;
#76479 = CARTESIAN_POINT('Ctrl Pts',(-1.49537111971372,0.391080479058958,
6.35)) ;
#76480 = CARTESIAN_POINT('Ctrl Pts',(-1.38610400169531,0.811924375960986,
6.35)) ;
#76481 = CARTESIAN_POINT('Ctrl Pts',(-0.868860228253576,1.48809999212573,
6.35)) ;
#76482 = CARTESIAN_POINT('Ctrl Pts',(-0.449431913012853,1.72660011723795,
6.35)) ;
#76483 = CARTESIAN_POINT('Ctrl Pts',(0.198511164979717,1.80338489258088,6.35000000000001)) ;
#76484 = CARTESIAN_POINT('Ctrl Pts',(0.406783901269564,1.79372039191405,6.35)) ;
#76485 = CARTESIAN_POINT('Ctrl Pts',(0.607919162256355,1.75001744338779,6.35)) ;
#76486 = CARTESIAN_POINT('',(0.594304716461005,1.70160433312498,6.33648831456159)) ;
#76487 = CARTESIAN_POINT('Ctrl Pts',(0.60791916225634,1.75001744338779,6.35)) ;
#76488 = CARTESIAN_POINT('Ctrl Pts',(0.604753665677747,1.74176297877533,6.35)) ;
#76489 = CARTESIAN_POINT('Ctrl Pts',(0.602355935083414,1.7333216626848,6.34883057893477)) ;
#76490 = CARTESIAN_POINT('Ctrl Pts',(0.60025191269834,1.72507625378891,6.34654040403937)) ;
#76491 = CARTESIAN_POINT('Ctrl Pts',(0.598158805400061,1.71687361979617,6.34426210993854)) ;
#76492 = CARTESIAN_POINT('Ctrl Pts',(0.596356014106384,1.70891213133337,6.34088508516807)) ;
#76493 = CARTESIAN_POINT('Ctrl Pts',(0.594304466751201,1.70160440748,6.3364883075039)) ;
#76494 = CARTESIAN_POINT('',(0.19398202776272,1.74176856709214,6.33644353759349)) ;
#76495 = CARTESIAN_POINT('Origin',(0.16425687912765,-0.0151938657249959,6.33858452768918)) ;
#76496 = CARTESIAN_POINT('',(-4.4909026429235E-6,1.72916360454791,6.3364693018353)) ;
#76497 = CARTESIAN_POINT('Origin',(0.213889544320394,-0.0749718660965196,
6.33467644420639)) ;
#76498 = CARTESIAN_POINT('',(-1.10119630440643,1.10117706072883,6.33647087602767)) ;
#76499 = CARTESIAN_POINT('Ctrl Pts',(-4.4909026429235E-6,1.72916360454791,
6.3364693018353)) ;
#76500 = CARTESIAN_POINT('Ctrl Pts',(-0.0665061084793492,1.72124714308604,
6.33650496012767)) ;
#76501 = CARTESIAN_POINT('Ctrl Pts',(-0.132510009690253,1.70920342784116,
6.33651427418665)) ;
#76502 = CARTESIAN_POINT('Ctrl Pts',(-0.263070109646108,1.67694172545347,
6.33650910196814)) ;
#76503 = CARTESIAN_POINT('Ctrl Pts',(-0.327610814596463,1.6566587125351,6.33649450722964)) ;
#76504 = CARTESIAN_POINT('Ctrl Pts',(-0.452410105447889,1.60873680599921,
6.33646432848932)) ;
#76505 = CARTESIAN_POINT('Ctrl Pts',(-0.512730304175064,1.58126016034659,
6.33644883463083)) ;
#76506 = CARTESIAN_POINT('Ctrl Pts',(-0.626197844265137,1.52099206858123,
6.33642982252685)) ;
#76507 = CARTESIAN_POINT('Ctrl Pts',(-0.679558438269731,1.48860977014624,
6.33642565469618)) ;
#76508 = CARTESIAN_POINT('Ctrl Pts',(-0.780540073139769,1.41911622837787,
6.33642910803844)) ;
#76509 = CARTESIAN_POINT('Ctrl Pts',(-0.828293287848511,1.38219980328802,
6.33643632858415)) ;
#76510 = CARTESIAN_POINT('Ctrl Pts',(-0.917251046616824,1.30518172810159,
6.33645463390669)) ;
#76511 = CARTESIAN_POINT('Ctrl Pts',(-0.958658491361404,1.26531484067809,
6.33646547200062)) ;
#76512 = CARTESIAN_POINT('Ctrl Pts',(-1.03416386990157,1.18449355631453,6.33647786812632)) ;
#76513 = CARTESIAN_POINT('Ctrl Pts',(-1.06857292586319,1.14382378089233,6.33647997034051)) ;
#76514 = CARTESIAN_POINT('Ctrl Pts',(-1.10097095202783,1.10147182646993,6.33647094593189)) ;
#76515 = CARTESIAN_POINT('Ctrl Pts',(-1.10108364246668,1.10132445464862,6.33647091226235)) ;
#76516 = CARTESIAN_POINT('Ctrl Pts',(-1.1011963026744,1.10117706299481,6.33647087602822)) ;
#76517 = CARTESIAN_POINT('',(-1.3852993521282,-4.08688681438726E-6,6.33637672541782)) ;
#76518 = CARTESIAN_POINT('Ctrl Pts',(-1.10119630613845,1.10117705846285,6.33647087602712)) ;
#76519 = CARTESIAN_POINT('Ctrl Pts',(-1.13938277645153,1.051218319285,6.33645864387353)) ;
#76520 = CARTESIAN_POINT('Ctrl Pts',(-1.17431132247377,0.998818901911678,
6.33643471829354)) ;
#76521 = CARTESIAN_POINT('Ctrl Pts',(-1.23721697009887,0.889841017732942,
6.33638704294256)) ;
#76522 = CARTESIAN_POINT('Ctrl Pts',(-1.26517422524756,0.833250534509621,
6.33636340531505)) ;
#76523 = CARTESIAN_POINT('Ctrl Pts',(-1.31279727825361,0.718791029418644,
6.3363325975561)) ;
#76524 = CARTESIAN_POINT('Ctrl Pts',(-1.33269939463148,0.661020067748072,
6.33632499965946)) ;
#76525 = CARTESIAN_POINT('Ctrl Pts',(-1.36402855946461,0.54744755398184,6.33632837595744)) ;
#76526 = CARTESIAN_POINT('Ctrl Pts',(-1.3759424927561,0.491781944166528,6.3363381112914)) ;
#76527 = CARTESIAN_POINT('Ctrl Pts',(-1.39287767449329,0.381480997714738,
6.33636606701108)) ;
#76528 = CARTESIAN_POINT('Ctrl Pts',(-1.39813367468696,0.326882051026805,
6.33638395114502)) ;
#76529 = CARTESIAN_POINT('Ctrl Pts',(-1.40234100536283,0.220109276797855,
6.33641137980185)) ;
#76530 = CARTESIAN_POINT('Ctrl Pts',(-1.40158254582667,0.167945264364892,
6.3364212275538)) ;
#76531 = CARTESIAN_POINT('Ctrl Pts',(-1.39534727997868,0.0772083222647631,
6.33641343495368)) ;
#76532 = CARTESIAN_POINT('Ctrl Pts',(-1.39110922614765,0.0385255715080943,
6.33640201154189)) ;
#76533 = CARTESIAN_POINT('Ctrl Pts',(-1.38531426391836,9.48044437915691E-5,
6.33637679031753)) ;
#76534 = CARTESIAN_POINT('Ctrl Pts',(-1.38530680871705,4.53633786673787E-5,
6.3363767578705)) ;
#76535 = CARTESIAN_POINT('Ctrl Pts',(-1.38529935351574,-4.07768645681171E-6,
6.33637672542347)) ;
#76536 = CARTESIAN_POINT('Ctrl Pts',(-1.38529935074065,-4.09608717196282E-6,
6.33637672541216)) ;
#76537 = CARTESIAN_POINT('Ctrl Pts',(-1.37604524760285,-0.0613380044097079,
6.33633667262024)) ;
#76538 = CARTESIAN_POINT('Ctrl Pts',(-1.36241347430925,-0.12191631163429,
6.33631060447636)) ;
#76539 = CARTESIAN_POINT('Ctrl Pts',(-1.32811348145613,-0.23561790872716,
6.33628334303435)) ;
#76540 = CARTESIAN_POINT('Ctrl Pts',(-1.30810808812469,-0.288947817502873,
6.33628041020224)) ;
#76541 = CARTESIAN_POINT('Ctrl Pts',(-1.26130677709146,-0.392319081970156,
6.33628196319371)) ;
#76542 = CARTESIAN_POINT('Ctrl Pts',(-1.23453616146347,-0.442372792708542,
6.33628658201929)) ;
#76543 = CARTESIAN_POINT('Ctrl Pts',(-1.20454071887332,-0.490453469945117,
6.33628168225624)) ;
#76544 = CARTESIAN_POINT('Origin',(0.,0.,6.25)) ;
#76545 = CARTESIAN_POINT('Ctrl Pts',(1.24732203681758,1.23117606233602,6.24999999746782)) ;
#76546 = CARTESIAN_POINT('Ctrl Pts',(1.18413913631208,1.29518756019404,6.25616282366101)) ;
#76547 = CARTESIAN_POINT('Ctrl Pts',(1.11684156410954,1.35433254331176,6.26273026309037)) ;
#76548 = CARTESIAN_POINT('Ctrl Pts',(0.99465531308325,1.44818563488623,6.27524755812259)) ;
#76549 = CARTESIAN_POINT('Ctrl Pts',(0.942382820096697,1.48454101942919,6.28074455832599)) ;
#76550 = CARTESIAN_POINT('Ctrl Pts',(0.830300417999892,1.5558341017124,6.29330561895835)) ;
#76551 = CARTESIAN_POINT('Ctrl Pts',(0.771237474584706,1.58951246918406,6.30027618346742)) ;
#76552 = CARTESIAN_POINT('Ctrl Pts',(0.679530090341938,1.64018276569364,6.31325056551678)) ;
#76553 = CARTESIAN_POINT('Ctrl Pts',(0.648785354293156,1.65688362190668,6.31827793155166)) ;
#76554 = CARTESIAN_POINT('Ctrl Pts',(0.617263445317367,1.67664530547039,6.32521291659261)) ;
#76555 = CARTESIAN_POINT('Ctrl Pts',(0.606958715238955,1.68359083166877,6.32782718462676)) ;
#76556 = CARTESIAN_POINT('Ctrl Pts',(0.598340879348292,1.69193026794475,6.33148558224764)) ;
#76557 = CARTESIAN_POINT('Ctrl Pts',(0.596313784588478,1.69425091096469,6.33255389399815)) ;
#76558 = CARTESIAN_POINT('Ctrl Pts',(0.594687442078795,1.69738144367564,6.33413367934689)) ;
#76559 = CARTESIAN_POINT('Ctrl Pts',(0.594327845458634,1.69831237814393,6.33461894425858)) ;
#76560 = CARTESIAN_POINT('Ctrl Pts',(0.594048306100336,1.70005354271567,6.33557488964638)) ;
#76561 = CARTESIAN_POINT('Ctrl Pts',(0.594073405242955,1.70083850204704,6.33602442146924)) ;
#76562 = CARTESIAN_POINT('Ctrl Pts',(0.594304965275971,1.70160425498376,6.33648831934986)) ;
#76563 = CARTESIAN_POINT('',(1.65743956651353,-0.827659859698077,6.35)) ;
#76564 = CARTESIAN_POINT('Origin',(0.,0.,6.35)) ;
#76565 = CARTESIAN_POINT('Ctrl Pts',(1.65743956651353,-0.827659859698078,
6.35)) ;
#76566 = CARTESIAN_POINT('Ctrl Pts',(1.65708852425179,-0.827457333128657,
6.35)) ;
#76567 = CARTESIAN_POINT('Ctrl Pts',(1.65673746283553,-0.827254793665606,
6.34999757623592)) ;
#76568 = CARTESIAN_POINT('Ctrl Pts',(1.65638640318299,-0.827052253325088,
6.34999273010545)) ;
#76569 = CARTESIAN_POINT('Ctrl Pts',(1.64951073718717,-0.823085406887498,
6.3498978163941)) ;
#76570 = CARTESIAN_POINT('Ctrl Pts',(1.64267636638568,-0.819141560396678,
6.34887859204913)) ;
#76571 = CARTESIAN_POINT('Ctrl Pts',(1.63603787271552,-0.815310093330816,
6.34695079806314)) ;
#76572 = CARTESIAN_POINT('Ctrl Pts',(1.63254991824201,-0.813296988648264,
6.34593790899651)) ;
#76573 = CARTESIAN_POINT('Ctrl Pts',(1.62911592055215,-0.811314902311204,
6.34467332331189)) ;
#76574 = CARTESIAN_POINT('Ctrl Pts',(1.62575902753902,-0.809378263250201,
6.34315366875848)) ;
#76575 = CARTESIAN_POINT('Ctrl Pts',(1.62494337864994,-0.808907703869104,
6.34278442715815)) ;
#76576 = CARTESIAN_POINT('Ctrl Pts',(1.62413229353693,-0.808439840243547,
6.34240011167817)) ;
#76577 = CARTESIAN_POINT('Ctrl Pts',(1.62332600671688,-0.807974803235035,
6.34200093725414)) ;
#76578 = CARTESIAN_POINT('Ctrl Pts',(1.61699826737659,-0.804325192575065,
6.33886821618793)) ;
#76579 = CARTESIAN_POINT('Ctrl Pts',(1.61103685589427,-0.800890447046913,
6.33486039023559)) ;
#76580 = CARTESIAN_POINT('Ctrl Pts',(1.60554240364908,-0.797722810935053,
6.33011214573865)) ;
#76581 = CARTESIAN_POINT('Ctrl Pts',(1.6020280918537,-0.795696756206643,6.32707511658664)) ;
#76582 = CARTESIAN_POINT('Ctrl Pts',(1.59870513294145,-0.79378006756951,6.32373401573313)) ;
#76583 = CARTESIAN_POINT('Ctrl Pts',(1.5956055098213,-0.791990624580966,6.32011539552532)) ;
#76584 = CARTESIAN_POINT('Ctrl Pts',(1.59077222390879,-0.789200320969043,
6.31447283015682)) ;
#76585 = CARTESIAN_POINT('Ctrl Pts',(1.5865365972947,-0.786749991588918,6.30822233253495)) ;
#76586 = CARTESIAN_POINT('Ctrl Pts',(1.5830020225687,-0.784706540691024,6.3014789531298)) ;
#76587 = CARTESIAN_POINT('Ctrl Pts',(1.58165450135156,-0.78392749550042,6.29890810726343)) ;
#76588 = CARTESIAN_POINT('Ctrl Pts',(1.58040913941073,-0.783207875063578,
6.29626524041211)) ;
#76589 = CARTESIAN_POINT('Ctrl Pts',(1.57927293875872,-0.782552610644341,
6.29355567099931)) ;
#76590 = CARTESIAN_POINT('Ctrl Pts',(1.57850015058202,-0.782106931797997,
6.29171275425527)) ;
#76591 = CARTESIAN_POINT('Ctrl Pts',(1.57777789040688,-0.781691051893247,
6.28983899945262)) ;
#76592 = CARTESIAN_POINT('Ctrl Pts',(1.57710659769393,-0.781304970163598,
6.28793731545109)) ;
#76593 = CARTESIAN_POINT('Ctrl Pts',(1.57451220409407,-0.779812852121637,
6.28058773946527)) ;
#76594 = CARTESIAN_POINT('Ctrl Pts',(1.57270609928185,-0.778780519248468,
6.2729080946375)) ;
#76595 = CARTESIAN_POINT('Ctrl Pts',(1.57168491163117,-0.778195616556964,
6.26507674204093)) ;
#76596 = CARTESIAN_POINT('Ctrl Pts',(1.57103619973019,-0.777824055721258,
6.26010185654672)) ;
#76597 = CARTESIAN_POINT('Ctrl Pts',(1.57070507101749,-0.77763367306192,6.25506517605237)) ;
#76598 = CARTESIAN_POINT('Ctrl Pts',(1.57069890812158,-0.777628441215486,
6.25001120443579)) ;
#76599 = CARTESIAN_POINT('Ctrl Pts',(1.61549606864524,-0.799973712389905,
6.16354642763013)) ;
#76600 = CARTESIAN_POINT('Ctrl Pts',(1.50866006753038,-0.961820010632383,
6.16354845333704)) ;
#76601 = CARTESIAN_POINT('Ctrl Pts',(1.37608293211674,-1.10532255898405,6.16354532462513)) ;
#76602 = CARTESIAN_POINT('Ctrl Pts',(0.883476931069763,-1.4943581457905,6.163531510563)) ;
#76603 = CARTESIAN_POINT('Ctrl Pts',(0.43189736308726,-1.61774218765324,6.16360457949385)) ;
#76604 = CARTESIAN_POINT('Ctrl Pts',(-0.387735196455891,-1.50955658539216,
6.16357104016601)) ;
#76605 = CARTESIAN_POINT('Ctrl Pts',(-0.749793159276284,-1.2953985605636,
6.16366106980508)) ;
#76606 = CARTESIAN_POINT('Ctrl Pts',(-1.1629753731845,-0.736642926916648,
6.16361636307964)) ;
#76607 = CARTESIAN_POINT('Ctrl Pts',(-1.25283238131601,-0.42534079606347,
6.16372466795802)) ;
#76608 = CARTESIAN_POINT('Ctrl Pts',(-1.23093886224037,-0.123053381526151,
6.16370469001445)) ;
#76609 = CARTESIAN_POINT('Ctrl Pts',(1.59752029062636,-0.788108225162961,
6.1760668526113)) ;
#76610 = CARTESIAN_POINT('Ctrl Pts',(1.49196189973369,-0.948020502054166,
6.17606956401923)) ;
#76611 = CARTESIAN_POINT('Ctrl Pts',(1.3609705278398,-1.08981355145533,6.17606534815012)) ;
#76612 = CARTESIAN_POINT('Ctrl Pts',(0.87434993641677,-1.47414249680429,6.17604676793019)) ;
#76613 = CARTESIAN_POINT('Ctrl Pts',(0.429056350360505,-1.59568033539221,
6.17614438922054)) ;
#76614 = CARTESIAN_POINT('Ctrl Pts',(-0.379620525679053,-1.48898582643579,
6.17609935232033)) ;
#76615 = CARTESIAN_POINT('Ctrl Pts',(-0.735908001637101,-1.27801942757034,
6.17621960211951)) ;
#76616 = CARTESIAN_POINT('Ctrl Pts',(-1.14294046129122,-0.727613085333748,
6.17615971202283)) ;
#76617 = CARTESIAN_POINT('Ctrl Pts',(-1.23105598826309,-0.421830171326285,
6.17630424830084)) ;
#76618 = CARTESIAN_POINT('Ctrl Pts',(-1.20952162058803,-0.124606974019317,
6.1762775805103)) ;
#76619 = CARTESIAN_POINT('Ctrl Pts',(1.5698483850616,-0.769842498823944,6.21788308551004)) ;
#76620 = CARTESIAN_POINT('Ctrl Pts',(1.46625562510329,-0.926780606179969,
6.21788619683742)) ;
#76621 = CARTESIAN_POINT('Ctrl Pts',(1.33770404860818,-1.06594373674671,6.21788139808894)) ;
#76622 = CARTESIAN_POINT('Ctrl Pts',(0.860292194298888,-1.44302923241305,
6.21786016739722)) ;
#76623 = CARTESIAN_POINT('Ctrl Pts',(0.424681867511836,-1.56175458111409,
6.21797238130401)) ;
#76624 = CARTESIAN_POINT('Ctrl Pts',(-0.367140476130573,-1.45734375378515,
6.21792091065796)) ;
#76625 = CARTESIAN_POINT('Ctrl Pts',(-0.714565467179568,-1.25131365505249,
6.21805897503878)) ;
#76626 = CARTESIAN_POINT('Ctrl Pts',(-1.11212916749052,-0.713731553118314,
6.21799049458104)) ;
#76627 = CARTESIAN_POINT('Ctrl Pts',(-1.19759938063696,-0.416441940029509,
6.21815621890648)) ;
#76628 = CARTESIAN_POINT('Ctrl Pts',(-1.17660907946778,-0.126994427905559,
6.21812569329284)) ;
#76629 = CARTESIAN_POINT('Ctrl Pts',(1.57493624982465,-0.773200906693405,
6.29781698992439)) ;
#76630 = CARTESIAN_POINT('Ctrl Pts',(1.47098173367402,-0.930690200837764,
6.29781856153337)) ;
#76631 = CARTESIAN_POINT('Ctrl Pts',(1.34197704834607,-1.07033809638994,6.29781612216889)) ;
#76632 = CARTESIAN_POINT('Ctrl Pts',(0.862860470622287,-1.44875060656876,
6.29780535264256)) ;
#76633 = CARTESIAN_POINT('Ctrl Pts',(0.425481538277075,-1.56806968519663,
6.29786194185147)) ;
#76634 = CARTESIAN_POINT('Ctrl Pts',(-0.369463134207585,-1.46320470671826,
6.2978358625339)) ;
#76635 = CARTESIAN_POINT('Ctrl Pts',(-0.718577475421128,-1.25633176165636,
6.29790549425836)) ;
#76636 = CARTESIAN_POINT('Ctrl Pts',(-1.11787505857057,-0.716322512675761,
6.29787085558639)) ;
#76637 = CARTESIAN_POINT('Ctrl Pts',(-1.20393830023574,-0.417466203903967,
6.29795441514621)) ;
#76638 = CARTESIAN_POINT('Ctrl Pts',(-1.18282403856848,-0.126543598897747,
6.29793901542275)) ;
#76639 = CARTESIAN_POINT('Ctrl Pts',(1.61581214044334,-0.800182345689632,
6.34311290859866)) ;
#76640 = CARTESIAN_POINT('Ctrl Pts',(1.50895784490124,-0.962064092159509,
6.34311311389927)) ;
#76641 = CARTESIAN_POINT('Ctrl Pts',(1.37634244782511,-1.10559303782759,6.34311280868517)) ;
#76642 = CARTESIAN_POINT('Ctrl Pts',(0.883613373539448,-1.49468359196346,
6.34311143808909)) ;
#76643 = CARTESIAN_POINT('Ctrl Pts',(0.431936536099549,-1.61824483101601,
6.34311890585529)) ;
#76644 = CARTESIAN_POINT('Ctrl Pts',(-0.387923824817847,-1.50996073963872,
6.34311556995257)) ;
#76645 = CARTESIAN_POINT('Ctrl Pts',(-0.750207415867593,-1.29587835204616,
6.34312473370235)) ;
#76646 = CARTESIAN_POINT('Ctrl Pts',(-1.16347886666241,-0.736854773631983,
6.34312026707438)) ;
#76647 = CARTESIAN_POINT('Ctrl Pts',(-1.25359438063852,-0.425451420865333,
6.34313124490448)) ;
#76648 = CARTESIAN_POINT('Ctrl Pts',(-1.23164727574712,-0.123001993680601,
6.3431292332343)) ;
#76649 = CARTESIAN_POINT('Ctrl Pts',(1.64705017975234,-0.820802012667411,
6.35000039278962)) ;
#76650 = CARTESIAN_POINT('Ctrl Pts',(1.53797666056991,-0.986044738024822,
6.35000039841076)) ;
#76651 = CARTESIAN_POINT('Ctrl Pts',(1.40260339195363,-1.13254350570539,6.35000037441355)) ;
#76652 = CARTESIAN_POINT('Ctrl Pts',(0.899469482201931,-1.52980706906964,
6.35000029469085)) ;
#76653 = CARTESIAN_POINT('Ctrl Pts',(0.436871148542969,-1.6566054637442,6.3500004112916)) ;
#76654 = CARTESIAN_POINT('Ctrl Pts',(-0.402034709739736,-1.54571554501082,
6.3500002375136)) ;
#76655 = CARTESIAN_POINT('Ctrl Pts',(-0.774371464292586,-1.32611335453818,
6.35000040938403)) ;
#76656 = CARTESIAN_POINT('Ctrl Pts',(-1.19832606513914,-0.752556628717804,
6.35000021947629)) ;
#76657 = CARTESIAN_POINT('Ctrl Pts',(-1.29151446365418,-0.431561348191218,
6.3500004467796)) ;
#76658 = CARTESIAN_POINT('Ctrl Pts',(-1.2689337108479,-0.120297260428306,
6.35000039185858)) ;
#76659 = CARTESIAN_POINT('Ctrl Pts',(1.65744223319009,-0.82766161992323,6.3499999999496)) ;
#76660 = CARTESIAN_POINT('Ctrl Pts',(1.54763268784084,-0.994019054114616,
6.34999999994815)) ;
#76661 = CARTESIAN_POINT('Ctrl Pts',(1.41134138578638,-1.14150297307001,6.34999999995431)) ;
#76662 = CARTESIAN_POINT('Ctrl Pts',(0.904748656557809,-1.5414771327564,6.34999999997478)) ;
#76663 = CARTESIAN_POINT('Ctrl Pts',(0.438512116572987,-1.66934757026883,
6.34999999994481)) ;
#76664 = CARTESIAN_POINT('Ctrl Pts',(-0.406724020702625,-1.55758946118512,
6.34999999998944)) ;
#76665 = CARTESIAN_POINT('Ctrl Pts',(-0.782406486305098,-1.33615118986062,
6.34999999994525)) ;
#76666 = CARTESIAN_POINT('Ctrl Pts',(-1.20991300026391,-0.757768547394265,
6.34999999999403)) ;
#76667 = CARTESIAN_POINT('Ctrl Pts',(-1.30412899404698,-0.433585113928121,
6.34999999993561)) ;
#76668 = CARTESIAN_POINT('Ctrl Pts',(-1.28133803060964,-0.119397459306505,
6.34999999994972)) ;
#76669 = CARTESIAN_POINT('Ctrl Pts',(-1.1832560635873,-0.36080960203242,6.28787103703615)) ;
#76670 = CARTESIAN_POINT('Ctrl Pts',(-1.18290594752794,-0.38604397996115,
6.29445533087948)) ;
#76671 = CARTESIAN_POINT('Ctrl Pts',(-1.18269642318132,-0.415843789426796,
6.30282243761288)) ;
#76672 = CARTESIAN_POINT('Ctrl Pts',(-1.18596333720351,-0.454630048457181,
6.31600036209296)) ;
#76673 = CARTESIAN_POINT('Ctrl Pts',(-1.18798952321357,-0.467363137142688,
6.32090935151571)) ;
#76674 = CARTESIAN_POINT('Ctrl Pts',(-1.19281338362405,-0.480676013117452,
6.32741836869324)) ;
#76675 = CARTESIAN_POINT('Ctrl Pts',(-1.19465667987756,-0.484582846773843,
6.32954668642152)) ;
#76676 = CARTESIAN_POINT('Ctrl Pts',(-1.19814970936632,-0.488952031482846,
6.33263966472036)) ;
#76677 = CARTESIAN_POINT('Ctrl Pts',(-1.19930907268144,-0.490123758409715,
6.33357989117064)) ;
#76678 = CARTESIAN_POINT('Ctrl Pts',(-1.20150568184695,-0.491744394553401,
6.3351747366642)) ;
#76679 = CARTESIAN_POINT('Ctrl Pts',(-1.20245370818922,-0.492297942372149,
6.33581763637434)) ;
#76680 = CARTESIAN_POINT('Ctrl Pts',(-1.20346579048344,-0.492729032924015,
6.33645424047249)) ;
#76681 = CARTESIAN_POINT('',(-0.981372199195172,-0.981394101666046,6.16407961983129)) ;
#76682 = CARTESIAN_POINT('Ctrl Pts',(-1.23064526020309,-0.123127494296425,
6.16388000977423)) ;
#76683 = CARTESIAN_POINT('Ctrl Pts',(-1.25250788324639,-0.425166570526641,
6.16390005359003)) ;
#76684 = CARTESIAN_POINT('Ctrl Pts',(-1.16278265791006,-0.736199040603134,
6.1637913874525)) ;
#76685 = CARTESIAN_POINT('Ctrl Pts',(-0.981532123342657,-0.981510743966889,
6.16381096867958)) ;
#76686 = CARTESIAN_POINT('',(-6.49131666398584E-5,-1.5604080583864,6.16377232746739)) ;
#76687 = CARTESIAN_POINT('Ctrl Pts',(-0.981288525738987,-0.981332430047466,
6.16398951297446)) ;
#76688 = CARTESIAN_POINT('Ctrl Pts',(-0.981191603913097,-0.981463607802477,
6.16398952349692)) ;
#76689 = CARTESIAN_POINT('Ctrl Pts',(-0.98109465590878,-0.981594766764438,
6.16398953405623)) ;
#76690 = CARTESIAN_POINT('Ctrl Pts',(-0.74957909382456,-1.29467797482235,
6.16401483138177)) ;
#76691 = CARTESIAN_POINT('Ctrl Pts',(-0.388051709564117,-1.50866049563573,
6.16392411658099)) ;
#76692 = CARTESIAN_POINT('Ctrl Pts',(-2.7475723418453E-5,-1.56012574561803,
6.16393999325065)) ;
#76693 = CARTESIAN_POINT('',(1.22475281344944,-1.22479663701074,6.16355881950494)) ;
#76694 = CARTESIAN_POINT('Origin',(0.31156214245914,-0.314022316645595,6.16355474486492)) ;
#76695 = CARTESIAN_POINT('Origin',(0.0911459276996181,0.210924778456014,6.16345720164817)) ;
#76696 = CARTESIAN_POINT('Ctrl Pts',(1.65743956651353,-0.827659859698077,
6.35)) ;
#76697 = CARTESIAN_POINT('Ctrl Pts',(1.54763021003401,-0.994017007846987,
6.35)) ;
#76698 = CARTESIAN_POINT('Ctrl Pts',(1.41133914355359,-1.14150067400533,6.35)) ;
#76699 = CARTESIAN_POINT('Ctrl Pts',(0.904747301883336,-1.54147413813279,
6.35)) ;
#76700 = CARTESIAN_POINT('Ctrl Pts',(0.438511695488632,-1.66934430055112,
6.35)) ;
#76701 = CARTESIAN_POINT('Ctrl Pts',(-0.406722817391188,-1.55758641425134,
6.35000000000001)) ;
#76702 = CARTESIAN_POINT('Ctrl Pts',(-0.782404424459881,-1.33614861407856,
6.35)) ;
#76703 = CARTESIAN_POINT('Ctrl Pts',(-1.13178243085231,-0.863467693146003,
6.35000000000001)) ;
#76704 = CARTESIAN_POINT('Ctrl Pts',(-1.20953277971566,-0.691197369173528,
6.35)) ;
#76705 = CARTESIAN_POINT('Ctrl Pts',(-1.25070895267785,-0.510968789729886,
6.35)) ;
#76706 = CARTESIAN_POINT('Ctrl Pts',(0.,4.49979483821861,1.58609367936188)) ;
#76707 = CARTESIAN_POINT('Ctrl Pts',(-1.8638760498866,4.49979483821861,1.63570305436188)) ;
#76708 = CARTESIAN_POINT('Ctrl Pts',(-3.1818354440526,3.1818354440526,1.68531242936188)) ;
#76709 = CARTESIAN_POINT('Ctrl Pts',(-4.49979483821861,1.8638760498866,1.73492180436188)) ;
#76710 = CARTESIAN_POINT('Ctrl Pts',(-4.49979483821861,2.7553296727221E-16,
1.78453117936188)) ;
#76711 = CARTESIAN_POINT('Ctrl Pts',(-4.49979483821861,-1.8638760498866,1.83414055436188)) ;
#76712 = CARTESIAN_POINT('Ctrl Pts',(-3.1818354440526,-3.1818354440526,1.88374992936188)) ;
#76713 = CARTESIAN_POINT('Ctrl Pts',(-1.8638760498866,-4.49979483821861,1.93335930436188)) ;
#76714 = CARTESIAN_POINT('Ctrl Pts',(-5.5106593454442E-16,-4.49979483821861,
1.98296867936188)) ;
#76715 = CARTESIAN_POINT('Ctrl Pts',(1.86387604988659,-4.49979483821861,2.03257805436188)) ;
#76716 = CARTESIAN_POINT('Ctrl Pts',(3.1818354440526,-3.18183544405261,2.08218742936188)) ;
#76717 = CARTESIAN_POINT('Ctrl Pts',(4.49979483821861,-1.8638760498866,2.13179680436188)) ;
#76718 = CARTESIAN_POINT('Ctrl Pts',(4.49979483821861,-8.2659890181663E-16,
2.18140617936188)) ;
#76719 = CARTESIAN_POINT('Ctrl Pts',(4.49979483821861,1.8638760498866,2.23101555436188)) ;
#76720 = CARTESIAN_POINT('Ctrl Pts',(3.18183544405261,3.1818354440526,2.28062492936188)) ;
#76721 = CARTESIAN_POINT('Ctrl Pts',(1.8638760498866,4.49979483821861,2.33023430436188)) ;
#76722 = CARTESIAN_POINT('Ctrl Pts',(0.,4.49979483821861,2.37984367936188)) ;
#76723 = CARTESIAN_POINT('Ctrl Pts',(-1.8638760498866,4.49979483821861,2.42945305436188)) ;
#76724 = CARTESIAN_POINT('Ctrl Pts',(-3.1818354440526,3.1818354440526,2.47906242936188)) ;
#76725 = CARTESIAN_POINT('Ctrl Pts',(-4.49979483821861,1.8638760498866,2.52867180436188)) ;
#76726 = CARTESIAN_POINT('Ctrl Pts',(-4.49979483821861,2.7553296727221E-16,
2.57828117936188)) ;
#76727 = CARTESIAN_POINT('Ctrl Pts',(-4.49979483821861,-1.8638760498866,2.62789055436188)) ;
#76728 = CARTESIAN_POINT('Ctrl Pts',(-3.1818354440526,-3.1818354440526,2.67749992936188)) ;
#76729 = CARTESIAN_POINT('Ctrl Pts',(-1.8638760498866,-4.49979483821861,2.72710930436188)) ;
#76730 = CARTESIAN_POINT('Ctrl Pts',(-5.5106593454442E-16,-4.49979483821861,
2.77671867936188)) ;
#76731 = CARTESIAN_POINT('Ctrl Pts',(1.86387604988659,-4.49979483821861,2.82632805436188)) ;
#76732 = CARTESIAN_POINT('Ctrl Pts',(3.1818354440526,-3.18183544405261,2.87593742936188)) ;
#76733 = CARTESIAN_POINT('Ctrl Pts',(4.49979483821861,-1.8638760498866,2.92554680436188)) ;
#76734 = CARTESIAN_POINT('Ctrl Pts',(4.49979483821861,-8.2659890181663E-16,
2.97515617936187)) ;
#76735 = CARTESIAN_POINT('Ctrl Pts',(4.49979483821861,1.8638760498866,3.02476555436188)) ;
#76736 = CARTESIAN_POINT('Ctrl Pts',(3.18183544405261,3.1818354440526,3.07437492936188)) ;
#76737 = CARTESIAN_POINT('Ctrl Pts',(1.8638760498866,4.49979483821861,3.12398430436187)) ;
#76738 = CARTESIAN_POINT('Ctrl Pts',(0.,4.49979483821861,3.17359367936188)) ;
#76739 = CARTESIAN_POINT('Ctrl Pts',(-1.8638760498866,4.49979483821861,3.22320305436188)) ;
#76740 = CARTESIAN_POINT('Ctrl Pts',(-3.1818354440526,3.1818354440526,3.27281242936188)) ;
#76741 = CARTESIAN_POINT('Ctrl Pts',(-4.49979483821861,1.8638760498866,3.32242180436188)) ;
#76742 = CARTESIAN_POINT('Ctrl Pts',(-4.49979483821861,2.7553296727221E-16,
3.37203117936187)) ;
#76743 = CARTESIAN_POINT('Ctrl Pts',(-4.49979483821861,-1.8638760498866,3.42164055436188)) ;
#76744 = CARTESIAN_POINT('Ctrl Pts',(-3.1818354440526,-3.1818354440526,3.47124992936188)) ;
#76745 = CARTESIAN_POINT('Ctrl Pts',(-1.8638760498866,-4.49979483821861,3.52085930436187)) ;
#76746 = CARTESIAN_POINT('Ctrl Pts',(-5.5106593454442E-16,-4.49979483821861,
3.57046867936188)) ;
#76747 = CARTESIAN_POINT('Ctrl Pts',(1.86387604988659,-4.49979483821861,3.62007805436187)) ;
#76748 = CARTESIAN_POINT('Ctrl Pts',(3.1818354440526,-3.18183544405261,3.66968742936188)) ;
#76749 = CARTESIAN_POINT('Ctrl Pts',(4.49979483821861,-1.8638760498866,3.71929680436188)) ;
#76750 = CARTESIAN_POINT('Ctrl Pts',(4.49979483821861,-8.2659890181663E-16,
3.76890617936188)) ;
#76751 = CARTESIAN_POINT('Ctrl Pts',(4.49979483821861,1.8638760498866,3.81851555436188)) ;
#76752 = CARTESIAN_POINT('Ctrl Pts',(3.18183544405261,3.1818354440526,3.86812492936188)) ;
#76753 = CARTESIAN_POINT('Ctrl Pts',(1.8638760498866,4.49979483821861,3.91773430436188)) ;
#76754 = CARTESIAN_POINT('Ctrl Pts',(0.,4.49979483821861,3.96734367936188)) ;
#76755 = CARTESIAN_POINT('Ctrl Pts',(-1.8638760498866,4.49979483821861,4.01695305436187)) ;
#76756 = CARTESIAN_POINT('Ctrl Pts',(-3.1818354440526,3.1818354440526,4.06656242936188)) ;
#76757 = CARTESIAN_POINT('Ctrl Pts',(-4.49979483821861,1.8638760498866,4.11617180436188)) ;
#76758 = CARTESIAN_POINT('Ctrl Pts',(-4.49979483821861,2.7553296727221E-16,
4.16578117936188)) ;
#76759 = CARTESIAN_POINT('Ctrl Pts',(-4.49979483821861,-1.8638760498866,4.21539055436187)) ;
#76760 = CARTESIAN_POINT('Ctrl Pts',(-3.1818354440526,-3.1818354440526,4.26499992936188)) ;
#76761 = CARTESIAN_POINT('Ctrl Pts',(-1.8638760498866,-4.49979483821861,4.31460930436188)) ;
#76762 = CARTESIAN_POINT('Ctrl Pts',(-5.5106593454442E-16,-4.49979483821861,
4.36421867936188)) ;
#76763 = CARTESIAN_POINT('Ctrl Pts',(1.86387604988659,-4.49979483821861,4.41382805436188)) ;
#76764 = CARTESIAN_POINT('Ctrl Pts',(3.1818354440526,-3.18183544405261,4.46343742936188)) ;
#76765 = CARTESIAN_POINT('Ctrl Pts',(4.49979483821861,-1.8638760498866,4.51304680436187)) ;
#76766 = CARTESIAN_POINT('Ctrl Pts',(4.49979483821861,-8.2659890181663E-16,
4.56265617936188)) ;
#76767 = CARTESIAN_POINT('Ctrl Pts',(4.49979483821861,1.8638760498866,4.61226555436188)) ;
#76768 = CARTESIAN_POINT('Ctrl Pts',(3.18183544405261,3.1818354440526,4.66187492936188)) ;
#76769 = CARTESIAN_POINT('Ctrl Pts',(1.8638760498866,4.49979483821861,4.71148430436188)) ;
#76770 = CARTESIAN_POINT('Ctrl Pts',(0.,4.49979483821861,4.76109367936188)) ;
#76771 = CARTESIAN_POINT('Ctrl Pts',(-1.8638760498866,4.49979483821861,4.81070305436188)) ;
#76772 = CARTESIAN_POINT('Ctrl Pts',(-3.1818354440526,3.1818354440526,4.86031242936188)) ;
#76773 = CARTESIAN_POINT('Ctrl Pts',(-4.49979483821861,1.8638760498866,4.90992180436188)) ;
#76774 = CARTESIAN_POINT('Ctrl Pts',(-4.49979483821861,2.7553296727221E-16,
4.95953117936188)) ;
#76775 = CARTESIAN_POINT('Ctrl Pts',(-4.49979483821861,-1.8638760498866,5.00914055436187)) ;
#76776 = CARTESIAN_POINT('Ctrl Pts',(-3.1818354440526,-3.1818354440526,5.05874992936188)) ;
#76777 = CARTESIAN_POINT('Ctrl Pts',(-1.8638760498866,-4.49979483821861,5.10835930436188)) ;
#76778 = CARTESIAN_POINT('Ctrl Pts',(-5.5106593454442E-16,-4.49979483821861,
5.15796867936188)) ;
#76779 = CARTESIAN_POINT('Ctrl Pts',(1.86387604988659,-4.49979483821861,5.20757805436187)) ;
#76780 = CARTESIAN_POINT('Ctrl Pts',(3.1818354440526,-3.18183544405261,5.25718742936188)) ;
#76781 = CARTESIAN_POINT('Ctrl Pts',(4.49979483821861,-1.8638760498866,5.30679680436188)) ;
#76782 = CARTESIAN_POINT('Ctrl Pts',(4.49979483821861,-8.2659890181663E-16,
5.35640617936188)) ;
#76783 = CARTESIAN_POINT('Ctrl Pts',(4.49979483821861,1.8638760498866,5.40601555436188)) ;
#76784 = CARTESIAN_POINT('Ctrl Pts',(3.18183544405261,3.1818354440526,5.45562492936187)) ;
#76785 = CARTESIAN_POINT('Ctrl Pts',(1.8638760498866,4.49979483821861,5.50523430436188)) ;
#76786 = CARTESIAN_POINT('Ctrl Pts',(0.,4.49979483821861,5.55484367936188)) ;
#76787 = CARTESIAN_POINT('Ctrl Pts',(-1.8638760498866,4.49979483821861,5.60445305436188)) ;
#76788 = CARTESIAN_POINT('Ctrl Pts',(-3.1818354440526,3.1818354440526,5.65406242936188)) ;
#76789 = CARTESIAN_POINT('Ctrl Pts',(-4.49979483821861,1.8638760498866,5.70367180436188)) ;
#76790 = CARTESIAN_POINT('Ctrl Pts',(-4.49979483821861,2.7553296727221E-16,
5.75328117936188)) ;
#76791 = CARTESIAN_POINT('Ctrl Pts',(-4.49979483821861,-1.8638760498866,5.80289055436188)) ;
#76792 = CARTESIAN_POINT('Ctrl Pts',(-3.1818354440526,-3.1818354440526,5.85249992936188)) ;
#76793 = CARTESIAN_POINT('Ctrl Pts',(-1.8638760498866,-4.49979483821861,5.90210930436188)) ;
#76794 = CARTESIAN_POINT('Ctrl Pts',(-5.5106593454442E-16,-4.49979483821861,
5.95171867936188)) ;
#76795 = CARTESIAN_POINT('Ctrl Pts',(1.86387604988659,-4.49979483821861,6.00132805436188)) ;
#76796 = CARTESIAN_POINT('Ctrl Pts',(3.1818354440526,-3.18183544405261,6.05093742936188)) ;
#76797 = CARTESIAN_POINT('Ctrl Pts',(4.49979483821861,-1.8638760498866,6.10054680436188)) ;
#76798 = CARTESIAN_POINT('Ctrl Pts',(4.49979483821861,-8.2659890181663E-16,
6.15015617936188)) ;
#76799 = CARTESIAN_POINT('Ctrl Pts',(4.49979483821861,1.8638760498866,6.19976555436188)) ;
#76800 = CARTESIAN_POINT('Ctrl Pts',(3.18183544405261,3.1818354440526,6.24937492936188)) ;
#76801 = CARTESIAN_POINT('Ctrl Pts',(1.8638760498866,4.49979483821861,6.29898430436187)) ;
#76802 = CARTESIAN_POINT('Ctrl Pts',(0.,4.49979483821861,6.34859367936188)) ;
#76803 = CARTESIAN_POINT('Ctrl Pts',(-1.8638760498866,4.49979483821861,6.39820305436188)) ;
#76804 = CARTESIAN_POINT('Ctrl Pts',(-3.1818354440526,3.1818354440526,6.44781242936188)) ;
#76805 = CARTESIAN_POINT('Ctrl Pts',(-4.49979483821861,1.8638760498866,6.49742180436188)) ;
#76806 = CARTESIAN_POINT('Ctrl Pts',(-4.49979483821861,2.7553296727221E-16,
6.54703117936188)) ;
#76807 = CARTESIAN_POINT('Ctrl Pts',(-4.49979483821861,-1.8638760498866,6.59664055436189)) ;
#76808 = CARTESIAN_POINT('Ctrl Pts',(-3.1818354440526,-3.1818354440526,6.64624992936188)) ;
#76809 = CARTESIAN_POINT('Ctrl Pts',(-1.8638760498866,-4.49979483821861,6.69585930436188)) ;
#76810 = CARTESIAN_POINT('Ctrl Pts',(-5.5106593454442E-16,-4.49979483821861,
6.74546867936188)) ;
#76811 = CARTESIAN_POINT('Ctrl Pts',(1.86387604988659,-4.49979483821861,6.79507805436187)) ;
#76812 = CARTESIAN_POINT('Ctrl Pts',(3.1818354440526,-3.18183544405261,6.84468742936188)) ;
#76813 = CARTESIAN_POINT('Ctrl Pts',(4.49979483821861,-1.8638760498866,6.89429680436188)) ;
#76814 = CARTESIAN_POINT('Ctrl Pts',(4.49979483821861,-8.2659890181663E-16,
6.94390617936188)) ;
#76815 = CARTESIAN_POINT('Ctrl Pts',(4.49979483821861,1.8638760498866,6.99351555436188)) ;
#76816 = CARTESIAN_POINT('Ctrl Pts',(3.18183544405261,3.1818354440526,7.04312492936188)) ;
#76817 = CARTESIAN_POINT('Ctrl Pts',(1.8638760498866,4.49979483821861,7.09273430436188)) ;
#76818 = CARTESIAN_POINT('Ctrl Pts',(0.,4.49979483821861,7.14234367936188)) ;
#76819 = CARTESIAN_POINT('Ctrl Pts',(-1.8638760498866,4.49979483821861,7.19195305436187)) ;
#76820 = CARTESIAN_POINT('Ctrl Pts',(-3.1818354440526,3.1818354440526,7.24156242936188)) ;
#76821 = CARTESIAN_POINT('Ctrl Pts',(-4.49979483821861,1.8638760498866,7.29117180436188)) ;
#76822 = CARTESIAN_POINT('Ctrl Pts',(-4.49979483821861,2.7553296727221E-16,
7.34078117936187)) ;
#76823 = CARTESIAN_POINT('Ctrl Pts',(-4.49979483821861,-1.8638760498866,7.39039055436188)) ;
#76824 = CARTESIAN_POINT('Ctrl Pts',(-3.1818354440526,-3.1818354440526,7.43999992936188)) ;
#76825 = CARTESIAN_POINT('Ctrl Pts',(-1.8638760498866,-4.49979483821861,7.48960930436188)) ;
#76826 = CARTESIAN_POINT('Ctrl Pts',(-5.5106593454442E-16,-4.49979483821861,
7.53921867936188)) ;
#76827 = CARTESIAN_POINT('Ctrl Pts',(1.86387604988659,-4.49979483821861,7.58882805436189)) ;
#76828 = CARTESIAN_POINT('Ctrl Pts',(3.1818354440526,-3.18183544405261,7.63843742936188)) ;
#76829 = CARTESIAN_POINT('Ctrl Pts',(4.49979483821861,-1.8638760498866,7.68804680436188)) ;
#76830 = CARTESIAN_POINT('Ctrl Pts',(4.49979483821861,-8.2659890181663E-16,
7.73765617936188)) ;
#76831 = CARTESIAN_POINT('Ctrl Pts',(4.49979483821861,1.8638760498866,7.78726555436187)) ;
#76832 = CARTESIAN_POINT('Ctrl Pts',(3.18183544405261,3.1818354440526,7.83687492936187)) ;
#76833 = CARTESIAN_POINT('Ctrl Pts',(1.8638760498866,4.49979483821861,7.88648430436188)) ;
#76834 = CARTESIAN_POINT('Ctrl Pts',(0.,4.49979483821861,7.93609367936188)) ;
#76835 = CARTESIAN_POINT('Ctrl Pts',(-1.8638760498866,4.49979483821861,7.98570305436189)) ;
#76836 = CARTESIAN_POINT('Ctrl Pts',(-3.1818354440526,3.1818354440526,8.03531242936188)) ;
#76837 = CARTESIAN_POINT('Ctrl Pts',(-4.49979483821861,1.8638760498866,8.08492180436188)) ;
#76838 = CARTESIAN_POINT('Ctrl Pts',(-4.49979483821861,2.7553296727221E-16,
8.13453117936188)) ;
#76839 = CARTESIAN_POINT('Ctrl Pts',(-4.49979483821861,-1.8638760498866,8.18414055436188)) ;
#76840 = CARTESIAN_POINT('Ctrl Pts',(-3.1818354440526,-3.1818354440526,8.23374992936188)) ;
#76841 = CARTESIAN_POINT('Ctrl Pts',(-1.8638760498866,-4.49979483821861,8.28335930436188)) ;
#76842 = CARTESIAN_POINT('Ctrl Pts',(-5.5106593454442E-16,-4.49979483821861,
8.33296867936188)) ;
#76843 = CARTESIAN_POINT('Ctrl Pts',(1.86387604988659,-4.49979483821861,8.38257805436188)) ;
#76844 = CARTESIAN_POINT('Ctrl Pts',(3.1818354440526,-3.18183544405261,8.43218742936187)) ;
#76845 = CARTESIAN_POINT('Ctrl Pts',(4.49979483821861,-1.8638760498866,8.48179680436188)) ;
#76846 = CARTESIAN_POINT('Ctrl Pts',(4.49979483821861,-8.2659890181663E-16,
8.53140617936188)) ;
#76847 = CARTESIAN_POINT('Ctrl Pts',(4.49979483821861,1.8638760498866,8.58101555436188)) ;
#76848 = CARTESIAN_POINT('Ctrl Pts',(3.18183544405261,3.1818354440526,8.63062492936188)) ;
#76849 = CARTESIAN_POINT('Ctrl Pts',(1.8638760498866,4.49979483821861,8.68023430436188)) ;
#76850 = CARTESIAN_POINT('Ctrl Pts',(0.,4.49979483821861,8.72984367936187)) ;
#76851 = CARTESIAN_POINT('Ctrl Pts',(0.,1.7526,-1.0842021724855E-16)) ;
#76852 = CARTESIAN_POINT('Ctrl Pts',(-0.725950689415087,1.7526,0.0496093749999999)) ;
#76853 = CARTESIAN_POINT('Ctrl Pts',(-1.23927534470754,1.23927534470754,0.0992187499999999)) ;
#76854 = CARTESIAN_POINT('Ctrl Pts',(-1.7526,0.725950689415087,0.148828125)) ;
#76855 = CARTESIAN_POINT('Ctrl Pts',(-1.7526,1.07315799009283E-16,0.1984375)) ;
#76856 = CARTESIAN_POINT('Ctrl Pts',(-1.7526,-0.725950689415086,0.248046875)) ;
#76857 = CARTESIAN_POINT('Ctrl Pts',(-1.23927534470754,-1.23927534470754,
0.29765625)) ;
#76858 = CARTESIAN_POINT('Ctrl Pts',(-0.725950689415087,-1.7526,0.347265625)) ;
#76859 = CARTESIAN_POINT('Ctrl Pts',(-2.14631598018565E-16,-1.7526,0.396875)) ;
#76860 = CARTESIAN_POINT('Ctrl Pts',(0.725950689415086,-1.7526,0.446484375)) ;
#76861 = CARTESIAN_POINT('Ctrl Pts',(1.23927534470754,-1.23927534470754,0.49609375)) ;
#76862 = CARTESIAN_POINT('Ctrl Pts',(1.7526,-0.725950689415087,0.545703125)) ;
#76863 = CARTESIAN_POINT('Ctrl Pts',(1.7526,-3.21947397027848E-16,0.5953125)) ;
#76864 = CARTESIAN_POINT('Ctrl Pts',(1.7526,0.725950689415087,0.644921875)) ;
#76865 = CARTESIAN_POINT('Ctrl Pts',(1.23927534470754,1.23927534470754,0.69453125)) ;
#76866 = CARTESIAN_POINT('Ctrl Pts',(0.725950689415088,1.7526,0.744140625)) ;
#76867 = CARTESIAN_POINT('Ctrl Pts',(0.,1.7526,0.79375)) ;
#76868 = CARTESIAN_POINT('Ctrl Pts',(-0.725950689415087,1.7526,0.843359375)) ;
#76869 = CARTESIAN_POINT('Ctrl Pts',(-1.23927534470754,1.23927534470754,0.89296875)) ;
#76870 = CARTESIAN_POINT('Ctrl Pts',(-1.7526,0.725950689415087,0.942578125)) ;
#76871 = CARTESIAN_POINT('Ctrl Pts',(-1.7526,1.07315799009283E-16,0.9921875)) ;
#76872 = CARTESIAN_POINT('Ctrl Pts',(-1.7526,-0.725950689415086,1.041796875)) ;
#76873 = CARTESIAN_POINT('Ctrl Pts',(-1.23927534470754,-1.23927534470754,
1.09140625)) ;
#76874 = CARTESIAN_POINT('Ctrl Pts',(-0.725950689415087,-1.7526,1.141015625)) ;
#76875 = CARTESIAN_POINT('Ctrl Pts',(-2.14631598018565E-16,-1.7526,1.190625)) ;
#76876 = CARTESIAN_POINT('Ctrl Pts',(0.725950689415086,-1.7526,1.240234375)) ;
#76877 = CARTESIAN_POINT('Ctrl Pts',(1.23927534470754,-1.23927534470754,1.28984375)) ;
#76878 = CARTESIAN_POINT('Ctrl Pts',(1.7526,-0.725950689415087,1.339453125)) ;
#76879 = CARTESIAN_POINT('Ctrl Pts',(1.7526,-3.21947397027848E-16,1.3890625)) ;
#76880 = CARTESIAN_POINT('Ctrl Pts',(1.7526,0.725950689415087,1.438671875)) ;
#76881 = CARTESIAN_POINT('Ctrl Pts',(1.23927534470754,1.23927534470754,1.48828125)) ;
#76882 = CARTESIAN_POINT('Ctrl Pts',(0.725950689415088,1.7526,1.537890625)) ;
#76883 = CARTESIAN_POINT('Ctrl Pts',(0.,1.7526,1.5875)) ;
#76884 = CARTESIAN_POINT('Ctrl Pts',(-0.725950689415087,1.7526,1.637109375)) ;
#76885 = CARTESIAN_POINT('Ctrl Pts',(-1.23927534470754,1.23927534470754,1.68671875)) ;
#76886 = CARTESIAN_POINT('Ctrl Pts',(-1.7526,0.725950689415087,1.736328125)) ;
#76887 = CARTESIAN_POINT('Ctrl Pts',(-1.7526,1.07315799009283E-16,1.7859375)) ;
#76888 = CARTESIAN_POINT('Ctrl Pts',(-1.7526,-0.725950689415086,1.835546875)) ;
#76889 = CARTESIAN_POINT('Ctrl Pts',(-1.23927534470754,-1.23927534470754,
1.88515625)) ;
#76890 = CARTESIAN_POINT('Ctrl Pts',(-0.725950689415087,-1.7526,1.934765625)) ;
#76891 = CARTESIAN_POINT('Ctrl Pts',(-2.14631598018565E-16,-1.7526,1.984375)) ;
#76892 = CARTESIAN_POINT('Ctrl Pts',(0.725950689415086,-1.7526,2.033984375)) ;
#76893 = CARTESIAN_POINT('Ctrl Pts',(1.23927534470754,-1.23927534470754,2.08359375)) ;
#76894 = CARTESIAN_POINT('Ctrl Pts',(1.7526,-0.725950689415087,2.133203125)) ;
#76895 = CARTESIAN_POINT('Ctrl Pts',(1.7526,-3.21947397027848E-16,2.1828125)) ;
#76896 = CARTESIAN_POINT('Ctrl Pts',(1.7526,0.725950689415087,2.232421875)) ;
#76897 = CARTESIAN_POINT('Ctrl Pts',(1.23927534470754,1.23927534470754,2.28203125)) ;
#76898 = CARTESIAN_POINT('Ctrl Pts',(0.725950689415088,1.7526,2.331640625)) ;
#76899 = CARTESIAN_POINT('Ctrl Pts',(0.,1.7526,2.38125)) ;
#76900 = CARTESIAN_POINT('Ctrl Pts',(-0.725950689415087,1.7526,2.430859375)) ;
#76901 = CARTESIAN_POINT('Ctrl Pts',(-1.23927534470754,1.23927534470754,2.48046875)) ;
#76902 = CARTESIAN_POINT('Ctrl Pts',(-1.7526,0.725950689415087,2.530078125)) ;
#76903 = CARTESIAN_POINT('Ctrl Pts',(-1.7526,1.07315799009283E-16,2.5796875)) ;
#76904 = CARTESIAN_POINT('Ctrl Pts',(-1.7526,-0.725950689415086,2.629296875)) ;
#76905 = CARTESIAN_POINT('Ctrl Pts',(-1.23927534470754,-1.23927534470754,
2.67890625)) ;
#76906 = CARTESIAN_POINT('Ctrl Pts',(-0.725950689415087,-1.7526,2.728515625)) ;
#76907 = CARTESIAN_POINT('Ctrl Pts',(-2.14631598018565E-16,-1.7526,2.778125)) ;
#76908 = CARTESIAN_POINT('Ctrl Pts',(0.725950689415086,-1.7526,2.827734375)) ;
#76909 = CARTESIAN_POINT('Ctrl Pts',(1.23927534470754,-1.23927534470754,2.87734375)) ;
#76910 = CARTESIAN_POINT('Ctrl Pts',(1.7526,-0.725950689415087,2.926953125)) ;
#76911 = CARTESIAN_POINT('Ctrl Pts',(1.7526,-3.21947397027848E-16,2.9765625)) ;
#76912 = CARTESIAN_POINT('Ctrl Pts',(1.7526,0.725950689415087,3.026171875)) ;
#76913 = CARTESIAN_POINT('Ctrl Pts',(1.23927534470754,1.23927534470754,3.07578125)) ;
#76914 = CARTESIAN_POINT('Ctrl Pts',(0.725950689415088,1.7526,3.125390625)) ;
#76915 = CARTESIAN_POINT('Ctrl Pts',(0.,1.7526,3.175)) ;
#76916 = CARTESIAN_POINT('Ctrl Pts',(-0.725950689415087,1.7526,3.224609375)) ;
#76917 = CARTESIAN_POINT('Ctrl Pts',(-1.23927534470754,1.23927534470754,3.27421875)) ;
#76918 = CARTESIAN_POINT('Ctrl Pts',(-1.7526,0.725950689415087,3.323828125)) ;
#76919 = CARTESIAN_POINT('Ctrl Pts',(-1.7526,1.07315799009283E-16,3.3734375)) ;
#76920 = CARTESIAN_POINT('Ctrl Pts',(-1.7526,-0.725950689415086,3.423046875)) ;
#76921 = CARTESIAN_POINT('Ctrl Pts',(-1.23927534470754,-1.23927534470754,
3.47265625)) ;
#76922 = CARTESIAN_POINT('Ctrl Pts',(-0.725950689415087,-1.7526,3.522265625)) ;
#76923 = CARTESIAN_POINT('Ctrl Pts',(-2.14631598018565E-16,-1.7526,3.571875)) ;
#76924 = CARTESIAN_POINT('Ctrl Pts',(0.725950689415086,-1.7526,3.621484375)) ;
#76925 = CARTESIAN_POINT('Ctrl Pts',(1.23927534470754,-1.23927534470754,3.67109375)) ;
#76926 = CARTESIAN_POINT('Ctrl Pts',(1.7526,-0.725950689415087,3.720703125)) ;
#76927 = CARTESIAN_POINT('Ctrl Pts',(1.7526,-3.21947397027848E-16,3.7703125)) ;
#76928 = CARTESIAN_POINT('Ctrl Pts',(1.7526,0.725950689415087,3.819921875)) ;
#76929 = CARTESIAN_POINT('Ctrl Pts',(1.23927534470754,1.23927534470754,3.86953125)) ;
#76930 = CARTESIAN_POINT('Ctrl Pts',(0.725950689415088,1.7526,3.919140625)) ;
#76931 = CARTESIAN_POINT('Ctrl Pts',(0.,1.7526,3.96875)) ;
#76932 = CARTESIAN_POINT('Ctrl Pts',(-0.725950689415087,1.7526,4.018359375)) ;
#76933 = CARTESIAN_POINT('Ctrl Pts',(-1.23927534470754,1.23927534470754,4.06796875)) ;
#76934 = CARTESIAN_POINT('Ctrl Pts',(-1.7526,0.725950689415087,4.117578125)) ;
#76935 = CARTESIAN_POINT('Ctrl Pts',(-1.7526,1.07315799009283E-16,4.1671875)) ;
#76936 = CARTESIAN_POINT('Ctrl Pts',(-1.7526,-0.725950689415086,4.216796875)) ;
#76937 = CARTESIAN_POINT('Ctrl Pts',(-1.23927534470754,-1.23927534470754,
4.26640625)) ;
#76938 = CARTESIAN_POINT('Ctrl Pts',(-0.725950689415087,-1.7526,4.316015625)) ;
#76939 = CARTESIAN_POINT('Ctrl Pts',(-2.14631598018565E-16,-1.7526,4.365625)) ;
#76940 = CARTESIAN_POINT('Ctrl Pts',(0.725950689415086,-1.7526,4.415234375)) ;
#76941 = CARTESIAN_POINT('Ctrl Pts',(1.23927534470754,-1.23927534470754,4.46484375)) ;
#76942 = CARTESIAN_POINT('Ctrl Pts',(1.7526,-0.725950689415087,4.514453125)) ;
#76943 = CARTESIAN_POINT('Ctrl Pts',(1.7526,-3.21947397027848E-16,4.5640625)) ;
#76944 = CARTESIAN_POINT('Ctrl Pts',(1.7526,0.725950689415087,4.613671875)) ;
#76945 = CARTESIAN_POINT('Ctrl Pts',(1.23927534470754,1.23927534470754,4.66328125)) ;
#76946 = CARTESIAN_POINT('Ctrl Pts',(0.725950689415088,1.7526,4.712890625)) ;
#76947 = CARTESIAN_POINT('Ctrl Pts',(0.,1.7526,4.7625)) ;
#76948 = CARTESIAN_POINT('Ctrl Pts',(-0.725950689415087,1.7526,4.812109375)) ;
#76949 = CARTESIAN_POINT('Ctrl Pts',(-1.23927534470754,1.23927534470754,4.86171875)) ;
#76950 = CARTESIAN_POINT('Ctrl Pts',(-1.7526,0.725950689415087,4.911328125)) ;
#76951 = CARTESIAN_POINT('Ctrl Pts',(-1.7526,1.07315799009283E-16,4.9609375)) ;
#76952 = CARTESIAN_POINT('Ctrl Pts',(-1.7526,-0.725950689415086,5.010546875)) ;
#76953 = CARTESIAN_POINT('Ctrl Pts',(-1.23927534470754,-1.23927534470754,
5.06015625)) ;
#76954 = CARTESIAN_POINT('Ctrl Pts',(-0.725950689415087,-1.7526,5.109765625)) ;
#76955 = CARTESIAN_POINT('Ctrl Pts',(-2.14631598018565E-16,-1.7526,5.159375)) ;
#76956 = CARTESIAN_POINT('Ctrl Pts',(0.725950689415086,-1.7526,5.208984375)) ;
#76957 = CARTESIAN_POINT('Ctrl Pts',(1.23927534470754,-1.23927534470754,5.25859375)) ;
#76958 = CARTESIAN_POINT('Ctrl Pts',(1.7526,-0.725950689415087,5.308203125)) ;
#76959 = CARTESIAN_POINT('Ctrl Pts',(1.7526,-3.21947397027848E-16,5.3578125)) ;
#76960 = CARTESIAN_POINT('Ctrl Pts',(1.7526,0.725950689415087,5.407421875)) ;
#76961 = CARTESIAN_POINT('Ctrl Pts',(1.23927534470754,1.23927534470754,5.45703125)) ;
#76962 = CARTESIAN_POINT('Ctrl Pts',(0.725950689415088,1.7526,5.506640625)) ;
#76963 = CARTESIAN_POINT('Ctrl Pts',(0.,1.7526,5.55625)) ;
#76964 = CARTESIAN_POINT('Ctrl Pts',(-0.725950689415087,1.7526,5.605859375)) ;
#76965 = CARTESIAN_POINT('Ctrl Pts',(-1.23927534470754,1.23927534470754,5.65546875)) ;
#76966 = CARTESIAN_POINT('Ctrl Pts',(-1.7526,0.725950689415087,5.705078125)) ;
#76967 = CARTESIAN_POINT('Ctrl Pts',(-1.7526,1.07315799009283E-16,5.7546875)) ;
#76968 = CARTESIAN_POINT('Ctrl Pts',(-1.7526,-0.725950689415086,5.804296875)) ;
#76969 = CARTESIAN_POINT('Ctrl Pts',(-1.23927534470754,-1.23927534470754,
5.85390625)) ;
#76970 = CARTESIAN_POINT('Ctrl Pts',(-0.725950689415087,-1.7526,5.903515625)) ;
#76971 = CARTESIAN_POINT('Ctrl Pts',(-2.14631598018565E-16,-1.7526,5.953125)) ;
#76972 = CARTESIAN_POINT('Ctrl Pts',(0.725950689415086,-1.7526,6.002734375)) ;
#76973 = CARTESIAN_POINT('Ctrl Pts',(1.23927534470754,-1.23927534470754,6.05234375)) ;
#76974 = CARTESIAN_POINT('Ctrl Pts',(1.7526,-0.725950689415087,6.101953125)) ;
#76975 = CARTESIAN_POINT('Ctrl Pts',(1.7526,-3.21947397027848E-16,6.1515625)) ;
#76976 = CARTESIAN_POINT('Ctrl Pts',(1.7526,0.725950689415087,6.201171875)) ;
#76977 = CARTESIAN_POINT('Ctrl Pts',(1.23927534470754,1.23927534470754,6.25078125)) ;
#76978 = CARTESIAN_POINT('Ctrl Pts',(0.725950689415088,1.7526,6.300390625)) ;
#76979 = CARTESIAN_POINT('Ctrl Pts',(0.,1.7526,6.35)) ;
#76980 = CARTESIAN_POINT('Ctrl Pts',(-0.725950689415087,1.7526,6.399609375)) ;
#76981 = CARTESIAN_POINT('Ctrl Pts',(-1.23927534470754,1.23927534470754,6.44921875)) ;
#76982 = CARTESIAN_POINT('Ctrl Pts',(-1.7526,0.725950689415087,6.498828125)) ;
#76983 = CARTESIAN_POINT('Ctrl Pts',(-1.7526,1.07315799009283E-16,6.5484375)) ;
#76984 = CARTESIAN_POINT('Ctrl Pts',(-1.7526,-0.725950689415086,6.598046875)) ;
#76985 = CARTESIAN_POINT('Ctrl Pts',(-1.23927534470754,-1.23927534470754,
6.64765625)) ;
#76986 = CARTESIAN_POINT('Ctrl Pts',(-0.725950689415087,-1.7526,6.697265625)) ;
#76987 = CARTESIAN_POINT('Ctrl Pts',(-2.14631598018565E-16,-1.7526,6.746875)) ;
#76988 = CARTESIAN_POINT('Ctrl Pts',(0.725950689415086,-1.7526,6.796484375)) ;
#76989 = CARTESIAN_POINT('Ctrl Pts',(1.23927534470754,-1.23927534470754,6.84609375)) ;
#76990 = CARTESIAN_POINT('Ctrl Pts',(1.7526,-0.725950689415087,6.895703125)) ;
#76991 = CARTESIAN_POINT('Ctrl Pts',(1.7526,-3.21947397027848E-16,6.9453125)) ;
#76992 = CARTESIAN_POINT('Ctrl Pts',(1.7526,0.725950689415087,6.994921875)) ;
#76993 = CARTESIAN_POINT('Ctrl Pts',(1.23927534470754,1.23927534470754,7.04453125)) ;
#76994 = CARTESIAN_POINT('Ctrl Pts',(0.725950689415088,1.7526,7.094140625)) ;
#76995 = CARTESIAN_POINT('Ctrl Pts',(0.,1.7526,7.14375)) ;
#76996 = CARTESIAN_POINT('Ctrl Pts',(0.,1.23704425180958,-0.297656250000002)) ;
#76997 = CARTESIAN_POINT('Ctrl Pts',(-0.512400506355205,1.23704425180958,
-0.248046875000002)) ;
#76998 = CARTESIAN_POINT('Ctrl Pts',(-0.874722379082391,0.874722379082391,
-0.198437500000002)) ;
#76999 = CARTESIAN_POINT('Ctrl Pts',(-1.23704425180958,0.512400506355205,
-0.148828125000002)) ;
#77000 = CARTESIAN_POINT('Ctrl Pts',(-1.23704425180958,7.57471141691116E-17,
-0.0992187500000015)) ;
#77001 = CARTESIAN_POINT('Ctrl Pts',(-1.23704425180958,-0.512400506355205,
-0.0496093750000015)) ;
#77002 = CARTESIAN_POINT('Ctrl Pts',(-0.874722379082391,-0.874722379082391,
-1.57209315010398E-15)) ;
#77003 = CARTESIAN_POINT('Ctrl Pts',(-0.512400506355205,-1.23704425180958,
0.0496093749999984)) ;
#77004 = CARTESIAN_POINT('Ctrl Pts',(-1.51494228338223E-16,-1.23704425180958,
0.0992187499999985)) ;
#77005 = CARTESIAN_POINT('Ctrl Pts',(0.512400506355205,-1.23704425180958,
0.148828124999998)) ;
#77006 = CARTESIAN_POINT('Ctrl Pts',(0.874722379082391,-0.874722379082391,
0.198437499999998)) ;
#77007 = CARTESIAN_POINT('Ctrl Pts',(1.23704425180958,-0.512400506355206,
0.248046874999998)) ;
#77008 = CARTESIAN_POINT('Ctrl Pts',(1.23704425180958,-2.27241342507335E-16,
0.297656249999998)) ;
#77009 = CARTESIAN_POINT('Ctrl Pts',(1.23704425180958,0.512400506355206,0.347265624999998)) ;
#77010 = CARTESIAN_POINT('Ctrl Pts',(0.874722379082391,0.874722379082391,
0.396874999999998)) ;
#77011 = CARTESIAN_POINT('Ctrl Pts',(0.512400506355206,1.23704425180958,0.446484374999998)) ;
#77012 = CARTESIAN_POINT('Ctrl Pts',(0.,1.23704425180958,0.496093749999999)) ;
#77013 = CARTESIAN_POINT('Ctrl Pts',(-0.512400506355205,1.23704425180958,
0.545703124999998)) ;
#77014 = CARTESIAN_POINT('Ctrl Pts',(-0.874722379082391,0.874722379082391,
0.595312499999998)) ;
#77015 = CARTESIAN_POINT('Ctrl Pts',(-1.23704425180958,0.512400506355205,
0.644921874999998)) ;
#77016 = CARTESIAN_POINT('Ctrl Pts',(-1.23704425180958,7.57471141691116E-17,
0.694531249999999)) ;
#77017 = CARTESIAN_POINT('Ctrl Pts',(-1.23704425180958,-0.512400506355205,
0.744140624999998)) ;
#77018 = CARTESIAN_POINT('Ctrl Pts',(-0.874722379082391,-0.874722379082391,
0.793749999999999)) ;
#77019 = CARTESIAN_POINT('Ctrl Pts',(-0.512400506355205,-1.23704425180958,
0.843359374999998)) ;
#77020 = CARTESIAN_POINT('Ctrl Pts',(-1.51494228338223E-16,-1.23704425180958,
0.892968749999998)) ;
#77021 = CARTESIAN_POINT('Ctrl Pts',(0.512400506355205,-1.23704425180958,
0.942578124999999)) ;
#77022 = CARTESIAN_POINT('Ctrl Pts',(0.874722379082391,-0.874722379082391,
0.992187499999999)) ;
#77023 = CARTESIAN_POINT('Ctrl Pts',(1.23704425180958,-0.512400506355206,
1.041796875)) ;
#77024 = CARTESIAN_POINT('Ctrl Pts',(1.23704425180958,-2.27241342507335E-16,
1.09140625)) ;
#77025 = CARTESIAN_POINT('Ctrl Pts',(1.23704425180958,0.512400506355206,1.141015625)) ;
#77026 = CARTESIAN_POINT('Ctrl Pts',(0.874722379082391,0.874722379082391,
1.190625)) ;
#77027 = CARTESIAN_POINT('Ctrl Pts',(0.512400506355206,1.23704425180958,1.240234375)) ;
#77028 = CARTESIAN_POINT('Ctrl Pts',(0.,1.23704425180958,1.28984375)) ;
#77029 = CARTESIAN_POINT('Ctrl Pts',(-0.512400506355205,1.23704425180958,
1.339453125)) ;
#77030 = CARTESIAN_POINT('Ctrl Pts',(-0.874722379082391,0.874722379082391,
1.3890625)) ;
#77031 = CARTESIAN_POINT('Ctrl Pts',(-1.23704425180958,0.512400506355205,
1.438671875)) ;
#77032 = CARTESIAN_POINT('Ctrl Pts',(-1.23704425180958,7.57471141691116E-17,
1.48828125)) ;
#77033 = CARTESIAN_POINT('Ctrl Pts',(-1.23704425180958,-0.512400506355205,
1.537890625)) ;
#77034 = CARTESIAN_POINT('Ctrl Pts',(-0.874722379082391,-0.874722379082391,
1.5875)) ;
#77035 = CARTESIAN_POINT('Ctrl Pts',(-0.512400506355205,-1.23704425180958,
1.637109375)) ;
#77036 = CARTESIAN_POINT('Ctrl Pts',(-1.51494228338223E-16,-1.23704425180958,
1.68671875)) ;
#77037 = CARTESIAN_POINT('Ctrl Pts',(0.512400506355205,-1.23704425180958,
1.736328125)) ;
#77038 = CARTESIAN_POINT('Ctrl Pts',(0.874722379082391,-0.874722379082391,
1.7859375)) ;
#77039 = CARTESIAN_POINT('Ctrl Pts',(1.23704425180958,-0.512400506355206,
1.835546875)) ;
#77040 = CARTESIAN_POINT('Ctrl Pts',(1.23704425180958,-2.27241342507335E-16,
1.88515625)) ;
#77041 = CARTESIAN_POINT('Ctrl Pts',(1.23704425180958,0.512400506355206,1.934765625)) ;
#77042 = CARTESIAN_POINT('Ctrl Pts',(0.874722379082391,0.874722379082391,
1.984375)) ;
#77043 = CARTESIAN_POINT('Ctrl Pts',(0.512400506355206,1.23704425180958,2.033984375)) ;
#77044 = CARTESIAN_POINT('Ctrl Pts',(0.,1.23704425180958,2.08359375)) ;
#77045 = CARTESIAN_POINT('Ctrl Pts',(-0.512400506355205,1.23704425180958,
2.133203125)) ;
#77046 = CARTESIAN_POINT('Ctrl Pts',(-0.874722379082391,0.874722379082391,
2.1828125)) ;
#77047 = CARTESIAN_POINT('Ctrl Pts',(-1.23704425180958,0.512400506355205,
2.232421875)) ;
#77048 = CARTESIAN_POINT('Ctrl Pts',(-1.23704425180958,7.57471141691116E-17,
2.28203125)) ;
#77049 = CARTESIAN_POINT('Ctrl Pts',(-1.23704425180958,-0.512400506355205,
2.331640625)) ;
#77050 = CARTESIAN_POINT('Ctrl Pts',(-0.874722379082391,-0.874722379082391,
2.38125)) ;
#77051 = CARTESIAN_POINT('Ctrl Pts',(-0.512400506355205,-1.23704425180958,
2.430859375)) ;
#77052 = CARTESIAN_POINT('Ctrl Pts',(-1.51494228338223E-16,-1.23704425180958,
2.48046875)) ;
#77053 = CARTESIAN_POINT('Ctrl Pts',(0.512400506355205,-1.23704425180958,
2.530078125)) ;
#77054 = CARTESIAN_POINT('Ctrl Pts',(0.874722379082391,-0.874722379082391,
2.5796875)) ;
#77055 = CARTESIAN_POINT('Ctrl Pts',(1.23704425180958,-0.512400506355206,
2.629296875)) ;
#77056 = CARTESIAN_POINT('Ctrl Pts',(1.23704425180958,-2.27241342507335E-16,
2.67890625)) ;
#77057 = CARTESIAN_POINT('Ctrl Pts',(1.23704425180958,0.512400506355206,2.728515625)) ;
#77058 = CARTESIAN_POINT('Ctrl Pts',(0.874722379082391,0.874722379082391,
2.778125)) ;
#77059 = CARTESIAN_POINT('Ctrl Pts',(0.512400506355206,1.23704425180958,2.827734375)) ;
#77060 = CARTESIAN_POINT('Ctrl Pts',(0.,1.23704425180958,2.87734375)) ;
#77061 = CARTESIAN_POINT('Ctrl Pts',(-0.512400506355205,1.23704425180958,
2.926953125)) ;
#77062 = CARTESIAN_POINT('Ctrl Pts',(-0.874722379082391,0.874722379082391,
2.9765625)) ;
#77063 = CARTESIAN_POINT('Ctrl Pts',(-1.23704425180958,0.512400506355205,
3.026171875)) ;
#77064 = CARTESIAN_POINT('Ctrl Pts',(-1.23704425180958,7.57471141691116E-17,
3.07578125)) ;
#77065 = CARTESIAN_POINT('Ctrl Pts',(-1.23704425180958,-0.512400506355205,
3.125390625)) ;
#77066 = CARTESIAN_POINT('Ctrl Pts',(-0.874722379082391,-0.874722379082391,
3.175)) ;
#77067 = CARTESIAN_POINT('Ctrl Pts',(-0.512400506355205,-1.23704425180958,
3.224609375)) ;
#77068 = CARTESIAN_POINT('Ctrl Pts',(-1.51494228338223E-16,-1.23704425180958,
3.27421875)) ;
#77069 = CARTESIAN_POINT('Ctrl Pts',(0.512400506355205,-1.23704425180958,
3.323828125)) ;
#77070 = CARTESIAN_POINT('Ctrl Pts',(0.874722379082391,-0.874722379082391,
3.3734375)) ;
#77071 = CARTESIAN_POINT('Ctrl Pts',(1.23704425180958,-0.512400506355206,
3.423046875)) ;
#77072 = CARTESIAN_POINT('Ctrl Pts',(1.23704425180958,-2.27241342507335E-16,
3.47265625)) ;
#77073 = CARTESIAN_POINT('Ctrl Pts',(1.23704425180958,0.512400506355206,3.522265625)) ;
#77074 = CARTESIAN_POINT('Ctrl Pts',(0.874722379082391,0.874722379082391,
3.571875)) ;
#77075 = CARTESIAN_POINT('Ctrl Pts',(0.512400506355206,1.23704425180958,3.621484375)) ;
#77076 = CARTESIAN_POINT('Ctrl Pts',(0.,1.23704425180958,3.67109375)) ;
#77077 = CARTESIAN_POINT('Ctrl Pts',(-0.512400506355205,1.23704425180958,
3.720703125)) ;
#77078 = CARTESIAN_POINT('Ctrl Pts',(-0.874722379082391,0.874722379082391,
3.7703125)) ;
#77079 = CARTESIAN_POINT('Ctrl Pts',(-1.23704425180958,0.512400506355205,
3.819921875)) ;
#77080 = CARTESIAN_POINT('Ctrl Pts',(-1.23704425180958,7.57471141691116E-17,
3.86953125)) ;
#77081 = CARTESIAN_POINT('Ctrl Pts',(-1.23704425180958,-0.512400506355205,
3.919140625)) ;
#77082 = CARTESIAN_POINT('Ctrl Pts',(-0.874722379082391,-0.874722379082391,
3.96875)) ;
#77083 = CARTESIAN_POINT('Ctrl Pts',(-0.512400506355205,-1.23704425180958,
4.018359375)) ;
#77084 = CARTESIAN_POINT('Ctrl Pts',(-1.51494228338223E-16,-1.23704425180958,
4.06796875)) ;
#77085 = CARTESIAN_POINT('Ctrl Pts',(0.512400506355205,-1.23704425180958,
4.117578125)) ;
#77086 = CARTESIAN_POINT('Ctrl Pts',(0.874722379082391,-0.874722379082391,
4.1671875)) ;
#77087 = CARTESIAN_POINT('Ctrl Pts',(1.23704425180958,-0.512400506355206,
4.216796875)) ;
#77088 = CARTESIAN_POINT('Ctrl Pts',(1.23704425180958,-2.27241342507335E-16,
4.26640625)) ;
#77089 = CARTESIAN_POINT('Ctrl Pts',(1.23704425180958,0.512400506355206,4.316015625)) ;
#77090 = CARTESIAN_POINT('Ctrl Pts',(0.874722379082391,0.874722379082391,
4.365625)) ;
#77091 = CARTESIAN_POINT('Ctrl Pts',(0.512400506355206,1.23704425180958,4.415234375)) ;
#77092 = CARTESIAN_POINT('Ctrl Pts',(0.,1.23704425180958,4.46484375)) ;
#77093 = CARTESIAN_POINT('Ctrl Pts',(-0.512400506355205,1.23704425180958,
4.514453125)) ;
#77094 = CARTESIAN_POINT('Ctrl Pts',(-0.874722379082391,0.874722379082391,
4.5640625)) ;
#77095 = CARTESIAN_POINT('Ctrl Pts',(-1.23704425180958,0.512400506355205,
4.613671875)) ;
#77096 = CARTESIAN_POINT('Ctrl Pts',(-1.23704425180958,7.57471141691116E-17,
4.66328125)) ;
#77097 = CARTESIAN_POINT('Ctrl Pts',(-1.23704425180958,-0.512400506355205,
4.712890625)) ;
#77098 = CARTESIAN_POINT('Ctrl Pts',(-0.874722379082391,-0.874722379082391,
4.7625)) ;
#77099 = CARTESIAN_POINT('Ctrl Pts',(-0.512400506355205,-1.23704425180958,
4.812109375)) ;
#77100 = CARTESIAN_POINT('Ctrl Pts',(-1.51494228338223E-16,-1.23704425180958,
4.86171875)) ;
#77101 = CARTESIAN_POINT('Ctrl Pts',(0.512400506355205,-1.23704425180958,
4.911328125)) ;
#77102 = CARTESIAN_POINT('Ctrl Pts',(0.874722379082391,-0.874722379082391,
4.9609375)) ;
#77103 = CARTESIAN_POINT('Ctrl Pts',(1.23704425180958,-0.512400506355206,
5.010546875)) ;
#77104 = CARTESIAN_POINT('Ctrl Pts',(1.23704425180958,-2.27241342507335E-16,
5.06015625)) ;
#77105 = CARTESIAN_POINT('Ctrl Pts',(1.23704425180958,0.512400506355206,5.109765625)) ;
#77106 = CARTESIAN_POINT('Ctrl Pts',(0.874722379082391,0.874722379082391,
5.159375)) ;
#77107 = CARTESIAN_POINT('Ctrl Pts',(0.512400506355206,1.23704425180958,5.208984375)) ;
#77108 = CARTESIAN_POINT('Ctrl Pts',(0.,1.23704425180958,5.25859375)) ;
#77109 = CARTESIAN_POINT('Ctrl Pts',(-0.512400506355205,1.23704425180958,
5.308203125)) ;
#77110 = CARTESIAN_POINT('Ctrl Pts',(-0.874722379082391,0.874722379082391,
5.3578125)) ;
#77111 = CARTESIAN_POINT('Ctrl Pts',(-1.23704425180958,0.512400506355205,
5.407421875)) ;
#77112 = CARTESIAN_POINT('Ctrl Pts',(-1.23704425180958,7.57471141691116E-17,
5.45703125)) ;
#77113 = CARTESIAN_POINT('Ctrl Pts',(-1.23704425180958,-0.512400506355205,
5.506640625)) ;
#77114 = CARTESIAN_POINT('Ctrl Pts',(-0.874722379082391,-0.874722379082391,
5.55625)) ;
#77115 = CARTESIAN_POINT('Ctrl Pts',(-0.512400506355205,-1.23704425180958,
5.605859375)) ;
#77116 = CARTESIAN_POINT('Ctrl Pts',(-1.51494228338223E-16,-1.23704425180958,
5.65546875)) ;
#77117 = CARTESIAN_POINT('Ctrl Pts',(0.512400506355205,-1.23704425180958,
5.705078125)) ;
#77118 = CARTESIAN_POINT('Ctrl Pts',(0.874722379082391,-0.874722379082391,
5.7546875)) ;
#77119 = CARTESIAN_POINT('Ctrl Pts',(1.23704425180958,-0.512400506355206,
5.804296875)) ;
#77120 = CARTESIAN_POINT('Ctrl Pts',(1.23704425180958,-2.27241342507335E-16,
5.85390625)) ;
#77121 = CARTESIAN_POINT('Ctrl Pts',(1.23704425180958,0.512400506355206,5.903515625)) ;
#77122 = CARTESIAN_POINT('Ctrl Pts',(0.874722379082391,0.874722379082391,
5.953125)) ;
#77123 = CARTESIAN_POINT('Ctrl Pts',(0.512400506355206,1.23704425180958,6.002734375)) ;
#77124 = CARTESIAN_POINT('Ctrl Pts',(0.,1.23704425180958,6.05234375)) ;
#77125 = CARTESIAN_POINT('Ctrl Pts',(-0.512400506355205,1.23704425180958,
6.101953125)) ;
#77126 = CARTESIAN_POINT('Ctrl Pts',(-0.874722379082391,0.874722379082391,
6.1515625)) ;
#77127 = CARTESIAN_POINT('Ctrl Pts',(-1.23704425180958,0.512400506355205,
6.201171875)) ;
#77128 = CARTESIAN_POINT('Ctrl Pts',(-1.23704425180958,7.57471141691116E-17,
6.25078125)) ;
#77129 = CARTESIAN_POINT('Ctrl Pts',(-1.23704425180958,-0.512400506355205,
6.300390625)) ;
#77130 = CARTESIAN_POINT('Ctrl Pts',(-0.874722379082391,-0.874722379082391,
6.35)) ;
#77131 = CARTESIAN_POINT('Ctrl Pts',(-0.512400506355205,-1.23704425180958,
6.399609375)) ;
#77132 = CARTESIAN_POINT('Ctrl Pts',(-1.51494228338223E-16,-1.23704425180958,
6.44921875)) ;
#77133 = CARTESIAN_POINT('Ctrl Pts',(0.512400506355205,-1.23704425180958,
6.498828125)) ;
#77134 = CARTESIAN_POINT('Ctrl Pts',(0.874722379082391,-0.874722379082391,
6.5484375)) ;
#77135 = CARTESIAN_POINT('Ctrl Pts',(1.23704425180958,-0.512400506355206,
6.598046875)) ;
#77136 = CARTESIAN_POINT('Ctrl Pts',(1.23704425180958,-2.27241342507335E-16,
6.64765625)) ;
#77137 = CARTESIAN_POINT('Ctrl Pts',(1.23704425180958,0.512400506355206,6.697265625)) ;
#77138 = CARTESIAN_POINT('Ctrl Pts',(0.874722379082391,0.874722379082391,
6.746875)) ;
#77139 = CARTESIAN_POINT('Ctrl Pts',(0.512400506355206,1.23704425180958,6.796484375)) ;
#77140 = CARTESIAN_POINT('Ctrl Pts',(0.,1.23704425180958,6.84609375)) ;
#77141 = CARTESIAN_POINT('Ctrl Pts',(0.,0.417702301404716,-0.770703545624604)) ;
#77142 = CARTESIAN_POINT('Ctrl Pts',(-0.173017958276288,0.417702301404717,
-0.721094170624604)) ;
#77143 = CARTESIAN_POINT('Ctrl Pts',(-0.295360129840502,0.295360129840502,
-0.671484795624604)) ;
#77144 = CARTESIAN_POINT('Ctrl Pts',(-0.417702301404717,0.173017958276288,
-0.621875420624604)) ;
#77145 = CARTESIAN_POINT('Ctrl Pts',(-0.417702301404716,2.55768893205885E-17,
-0.572266045624604)) ;
#77146 = CARTESIAN_POINT('Ctrl Pts',(-0.417702301404717,-0.173017958276288,
-0.522656670624604)) ;
#77147 = CARTESIAN_POINT('Ctrl Pts',(-0.295360129840502,-0.295360129840502,
-0.473047295624604)) ;
#77148 = CARTESIAN_POINT('Ctrl Pts',(-0.173017958276288,-0.417702301404717,
-0.423437920624604)) ;
#77149 = CARTESIAN_POINT('Ctrl Pts',(-5.1153778641177E-17,-0.417702301404716,
-0.373828545624604)) ;
#77150 = CARTESIAN_POINT('Ctrl Pts',(0.173017958276288,-0.417702301404716,
-0.324219170624604)) ;
#77151 = CARTESIAN_POINT('Ctrl Pts',(0.295360129840502,-0.295360129840502,
-0.274609795624604)) ;
#77152 = CARTESIAN_POINT('Ctrl Pts',(0.417702301404717,-0.173017958276288,
-0.225000420624604)) ;
#77153 = CARTESIAN_POINT('Ctrl Pts',(0.417702301404716,-7.67306679617654E-17,
-0.175391045624604)) ;
#77154 = CARTESIAN_POINT('Ctrl Pts',(0.417702301404717,0.173017958276288,
-0.125781670624604)) ;
#77155 = CARTESIAN_POINT('Ctrl Pts',(0.295360129840502,0.295360129840503,
-0.0761722956246044)) ;
#77156 = CARTESIAN_POINT('Ctrl Pts',(0.173017958276288,0.417702301404717,
-0.0265629206246046)) ;
#77157 = CARTESIAN_POINT('Ctrl Pts',(0.,0.417702301404716,0.0230464543753958)) ;
#77158 = CARTESIAN_POINT('Ctrl Pts',(-0.173017958276288,0.417702301404717,
0.0726558293753954)) ;
#77159 = CARTESIAN_POINT('Ctrl Pts',(-0.295360129840502,0.295360129840502,
0.122265204375396)) ;
#77160 = CARTESIAN_POINT('Ctrl Pts',(-0.417702301404717,0.173017958276288,
0.171874579375395)) ;
#77161 = CARTESIAN_POINT('Ctrl Pts',(-0.417702301404716,2.55768893205885E-17,
0.221483954375396)) ;
#77162 = CARTESIAN_POINT('Ctrl Pts',(-0.417702301404717,-0.173017958276288,
0.271093329375396)) ;
#77163 = CARTESIAN_POINT('Ctrl Pts',(-0.295360129840502,-0.295360129840502,
0.320702704375395)) ;
#77164 = CARTESIAN_POINT('Ctrl Pts',(-0.173017958276288,-0.417702301404717,
0.370312079375396)) ;
#77165 = CARTESIAN_POINT('Ctrl Pts',(-5.1153778641177E-17,-0.417702301404716,
0.419921454375396)) ;
#77166 = CARTESIAN_POINT('Ctrl Pts',(0.173017958276288,-0.417702301404716,
0.469530829375396)) ;
#77167 = CARTESIAN_POINT('Ctrl Pts',(0.295360129840502,-0.295360129840502,
0.519140204375396)) ;
#77168 = CARTESIAN_POINT('Ctrl Pts',(0.417702301404717,-0.173017958276288,
0.568749579375395)) ;
#77169 = CARTESIAN_POINT('Ctrl Pts',(0.417702301404716,-7.67306679617654E-17,
0.618358954375396)) ;
#77170 = CARTESIAN_POINT('Ctrl Pts',(0.417702301404717,0.173017958276288,
0.667968329375395)) ;
#77171 = CARTESIAN_POINT('Ctrl Pts',(0.295360129840502,0.295360129840503,
0.717577704375396)) ;
#77172 = CARTESIAN_POINT('Ctrl Pts',(0.173017958276288,0.417702301404717,
0.767187079375397)) ;
#77173 = CARTESIAN_POINT('Ctrl Pts',(0.,0.417702301404716,0.816796454375395)) ;
#77174 = CARTESIAN_POINT('Ctrl Pts',(-0.173017958276288,0.417702301404717,
0.866405829375395)) ;
#77175 = CARTESIAN_POINT('Ctrl Pts',(-0.295360129840502,0.295360129840502,
0.916015204375395)) ;
#77176 = CARTESIAN_POINT('Ctrl Pts',(-0.417702301404717,0.173017958276288,
0.965624579375395)) ;
#77177 = CARTESIAN_POINT('Ctrl Pts',(-0.417702301404716,2.55768893205885E-17,
1.0152339543754)) ;
#77178 = CARTESIAN_POINT('Ctrl Pts',(-0.417702301404717,-0.173017958276288,
1.0648433293754)) ;
#77179 = CARTESIAN_POINT('Ctrl Pts',(-0.295360129840502,-0.295360129840502,
1.1144527043754)) ;
#77180 = CARTESIAN_POINT('Ctrl Pts',(-0.173017958276288,-0.417702301404717,
1.1640620793754)) ;
#77181 = CARTESIAN_POINT('Ctrl Pts',(-5.1153778641177E-17,-0.417702301404716,
1.2136714543754)) ;
#77182 = CARTESIAN_POINT('Ctrl Pts',(0.173017958276288,-0.417702301404716,
1.2632808293754)) ;
#77183 = CARTESIAN_POINT('Ctrl Pts',(0.295360129840502,-0.295360129840502,
1.3128902043754)) ;
#77184 = CARTESIAN_POINT('Ctrl Pts',(0.417702301404717,-0.173017958276288,
1.3624995793754)) ;
#77185 = CARTESIAN_POINT('Ctrl Pts',(0.417702301404716,-7.67306679617654E-17,
1.4121089543754)) ;
#77186 = CARTESIAN_POINT('Ctrl Pts',(0.417702301404717,0.173017958276288,
1.4617183293754)) ;
#77187 = CARTESIAN_POINT('Ctrl Pts',(0.295360129840502,0.295360129840503,
1.51132770437539)) ;
#77188 = CARTESIAN_POINT('Ctrl Pts',(0.173017958276288,0.417702301404717,
1.5609370793754)) ;
#77189 = CARTESIAN_POINT('Ctrl Pts',(0.,0.417702301404716,1.61054645437539)) ;
#77190 = CARTESIAN_POINT('Ctrl Pts',(-0.173017958276288,0.417702301404717,
1.6601558293754)) ;
#77191 = CARTESIAN_POINT('Ctrl Pts',(-0.295360129840502,0.295360129840502,
1.7097652043754)) ;
#77192 = CARTESIAN_POINT('Ctrl Pts',(-0.417702301404717,0.173017958276288,
1.75937457937539)) ;
#77193 = CARTESIAN_POINT('Ctrl Pts',(-0.417702301404716,2.55768893205885E-17,
1.8089839543754)) ;
#77194 = CARTESIAN_POINT('Ctrl Pts',(-0.417702301404717,-0.173017958276288,
1.8585933293754)) ;
#77195 = CARTESIAN_POINT('Ctrl Pts',(-0.295360129840502,-0.295360129840502,
1.9082027043754)) ;
#77196 = CARTESIAN_POINT('Ctrl Pts',(-0.173017958276288,-0.417702301404717,
1.9578120793754)) ;
#77197 = CARTESIAN_POINT('Ctrl Pts',(-5.1153778641177E-17,-0.417702301404716,
2.00742145437539)) ;
#77198 = CARTESIAN_POINT('Ctrl Pts',(0.173017958276288,-0.417702301404716,
2.0570308293754)) ;
#77199 = CARTESIAN_POINT('Ctrl Pts',(0.295360129840502,-0.295360129840502,
2.10664020437539)) ;
#77200 = CARTESIAN_POINT('Ctrl Pts',(0.417702301404717,-0.173017958276288,
2.1562495793754)) ;
#77201 = CARTESIAN_POINT('Ctrl Pts',(0.417702301404716,-7.67306679617654E-17,
2.2058589543754)) ;
#77202 = CARTESIAN_POINT('Ctrl Pts',(0.417702301404717,0.173017958276288,
2.2554683293754)) ;
#77203 = CARTESIAN_POINT('Ctrl Pts',(0.295360129840502,0.295360129840503,
2.3050777043754)) ;
#77204 = CARTESIAN_POINT('Ctrl Pts',(0.173017958276288,0.417702301404717,
2.3546870793754)) ;
#77205 = CARTESIAN_POINT('Ctrl Pts',(0.,0.417702301404716,2.4042964543754)) ;
#77206 = CARTESIAN_POINT('Ctrl Pts',(-0.173017958276288,0.417702301404717,
2.4539058293754)) ;
#77207 = CARTESIAN_POINT('Ctrl Pts',(-0.295360129840502,0.295360129840502,
2.50351520437539)) ;
#77208 = CARTESIAN_POINT('Ctrl Pts',(-0.417702301404717,0.173017958276288,
2.55312457937539)) ;
#77209 = CARTESIAN_POINT('Ctrl Pts',(-0.417702301404716,2.55768893205885E-17,
2.60273395437539)) ;
#77210 = CARTESIAN_POINT('Ctrl Pts',(-0.417702301404717,-0.173017958276288,
2.6523433293754)) ;
#77211 = CARTESIAN_POINT('Ctrl Pts',(-0.295360129840502,-0.295360129840502,
2.70195270437539)) ;
#77212 = CARTESIAN_POINT('Ctrl Pts',(-0.173017958276288,-0.417702301404717,
2.7515620793754)) ;
#77213 = CARTESIAN_POINT('Ctrl Pts',(-5.1153778641177E-17,-0.417702301404716,
2.8011714543754)) ;
#77214 = CARTESIAN_POINT('Ctrl Pts',(0.173017958276288,-0.417702301404716,
2.8507808293754)) ;
#77215 = CARTESIAN_POINT('Ctrl Pts',(0.295360129840502,-0.295360129840502,
2.9003902043754)) ;
#77216 = CARTESIAN_POINT('Ctrl Pts',(0.417702301404717,-0.173017958276288,
2.9499995793754)) ;
#77217 = CARTESIAN_POINT('Ctrl Pts',(0.417702301404716,-7.67306679617654E-17,
2.9996089543754)) ;
#77218 = CARTESIAN_POINT('Ctrl Pts',(0.417702301404717,0.173017958276288,
3.04921832937539)) ;
#77219 = CARTESIAN_POINT('Ctrl Pts',(0.295360129840502,0.295360129840503,
3.0988277043754)) ;
#77220 = CARTESIAN_POINT('Ctrl Pts',(0.173017958276288,0.417702301404717,
3.1484370793754)) ;
#77221 = CARTESIAN_POINT('Ctrl Pts',(0.,0.417702301404716,3.1980464543754)) ;
#77222 = CARTESIAN_POINT('Ctrl Pts',(-0.173017958276288,0.417702301404717,
3.2476558293754)) ;
#77223 = CARTESIAN_POINT('Ctrl Pts',(-0.295360129840502,0.295360129840502,
3.29726520437539)) ;
#77224 = CARTESIAN_POINT('Ctrl Pts',(-0.417702301404717,0.173017958276288,
3.3468745793754)) ;
#77225 = CARTESIAN_POINT('Ctrl Pts',(-0.417702301404716,2.55768893205885E-17,
3.3964839543754)) ;
#77226 = CARTESIAN_POINT('Ctrl Pts',(-0.417702301404717,-0.173017958276288,
3.44609332937539)) ;
#77227 = CARTESIAN_POINT('Ctrl Pts',(-0.295360129840502,-0.295360129840502,
3.49570270437539)) ;
#77228 = CARTESIAN_POINT('Ctrl Pts',(-0.173017958276288,-0.417702301404717,
3.5453120793754)) ;
#77229 = CARTESIAN_POINT('Ctrl Pts',(-5.1153778641177E-17,-0.417702301404716,
3.59492145437539)) ;
#77230 = CARTESIAN_POINT('Ctrl Pts',(0.173017958276288,-0.417702301404716,
3.64453082937539)) ;
#77231 = CARTESIAN_POINT('Ctrl Pts',(0.295360129840502,-0.295360129840502,
3.6941402043754)) ;
#77232 = CARTESIAN_POINT('Ctrl Pts',(0.417702301404717,-0.173017958276288,
3.74374957937539)) ;
#77233 = CARTESIAN_POINT('Ctrl Pts',(0.417702301404716,-7.67306679617654E-17,
3.79335895437539)) ;
#77234 = CARTESIAN_POINT('Ctrl Pts',(0.417702301404717,0.173017958276288,
3.84296832937539)) ;
#77235 = CARTESIAN_POINT('Ctrl Pts',(0.295360129840502,0.295360129840503,
3.89257770437539)) ;
#77236 = CARTESIAN_POINT('Ctrl Pts',(0.173017958276288,0.417702301404717,
3.9421870793754)) ;
#77237 = CARTESIAN_POINT('Ctrl Pts',(0.,0.417702301404716,3.9917964543754)) ;
#77238 = CARTESIAN_POINT('Ctrl Pts',(-0.173017958276288,0.417702301404717,
4.04140582937539)) ;
#77239 = CARTESIAN_POINT('Ctrl Pts',(-0.295360129840502,0.295360129840502,
4.09101520437539)) ;
#77240 = CARTESIAN_POINT('Ctrl Pts',(-0.417702301404717,0.173017958276288,
4.14062457937539)) ;
#77241 = CARTESIAN_POINT('Ctrl Pts',(-0.417702301404716,2.55768893205885E-17,
4.1902339543754)) ;
#77242 = CARTESIAN_POINT('Ctrl Pts',(-0.417702301404717,-0.173017958276288,
4.23984332937539)) ;
#77243 = CARTESIAN_POINT('Ctrl Pts',(-0.295360129840502,-0.295360129840502,
4.28945270437539)) ;
#77244 = CARTESIAN_POINT('Ctrl Pts',(-0.173017958276288,-0.417702301404717,
4.3390620793754)) ;
#77245 = CARTESIAN_POINT('Ctrl Pts',(-5.1153778641177E-17,-0.417702301404716,
4.38867145437539)) ;
#77246 = CARTESIAN_POINT('Ctrl Pts',(0.173017958276288,-0.417702301404716,
4.4382808293754)) ;
#77247 = CARTESIAN_POINT('Ctrl Pts',(0.295360129840502,-0.295360129840502,
4.48789020437539)) ;
#77248 = CARTESIAN_POINT('Ctrl Pts',(0.417702301404717,-0.173017958276288,
4.53749957937539)) ;
#77249 = CARTESIAN_POINT('Ctrl Pts',(0.417702301404716,-7.67306679617654E-17,
4.58710895437539)) ;
#77250 = CARTESIAN_POINT('Ctrl Pts',(0.417702301404717,0.173017958276288,
4.63671832937539)) ;
#77251 = CARTESIAN_POINT('Ctrl Pts',(0.295360129840502,0.295360129840503,
4.6863277043754)) ;
#77252 = CARTESIAN_POINT('Ctrl Pts',(0.173017958276288,0.417702301404717,
4.73593707937539)) ;
#77253 = CARTESIAN_POINT('Ctrl Pts',(0.,0.417702301404716,4.78554645437539)) ;
#77254 = CARTESIAN_POINT('Ctrl Pts',(-0.173017958276288,0.417702301404717,
4.8351558293754)) ;
#77255 = CARTESIAN_POINT('Ctrl Pts',(-0.295360129840502,0.295360129840502,
4.88476520437539)) ;
#77256 = CARTESIAN_POINT('Ctrl Pts',(-0.417702301404717,0.173017958276288,
4.9343745793754)) ;
#77257 = CARTESIAN_POINT('Ctrl Pts',(-0.417702301404716,2.55768893205885E-17,
4.9839839543754)) ;
#77258 = CARTESIAN_POINT('Ctrl Pts',(-0.417702301404717,-0.173017958276288,
5.03359332937539)) ;
#77259 = CARTESIAN_POINT('Ctrl Pts',(-0.295360129840502,-0.295360129840502,
5.08320270437539)) ;
#77260 = CARTESIAN_POINT('Ctrl Pts',(-0.173017958276288,-0.417702301404717,
5.13281207937539)) ;
#77261 = CARTESIAN_POINT('Ctrl Pts',(-5.1153778641177E-17,-0.417702301404716,
5.1824214543754)) ;
#77262 = CARTESIAN_POINT('Ctrl Pts',(0.173017958276288,-0.417702301404716,
5.23203082937539)) ;
#77263 = CARTESIAN_POINT('Ctrl Pts',(0.295360129840502,-0.295360129840502,
5.28164020437539)) ;
#77264 = CARTESIAN_POINT('Ctrl Pts',(0.417702301404717,-0.173017958276288,
5.33124957937539)) ;
#77265 = CARTESIAN_POINT('Ctrl Pts',(0.417702301404716,-7.67306679617654E-17,
5.3808589543754)) ;
#77266 = CARTESIAN_POINT('Ctrl Pts',(0.417702301404717,0.173017958276288,
5.4304683293754)) ;
#77267 = CARTESIAN_POINT('Ctrl Pts',(0.295360129840502,0.295360129840503,
5.4800777043754)) ;
#77268 = CARTESIAN_POINT('Ctrl Pts',(0.173017958276288,0.417702301404717,
5.5296870793754)) ;
#77269 = CARTESIAN_POINT('Ctrl Pts',(0.,0.417702301404716,5.57929645437539)) ;
#77270 = CARTESIAN_POINT('Ctrl Pts',(-0.173017958276288,0.417702301404717,
5.62890582937539)) ;
#77271 = CARTESIAN_POINT('Ctrl Pts',(-0.295360129840502,0.295360129840502,
5.6785152043754)) ;
#77272 = CARTESIAN_POINT('Ctrl Pts',(-0.417702301404717,0.173017958276288,
5.72812457937539)) ;
#77273 = CARTESIAN_POINT('Ctrl Pts',(-0.417702301404716,2.55768893205885E-17,
5.77773395437539)) ;
#77274 = CARTESIAN_POINT('Ctrl Pts',(-0.417702301404717,-0.173017958276288,
5.82734332937539)) ;
#77275 = CARTESIAN_POINT('Ctrl Pts',(-0.295360129840502,-0.295360129840502,
5.87695270437539)) ;
#77276 = CARTESIAN_POINT('Ctrl Pts',(-0.173017958276288,-0.417702301404717,
5.9265620793754)) ;
#77277 = CARTESIAN_POINT('Ctrl Pts',(-5.1153778641177E-17,-0.417702301404716,
5.97617145437539)) ;
#77278 = CARTESIAN_POINT('Ctrl Pts',(0.173017958276288,-0.417702301404716,
6.0257808293754)) ;
#77279 = CARTESIAN_POINT('Ctrl Pts',(0.295360129840502,-0.295360129840502,
6.0753902043754)) ;
#77280 = CARTESIAN_POINT('Ctrl Pts',(0.417702301404717,-0.173017958276288,
6.12499957937539)) ;
#77281 = CARTESIAN_POINT('Ctrl Pts',(0.417702301404716,-7.67306679617654E-17,
6.1746089543754)) ;
#77282 = CARTESIAN_POINT('Ctrl Pts',(0.417702301404717,0.173017958276288,
6.22421832937539)) ;
#77283 = CARTESIAN_POINT('Ctrl Pts',(0.295360129840502,0.295360129840503,
6.27382770437539)) ;
#77284 = CARTESIAN_POINT('Ctrl Pts',(0.173017958276288,0.417702301404717,
6.3234370793754)) ;
#77285 = CARTESIAN_POINT('Ctrl Pts',(0.,0.417702301404716,6.3730464543754)) ;
#77286 = CARTESIAN_POINT('Ctrl Pts',(-0.194635088947967,-1.22163646928409,
0.0797567518094009)) ;
#77287 = CARTESIAN_POINT('Ctrl Pts',(-0.0043082693312935,-1.30090248401962,
0.128089684784921)) ;
#77288 = CARTESIAN_POINT('Ctrl Pts',(0.17965409482365,-1.316658036297,0.165447546864525)) ;
#77289 = CARTESIAN_POINT('Ctrl Pts',(0.484008391354344,-1.31323795873721,
0.23199194234403)) ;
#77290 = CARTESIAN_POINT('Ctrl Pts',(0.655998289214855,-1.27815569745546,
0.269189612454462)) ;
#77291 = CARTESIAN_POINT('Ctrl Pts',(1.01370529834126,-1.13088907272712,0.347108578180816)) ;
#77292 = CARTESIAN_POINT('Ctrl Pts',(1.17648098544676,-1.01084917584401,0.382416490912591)) ;
#77293 = CARTESIAN_POINT('Ctrl Pts',(1.42251858408678,-0.760738367422026,
0.448222681167146)) ;
#77294 = CARTESIAN_POINT('Ctrl Pts',(1.51694609891737,-0.630767018075734,
0.478024324337763)) ;
#77295 = CARTESIAN_POINT('Ctrl Pts',(1.7004605039317,-0.277947938509247,0.549796632634112)) ;
#77296 = CARTESIAN_POINT('Ctrl Pts',(1.73763017634033,-0.0925850035561787,
0.580342676340329)) ;
#77297 = CARTESIAN_POINT('Ctrl Pts',(1.7526,-3.21947397027848E-16,0.5953125)) ;
#77298 = CARTESIAN_POINT('Origin',(0.,-2.985516,6.35)) ;
#77299 = CARTESIAN_POINT('Ctrl Pts',(-1.94288959754296,-0.448102752174796,
7.0818)) ;
#77300 = CARTESIAN_POINT('Ctrl Pts',(-1.94270197516804,-0.44756275002075,
7.0818)) ;
#77301 = CARTESIAN_POINT('Ctrl Pts',(-1.94251230527771,-0.447017983233947,
7.08179766992681)) ;
#77302 = CARTESIAN_POINT('Ctrl Pts',(-1.91803916780255,-0.376442475898735,
7.08160456336027)) ;
#77303 = CARTESIAN_POINT('Ctrl Pts',(-1.88761451839117,-0.293719590124047,
7.05576035709451)) ;
#77304 = CARTESIAN_POINT('Ctrl Pts',(-1.87819429271644,-0.268591723493095,
7.00768190451026)) ;
#77305 = CARTESIAN_POINT('Ctrl Pts',(-1.94288959754296,-0.448102752174796,
7.0818)) ;
#77306 = CARTESIAN_POINT('Ctrl Pts',(-1.94252901127664,-0.44757378511647,
7.0818)) ;
#77307 = CARTESIAN_POINT('Ctrl Pts',(-1.94238760924975,-0.447241733483015,
7.08171624908906)) ;
#77308 = CARTESIAN_POINT('Ctrl Pts',(-1.90274378880994,-0.385137079174368,
7.0842962048653)) ;
#77309 = CARTESIAN_POINT('Ctrl Pts',(-1.86635603372515,-0.320809755584884,
7.03323707646529)) ;
#77310 = CARTESIAN_POINT('Ctrl Pts',(-1.86932161172289,-0.312347136547012,
6.9980193066578)) ;
#77311 = CARTESIAN_POINT('Ctrl Pts',(-1.94288959754296,-0.448102752174796,
7.0818)) ;
#77312 = CARTESIAN_POINT('Ctrl Pts',(-1.94245161464451,-0.447640464231361,
7.0818)) ;
#77313 = CARTESIAN_POINT('Ctrl Pts',(-1.94216670833245,-0.447413283195794,
7.08171624908906)) ;
#77314 = CARTESIAN_POINT('Ctrl Pts',(-1.89052514974837,-0.394910453248505,
7.08429620486504)) ;
#77315 = CARTESIAN_POINT('Ctrl Pts',(-1.8347389543407,-0.347957809715575,
7.0332370764653)) ;
#77316 = CARTESIAN_POINT('Ctrl Pts',(-1.82714531063845,-0.348921084254559,
6.9980193066578)) ;
#77317 = CARTESIAN_POINT('Ctrl Pts',(-1.94288959754296,-0.448102752174796,
7.0818)) ;
#77318 = CARTESIAN_POINT('Ctrl Pts',(-1.94240557475944,-0.447798570605971,
7.0818)) ;
#77319 = CARTESIAN_POINT('Ctrl Pts',(-1.94191738994489,-0.447492388347843,
7.08179766992681)) ;
#77320 = CARTESIAN_POINT('Ctrl Pts',(-1.87864342769047,-0.407664231468328,
7.08160456336)) ;
#77321 = CARTESIAN_POINT('Ctrl Pts',(-1.80491723090524,-0.364392752089199,
7.05576035709452)) ;
#77322 = CARTESIAN_POINT('Ctrl Pts',(-1.78257449869962,-0.351510169545915,
7.00768190451026)) ;
#77323 = CARTESIAN_POINT('',(-1.78257449869962,-0.35151016954591,7.00768190451024)) ;
#77324 = CARTESIAN_POINT('',(-1.87819429271644,-0.268591723493095,7.00768190451026)) ;
#77325 = CARTESIAN_POINT('Origin',(-1.78257449869962,-0.254917586917006,7.03356380902051)) ;
#77326 = CARTESIAN_POINT('',(-1.89249580907583,-0.307272596057229,7.04638255392192)) ;
#77327 = CARTESIAN_POINT('Origin',(-1.98523598945348,-0.564759059977123,6.9430176984354)) ;
#77328 = CARTESIAN_POINT('',(-1.91807183825027,-0.377810206882459,7.07388013398117)) ;
#77329 = CARTESIAN_POINT('Origin',(-1.9365430293827,-0.434616459037521,6.99727618798715)) ;
#77330 = CARTESIAN_POINT('',(-1.94182783334028,-0.445044808441315,7.08178867415542)) ;
#77331 = CARTESIAN_POINT('Origin',(-1.92795162512393,-0.413874762423167,7.02228347025522)) ;
#77332 = CARTESIAN_POINT('',(-1.94288959754296,-0.448102752174818,7.0818)) ;
#77333 = CARTESIAN_POINT('',(-1.94182783307279,-0.445044807670936,7.08178867415257)) ;
#77334 = CARTESIAN_POINT('',(-1.94014976372661,-0.4463802141404,7.08178692473713)) ;
#77335 = CARTESIAN_POINT('',(-1.94288959754295,-0.448102752174801,7.0818)) ;
#77336 = CARTESIAN_POINT('',(-1.87964216948038,-0.409078843661158,7.07382903170985)) ;
#77337 = CARTESIAN_POINT('Origin',(-1.92743649770787,-0.446270284367414,6.99208610043499)) ;
#77338 = CARTESIAN_POINT('',(-1.81813539254511,-0.372312156582617,7.04714690179984)) ;
#77339 = CARTESIAN_POINT('Origin',(-1.9325040879477,-0.44453393011351,6.99487389856661)) ;
#77340 = CARTESIAN_POINT('Origin',(-2.04686400773891,-0.509803748797932,6.94140176115792)) ;
#77341 = CARTESIAN_POINT('Ctrl Pts',(-1.87819429271643,-0.268591723493085,
7.00768190451022)) ;
#77342 = CARTESIAN_POINT('Ctrl Pts',(-1.87559269584778,-0.265429455820014,
6.99639968079939)) ;
#77343 = CARTESIAN_POINT('Ctrl Pts',(-1.87277553216538,-0.263323474391198,
6.98489826419215)) ;
#77344 = CARTESIAN_POINT('Ctrl Pts',(-1.86979680842784,-0.262281765411183,
6.97334924403636)) ;
#77345 = CARTESIAN_POINT('Ctrl Pts',(-1.87312418929155,-0.293594816666754,
7.00216042002311)) ;
#77346 = CARTESIAN_POINT('Ctrl Pts',(-1.87084473493899,-0.291084530404652,
6.99224479183829)) ;
#77347 = CARTESIAN_POINT('Ctrl Pts',(-1.86834496343776,-0.289501530632308,
6.98216124843708)) ;
#77348 = CARTESIAN_POINT('Ctrl Pts',(-1.86572206147513,-0.288873179727176,
6.97207530474358)) ;
#77349 = CARTESIAN_POINT('Ctrl Pts',(-1.84631328088201,-0.334524427261344,
6.9974230667741)) ;
#77350 = CARTESIAN_POINT('Ctrl Pts',(-1.84417962418044,-0.333091612281746,
6.98998909901151)) ;
#77351 = CARTESIAN_POINT('Ctrl Pts',(-1.84187319629001,-0.332400676673093,
6.98249471608034)) ;
#77352 = CARTESIAN_POINT('Ctrl Pts',(-1.83942120369611,-0.332407181519401,
6.97506009028094)) ;
#77353 = CARTESIAN_POINT('Ctrl Pts',(-1.80167627524482,-0.350400561563901,
7.0035407911449)) ;
#77354 = CARTESIAN_POINT('Ctrl Pts',(-1.79920012229604,-0.349063108054369,
6.9975751162926)) ;
#77355 = CARTESIAN_POINT('Ctrl Pts',(-1.79652736146151,-0.348276516130449,
6.99152359092133)) ;
#77356 = CARTESIAN_POINT('Ctrl Pts',(-1.79370245617676,-0.348044577753767,
6.98550115761471)) ;
#77357 = CARTESIAN_POINT('Ctrl Pts',(-1.78257449869961,-0.35151016954591,
7.00768190451025)) ;
#77358 = CARTESIAN_POINT('Ctrl Pts',(-1.77995299478772,-0.34999863817984,
7.00204079265483)) ;
#77359 = CARTESIAN_POINT('Ctrl Pts',(-1.77712384321892,-0.348988486534664,
6.99629008435121)) ;
#77360 = CARTESIAN_POINT('Ctrl Pts',(-1.77414072885052,-0.348483282365518,
6.99051557427332)) ;
#77361 = CARTESIAN_POINT('',(-1.77414072885053,-0.348483282365581,6.99051557427404)) ;
#77362 = CARTESIAN_POINT('',(-1.86979680842784,-0.262281765411183,6.97334924403636)) ;
#77363 = CARTESIAN_POINT('Origin',(-1.77414072885052,-0.248863812556215,6.99923114854662)) ;
#77364 = CARTESIAN_POINT('Origin',(-1.84377759622581,-0.424925231995625,6.96360853180443)) ;
#77365 = CARTESIAN_POINT('Origin',(-1.74961486668251,-0.42410100616838,6.98537442847036)) ;
#77366 = CARTESIAN_POINT('Ctrl Pts',(-1.72771014821048,-0.332764968591514,
6.81085442572523)) ;
#77367 = CARTESIAN_POINT('Ctrl Pts',(-1.74319473414623,-0.338004233132819,
6.87073949346036)) ;
#77368 = CARTESIAN_POINT('Ctrl Pts',(-1.75867139282682,-0.343243675639426,
6.93062659534819)) ;
#77369 = CARTESIAN_POINT('Ctrl Pts',(-1.77414072885052,-0.348483282365389,
6.99051557427185)) ;
#77370 = CARTESIAN_POINT('Ctrl Pts',(-1.75388379891716,-0.332177363448602,
6.80413806820838)) ;
#77371 = CARTESIAN_POINT('Ctrl Pts',(-1.76933665987689,-0.337416538558189,
6.86403381882623)) ;
#77372 = CARTESIAN_POINT('Ctrl Pts',(-1.78478377705788,-0.342658817603973,
6.92393065445506)) ;
#77373 = CARTESIAN_POINT('Ctrl Pts',(-1.80022303195211,-0.347898342882965,
6.98382968539379)) ;
#77374 = CARTESIAN_POINT('Ctrl Pts',(-1.79938284222792,-0.310992589547657,
6.79422672914051)) ;
#77375 = CARTESIAN_POINT('Ctrl Pts',(-1.81478360858998,-0.316286258253172,
6.85413545484315)) ;
#77376 = CARTESIAN_POINT('Ctrl Pts',(-1.8301777875902,-0.321577463411775,
6.91404581861747)) ;
#77377 = CARTESIAN_POINT('Ctrl Pts',(-1.84556760072685,-0.326868409115673,
6.97395705441162)) ;
#77378 = CARTESIAN_POINT('Ctrl Pts',(-1.82046616955548,-0.266091328799139,
6.79270352788241)) ;
#77379 = CARTESIAN_POINT('Ctrl Pts',(-1.83589739021241,-0.271473267897804,
6.85259865161434)) ;
#77380 = CARTESIAN_POINT('Ctrl Pts',(-1.85132258737841,-0.276850760615209,
6.91249534127297)) ;
#77381 = CARTESIAN_POINT('Ctrl Pts',(-1.86674074821324,-0.282225326148102,
6.9723937895665)) ;
#77382 = CARTESIAN_POINT('Ctrl Pts',(-1.82343508275074,-0.246063080838804,
6.79368809548975)) ;
#77383 = CARTESIAN_POINT('Ctrl Pts',(-1.83889654046897,-0.251473735590624,
6.85357316322487)) ;
#77384 = CARTESIAN_POINT('Ctrl Pts',(-1.85435024060401,-0.256879845047546,
6.9134602651127)) ;
#77385 = CARTESIAN_POINT('Ctrl Pts',(-1.86979680842784,-0.262281765411184,
6.97334924403636)) ;
#77386 = CARTESIAN_POINT('',(-1.72771014821048,-0.332764968591514,6.81085442572523)) ;
#77387 = CARTESIAN_POINT('',(-1.77414072885052,-0.348483282365389,6.99051557427185)) ;
#77388 = CARTESIAN_POINT('',(-1.82343508275074,-0.246063080838804,6.79368809548975)) ;
#77389 = CARTESIAN_POINT('Origin',(-1.72771014821048,-0.233145498782339,6.81957)) ;
#77390 = CARTESIAN_POINT('',(-1.82343508275074,-0.246063080838804,6.79368809548975)) ;
#77391 = CARTESIAN_POINT('Origin',(-1.72771014821048,-0.233145498782339,6.81957)) ;
#77392 = CARTESIAN_POINT('',(-1.72771014821048,-0.233145498782339,6.71957)) ;
#77393 = CARTESIAN_POINT('Origin',(-1.72771014821048,-0.233145498782339,6.81957)) ;
#77394 = CARTESIAN_POINT('Origin',(-1.72771014821048,-0.233145498782339,6.81957)) ;
#77395 = CARTESIAN_POINT('Origin',(-3.54734504026457E-15,-0.507999999999988,
8.8138)) ;
#77396 = CARTESIAN_POINT('',(-1.17871069663557,-0.348483282365649,6.99051557427477)) ;
#77397 = CARTESIAN_POINT('',(4.7625,-0.34848328236569,6.99051557427477)) ;
#77398 = CARTESIAN_POINT('',(-1.17558412963155,-0.332764968591518,6.81085442572523)) ;
#77399 = CARTESIAN_POINT('',(-1.21039177030076,-0.507754795155569,8.81099729580349)) ;
#77400 = CARTESIAN_POINT('',(-2.32368535611608E-15,-0.332764968591526,6.81085442572523)) ;
#77401 = CARTESIAN_POINT('Origin',(4.7625,-0.448102752174865,6.9818)) ;
#77402 = CARTESIAN_POINT('',(-1.17871069663558,-0.448102752174823,7.0818)) ;
#77403 = CARTESIAN_POINT('',(4.7625,-0.448102752174865,7.0818)) ;
#77404 = CARTESIAN_POINT('Origin',(-1.17871069663558,-0.448102752174823,6.9818)) ;
#77405 = CARTESIAN_POINT('Origin',(-4.45650581216736E-16,7.57196551496331E-15,
6.98180000000001)) ;
#77406 = CARTESIAN_POINT('',(-1.87819429271644,0.268591723493141,7.00768190451026)) ;
#77407 = CARTESIAN_POINT('Origin',(0.,7.3282997741086E-15,7.00768190451026)) ;
#77408 = CARTESIAN_POINT('',(-1.93516376196126,0.425958697938772,7.08103018110414)) ;
#77409 = CARTESIAN_POINT('Ctrl Pts',(-1.93516376196126,0.425958697938772,
7.08103018110414)) ;
#77410 = CARTESIAN_POINT('Ctrl Pts',(-1.91237404551335,0.361043831880854,
7.07642065497011)) ;
#77411 = CARTESIAN_POINT('Ctrl Pts',(-1.88670733098046,0.291299724077108,
7.05113030167797)) ;
#77412 = CARTESIAN_POINT('Ctrl Pts',(-1.87819429271644,0.268591723493142,
7.00768190451026)) ;
#77413 = CARTESIAN_POINT('',(-1.94288959754295,0.448102752174865,7.0818)) ;
#77414 = CARTESIAN_POINT('Ctrl Pts',(-1.94288959754295,0.448102752174872,
7.0818)) ;
#77415 = CARTESIAN_POINT('Ctrl Pts',(-1.94270198330611,0.44756277344327,7.0818)) ;
#77416 = CARTESIAN_POINT('Ctrl Pts',(-1.94251232165803,0.447018030321751,
7.08179767010457)) ;
#77417 = CARTESIAN_POINT('Ctrl Pts',(-1.9399882560469,0.43973914278705,7.08177775516638)) ;
#77418 = CARTESIAN_POINT('Ctrl Pts',(-1.93759234469623,0.432876340960395,
7.08152139456926)) ;
#77419 = CARTESIAN_POINT('Ctrl Pts',(-1.93516376196126,0.425958697938772,
7.08103018110414)) ;
#77420 = CARTESIAN_POINT('Origin',(-4.45650581216736E-16,7.57196551496331E-15,
7.0818)) ;
#77421 = CARTESIAN_POINT('Origin',(-1.72771014821048,0.233145498782383,6.81957)) ;
#77422 = CARTESIAN_POINT('',(-1.72771014821048,0.332764968591557,6.81085442572523)) ;
#77423 = CARTESIAN_POINT('',(-1.82343508275074,0.246063080838849,6.79368809548975)) ;
#77424 = CARTESIAN_POINT('Origin',(-1.72771014821048,0.233145498782383,6.81957)) ;
#77425 = CARTESIAN_POINT('',(-1.72771014821048,0.233145498782383,6.71957)) ;
#77426 = CARTESIAN_POINT('Origin',(-1.72771014821048,0.233145498782383,6.81957)) ;
#77427 = CARTESIAN_POINT('Origin',(-1.72771014821048,0.233145498782383,6.81957)) ;
#77428 = CARTESIAN_POINT('Ctrl Pts',(-1.82343508274976,0.246063080838507,
6.79368809548596)) ;
#77429 = CARTESIAN_POINT('Ctrl Pts',(-1.8388965404683,0.251473735590436,6.85357316322228)) ;
#77430 = CARTESIAN_POINT('Ctrl Pts',(-1.85435024060365,0.256879845047465,
6.91346026511131)) ;
#77431 = CARTESIAN_POINT('Ctrl Pts',(-1.86979680842779,0.262281765411211,
6.97334924403617)) ;
#77432 = CARTESIAN_POINT('Ctrl Pts',(-1.81947653182275,0.272767411452289,
6.79237533867617)) ;
#77433 = CARTESIAN_POINT('Ctrl Pts',(-1.83489694400734,0.278139250484315,
6.85227406114401)) ;
#77434 = CARTESIAN_POINT('Ctrl Pts',(-1.85031405219097,0.283508230262916,
6.91217346932062)) ;
#77435 = CARTESIAN_POINT('Ctrl Pts',(-1.86572206147498,0.288873179727103,
6.97207530474301)) ;
#77436 = CARTESIAN_POINT('Ctrl Pts',(-1.79322013108717,0.316574402604316,
6.79533188669133)) ;
#77437 = CARTESIAN_POINT('Ctrl Pts',(-1.80862659259988,0.321853195169872,
6.85523985899826)) ;
#77438 = CARTESIAN_POINT('Ctrl Pts',(-1.82402601364689,0.327130342614484,
6.91514954549618)) ;
#77439 = CARTESIAN_POINT('Ctrl Pts',(-1.83942125592947,0.332407254608791,
6.97506007039325)) ;
#77440 = CARTESIAN_POINT('Ctrl Pts',(-1.74734038623951,0.332324264734042,
6.8058171575838)) ;
#77441 = CARTESIAN_POINT('Ctrl Pts',(-1.76280167491966,0.337563919259398,
6.86571006109106)) ;
#77442 = CARTESIAN_POINT('Ctrl Pts',(-1.77825521655385,0.342804601986218,
6.92560480456484)) ;
#77443 = CARTESIAN_POINT('Ctrl Pts',(-1.79370245617666,0.348044577753599,
6.98550115761311)) ;
#77444 = CARTESIAN_POINT('Ctrl Pts',(-1.7277101482095,0.332764968591226,6.81085442572145)) ;
#77445 = CARTESIAN_POINT('Ctrl Pts',(-1.74319473414556,0.338004233132636,
6.87073949345777)) ;
#77446 = CARTESIAN_POINT('Ctrl Pts',(-1.75867139282645,0.343243675639348,
6.93062659534679)) ;
#77447 = CARTESIAN_POINT('Ctrl Pts',(-1.77414072885046,0.348483282365417,
6.99051557427166)) ;
#77448 = CARTESIAN_POINT('',(-1.77414072885046,0.348483282365553,6.99051557427321)) ;
#77449 = CARTESIAN_POINT('',(-1.86979680842779,0.262281765411211,6.97334924403617)) ;
#77450 = CARTESIAN_POINT('Origin',(-1.77414072885046,0.248863812556242,6.99923114854642)) ;
#77451 = CARTESIAN_POINT('',(-1.86979680842779,0.262281765411211,6.97334924403617)) ;
#77452 = CARTESIAN_POINT('',(-1.7277101482095,0.332764968591226,6.81085442572145)) ;
#77453 = CARTESIAN_POINT('Ctrl Pts',(-1.78257449869961,0.351510169545958,
7.00768190451026)) ;
#77454 = CARTESIAN_POINT('Ctrl Pts',(-1.7799529947877,0.349998638179875,7.0020407926548)) ;
#77455 = CARTESIAN_POINT('Ctrl Pts',(-1.77712384321888,0.348988486534698,
6.99629008435115)) ;
#77456 = CARTESIAN_POINT('Ctrl Pts',(-1.77414072885046,0.348483282365553,
6.99051557427321)) ;
#77457 = CARTESIAN_POINT('Ctrl Pts',(-1.80804353409323,0.350030692236613,
7.00216042002313)) ;
#77458 = CARTESIAN_POINT('Ctrl Pts',(-1.80562039408462,0.348758544781101,
6.99609033866213)) ;
#77459 = CARTESIAN_POINT('Ctrl Pts',(-1.80298985197567,0.348031691489769,
6.98992923493179)) ;
#77460 = CARTESIAN_POINT('Ctrl Pts',(-1.80022303195211,0.347898342883226,
6.98382968539506)) ;
#77461 = CARTESIAN_POINT('Ctrl Pts',(-1.85235642894571,0.329284001344761,
6.99742306677412)) ;
#77462 = CARTESIAN_POINT('Ctrl Pts',(-1.85025698915433,0.327717973988231,
6.98963152733253)) ;
#77463 = CARTESIAN_POINT('Ctrl Pts',(-1.84798352930075,0.326928615466665,
6.98177037827478)) ;
#77464 = CARTESIAN_POINT('Ctrl Pts',(-1.84556753758067,0.326868345860465,
6.97395707625727)) ;
#77465 = CARTESIAN_POINT('Ctrl Pts',(-1.87439171514777,0.287344043373391,
7.00354079114492)) ;
#77466 = CARTESIAN_POINT('Ctrl Pts',(-1.87202794762724,0.284665751804286,
6.99328116783748)) ;
#77467 = CARTESIAN_POINT('Ctrl Pts',(-1.86945702547209,0.282962222021335,
6.98284900252258)) ;
#77468 = CARTESIAN_POINT('Ctrl Pts',(-1.86674074821325,0.282225326148211,
6.9723937895666)) ;
#77469 = CARTESIAN_POINT('Ctrl Pts',(-1.87819429271644,0.268591723493141,
7.00768190451026)) ;
#77470 = CARTESIAN_POINT('Ctrl Pts',(-1.87559269584777,0.265429455820045,
6.99639968079935)) ;
#77471 = CARTESIAN_POINT('Ctrl Pts',(-1.87277553216535,0.263323474391225,
6.98489826419204)) ;
#77472 = CARTESIAN_POINT('Ctrl Pts',(-1.86979680842779,0.262281765411211,
6.97334924403617)) ;
#77473 = CARTESIAN_POINT('',(-1.78257449869961,0.351510169545958,7.00768190451026)) ;
#77474 = CARTESIAN_POINT('Origin',(-1.74961486676053,0.424101005970564,6.98537442850825)) ;
#77475 = CARTESIAN_POINT('Origin',(-1.78257449869961,0.254917586917051,7.03356380902051)) ;
#77476 = CARTESIAN_POINT('Origin',(-1.8437775962501,0.424925231867001,6.96360853182487)) ;
#77477 = CARTESIAN_POINT('Ctrl Pts',(-1.87819429271644,0.268591723493142,
7.00768190451026)) ;
#77478 = CARTESIAN_POINT('Ctrl Pts',(-1.88761452163364,0.293719598773215,
7.0557603736433)) ;
#77479 = CARTESIAN_POINT('Ctrl Pts',(-1.91803918303173,0.376442517983045,
7.08160457645398)) ;
#77480 = CARTESIAN_POINT('Ctrl Pts',(-1.94251232165803,0.447018030321751,
7.08179767010457)) ;
#77481 = CARTESIAN_POINT('Ctrl Pts',(-1.94270198330611,0.44756277344327,7.0818)) ;
#77482 = CARTESIAN_POINT('Ctrl Pts',(-1.94288959754295,0.448102752174872,
7.0818)) ;
#77483 = CARTESIAN_POINT('Ctrl Pts',(-1.87312418929155,0.293594816666808,
7.00216042002314)) ;
#77484 = CARTESIAN_POINT('Ctrl Pts',(-1.87796531081865,0.311402705036892,
7.04213224265873)) ;
#77485 = CARTESIAN_POINT('Ctrl Pts',(-1.90981006048309,0.381903712030246,
7.08210548357769)) ;
#77486 = CARTESIAN_POINT('Ctrl Pts',(-1.9424029083422,0.447111003798291,7.08179401271422)) ;
#77487 = CARTESIAN_POINT('Ctrl Pts',(-1.94264552853424,0.447607689701659,
7.0818)) ;
#77488 = CARTESIAN_POINT('Ctrl Pts',(-1.94288959754295,0.448102752174872,
7.0818)) ;
#77489 = CARTESIAN_POINT('Ctrl Pts',(-1.84631288834535,0.334523890843312,
6.99742330171556)) ;
#77490 = CARTESIAN_POINT('Ctrl Pts',(-1.85235243119885,0.341052363542256,
7.03081187673423)) ;
#77491 = CARTESIAN_POINT('Ctrl Pts',(-1.89649530788188,0.39165635273821,7.08258953702512)) ;
#77492 = CARTESIAN_POINT('Ctrl Pts',(-1.94220561752678,0.447272672620756,
7.08179067948989)) ;
#77493 = CARTESIAN_POINT('Ctrl Pts',(-1.94254673268347,0.447686293153841,
7.0818)) ;
#77494 = CARTESIAN_POINT('Ctrl Pts',(-1.94288959754295,0.448102752174872,
7.0818)) ;
#77495 = CARTESIAN_POINT('Ctrl Pts',(-1.80167627524482,0.350400561563948,
7.00354079114491)) ;
#77496 = CARTESIAN_POINT('Ctrl Pts',(-1.81914768429023,0.359424731059564,
7.04558504389613)) ;
#77497 = CARTESIAN_POINT('Ctrl Pts',(-1.88400085756141,0.402627171214686,
7.08196334045253)) ;
#77498 = CARTESIAN_POINT('Ctrl Pts',(-1.94200387814168,0.4474277521,7.0817950153739)) ;
#77499 = CARTESIAN_POINT('Ctrl Pts',(-1.9424479368327,0.447764896606022,7.0818)) ;
#77500 = CARTESIAN_POINT('Ctrl Pts',(-1.94288959754295,0.448102752174872,
7.0818)) ;
#77501 = CARTESIAN_POINT('Ctrl Pts',(-1.78257449869961,0.351510169545957,
7.00768190451025)) ;
#77502 = CARTESIAN_POINT('Ctrl Pts',(-1.80491723859567,0.364392756523483,
7.0557603736433)) ;
#77503 = CARTESIAN_POINT('Ctrl Pts',(-1.87864346527326,0.40766425386111,7.08160457645373)) ;
#77504 = CARTESIAN_POINT('Ctrl Pts',(-1.94191743214594,0.447492414836652,
7.08179767010457)) ;
#77505 = CARTESIAN_POINT('Ctrl Pts',(-1.9424055957538,0.447798583799814,7.0818)) ;
#77506 = CARTESIAN_POINT('Ctrl Pts',(-1.94288959754295,0.448102752174872,
7.0818)) ;
#77507 = CARTESIAN_POINT('',(-1.92349887676128,0.435977594947785,7.0810654941764)) ;
#77508 = CARTESIAN_POINT('Ctrl Pts',(-1.78257449869961,0.351510169545957,
7.00768190451025)) ;
#77509 = CARTESIAN_POINT('Ctrl Pts',(-1.80281774439844,0.363182210425264,
7.05124255409984)) ;
#77510 = CARTESIAN_POINT('Ctrl Pts',(-1.8652414202704,0.399800345697346,7.07655121308281)) ;
#77511 = CARTESIAN_POINT('Ctrl Pts',(-1.92349887676128,0.435977594947785,
7.0810654941764)) ;
#77512 = CARTESIAN_POINT('Ctrl Pts',(-1.92349887676128,0.435977594947785,
7.0810654941764)) ;
#77513 = CARTESIAN_POINT('Ctrl Pts',(-1.92954095092606,0.439729657537118,
7.08153368525118)) ;
#77514 = CARTESIAN_POINT('Ctrl Pts',(-1.93553821134988,0.443476977756891,
7.08177820258746)) ;
#77515 = CARTESIAN_POINT('Ctrl Pts',(-1.94191743214594,0.447492414836652,
7.08179767010457)) ;
#77516 = CARTESIAN_POINT('Ctrl Pts',(-1.9424055957538,0.447798583799814,7.0818)) ;
#77517 = CARTESIAN_POINT('Ctrl Pts',(-1.94288959754295,0.448102752174872,
7.0818)) ;
#77518 = CARTESIAN_POINT('Origin',(4.76250000000001,0.448102752174797,6.9818)) ;
#77519 = CARTESIAN_POINT('',(-1.17871069663556,0.348483282365683,6.99051557427477)) ;
#77520 = CARTESIAN_POINT('',(4.76250000000001,0.348483282365622,6.99051557427477)) ;
#77521 = CARTESIAN_POINT('',(-1.17871069663556,0.448102752174857,7.0818)) ;
#77522 = CARTESIAN_POINT('Origin',(-1.17871069663556,0.448102752174857,6.9818)) ;
#77523 = CARTESIAN_POINT('',(4.76250000000001,0.448102752174797,7.0818)) ;
#77524 = CARTESIAN_POINT('Origin',(9.40062917021727E-15,0.508000000000005,
8.8138)) ;
#77525 = CARTESIAN_POINT('',(-1.17558412963153,0.332764968591552,6.81085442572523)) ;
#77526 = CARTESIAN_POINT('',(5.49947457873019E-15,0.33276496859154,6.81085442572523)) ;
#77527 = CARTESIAN_POINT('',(-1.21039177030074,0.507754795155606,8.81099729580349)) ;
#77528 = CARTESIAN_POINT('Origin',(4.4887220033037E-15,0.233145498782365,
6.81957)) ;
#77529 = CARTESIAN_POINT('',(-1.13595304047784,0.233145498782376,6.71957)) ;
#77530 = CARTESIAN_POINT('',(4.4887220033037E-15,0.233145498782365,6.71957)) ;
#77531 = CARTESIAN_POINT('Origin',(-1.13595304047784,0.233145498782377,6.81957)) ;
#77532 = CARTESIAN_POINT('Origin',(9.525,-0.761999999999999,7.0818)) ;
#77533 = CARTESIAN_POINT('',(-0.662097436533287,0.662040915604455,7.08180000837043)) ;
#77534 = CARTESIAN_POINT('',(3.59929774852521,2.42721865129353,7.0818)) ;
#77535 = CARTESIAN_POINT('',(0.,0.662,7.0818)) ;
#77536 = CARTESIAN_POINT('',(-0.662097436318068,-0.66204091586428,7.08180000837054)) ;
#77537 = CARTESIAN_POINT('',(0.,-0.662,7.0818)) ;
#77538 = CARTESIAN_POINT('',(3.86870543215719,-2.5388109676615,7.0818)) ;
#77539 = CARTESIAN_POINT('Ctrl Pts',(-0.611939867549494,0.558026198990156,
6.81085442572523)) ;
#77540 = CARTESIAN_POINT('Ctrl Pts',(-0.606991841672513,0.555410694880575,
6.7615916062195)) ;
#77541 = CARTESIAN_POINT('Ctrl Pts',(-0.55434393568323,0.527581249784821,
6.71957)) ;
#77542 = CARTESIAN_POINT('Ctrl Pts',(-0.497571705638597,0.497571705638616,
6.71957)) ;
#77543 = CARTESIAN_POINT('Ctrl Pts',(-0.587896866738722,0.568073880351635,
6.81179156524867)) ;
#77544 = CARTESIAN_POINT('Ctrl Pts',(-0.584594051674633,0.565801572147184,
6.76779239028237)) ;
#77545 = CARTESIAN_POINT('Ctrl Pts',(-0.545423040383754,0.536502145084297,
6.71957)) ;
#77546 = CARTESIAN_POINT('Ctrl Pts',(-0.497571705638597,0.497571705638616,
6.71957)) ;
#77547 = CARTESIAN_POINT('Ctrl Pts',(-0.568073880351614,0.587896866738742,
6.81179156524867)) ;
#77548 = CARTESIAN_POINT('Ctrl Pts',(-0.565801572147164,0.584594051674654,
6.76779239028237)) ;
#77549 = CARTESIAN_POINT('Ctrl Pts',(-0.536502145084278,0.545423040383773,
6.71957)) ;
#77550 = CARTESIAN_POINT('Ctrl Pts',(-0.497571705638597,0.497571705638616,
6.71957)) ;
#77551 = CARTESIAN_POINT('Ctrl Pts',(-0.558026198990135,0.611939867549514,
6.81085442572523)) ;
#77552 = CARTESIAN_POINT('Ctrl Pts',(-0.555410694880554,0.606991841672533,
6.7615916062195)) ;
#77553 = CARTESIAN_POINT('Ctrl Pts',(-0.527581249784801,0.55434393568325,
6.71957)) ;
#77554 = CARTESIAN_POINT('Ctrl Pts',(-0.497571705638597,0.497571705638616,
6.71957)) ;
#77555 = CARTESIAN_POINT('',(-0.611939867549494,0.558026198990157,6.81085442572523)) ;
#77556 = CARTESIAN_POINT('Origin',(-0.650062588186457,0.65006258818648,6.80213885145047)) ;
#77557 = CARTESIAN_POINT('Origin',(-0.497571705638597,0.497571705638616,6.81957)) ;
#77558 = CARTESIAN_POINT('Origin',(-0.783160989859995,0.783160989860022,8.78984143258953)) ;
#77559 = CARTESIAN_POINT('',(-0.57005647672015,0.623970146151627,6.99051559580133)) ;
#77560 = CARTESIAN_POINT('',(-0.623970146872331,0.57005647538499,6.9905155850314)) ;
#77561 = CARTESIAN_POINT('Origin',(-0.662092866158805,0.662092866158827,6.981800021508)) ;
#77562 = CARTESIAN_POINT('',(-0.745038269223031,0.691124600663699,8.7985570068643)) ;
#77563 = CARTESIAN_POINT('',(-0.691124600663673,0.745038269223056,8.7985570068643)) ;
#77564 = CARTESIAN_POINT('Ctrl Pts',(-0.57023634760258,0.62345266657714,6.99014289219157)) ;
#77565 = CARTESIAN_POINT('Ctrl Pts',(-0.54533484188452,0.683543323877059,
6.99003852336951)) ;
#77566 = CARTESIAN_POINT('Ctrl Pts',(-0.506923472001745,0.787787260371042,
7.04037308986155)) ;
#77567 = CARTESIAN_POINT('Ctrl Pts',(-0.501809041727926,0.824264612279483,
7.14592568521385)) ;
#77568 = CARTESIAN_POINT('Ctrl Pts',(-0.506127211986293,0.824152009463264,
7.19103163220241)) ;
#77569 = CARTESIAN_POINT('Ctrl Pts',(-0.572397806648059,0.624406912457803,
7.01844435877122)) ;
#77570 = CARTESIAN_POINT('Ctrl Pts',(-0.550442551132344,0.677132597440327,
7.01611788185536)) ;
#77571 = CARTESIAN_POINT('Ctrl Pts',(-0.515355266894961,0.771079003376811,
7.05746161336935)) ;
#77572 = CARTESIAN_POINT('Ctrl Pts',(-0.51068146638924,0.803741078261582,
7.15053005046882)) ;
#77573 = CARTESIAN_POINT('Ctrl Pts',(-0.514624648025357,0.80325589553316,
7.19016526188573)) ;
#77574 = CARTESIAN_POINT('Ctrl Pts',(-0.596834402166937,0.63463042661229,
7.06566080704229)) ;
#77575 = CARTESIAN_POINT('Ctrl Pts',(-0.576378560707317,0.673163424606222,
7.06005906508349)) ;
#77576 = CARTESIAN_POINT('Ctrl Pts',(-0.543010521615669,0.747243595992697,
7.08604143012023)) ;
#77577 = CARTESIAN_POINT('Ctrl Pts',(-0.538457963976829,0.772998673862634,
7.15737445737381)) ;
#77578 = CARTESIAN_POINT('Ctrl Pts',(-0.542247535400501,0.772088823972345,
7.18744210330885)) ;
#77579 = CARTESIAN_POINT('Ctrl Pts',(-0.642835376848303,0.653727314049703,
7.08186031165656)) ;
#77580 = CARTESIAN_POINT('Ctrl Pts',(-0.61927398724742,0.684773072748138,
7.07934238671448)) ;
#77581 = CARTESIAN_POINT('Ctrl Pts',(-0.582387971573308,0.742244553421204,
7.10272807520075)) ;
#77582 = CARTESIAN_POINT('Ctrl Pts',(-0.57744327389336,0.762394272353267,
7.15957559967768)) ;
#77583 = CARTESIAN_POINT('Ctrl Pts',(-0.58160171008854,0.761968609441389,
7.18364859166338)) ;
#77584 = CARTESIAN_POINT('Ctrl Pts',(-0.662485200451311,0.661870075855026,
7.08179987236142)) ;
#77585 = CARTESIAN_POINT('Ctrl Pts',(-0.637610174556416,0.691856881100706,
7.08175608902504)) ;
#77586 = CARTESIAN_POINT('Ctrl Pts',(-0.599228555531057,0.743859867172772,
7.10688022713665)) ;
#77587 = CARTESIAN_POINT('Ctrl Pts',(-0.594118370980124,0.762055140291634,
7.15953504564004)) ;
#77588 = CARTESIAN_POINT('Ctrl Pts',(-0.598433070233959,0.761999835561836,
7.18203726714093)) ;
#77589 = CARTESIAN_POINT('Origin',(-0.662092865474104,0.662092867823976,6.98180002156108)) ;
#77590 = CARTESIAN_POINT('',(-0.506191638276483,0.823877279363034,7.19051557427477)) ;
#77591 = CARTESIAN_POINT('Origin',(-0.589034350751103,0.623877279363034,7.19051557427477)) ;
#77592 = CARTESIAN_POINT('Origin',(-0.598228027472806,0.862,7.1818)) ;
#77593 = CARTESIAN_POINT('Origin',(-0.681070739947426,0.662,7.1818)) ;
#77594 = CARTESIAN_POINT('Origin',(-0.787882878836553,0.862,9.1845535952074)) ;
#77595 = CARTESIAN_POINT('',(-0.639686894805695,0.823877279363034,8.60022433223444)) ;
#77596 = CARTESIAN_POINT('Origin',(-0.731723284002018,0.862,8.59150875795967)) ;
#77597 = CARTESIAN_POINT('',(-0.69584648964023,0.823877279363034,9.19326916948217)) ;
#77598 = CARTESIAN_POINT('Origin',(-0.731723284002017,0.862,8.59150875795967)) ;
#77599 = CARTESIAN_POINT('',(-0.745560008319434,0.878300227999278,8.68919625781168)) ;
#77600 = CARTESIAN_POINT('Origin',(-0.731723284002017,0.862,8.59150875795967)) ;
#77601 = CARTESIAN_POINT('Origin',(-0.731723284002017,0.862,8.59150875795967)) ;
#77602 = CARTESIAN_POINT('Origin',(-0.662092866162308,0.66209286616233,6.98180002156031)) ;
#77603 = CARTESIAN_POINT('Origin',(-0.662092866162308,0.66209286616233,6.98180002156031)) ;
#77604 = CARTESIAN_POINT('Origin',(-0.248785852819289,0.600622180002925,6.81957)) ;
#77605 = CARTESIAN_POINT('',(-1.13746140899457,0.340348049204403,6.81085442572523)) ;
#77606 = CARTESIAN_POINT('',(-0.286908573456253,0.692658569199248,6.81085442572523)) ;
#77607 = CARTESIAN_POINT('Origin',(-1.13595304047784,0.233145498782377,6.81957)) ;
#77608 = CARTESIAN_POINT('',(-0.248785852819289,0.600622180002925,6.71957)) ;
#77609 = CARTESIAN_POINT('Origin',(-0.353968116746243,0.854554628096503,8.8138)) ;
#77610 = CARTESIAN_POINT('',(-1.1405879759986,0.356066362978534,6.99051557427477)) ;
#77611 = CARTESIAN_POINT('',(3.63742046916217,2.3351822620972,6.99051557427477)) ;
#77612 = CARTESIAN_POINT('',(-1.17226904966378,0.515337875768457,8.81099729580349)) ;
#77613 = CARTESIAN_POINT('Origin',(0.,0.662,7.1818)) ;
#77614 = CARTESIAN_POINT('Origin',(-1.17871069663556,0.448102752174857,6.9818)) ;
#77615 = CARTESIAN_POINT('Origin',(-1.17871069663556,0.448102752174857,6.9818)) ;
#77616 = CARTESIAN_POINT('Origin',(-1.17871069663556,0.448102752174857,6.9818)) ;
#77617 = CARTESIAN_POINT('Origin',(3.59929774852521,2.42721865129353,6.9818)) ;
#77618 = CARTESIAN_POINT('Origin',(-1.21039177030074,0.607374264964781,8.80228172152873)) ;
#77619 = CARTESIAN_POINT('Origin',(-1.17558412963153,0.432384438400726,6.80213885145047)) ;
#77620 = CARTESIAN_POINT('Ctrl Pts',(-1.17558412963154,0.332764968591552,
6.81085442572523)) ;
#77621 = CARTESIAN_POINT('Ctrl Pts',(-1.17386952959435,0.328455030351476,
6.7615916062195)) ;
#77622 = CARTESIAN_POINT('Ctrl Pts',(-1.15562586963554,0.282596494255549,
6.71957)) ;
#77623 = CARTESIAN_POINT('Ctrl Pts',(-1.13595304047784,0.233145498782377,
6.71957)) ;
#77624 = CARTESIAN_POINT('Ctrl Pts',(-1.16254657695483,0.332784667850045,
6.81107958928014)) ;
#77625 = CARTESIAN_POINT('Ctrl Pts',(-1.16142573132118,0.328698029275187,
6.76307285057327)) ;
#77626 = CARTESIAN_POINT('Ctrl Pts',(-1.14931784407502,0.283851238553283,
6.71957)) ;
#77627 = CARTESIAN_POINT('Ctrl Pts',(-1.13595304047784,0.233145498782377,
6.71957)) ;
#77628 = CARTESIAN_POINT('Ctrl Pts',(-1.14951407564647,0.335376993538169,
6.81107958928014)) ;
#77629 = CARTESIAN_POINT('Ctrl Pts',(-1.14898571310984,0.331172502747851,
6.76307285057327)) ;
#77630 = CARTESIAN_POINT('Ctrl Pts',(-1.14300981851451,0.285105982851016,
6.71957)) ;
#77631 = CARTESIAN_POINT('Ctrl Pts',(-1.13595304047784,0.233145498782377,
6.71957)) ;
#77632 = CARTESIAN_POINT('Ctrl Pts',(-1.13746140899457,0.340348049204403,
6.81085442572523)) ;
#77633 = CARTESIAN_POINT('Ctrl Pts',(-1.13739615091638,0.335710036450645,
6.7615916062195)) ;
#77634 = CARTESIAN_POINT('Ctrl Pts',(-1.13670179295399,0.286360727148749,
6.71957)) ;
#77635 = CARTESIAN_POINT('Ctrl Pts',(-1.13595304047784,0.233145498782377,
6.71957)) ;
#77636 = CARTESIAN_POINT('Ctrl Pts',(-0.506127211989078,-0.82415200945132,
7.19103163217991)) ;
#77637 = CARTESIAN_POINT('Ctrl Pts',(-0.501809041773239,-0.824264612261493,
7.14592568561392)) ;
#77638 = CARTESIAN_POINT('Ctrl Pts',(-0.506923471858881,-0.787787261003788,
7.04037309112128)) ;
#77639 = CARTESIAN_POINT('Ctrl Pts',(-0.545334841097472,-0.683543325948823,
6.99003852412021)) ;
#77640 = CARTESIAN_POINT('Ctrl Pts',(-0.570236346572291,-0.623452669067161,
6.99014289220396)) ;
#77641 = CARTESIAN_POINT('Ctrl Pts',(-0.514624648029491,-0.803255895526575,
7.1901652618658)) ;
#77642 = CARTESIAN_POINT('Ctrl Pts',(-0.510681466432051,-0.803741078245772,
7.15053005081949)) ;
#77643 = CARTESIAN_POINT('Ctrl Pts',(-0.515355266764847,-0.771079003955546,
7.05746161448053)) ;
#77644 = CARTESIAN_POINT('Ctrl Pts',(-0.550442550421403,-0.677132599298618,
7.01611788244042)) ;
#77645 = CARTESIAN_POINT('Ctrl Pts',(-0.572397805740086,-0.624406914644257,
7.01844435868783)) ;
#77646 = CARTESIAN_POINT('Ctrl Pts',(-0.542247535402147,-0.772088823972612,
7.18744210329385)) ;
#77647 = CARTESIAN_POINT('Ctrl Pts',(-0.53845796401558,-0.77299867385038,
7.15737445763862)) ;
#77648 = CARTESIAN_POINT('Ctrl Pts',(-0.543010521485572,-0.747243596469415,
7.08604143097494)) ;
#77649 = CARTESIAN_POINT('Ctrl Pts',(-0.576378560033109,-0.673163426046929,
7.06005906538994)) ;
#77650 = CARTESIAN_POINT('Ctrl Pts',(-0.596834401325316,-0.634630428210077,
7.06566080680978)) ;
#77651 = CARTESIAN_POINT('Ctrl Pts',(-0.581601710084174,-0.761968609442201,
7.18364859165186)) ;
#77652 = CARTESIAN_POINT('Ctrl Pts',(-0.577443273929769,-0.762394272347131,
7.15957559988957)) ;
#77653 = CARTESIAN_POINT('Ctrl Pts',(-0.582387971427533,-0.74224455378735,
7.10272807587653)) ;
#77654 = CARTESIAN_POINT('Ctrl Pts',(-0.619273986488663,-0.684773073873152,
7.07934238702148)) ;
#77655 = CARTESIAN_POINT('Ctrl Pts',(-0.642835375870018,-0.65372731533593,
7.08186031155258)) ;
#77656 = CARTESIAN_POINT('Ctrl Pts',(-0.598433070228347,-0.761999835561857,
7.18203726713029)) ;
#77657 = CARTESIAN_POINT('Ctrl Pts',(-0.594118371016825,-0.762055140288618,
7.15953504583831)) ;
#77658 = CARTESIAN_POINT('Ctrl Pts',(-0.599228555379944,-0.743859867492794,
7.10688022775928)) ;
#77659 = CARTESIAN_POINT('Ctrl Pts',(-0.637610173763258,-0.691856882134678,
7.08175608939188)) ;
#77660 = CARTESIAN_POINT('Ctrl Pts',(-0.662485199416716,-0.661870077095623,
7.08179987235985)) ;
#77661 = CARTESIAN_POINT('',(-0.598228027472817,-0.762,7.1818)) ;
#77662 = CARTESIAN_POINT('Origin',(-0.598228027472817,-0.862,7.1818)) ;
#77663 = CARTESIAN_POINT('Origin',(-0.662092864798467,-0.6620928694553,6.98180002156184)) ;
#77664 = CARTESIAN_POINT('Origin',(-0.681070739947432,-0.662,7.1818)) ;
#77665 = CARTESIAN_POINT('Origin',(-0.78788287883656,-0.862000000000001,9.1845535952074)) ;
#77666 = CARTESIAN_POINT('',(-0.731723284002027,-0.762,8.59150875795967)) ;
#77667 = CARTESIAN_POINT('Origin',(-0.731723284002027,-0.862000000000001,
8.59150875795967)) ;
#77668 = CARTESIAN_POINT('',(-0.78788287883656,-0.762,9.1845535952074)) ;
#77669 = CARTESIAN_POINT('Origin',(-0.731723284002027,-0.862,8.59150875795967)) ;
#77670 = CARTESIAN_POINT('',(-0.745560008319445,-0.878300227999277,8.68919625781168)) ;
#77671 = CARTESIAN_POINT('Origin',(-0.731723284002027,-0.862,8.59150875795967)) ;
#77672 = CARTESIAN_POINT('Origin',(-0.731723284002027,-0.862,8.59150875795967)) ;
#77673 = CARTESIAN_POINT('Origin',(-0.783160989860015,-0.783160989859993,
8.78984143258953)) ;
#77674 = CARTESIAN_POINT('',(-0.623970146870624,-0.570056475383248,6.99051558500572)) ;
#77675 = CARTESIAN_POINT('Origin',(-0.662092866155382,-0.662092866155364,
6.98180002145664)) ;
#77676 = CARTESIAN_POINT('',(-0.611939867549509,-0.558026198990134,6.81085442572523)) ;
#77677 = CARTESIAN_POINT('Origin',(-0.650062588186474,-0.650062588186457,
6.80213885145047)) ;
#77678 = CARTESIAN_POINT('',(-0.74503826922305,-0.691124600663671,8.7985570068643)) ;
#77679 = CARTESIAN_POINT('Ctrl Pts',(-0.558026198990151,-0.611939867549492,
6.81085442572523)) ;
#77680 = CARTESIAN_POINT('Ctrl Pts',(-0.55541069488057,-0.606991841672512,
6.7615916062195)) ;
#77681 = CARTESIAN_POINT('Ctrl Pts',(-0.527581249784816,-0.554343935683229,
6.71957)) ;
#77682 = CARTESIAN_POINT('Ctrl Pts',(-0.497571705638611,-0.497571705638596,
6.71957)) ;
#77683 = CARTESIAN_POINT('Ctrl Pts',(-0.568073880351629,-0.58789686673872,
6.81179156524867)) ;
#77684 = CARTESIAN_POINT('Ctrl Pts',(-0.565801572147179,-0.584594051674632,
6.76779239028237)) ;
#77685 = CARTESIAN_POINT('Ctrl Pts',(-0.536502145084292,-0.545423040383753,
6.71957)) ;
#77686 = CARTESIAN_POINT('Ctrl Pts',(-0.497571705638611,-0.497571705638596,
6.71957)) ;
#77687 = CARTESIAN_POINT('Ctrl Pts',(-0.587896866738737,-0.568073880351612,
6.81179156524867)) ;
#77688 = CARTESIAN_POINT('Ctrl Pts',(-0.584594051674648,-0.565801572147162,
6.76779239028237)) ;
#77689 = CARTESIAN_POINT('Ctrl Pts',(-0.545423040383768,-0.536502145084276,
6.71957)) ;
#77690 = CARTESIAN_POINT('Ctrl Pts',(-0.497571705638611,-0.497571705638596,
6.71957)) ;
#77691 = CARTESIAN_POINT('Ctrl Pts',(-0.611939867549509,-0.558026198990134,
6.81085442572523)) ;
#77692 = CARTESIAN_POINT('Ctrl Pts',(-0.606991841672528,-0.555410694880553,
6.7615916062195)) ;
#77693 = CARTESIAN_POINT('Ctrl Pts',(-0.554343935683244,-0.5275812497848,
6.71957)) ;
#77694 = CARTESIAN_POINT('Ctrl Pts',(-0.497571705638611,-0.497571705638596,
6.71957)) ;
#77695 = CARTESIAN_POINT('Origin',(-0.497571705638611,-0.497571705638596,
6.81957)) ;
#77696 = CARTESIAN_POINT('Origin',(-0.662092866162324,-0.662092866162307,
6.98180002156031)) ;
#77697 = CARTESIAN_POINT('Origin',(-0.662092866162324,-0.662092866162307,
6.98180002156031)) ;
#77698 = CARTESIAN_POINT('Origin',(-0.507879677365695,-0.210370650418533,
3.37743570668596)) ;
#77699 = CARTESIAN_POINT('Origin',(-0.517483568940243,-0.214348712560272,
3.376526246514)) ;
#77700 = CARTESIAN_POINT('Origin',(0.,-0.862,3.42553041237115)) ;
#77701 = CARTESIAN_POINT('',(-3.07434158440252,-0.762,7.64111756647598)) ;
#77702 = CARTESIAN_POINT('Origin',(0.,-0.762,3.42553041237115)) ;
#77703 = CARTESIAN_POINT('',(-3.13247669898886,-0.878300227999278,7.72083338058588)) ;
#77704 = CARTESIAN_POINT('Origin',(-3.07434158440252,-0.862,7.64111756647598)) ;
#77705 = CARTESIAN_POINT('Origin',(0.,-0.878300227999278,3.42553041237115)) ;
#77706 = CARTESIAN_POINT('Origin',(-9.525,-0.762,8.72161438184689)) ;
#77707 = CARTESIAN_POINT('',(-3.21546217517793,-0.762,7.36730649953872)) ;
#77708 = CARTESIAN_POINT('',(-3.21546217517793,-0.762,0.)) ;
#77709 = CARTESIAN_POINT('Origin',(-2.94522915997985,-0.762,7.40850798245898)) ;
#77710 = CARTESIAN_POINT('',(0.,-0.762,7.1818)) ;
#77711 = CARTESIAN_POINT('Origin',(0.,-0.662,7.1818)) ;
#77712 = CARTESIAN_POINT('Origin',(-0.353968116746264,-0.854554628096483,
8.8138)) ;
#77713 = CARTESIAN_POINT('',(-1.13746140899458,-0.34034804920437,6.81085442572523)) ;
#77714 = CARTESIAN_POINT('',(-0.286908573456268,-0.692658569199233,6.81085442572523)) ;
#77715 = CARTESIAN_POINT('',(-1.14058797599861,-0.356066362978501,6.99051557427476)) ;
#77716 = CARTESIAN_POINT('',(-1.17226904966379,-0.515337875768421,8.81099729580349)) ;
#77717 = CARTESIAN_POINT('',(3.90682815279416,-2.44677457846517,6.99051557427477)) ;
#77718 = CARTESIAN_POINT('Origin',(-1.17871069663558,-0.448102752174823,6.9818)) ;
#77719 = CARTESIAN_POINT('Origin',(-1.17871069663558,-0.448102752174823,6.9818)) ;
#77720 = CARTESIAN_POINT('Origin',(-1.17871069663558,-0.448102752174823,6.9818)) ;
#77721 = CARTESIAN_POINT('Origin',(3.86870543215719,-2.5388109676615,6.9818)) ;
#77722 = CARTESIAN_POINT('Origin',(-1.21039177030076,-0.607374264964743,8.80228172152873)) ;
#77723 = CARTESIAN_POINT('Origin',(-1.17558412963155,-0.432384438400692,6.80213885145047)) ;
#77724 = CARTESIAN_POINT('Ctrl Pts',(-1.13746140899458,-0.34034804920437,
6.81085442572523)) ;
#77725 = CARTESIAN_POINT('Ctrl Pts',(-1.13739615091639,-0.335710036450613,
6.7615916062195)) ;
#77726 = CARTESIAN_POINT('Ctrl Pts',(-1.136701792954,-0.286360727148716,6.71957)) ;
#77727 = CARTESIAN_POINT('Ctrl Pts',(-1.13595304047785,-0.233145498782344,
6.71957)) ;
#77728 = CARTESIAN_POINT('Ctrl Pts',(-1.14951407564648,-0.335376993538136,
6.81107958928014)) ;
#77729 = CARTESIAN_POINT('Ctrl Pts',(-1.14898571310985,-0.331172502747818,
6.76307285057327)) ;
#77730 = CARTESIAN_POINT('Ctrl Pts',(-1.14300981851452,-0.285105982850983,
6.71957)) ;
#77731 = CARTESIAN_POINT('Ctrl Pts',(-1.13595304047785,-0.233145498782344,
6.71957)) ;
#77732 = CARTESIAN_POINT('Ctrl Pts',(-1.16254657695484,-0.332784667850012,
6.81107958928014)) ;
#77733 = CARTESIAN_POINT('Ctrl Pts',(-1.16142573132119,-0.328698029275153,
6.76307285057327)) ;
#77734 = CARTESIAN_POINT('Ctrl Pts',(-1.14931784407503,-0.283851238553249,
6.71957)) ;
#77735 = CARTESIAN_POINT('Ctrl Pts',(-1.13595304047785,-0.233145498782344,
6.71957)) ;
#77736 = CARTESIAN_POINT('Ctrl Pts',(-1.17558412963155,-0.332764968591518,
6.81085442572523)) ;
#77737 = CARTESIAN_POINT('Ctrl Pts',(-1.17386952959436,-0.328455030351443,
6.7615916062195)) ;
#77738 = CARTESIAN_POINT('Ctrl Pts',(-1.15562586963555,-0.282596494255516,
6.71957)) ;
#77739 = CARTESIAN_POINT('Ctrl Pts',(-1.13595304047785,-0.233145498782344,
6.71957)) ;
#77740 = CARTESIAN_POINT('',(-1.13595304047785,-0.233145498782344,6.71957)) ;
#77741 = CARTESIAN_POINT('Origin',(-1.13595304047785,-0.233145498782344,6.81957)) ;
#77742 = CARTESIAN_POINT('Origin',(-1.13595304047785,-0.233145498782344,6.81957)) ;
#77743 = CARTESIAN_POINT('Origin',(-1.62804631646772E-15,-0.233145498782352,
6.81957)) ;
#77744 = CARTESIAN_POINT('',(-1.62804631646772E-15,-0.233145498782352,6.71957)) ;
#77745 = CARTESIAN_POINT('Origin',(-0.248785852819302,-0.60062218000291,6.81957)) ;
#77746 = CARTESIAN_POINT('',(-0.248785852819302,-0.60062218000291,6.71957)) ;
#77747 = CARTESIAN_POINT('Ctrl Pts',(-3.27942391815487,0.70707706204744,7.03908289042881)) ;
#77748 = CARTESIAN_POINT('Ctrl Pts',(-3.28250258905352,0.697893994312427,
7.03746804394249)) ;
#77749 = CARTESIAN_POINT('Ctrl Pts',(-3.28505418610036,0.68846516745384,7.03662526114751)) ;
#77750 = CARTESIAN_POINT('Ctrl Pts',(-3.2870264093502,0.678916496982226,7.03662526114754)) ;
#77751 = CARTESIAN_POINT('Ctrl Pts',(-3.27140856314617,0.702764080010679,
7.05223037429146)) ;
#77752 = CARTESIAN_POINT('Ctrl Pts',(-3.27436377099682,0.694432640985322,
7.05063990488633)) ;
#77753 = CARTESIAN_POINT('Ctrl Pts',(-3.27680438884804,0.685870405895161,
7.04975105907268)) ;
#77754 = CARTESIAN_POINT('Ctrl Pts',(-3.27867914825949,0.677192417965742,
7.04962706151202)) ;
#77755 = CARTESIAN_POINT('Ctrl Pts',(-3.2602197508559,0.697769125082712,7.06320246322391)) ;
#77756 = CARTESIAN_POINT('Ctrl Pts',(-3.26310028573039,0.690308451268357,
7.0616920887364)) ;
#77757 = CARTESIAN_POINT('Ctrl Pts',(-3.26548225911655,0.682632678233894,
7.0608038408065)) ;
#77758 = CARTESIAN_POINT('Ctrl Pts',(-3.26731641278819,0.674845509970035,
7.06059580486544)) ;
#77759 = CARTESIAN_POINT('Ctrl Pts',(-3.24710198979438,0.692647775796393,
7.07077875440785)) ;
#77760 = CARTESIAN_POINT('Ctrl Pts',(-3.24994267520402,0.685970018257057,
7.06941712332046)) ;
#77761 = CARTESIAN_POINT('Ctrl Pts',(-3.2523024328244,0.679097740077075,7.06859808355775)) ;
#77762 = CARTESIAN_POINT('Ctrl Pts',(-3.25413500684122,0.672122965993735,
7.06837618534763)) ;
#77763 = CARTESIAN_POINT('Ctrl Pts',(3.27942391815487,-0.70707706204744,7.03908289042881)) ;
#77764 = CARTESIAN_POINT('Ctrl Pts',(3.28250258905352,-0.697893994312428,
7.03746804394249)) ;
#77765 = CARTESIAN_POINT('Ctrl Pts',(3.28505418610036,-0.68846516745384,7.03662526114751)) ;
#77766 = CARTESIAN_POINT('Ctrl Pts',(3.2870264093502,-0.678916496982227,7.03662526114754)) ;
#77767 = CARTESIAN_POINT('Ctrl Pts',(3.27140856314617,-0.70276408001068,7.05223037429146)) ;
#77768 = CARTESIAN_POINT('Ctrl Pts',(3.27436377099682,-0.694432640985322,
7.05063990488633)) ;
#77769 = CARTESIAN_POINT('Ctrl Pts',(3.27680438884804,-0.685870405895162,
7.04975105907268)) ;
#77770 = CARTESIAN_POINT('Ctrl Pts',(3.2786791482595,-0.677192417965742,7.04962706151202)) ;
#77771 = CARTESIAN_POINT('Ctrl Pts',(3.2602197508559,-0.697769125082713,7.0632024632239)) ;
#77772 = CARTESIAN_POINT('Ctrl Pts',(3.26310028573039,-0.690308451268358,
7.0616920887364)) ;
#77773 = CARTESIAN_POINT('Ctrl Pts',(3.26548225911656,-0.682632678233895,
7.0608038408065)) ;
#77774 = CARTESIAN_POINT('Ctrl Pts',(3.26731641278819,-0.674845509970036,
7.06059580486544)) ;
#77775 = CARTESIAN_POINT('Ctrl Pts',(3.24710198979438,-0.692647775796394,
7.07077875440784)) ;
#77776 = CARTESIAN_POINT('Ctrl Pts',(3.24994267520403,-0.685970018257058,
7.06941712332046)) ;
#77777 = CARTESIAN_POINT('Ctrl Pts',(3.2523024328244,-0.679097740077076,7.06859808355775)) ;
#77778 = CARTESIAN_POINT('Ctrl Pts',(3.25413500684123,-0.672122965993735,
7.06837618534763)) ;
#77779 = CARTESIAN_POINT('Origin',(0.,0.662,7.1818)) ;
#77780 = CARTESIAN_POINT('',(0.662097436318065,0.662040915864284,7.08180000837054)) ;
#77781 = CARTESIAN_POINT('',(0.,0.662,7.0818)) ;
#77782 = CARTESIAN_POINT('',(0.598228027472816,0.762,7.1818)) ;
#77783 = CARTESIAN_POINT('',(0.,0.762,7.1818)) ;
#77784 = CARTESIAN_POINT('Origin',(0.681070739947433,0.662,7.1818)) ;
#77785 = CARTESIAN_POINT('Ctrl Pts',(1.94288959754296,0.448102752174838,7.0818)) ;
#77786 = CARTESIAN_POINT('Ctrl Pts',(1.94270197516852,0.447562750019821,7.0818)) ;
#77787 = CARTESIAN_POINT('Ctrl Pts',(1.94251230527809,0.447017983233615,7.08179766992681)) ;
#77788 = CARTESIAN_POINT('Ctrl Pts',(1.91803916779423,0.376442475910995,7.08160456336037)) ;
#77789 = CARTESIAN_POINT('Ctrl Pts',(1.88761451839117,0.293719590124098,7.05576035709455)) ;
#77790 = CARTESIAN_POINT('Ctrl Pts',(1.87819429271644,0.268591723493114,7.00768190451025)) ;
#77791 = CARTESIAN_POINT('Ctrl Pts',(1.94288959754296,0.448102752174838,7.0818)) ;
#77792 = CARTESIAN_POINT('Ctrl Pts',(1.94252901127699,0.447573785115438,7.0818)) ;
#77793 = CARTESIAN_POINT('Ctrl Pts',(1.94238760925022,0.447241733482732,7.08171624908905)) ;
#77794 = CARTESIAN_POINT('Ctrl Pts',(1.90274378880158,0.385137079186532,7.08429620486543)) ;
#77795 = CARTESIAN_POINT('Ctrl Pts',(1.86635603372516,0.320809755584945,7.03323707646533)) ;
#77796 = CARTESIAN_POINT('Ctrl Pts',(1.86932161172288,0.312347136547031,6.99801930665779)) ;
#77797 = CARTESIAN_POINT('Ctrl Pts',(1.94288959754296,0.448102752174838,7.0818)) ;
#77798 = CARTESIAN_POINT('Ctrl Pts',(1.94245161464468,0.447640464230166,7.0818)) ;
#77799 = CARTESIAN_POINT('Ctrl Pts',(1.94216670833305,0.447413283195622,7.08171624908906)) ;
#77800 = CARTESIAN_POINT('Ctrl Pts',(1.89052514973493,0.394910453254149,7.08429620486524)) ;
#77801 = CARTESIAN_POINT('Ctrl Pts',(1.83473895434066,0.347957809715557,7.03323707646533)) ;
#77802 = CARTESIAN_POINT('Ctrl Pts',(1.82714531063844,0.348921084254577,6.99801930665779)) ;
#77803 = CARTESIAN_POINT('Ctrl Pts',(1.94288959754296,0.448102752174838,7.0818)) ;
#77804 = CARTESIAN_POINT('Ctrl Pts',(1.94240557475948,0.447798570604672,7.0818)) ;
#77805 = CARTESIAN_POINT('Ctrl Pts',(1.94191738994558,0.447492388347723,7.08179766992681)) ;
#77806 = CARTESIAN_POINT('Ctrl Pts',(1.878643427677,0.407664231473883,7.08160456336017)) ;
#77807 = CARTESIAN_POINT('Ctrl Pts',(1.80491723090524,0.364392752089233,7.05576035709455)) ;
#77808 = CARTESIAN_POINT('Ctrl Pts',(1.78257449869961,0.351510169545931,7.00768190451025)) ;
#77809 = CARTESIAN_POINT('',(1.78257449869961,0.351510169545931,7.00768190451025)) ;
#77810 = CARTESIAN_POINT('',(1.87819429271644,0.268591723493114,7.00768190451025)) ;
#77811 = CARTESIAN_POINT('Origin',(1.78257449869961,0.254917586917024,7.0335638090205)) ;
#77812 = CARTESIAN_POINT('',(1.89249580907308,0.307272596056854,7.04638255392016)) ;
#77813 = CARTESIAN_POINT('Origin',(1.98523598941849,0.564759059985062,6.94301769845579)) ;
#77814 = CARTESIAN_POINT('',(1.91807183824094,0.377810206871834,7.07388013397756)) ;
#77815 = CARTESIAN_POINT('Origin',(1.93654302938549,0.434616459002425,6.9972761880138)) ;
#77816 = CARTESIAN_POINT('',(1.94182783334034,0.445044808441076,7.08178867415542)) ;
#77817 = CARTESIAN_POINT('Origin',(1.9279516251551,0.413874762390893,7.02228347027605)) ;
#77818 = CARTESIAN_POINT('',(1.94288959754296,0.448102752174838,7.0818)) ;
#77819 = CARTESIAN_POINT('',(1.94182783307285,0.445044807670698,7.08178867415257)) ;
#77820 = CARTESIAN_POINT('',(1.94014976372696,0.446380214140472,7.08178692473713)) ;
#77821 = CARTESIAN_POINT('',(1.94288959754296,0.448102752174838,7.0818)) ;
#77822 = CARTESIAN_POINT('',(1.87964216949001,0.409078843672791,7.0738290317143)) ;
#77823 = CARTESIAN_POINT('Origin',(1.92743649785841,0.446270284394762,6.99208610030143)) ;
#77824 = CARTESIAN_POINT('',(1.81813539254237,0.372312156583862,7.04714690179995)) ;
#77825 = CARTESIAN_POINT('Origin',(1.93250408796308,0.444533930106968,6.99487389855795)) ;
#77826 = CARTESIAN_POINT('Origin',(2.04686400774823,0.509803748843894,6.9414017611276)) ;
#77827 = CARTESIAN_POINT('Ctrl Pts',(1.87819429271644,0.268591723493114,7.00768190451025)) ;
#77828 = CARTESIAN_POINT('Ctrl Pts',(1.87559269584779,0.265429455820039,6.99639968079942)) ;
#77829 = CARTESIAN_POINT('Ctrl Pts',(1.87277553216538,0.263323474391224,6.98489826419217)) ;
#77830 = CARTESIAN_POINT('Ctrl Pts',(1.86979680842785,0.262281765411205,6.97334924403639)) ;
#77831 = CARTESIAN_POINT('Ctrl Pts',(1.87312418929155,0.293594816666781,7.00216042002313)) ;
#77832 = CARTESIAN_POINT('Ctrl Pts',(1.87084473493899,0.291084530404676,6.99224479183831)) ;
#77833 = CARTESIAN_POINT('Ctrl Pts',(1.86834496343776,0.289501530632332,6.9821612484371)) ;
#77834 = CARTESIAN_POINT('Ctrl Pts',(1.86572206147513,0.288873179727197,6.9720753047436)) ;
#77835 = CARTESIAN_POINT('Ctrl Pts',(1.84631328088201,0.334524427261367,6.99742306677411)) ;
#77836 = CARTESIAN_POINT('Ctrl Pts',(1.84417962418044,0.333091612281766,6.98998909901152)) ;
#77837 = CARTESIAN_POINT('Ctrl Pts',(1.84187319629001,0.332400676673115,6.98249471608034)) ;
#77838 = CARTESIAN_POINT('Ctrl Pts',(1.8394212036961,0.332407181519421,6.97506009028094)) ;
#77839 = CARTESIAN_POINT('Ctrl Pts',(1.80167627524482,0.350400561563922,7.00354079114491)) ;
#77840 = CARTESIAN_POINT('Ctrl Pts',(1.79920012229604,0.349063108054388,6.99757511629261)) ;
#77841 = CARTESIAN_POINT('Ctrl Pts',(1.79652736146151,0.34827651613047,6.99152359092133)) ;
#77842 = CARTESIAN_POINT('Ctrl Pts',(1.79370245617676,0.348044577753787,6.98550115761471)) ;
#77843 = CARTESIAN_POINT('Ctrl Pts',(1.78257449869961,0.351510169545931,7.00768190451025)) ;
#77844 = CARTESIAN_POINT('Ctrl Pts',(1.77995299478772,0.349998638179859,7.00204079265484)) ;
#77845 = CARTESIAN_POINT('Ctrl Pts',(1.77712384321892,0.348988486534684,6.99629008435121)) ;
#77846 = CARTESIAN_POINT('Ctrl Pts',(1.77414072885052,0.348483282365537,6.99051557427332)) ;
#77847 = CARTESIAN_POINT('',(1.77414072885052,0.3484832823656,6.99051557427404)) ;
#77848 = CARTESIAN_POINT('',(1.86979680842785,0.262281765411205,6.97334924403639)) ;
#77849 = CARTESIAN_POINT('Origin',(1.77414072885052,0.248863812556236,6.99923114854664)) ;
#77850 = CARTESIAN_POINT('Origin',(1.84377759624484,0.424925231893568,6.96360853181849)) ;
#77851 = CARTESIAN_POINT('Origin',(1.74961486665444,0.424101006244594,6.98537442845805)) ;
#77852 = CARTESIAN_POINT('Ctrl Pts',(1.72771014821069,0.332764968591604,6.81085442572606)) ;
#77853 = CARTESIAN_POINT('Ctrl Pts',(1.74319473414637,0.338004233132887,6.87073949346092)) ;
#77854 = CARTESIAN_POINT('Ctrl Pts',(1.75867139282689,0.34324367563947,6.93062659534848)) ;
#77855 = CARTESIAN_POINT('Ctrl Pts',(1.77414072885052,0.348483282365411,6.99051557427187)) ;
#77856 = CARTESIAN_POINT('Ctrl Pts',(1.75388379891737,0.332177363448692,6.8041380682092)) ;
#77857 = CARTESIAN_POINT('Ctrl Pts',(1.76933665987703,0.337416538558256,6.86403381882679)) ;
#77858 = CARTESIAN_POINT('Ctrl Pts',(1.78478377705795,0.342658817604018,6.92393065445535)) ;
#77859 = CARTESIAN_POINT('Ctrl Pts',(1.80022303195212,0.347898342882986,6.98382968539381)) ;
#77860 = CARTESIAN_POINT('Ctrl Pts',(1.79938284222813,0.310992589547749,6.79422672914133)) ;
#77861 = CARTESIAN_POINT('Ctrl Pts',(1.81478360859012,0.316286258253241,6.8541354548437)) ;
#77862 = CARTESIAN_POINT('Ctrl Pts',(1.83017778759028,0.321577463411819,6.91404581861776)) ;
#77863 = CARTESIAN_POINT('Ctrl Pts',(1.84556760072686,0.326868409115694,6.97395705441164)) ;
#77864 = CARTESIAN_POINT('Ctrl Pts',(1.82046616955569,0.266091328799232,6.79270352788323)) ;
#77865 = CARTESIAN_POINT('Ctrl Pts',(1.83589739021255,0.271473267897874,6.8525986516149)) ;
#77866 = CARTESIAN_POINT('Ctrl Pts',(1.85132258737849,0.276850760615254,6.91249534127326)) ;
#77867 = CARTESIAN_POINT('Ctrl Pts',(1.86674074821324,0.282225326148124,6.97239378956652)) ;
#77868 = CARTESIAN_POINT('Ctrl Pts',(1.82343508275095,0.246063080838898,6.79368809549057)) ;
#77869 = CARTESIAN_POINT('Ctrl Pts',(1.83889654046911,0.251473735590694,6.85357316322543)) ;
#77870 = CARTESIAN_POINT('Ctrl Pts',(1.85435024060408,0.256879845047591,6.91346026511299)) ;
#77871 = CARTESIAN_POINT('Ctrl Pts',(1.86979680842785,0.262281765411205,6.97334924403639)) ;
#77872 = CARTESIAN_POINT('',(1.72771014821069,0.332764968591568,6.81085442572565)) ;
#77873 = CARTESIAN_POINT('',(1.77414072885052,0.348483282365411,6.99051557427187)) ;
#77874 = CARTESIAN_POINT('',(1.82343508275095,0.246063080838898,6.79368809549016)) ;
#77875 = CARTESIAN_POINT('Origin',(1.72771014821069,0.23314549878243,6.81957000000082)) ;
#77876 = CARTESIAN_POINT('',(1.82343508275095,0.246063080838898,6.79368809549057)) ;
#77877 = CARTESIAN_POINT('Origin',(1.72771014821048,0.233145498782358,6.81957)) ;
#77878 = CARTESIAN_POINT('',(1.72771014821048,0.233145498782358,6.71957)) ;
#77879 = CARTESIAN_POINT('Origin',(1.72771014821048,0.233145498782358,6.81957)) ;
#77880 = CARTESIAN_POINT('Origin',(1.72771014821048,0.233145498782358,6.81957)) ;
#77881 = CARTESIAN_POINT('Origin',(0.,0.507999999999997,8.8138)) ;
#77882 = CARTESIAN_POINT('',(1.17871069663557,0.348483282365664,6.99051557427477)) ;
#77883 = CARTESIAN_POINT('',(4.7625,0.348483282365664,6.99051557427477)) ;
#77884 = CARTESIAN_POINT('',(1.17558412963154,0.332764968591532,6.81085442572523)) ;
#77885 = CARTESIAN_POINT('',(1.21039177030075,0.507754795155586,8.81099729580349)) ;
#77886 = CARTESIAN_POINT('',(0.,0.332764968591532,6.81085442572523)) ;
#77887 = CARTESIAN_POINT('Origin',(4.7625,0.448102752174838,6.9818)) ;
#77888 = CARTESIAN_POINT('',(1.17871069663557,0.448102752174838,7.0818)) ;
#77889 = CARTESIAN_POINT('',(4.7625,0.448102752174838,7.0818)) ;
#77890 = CARTESIAN_POINT('Origin',(1.17871069663557,0.448102752174838,6.9818)) ;
#77891 = CARTESIAN_POINT('Origin',(0.,0.,6.9818)) ;
#77892 = CARTESIAN_POINT('',(1.87819429271644,-0.268591723493119,7.00768190451025)) ;
#77893 = CARTESIAN_POINT('Origin',(0.,-3.71851796272644E-17,7.00768190451025)) ;
#77894 = CARTESIAN_POINT('',(1.93516376195716,-0.425958697933976,7.08103018110362)) ;
#77895 = CARTESIAN_POINT('Ctrl Pts',(1.93516376195716,-0.425958697933976,
7.08103018110362)) ;
#77896 = CARTESIAN_POINT('Ctrl Pts',(1.91237404550518,-0.3610438318848,7.07642065496821)) ;
#77897 = CARTESIAN_POINT('Ctrl Pts',(1.88670733098015,-0.291299724076243,
7.05113030167638)) ;
#77898 = CARTESIAN_POINT('Ctrl Pts',(1.87819429271644,-0.268591723493119,
7.00768190451025)) ;
#77899 = CARTESIAN_POINT('',(1.94288959754295,-0.448102752174844,7.0818)) ;
#77900 = CARTESIAN_POINT('Ctrl Pts',(1.94288959754296,-0.448102752174824,
7.0818)) ;
#77901 = CARTESIAN_POINT('Ctrl Pts',(1.94270198330657,-0.447562773442322,
7.0818)) ;
#77902 = CARTESIAN_POINT('Ctrl Pts',(1.94251232165841,-0.447018030321371,
7.08179767010457)) ;
#77903 = CARTESIAN_POINT('Ctrl Pts',(1.93998825604565,-0.439739142785562,
7.08177775516637)) ;
#77904 = CARTESIAN_POINT('Ctrl Pts',(1.93759234469349,-0.432876340957351,
7.08152139456908)) ;
#77905 = CARTESIAN_POINT('Ctrl Pts',(1.93516376195716,-0.425958697933976,
7.08103018110362)) ;
#77906 = CARTESIAN_POINT('Origin',(0.,0.,7.0818)) ;
#77907 = CARTESIAN_POINT('Origin',(1.72771014821048,-0.233145498782364,6.81957)) ;
#77908 = CARTESIAN_POINT('',(1.72771014821048,-0.332764968591539,6.81085442572523)) ;
#77909 = CARTESIAN_POINT('',(1.82343508275074,-0.24606308083883,6.79368809548975)) ;
#77910 = CARTESIAN_POINT('Origin',(1.72771014821048,-0.233145498782364,6.81957)) ;
#77911 = CARTESIAN_POINT('',(1.72771014821048,-0.233145498782364,6.71957)) ;
#77912 = CARTESIAN_POINT('Origin',(1.72771014821048,-0.233145498782364,6.81957)) ;
#77913 = CARTESIAN_POINT('Origin',(1.72771014821048,-0.233145498782364,6.81957)) ;
#77914 = CARTESIAN_POINT('Ctrl Pts',(1.82343508274976,-0.246063080838488,
6.79368809548596)) ;
#77915 = CARTESIAN_POINT('Ctrl Pts',(1.8388965404683,-0.251473735590417,6.85357316322228)) ;
#77916 = CARTESIAN_POINT('Ctrl Pts',(1.85435024060365,-0.256879845047446,
6.91346026511131)) ;
#77917 = CARTESIAN_POINT('Ctrl Pts',(1.86979680842779,-0.262281765411192,
6.97334924403617)) ;
#77918 = CARTESIAN_POINT('Ctrl Pts',(1.81947653182275,-0.27276741145227,6.79237533867617)) ;
#77919 = CARTESIAN_POINT('Ctrl Pts',(1.83489694400734,-0.278139250484296,
6.85227406114401)) ;
#77920 = CARTESIAN_POINT('Ctrl Pts',(1.85031405219097,-0.283508230262897,
6.91217346932062)) ;
#77921 = CARTESIAN_POINT('Ctrl Pts',(1.86572206147499,-0.288873179727084,
6.97207530474301)) ;
#77922 = CARTESIAN_POINT('Ctrl Pts',(1.79322013108717,-0.316574402604296,
6.79533188669132)) ;
#77923 = CARTESIAN_POINT('Ctrl Pts',(1.80862659259988,-0.321853195169852,
6.85523985899825)) ;
#77924 = CARTESIAN_POINT('Ctrl Pts',(1.8240260136469,-0.327130342614464,6.91514954549617)) ;
#77925 = CARTESIAN_POINT('Ctrl Pts',(1.83942125592947,-0.332407254608771,
6.97506007039324)) ;
#77926 = CARTESIAN_POINT('Ctrl Pts',(1.74734038623951,-0.332324264734023,
6.8058171575838)) ;
#77927 = CARTESIAN_POINT('Ctrl Pts',(1.76280167491966,-0.337563919259379,
6.86571006109106)) ;
#77928 = CARTESIAN_POINT('Ctrl Pts',(1.77825521655385,-0.342804601986199,
6.92560480456484)) ;
#77929 = CARTESIAN_POINT('Ctrl Pts',(1.79370245617666,-0.34804457775358,6.98550115761311)) ;
#77930 = CARTESIAN_POINT('Ctrl Pts',(1.7277101482095,-0.332764968591207,6.81085442572145)) ;
#77931 = CARTESIAN_POINT('Ctrl Pts',(1.74319473414556,-0.338004233132618,
6.87073949345777)) ;
#77932 = CARTESIAN_POINT('Ctrl Pts',(1.75867139282646,-0.343243675639329,
6.93062659534679)) ;
#77933 = CARTESIAN_POINT('Ctrl Pts',(1.77414072885046,-0.348483282365398,
6.99051557427166)) ;
#77934 = CARTESIAN_POINT('',(1.77414072885046,-0.348483282365534,6.99051557427321)) ;
#77935 = CARTESIAN_POINT('',(1.86979680842779,-0.262281765411192,6.97334924403617)) ;
#77936 = CARTESIAN_POINT('Origin',(1.77414072885046,-0.248863812556223,6.99923114854642)) ;
#77937 = CARTESIAN_POINT('',(1.86979680842779,-0.262281765411192,6.97334924403617)) ;
#77938 = CARTESIAN_POINT('',(1.7277101482095,-0.332764968591207,6.81085442572145)) ;
#77939 = CARTESIAN_POINT('Ctrl Pts',(1.78257449869961,-0.351510169545935,
7.00768190451024)) ;
#77940 = CARTESIAN_POINT('Ctrl Pts',(1.7799529947877,-0.349998638179854,7.00204079265479)) ;
#77941 = CARTESIAN_POINT('Ctrl Pts',(1.77712384321888,-0.348988486534676,
6.99629008435113)) ;
#77942 = CARTESIAN_POINT('Ctrl Pts',(1.77414072885046,-0.348483282365533,
6.9905155742732)) ;
#77943 = CARTESIAN_POINT('Ctrl Pts',(1.80804353409323,-0.350030692236589,
7.00216042002312)) ;
#77944 = CARTESIAN_POINT('Ctrl Pts',(1.80562039408462,-0.348758544781078,
6.99609033866212)) ;
#77945 = CARTESIAN_POINT('Ctrl Pts',(1.80298985197567,-0.348031691489746,
6.98992923493177)) ;
#77946 = CARTESIAN_POINT('Ctrl Pts',(1.80022303195211,-0.347898342883205,
6.98382968539505)) ;
#77947 = CARTESIAN_POINT('Ctrl Pts',(1.85235642894571,-0.329284001344736,
6.9974230667741)) ;
#77948 = CARTESIAN_POINT('Ctrl Pts',(1.85025698915433,-0.327717973988209,
6.98963152733252)) ;
#77949 = CARTESIAN_POINT('Ctrl Pts',(1.84798352930075,-0.326928615466642,
6.98177037827477)) ;
#77950 = CARTESIAN_POINT('Ctrl Pts',(1.84556753758067,-0.326868345860442,
6.97395707625726)) ;
#77951 = CARTESIAN_POINT('Ctrl Pts',(1.87439171514777,-0.287344043373369,
7.00354079114491)) ;
#77952 = CARTESIAN_POINT('Ctrl Pts',(1.87202794762724,-0.284665751804266,
6.99328116783747)) ;
#77953 = CARTESIAN_POINT('Ctrl Pts',(1.86945702547209,-0.282962222021312,
6.98284900252257)) ;
#77954 = CARTESIAN_POINT('Ctrl Pts',(1.86674074821325,-0.282225326148191,
6.97239378956659)) ;
#77955 = CARTESIAN_POINT('Ctrl Pts',(1.87819429271644,-0.268591723493119,
7.00768190451025)) ;
#77956 = CARTESIAN_POINT('Ctrl Pts',(1.87559269584777,-0.265429455820026,
6.99639968079935)) ;
#77957 = CARTESIAN_POINT('Ctrl Pts',(1.87277553216535,-0.263323474391202,
6.98489826419203)) ;
#77958 = CARTESIAN_POINT('Ctrl Pts',(1.86979680842779,-0.262281765411191,
6.97334924403617)) ;
#77959 = CARTESIAN_POINT('',(1.78257449869961,-0.351510169545935,7.00768190451024)) ;
#77960 = CARTESIAN_POINT('Origin',(1.7496148667176,-0.424101006082149,6.98537442848823)) ;
#77961 = CARTESIAN_POINT('Origin',(1.78257449869961,-0.25491758691703,7.0335638090205)) ;
#77962 = CARTESIAN_POINT('Origin',(1.8437775962156,-0.424925232050335,6.96360853179461)) ;
#77963 = CARTESIAN_POINT('Ctrl Pts',(1.87819429271644,-0.268591723493119,
7.00768190451025)) ;
#77964 = CARTESIAN_POINT('Ctrl Pts',(1.88761452163365,-0.293719598773199,
7.05576037364334)) ;
#77965 = CARTESIAN_POINT('Ctrl Pts',(1.91803918302408,-0.376442517994261,
7.08160457645395)) ;
#77966 = CARTESIAN_POINT('Ctrl Pts',(1.94251232165841,-0.447018030321371,
7.08179767010457)) ;
#77967 = CARTESIAN_POINT('Ctrl Pts',(1.94270198330657,-0.447562773442322,
7.0818)) ;
#77968 = CARTESIAN_POINT('Ctrl Pts',(1.94288959754295,-0.448102752174828,
7.0818)) ;
#77969 = CARTESIAN_POINT('Ctrl Pts',(1.87312418929155,-0.293594816666786,
7.00216042002313)) ;
#77970 = CARTESIAN_POINT('Ctrl Pts',(1.87796531081865,-0.311402705036871,
7.04213224265876)) ;
#77971 = CARTESIAN_POINT('Ctrl Pts',(1.90981006047448,-0.381903712040289,
7.08210548357766)) ;
#77972 = CARTESIAN_POINT('Ctrl Pts',(1.94240290834263,-0.447111003797951,
7.08179401271422)) ;
#77973 = CARTESIAN_POINT('Ctrl Pts',(1.94264552853462,-0.447607689700649,
7.0818)) ;
#77974 = CARTESIAN_POINT('Ctrl Pts',(1.94288959754295,-0.448102752174828,
7.0818)) ;
#77975 = CARTESIAN_POINT('Ctrl Pts',(1.84631288834535,-0.334523890843293,
6.99742330171556)) ;
#77976 = CARTESIAN_POINT('Ctrl Pts',(1.85235243119886,-0.341052363542231,
7.03081187673426)) ;
#77977 = CARTESIAN_POINT('Ctrl Pts',(1.89649530787172,-0.391656352746195,
7.08258953702515)) ;
#77978 = CARTESIAN_POINT('Ctrl Pts',(1.9422056175273,-0.447272672620484,7.08179067948988)) ;
#77979 = CARTESIAN_POINT('Ctrl Pts',(1.94254673268371,-0.447686293152721,
7.0818)) ;
#77980 = CARTESIAN_POINT('Ctrl Pts',(1.94288959754295,-0.448102752174828,
7.0818)) ;
#77981 = CARTESIAN_POINT('Ctrl Pts',(1.80167627524483,-0.35040056156393,7.00354079114492)) ;
#77982 = CARTESIAN_POINT('Ctrl Pts',(1.81914768429025,-0.359424731059544,
7.04558504389617)) ;
#77983 = CARTESIAN_POINT('Ctrl Pts',(1.88400085754965,-0.402627171220613,
7.08196334045259)) ;
#77984 = CARTESIAN_POINT('Ctrl Pts',(1.94200387814229,-0.447427752099798,
7.0817950153739)) ;
#77985 = CARTESIAN_POINT('Ctrl Pts',(1.9424479368328,-0.447764896604793,7.0818)) ;
#77986 = CARTESIAN_POINT('Ctrl Pts',(1.94288959754295,-0.448102752174828,
7.0818)) ;
#77987 = CARTESIAN_POINT('Ctrl Pts',(1.78257449869961,-0.351510169545939,
7.00768190451026)) ;
#77988 = CARTESIAN_POINT('Ctrl Pts',(1.8049172385957,-0.364392756523468,7.05576037364334)) ;
#77989 = CARTESIAN_POINT('Ctrl Pts',(1.87864346526083,-0.407664253866157,
7.0816045764537)) ;
#77990 = CARTESIAN_POINT('Ctrl Pts',(1.94191743214658,-0.447492414836479,
7.08179767010457)) ;
#77991 = CARTESIAN_POINT('Ctrl Pts',(1.94240559575384,-0.447798583798538,
7.0818)) ;
#77992 = CARTESIAN_POINT('Ctrl Pts',(1.94288959754295,-0.448102752174828,
7.0818)) ;
#77993 = CARTESIAN_POINT('',(1.92349887676295,-0.435977594951427,7.08106549417672)) ;
#77994 = CARTESIAN_POINT('Ctrl Pts',(1.78257449869961,-0.351510169545939,
7.00768190451026)) ;
#77995 = CARTESIAN_POINT('Ctrl Pts',(1.80281774439894,-0.363182210425523,
7.0512425541009)) ;
#77996 = CARTESIAN_POINT('Ctrl Pts',(1.86524142026312,-0.399800345703204,
7.07655121308398)) ;
#77997 = CARTESIAN_POINT('Ctrl Pts',(1.92349887676295,-0.435977594951427,
7.08106549417672)) ;
#77998 = CARTESIAN_POINT('Ctrl Pts',(1.92349887676295,-0.435977594951427,
7.08106549417672)) ;
#77999 = CARTESIAN_POINT('Ctrl Pts',(1.92954095092715,-0.439729657539593,
7.08153368525129)) ;
#78000 = CARTESIAN_POINT('Ctrl Pts',(1.93553821135059,-0.443476977758118,
7.08177820258746)) ;
#78001 = CARTESIAN_POINT('Ctrl Pts',(1.94191743214658,-0.447492414836479,
7.08179767010457)) ;
#78002 = CARTESIAN_POINT('Ctrl Pts',(1.94240559575384,-0.447798583798538,
7.0818)) ;
#78003 = CARTESIAN_POINT('Ctrl Pts',(1.94288959754295,-0.448102752174832,
7.0818)) ;
#78004 = CARTESIAN_POINT('Origin',(4.7625,-0.448102752174854,6.9818)) ;
#78005 = CARTESIAN_POINT('',(1.17871069663557,-0.348483282365668,6.99051557427477)) ;
#78006 = CARTESIAN_POINT('',(4.7625,-0.348483282365679,6.99051557427477)) ;
#78007 = CARTESIAN_POINT('',(1.17871069663557,-0.448102752174842,7.0818)) ;
#78008 = CARTESIAN_POINT('Origin',(1.17871069663557,-0.448102752174842,6.9818)) ;
#78009 = CARTESIAN_POINT('',(4.7625,-0.448102752174854,7.0818)) ;
#78010 = CARTESIAN_POINT('Origin',(-5.85328412995265E-15,-0.507999999999996,
8.8138)) ;
#78011 = CARTESIAN_POINT('',(1.17558412963154,-0.332764968591537,6.81085442572523)) ;
#78012 = CARTESIAN_POINT('',(-3.17578922261404E-15,-0.332764968591533,6.81085442572523)) ;
#78013 = CARTESIAN_POINT('',(1.21039177030075,-0.507754795155589,8.81099729580349)) ;
#78014 = CARTESIAN_POINT('Origin',(-2.86067568683591E-15,-0.233145498782359,
6.81957)) ;
#78015 = CARTESIAN_POINT('',(1.13595304047784,-0.233145498782362,6.71957)) ;
#78016 = CARTESIAN_POINT('',(-2.86067568683591E-15,-0.233145498782359,6.71957)) ;
#78017 = CARTESIAN_POINT('Origin',(1.13595304047784,-0.233145498782362,6.81957)) ;
#78018 = CARTESIAN_POINT('Origin',(9.525,-0.761999999999999,7.0818)) ;
#78019 = CARTESIAN_POINT('',(4.53079829687583,-0.940377394107333,7.0818)) ;
#78020 = CARTESIAN_POINT('',(0.662097436534802,-0.662040915602625,7.08180000837043)) ;
#78021 = CARTESIAN_POINT('',(4.26139061324377,0.828785077739394,7.0818)) ;
#78022 = CARTESIAN_POINT('',(0.,-0.662,7.0818)) ;
#78023 = CARTESIAN_POINT('Origin',(0.78316098986,-0.783160989860008,8.78984143258953)) ;
#78024 = CARTESIAN_POINT('',(0.570056476721783,-0.62397014614747,6.99051559580155)) ;
#78025 = CARTESIAN_POINT('',(0.623970146872346,-0.570056475384991,6.99051558503157)) ;
#78026 = CARTESIAN_POINT('Origin',(0.662092866158832,-0.662092866158839,6.98180002150834)) ;
#78027 = CARTESIAN_POINT('',(0.611939867549498,-0.558026198990146,6.81085442572523)) ;
#78028 = CARTESIAN_POINT('',(0.745038269223036,-0.691124600663685,8.7985570068643)) ;
#78029 = CARTESIAN_POINT('',(0.558026198990139,-0.611939867549503,6.81085442572523)) ;
#78030 = CARTESIAN_POINT('Origin',(0.650062588186462,-0.650062588186468,6.80213885145047)) ;
#78031 = CARTESIAN_POINT('',(0.691124600663678,-0.745038269223043,8.7985570068643)) ;
#78032 = CARTESIAN_POINT('Ctrl Pts',(0.611939867549498,-0.558026198990146,
6.81085442572523)) ;
#78033 = CARTESIAN_POINT('Ctrl Pts',(0.606991841672517,-0.555410694880565,
6.7615916062195)) ;
#78034 = CARTESIAN_POINT('Ctrl Pts',(0.554343935683234,-0.527581249784811,
6.71957)) ;
#78035 = CARTESIAN_POINT('Ctrl Pts',(0.497571705638601,-0.497571705638606,
6.71957)) ;
#78036 = CARTESIAN_POINT('Ctrl Pts',(0.587896866738726,-0.568073880351624,
6.81179156524867)) ;
#78037 = CARTESIAN_POINT('Ctrl Pts',(0.584594051674637,-0.565801572147174,
6.76779239028237)) ;
#78038 = CARTESIAN_POINT('Ctrl Pts',(0.545423040383758,-0.536502145084287,
6.71957)) ;
#78039 = CARTESIAN_POINT('Ctrl Pts',(0.497571705638601,-0.497571705638606,
6.71957)) ;
#78040 = CARTESIAN_POINT('Ctrl Pts',(0.568073880351618,-0.587896866738732,
6.81179156524867)) ;
#78041 = CARTESIAN_POINT('Ctrl Pts',(0.565801572147168,-0.584594051674643,
6.76779239028237)) ;
#78042 = CARTESIAN_POINT('Ctrl Pts',(0.536502145084281,-0.545423040383763,
6.71957)) ;
#78043 = CARTESIAN_POINT('Ctrl Pts',(0.497571705638601,-0.497571705638606,
6.71957)) ;
#78044 = CARTESIAN_POINT('Ctrl Pts',(0.558026198990139,-0.611939867549503,
6.81085442572523)) ;
#78045 = CARTESIAN_POINT('Ctrl Pts',(0.555410694880558,-0.606991841672523,
6.7615916062195)) ;
#78046 = CARTESIAN_POINT('Ctrl Pts',(0.527581249784805,-0.554343935683239,
6.71957)) ;
#78047 = CARTESIAN_POINT('Ctrl Pts',(0.497571705638601,-0.497571705638606,
6.71957)) ;
#78048 = CARTESIAN_POINT('',(0.497571705638601,-0.497571705638606,6.71957)) ;
#78049 = CARTESIAN_POINT('Origin',(0.497571705638601,-0.497571705638606,6.81957)) ;
#78050 = CARTESIAN_POINT('Origin',(0.497571705638601,-0.497571705638606,6.81957)) ;
#78051 = CARTESIAN_POINT('Ctrl Pts',(0.570211858508875,-0.623522814049366,
6.99019330104746)) ;
#78052 = CARTESIAN_POINT('Ctrl Pts',(0.551534852302403,-0.66859706764791,
6.99013167321749)) ;
#78053 = CARTESIAN_POINT('Ctrl Pts',(0.511323934476222,-0.774035717122834,
7.02669496601772)) ;
#78054 = CARTESIAN_POINT('Ctrl Pts',(0.500393372990465,-0.824248755690896,
7.13090837317487)) ;
#78055 = CARTESIAN_POINT('Ctrl Pts',(0.506135855656206,-0.824114843544343,
7.19096167963447)) ;
#78056 = CARTESIAN_POINT('Ctrl Pts',(0.572389430190026,-0.624473925984885,
7.01847383474068)) ;
#78057 = CARTESIAN_POINT('Ctrl Pts',(0.555919328144446,-0.664025668947801,
7.01674468353812)) ;
#78058 = CARTESIAN_POINT('Ctrl Pts',(0.51946533211283,-0.758487707726383,
7.04555073697094)) ;
#78059 = CARTESIAN_POINT('Ctrl Pts',(0.509392765209136,-0.803866506829236,
7.13733008166825)) ;
#78060 = CARTESIAN_POINT('Ctrl Pts',(0.514637480491472,-0.803235395049625,
7.19010329906211)) ;
#78061 = CARTESIAN_POINT('Ctrl Pts',(0.596834745786804,-0.634684162135971,
7.06567536889322)) ;
#78062 = CARTESIAN_POINT('Ctrl Pts',(0.58148813098266,-0.66359058095359,7.06148755378359)) ;
#78063 = CARTESIAN_POINT('Ctrl Pts',(0.547001094686732,-0.736858584687579,
7.07722761166001)) ;
#78064 = CARTESIAN_POINT('Ctrl Pts',(0.537223579811327,-0.773275882572783,
7.14735866455721)) ;
#78065 = CARTESIAN_POINT('Ctrl Pts',(0.542264225761618,-0.772076546520768,
7.18739432697539)) ;
#78066 = CARTESIAN_POINT('Ctrl Pts',(0.642838623428121,-0.653775168663864,
7.08186803342826)) ;
#78067 = CARTESIAN_POINT('Ctrl Pts',(0.625161390776304,-0.677065029661441,
7.0799917878996)) ;
#78068 = CARTESIAN_POINT('Ctrl Pts',(0.586673015296136,-0.734356346993357,
7.0955665033668)) ;
#78069 = CARTESIAN_POINT('Ctrl Pts',(0.576089846021631,-0.762519575633863,
7.15155633346424)) ;
#78070 = CARTESIAN_POINT('Ctrl Pts',(0.581621154777631,-0.761962620673718,
7.18360960381621)) ;
#78071 = CARTESIAN_POINT('Ctrl Pts',(0.662501876072284,-0.661922887444048,
7.08179967671293)) ;
#78072 = CARTESIAN_POINT('Ctrl Pts',(0.643838531330083,-0.684419215447178,
7.08178088077373)) ;
#78073 = CARTESIAN_POINT('Ctrl Pts',(0.603650630034209,-0.737021368067473,
7.10004943267476)) ;
#78074 = CARTESIAN_POINT('Ctrl Pts',(0.59272586137927,-0.762064059967634,
7.15203867446112)) ;
#78075 = CARTESIAN_POINT('Ctrl Pts',(0.59846509565877,-0.761999983546755,
7.18199944835428)) ;
#78076 = CARTESIAN_POINT('Origin',(0.662092865478666,-0.662092867812963,6.98180002156108)) ;
#78077 = CARTESIAN_POINT('',(0.506191638276484,-0.823877279363035,7.19051557427477)) ;
#78078 = CARTESIAN_POINT('Origin',(0.589034350751103,-0.623877279363035,7.19051557427477)) ;
#78079 = CARTESIAN_POINT('Origin',(0.598228027472807,-0.862,7.1818)) ;
#78080 = CARTESIAN_POINT('Origin',(0.681070739947425,-0.662,7.1818)) ;
#78081 = CARTESIAN_POINT('Origin',(0.703226309181215,-0.862,8.29058094955136)) ;
#78082 = CARTESIAN_POINT('',(0.639686894805695,-0.823877279363035,8.60022433223444)) ;
#78083 = CARTESIAN_POINT('Origin',(0.731723284002017,-0.862,8.59150875795967)) ;
#78084 = CARTESIAN_POINT('',(0.611189919984892,-0.823877279363035,8.29929652382612)) ;
#78085 = CARTESIAN_POINT('Origin',(0.731723284002018,-0.862,8.59150875795967)) ;
#78086 = CARTESIAN_POINT('',(0.745560008319435,-0.878300227999278,8.68919625781168)) ;
#78087 = CARTESIAN_POINT('Origin',(0.731723284002018,-0.862,8.59150875795967)) ;
#78088 = CARTESIAN_POINT('Origin',(0.731723284002018,-0.862,8.59150875795967)) ;
#78089 = CARTESIAN_POINT('Origin',(0.662092866162312,-0.662092866162319,6.98180002156031)) ;
#78090 = CARTESIAN_POINT('Origin',(0.662092866162312,-0.662092866162319,6.98180002156031)) ;
#78091 = CARTESIAN_POINT('Origin',(0.600622180002914,-0.248785852819298,6.81957)) ;
#78092 = CARTESIAN_POINT('',(0.692658569199237,-0.286908573456263,6.81085442572523)) ;
#78093 = CARTESIAN_POINT('',(0.600622180002914,-0.248785852819298,6.71957)) ;
#78094 = CARTESIAN_POINT('Origin',(0.248785852819292,-0.600622180002917,6.81957)) ;
#78095 = CARTESIAN_POINT('',(1.13746140899457,-0.340348049204389,6.81085442572523)) ;
#78096 = CARTESIAN_POINT('',(0.286908573456257,-0.692658569199239,6.81085442572523)) ;
#78097 = CARTESIAN_POINT('Origin',(1.13595304047784,-0.233145498782362,6.81957)) ;
#78098 = CARTESIAN_POINT('',(0.248785852819292,-0.600622180002917,6.71957)) ;
#78099 = CARTESIAN_POINT('Origin',(0.353968116746248,-0.854554628096492,8.8138)) ;
#78100 = CARTESIAN_POINT('',(1.1405879759986,-0.35606636297852,6.99051557427477)) ;
#78101 = CARTESIAN_POINT('',(4.22326789260681,0.920821466935716,6.99051557427477)) ;
#78102 = CARTESIAN_POINT('',(1.17226904966378,-0.515337875768441,8.81099729580349)) ;
#78103 = CARTESIAN_POINT('Origin',(0.,-0.662,7.1818)) ;
#78104 = CARTESIAN_POINT('Origin',(1.17871069663556,-0.448102752174842,6.9818)) ;
#78105 = CARTESIAN_POINT('Origin',(1.17871069663557,-0.448102752174842,6.9818)) ;
#78106 = CARTESIAN_POINT('Origin',(1.17871069663556,-0.448102752174842,6.9818)) ;
#78107 = CARTESIAN_POINT('Origin',(4.26139061324377,0.828785077739394,6.9818)) ;
#78108 = CARTESIAN_POINT('Ctrl Pts',(1.13595304047784,-0.233145498782362,
6.71957)) ;
#78109 = CARTESIAN_POINT('Ctrl Pts',(1.136701792954,-0.286360727148735,6.71957)) ;
#78110 = CARTESIAN_POINT('Ctrl Pts',(1.13739615091638,-0.335710036450631,
6.7615916062195)) ;
#78111 = CARTESIAN_POINT('Ctrl Pts',(1.13746140899457,-0.340348049204389,
6.81085442572523)) ;
#78112 = CARTESIAN_POINT('Ctrl Pts',(1.13595304047784,-0.233145498782362,
6.71957)) ;
#78113 = CARTESIAN_POINT('Ctrl Pts',(1.14300981851451,-0.285105982851002,
6.71957)) ;
#78114 = CARTESIAN_POINT('Ctrl Pts',(1.14898571310984,-0.331172502747836,
6.76307285057327)) ;
#78115 = CARTESIAN_POINT('Ctrl Pts',(1.14951407564647,-0.335376993538154,
6.81107958928014)) ;
#78116 = CARTESIAN_POINT('Ctrl Pts',(1.13595304047784,-0.233145498782362,
6.71957)) ;
#78117 = CARTESIAN_POINT('Ctrl Pts',(1.14931784407502,-0.283851238553268,
6.71957)) ;
#78118 = CARTESIAN_POINT('Ctrl Pts',(1.16142573132119,-0.328698029275172,
6.76307285057327)) ;
#78119 = CARTESIAN_POINT('Ctrl Pts',(1.16254657695483,-0.33278466785003,6.81107958928014)) ;
#78120 = CARTESIAN_POINT('Ctrl Pts',(1.13595304047784,-0.233145498782362,
6.71957)) ;
#78121 = CARTESIAN_POINT('Ctrl Pts',(1.15562586963554,-0.282596494255535,
6.71957)) ;
#78122 = CARTESIAN_POINT('Ctrl Pts',(1.17386952959435,-0.328455030351461,
6.7615916062195)) ;
#78123 = CARTESIAN_POINT('Ctrl Pts',(1.17558412963154,-0.332764968591537,
6.81085442572523)) ;
#78124 = CARTESIAN_POINT('Origin',(1.17558412963154,-0.432384438400711,6.80213885145047)) ;
#78125 = CARTESIAN_POINT('Origin',(1.21039177030075,-0.607374264964764,8.80228172152873)) ;
#78126 = CARTESIAN_POINT('Origin',(0.854554628096488,-0.353968116746257,8.8138)) ;
#78127 = CARTESIAN_POINT('Origin',(0.415843288169369,-0.172247929781575,3.38615128096072)) ;
#78128 = CARTESIAN_POINT('Ctrl Pts',(0.506127211989078,0.824152009451317,
7.1910316321799)) ;
#78129 = CARTESIAN_POINT('Ctrl Pts',(0.501809041773239,0.824264612261489,
7.14592568561393)) ;
#78130 = CARTESIAN_POINT('Ctrl Pts',(0.506923471858882,0.787787261003787,
7.04037309112129)) ;
#78131 = CARTESIAN_POINT('Ctrl Pts',(0.545334841097466,0.683543325948836,
6.99003852412023)) ;
#78132 = CARTESIAN_POINT('Ctrl Pts',(0.570236346572285,0.623452669067181,
6.99014289220396)) ;
#78133 = CARTESIAN_POINT('Ctrl Pts',(0.514624648029491,0.803255895526573,
7.19016526186579)) ;
#78134 = CARTESIAN_POINT('Ctrl Pts',(0.510681466432052,0.803741078245769,
7.15053005081949)) ;
#78135 = CARTESIAN_POINT('Ctrl Pts',(0.515355266764848,0.771079003955546,
7.05746161448055)) ;
#78136 = CARTESIAN_POINT('Ctrl Pts',(0.5504425504214,0.67713259929863,7.01611788244044)) ;
#78137 = CARTESIAN_POINT('Ctrl Pts',(0.57239780574008,0.624406914644273,7.01844435868783)) ;
#78138 = CARTESIAN_POINT('Ctrl Pts',(0.542247535402146,0.772088823972611,
7.18744210329384)) ;
#78139 = CARTESIAN_POINT('Ctrl Pts',(0.538457964015581,0.772998673850379,
7.15737445763862)) ;
#78140 = CARTESIAN_POINT('Ctrl Pts',(0.543010521485573,0.747243596469417,
7.08604143097494)) ;
#78141 = CARTESIAN_POINT('Ctrl Pts',(0.576378560033105,0.673163426046941,
7.06005906538994)) ;
#78142 = CARTESIAN_POINT('Ctrl Pts',(0.59683440132531,0.63463042821009,7.06566080680977)) ;
#78143 = CARTESIAN_POINT('Ctrl Pts',(0.581601710084173,0.761968609442201,
7.18364859165186)) ;
#78144 = CARTESIAN_POINT('Ctrl Pts',(0.577443273929768,0.76239427234713,7.15957559988958)) ;
#78145 = CARTESIAN_POINT('Ctrl Pts',(0.582387971427533,0.74224455378735,7.10272807587653)) ;
#78146 = CARTESIAN_POINT('Ctrl Pts',(0.619273986488659,0.68477307387316,7.07934238702147)) ;
#78147 = CARTESIAN_POINT('Ctrl Pts',(0.64283537587001,0.65372731533594,7.08186031155257)) ;
#78148 = CARTESIAN_POINT('Ctrl Pts',(0.598433070228347,0.761999835561857,
7.18203726713029)) ;
#78149 = CARTESIAN_POINT('Ctrl Pts',(0.594118371016825,0.762055140288617,
7.15953504583831)) ;
#78150 = CARTESIAN_POINT('Ctrl Pts',(0.599228555379945,0.743859867492796,
7.1068802277593)) ;
#78151 = CARTESIAN_POINT('Ctrl Pts',(0.637610173763254,0.691856882134685,
7.08175608939188)) ;
#78152 = CARTESIAN_POINT('Ctrl Pts',(0.66248519941671,0.661870077095634,7.08179987235985)) ;
#78153 = CARTESIAN_POINT('Origin',(0.598228027472816,0.862,7.1818)) ;
#78154 = CARTESIAN_POINT('Origin',(0.662092864798463,0.66209286945531,6.98180002156184)) ;
#78155 = CARTESIAN_POINT('Origin',(0.703226309181224,0.862,8.29058094955135)) ;
#78156 = CARTESIAN_POINT('',(0.731723284002027,0.762,8.59150875795967)) ;
#78157 = CARTESIAN_POINT('Origin',(0.731723284002027,0.862,8.59150875795967)) ;
#78158 = CARTESIAN_POINT('',(0.703226309181224,0.762,8.29058094955135)) ;
#78159 = CARTESIAN_POINT('Origin',(0.731723284002027,0.862,8.59150875795967)) ;
#78160 = CARTESIAN_POINT('',(0.745560008319444,0.878300227999278,8.68919625781167)) ;
#78161 = CARTESIAN_POINT('Origin',(0.731723284002027,0.862,8.59150875795967)) ;
#78162 = CARTESIAN_POINT('Origin',(0.731723284002027,0.862,8.59150875795967)) ;
#78163 = CARTESIAN_POINT('Origin',(0.78316098986001,0.783160989860007,8.78984143258953)) ;
#78164 = CARTESIAN_POINT('',(0.62397014687062,0.570056475383259,6.99051558500572)) ;
#78165 = CARTESIAN_POINT('Origin',(0.662092866155378,0.662092866155375,6.98180002145664)) ;
#78166 = CARTESIAN_POINT('',(0.611939867549505,0.558026198990145,6.81085442572523)) ;
#78167 = CARTESIAN_POINT('Origin',(0.65006258818647,0.650062588186467,6.80213885145047)) ;
#78168 = CARTESIAN_POINT('',(0.745038269223045,0.691124600663685,8.7985570068643)) ;
#78169 = CARTESIAN_POINT('Ctrl Pts',(0.558026198990147,0.611939867549503,
6.81085442572523)) ;
#78170 = CARTESIAN_POINT('Ctrl Pts',(0.555410694880566,0.606991841672522,
6.7615916062195)) ;
#78171 = CARTESIAN_POINT('Ctrl Pts',(0.527581249784812,0.554343935683239,
6.71957)) ;
#78172 = CARTESIAN_POINT('Ctrl Pts',(0.497571705638608,0.497571705638606,
6.71957)) ;
#78173 = CARTESIAN_POINT('Ctrl Pts',(0.568073880351625,0.587896866738731,
6.81179156524867)) ;
#78174 = CARTESIAN_POINT('Ctrl Pts',(0.565801572147175,0.584594051674642,
6.76779239028237)) ;
#78175 = CARTESIAN_POINT('Ctrl Pts',(0.536502145084289,0.545423040383763,
6.71957)) ;
#78176 = CARTESIAN_POINT('Ctrl Pts',(0.497571705638608,0.497571705638606,
6.71957)) ;
#78177 = CARTESIAN_POINT('Ctrl Pts',(0.587896866738733,0.568073880351623,
6.81179156524867)) ;
#78178 = CARTESIAN_POINT('Ctrl Pts',(0.584594051674644,0.565801572147173,
6.76779239028237)) ;
#78179 = CARTESIAN_POINT('Ctrl Pts',(0.545423040383765,0.536502145084287,
6.71957)) ;
#78180 = CARTESIAN_POINT('Ctrl Pts',(0.497571705638608,0.497571705638606,
6.71957)) ;
#78181 = CARTESIAN_POINT('Ctrl Pts',(0.611939867549505,0.558026198990145,
6.81085442572523)) ;
#78182 = CARTESIAN_POINT('Ctrl Pts',(0.606991841672524,0.555410694880564,
6.7615916062195)) ;
#78183 = CARTESIAN_POINT('Ctrl Pts',(0.554343935683241,0.52758124978481,6.71957)) ;
#78184 = CARTESIAN_POINT('Ctrl Pts',(0.497571705638608,0.497571705638606,
6.71957)) ;
#78185 = CARTESIAN_POINT('Origin',(0.497571705638608,0.497571705638606,6.81957)) ;
#78186 = CARTESIAN_POINT('Origin',(0.66209286616232,0.662092866162318,6.98180002156031)) ;
#78187 = CARTESIAN_POINT('Origin',(0.66209286616232,0.662092866162318,6.98180002156031)) ;
#78188 = CARTESIAN_POINT('Origin',(0.507879677365696,0.210370650418538,3.37743570668595)) ;
#78189 = CARTESIAN_POINT('Origin',(0.517483568940244,0.214348712560276,3.376526246514)) ;
#78190 = CARTESIAN_POINT('Origin',(0.,0.862,3.42553041237115)) ;
#78191 = CARTESIAN_POINT('',(3.07434158440252,0.762,7.64111756647598)) ;
#78192 = CARTESIAN_POINT('Origin',(0.,0.762,3.42553041237115)) ;
#78193 = CARTESIAN_POINT('',(3.13247669898886,0.878300227999278,7.72083338058588)) ;
#78194 = CARTESIAN_POINT('Origin',(3.07434158440252,0.862,7.64111756647598)) ;
#78195 = CARTESIAN_POINT('Origin',(0.,0.878300227999278,3.42553041237115)) ;
#78196 = CARTESIAN_POINT('Origin',(-9.525,0.762,8.72161438184689)) ;
#78197 = CARTESIAN_POINT('',(3.21546217517793,0.762,7.36730649953872)) ;
#78198 = CARTESIAN_POINT('',(3.21546217517793,0.762,0.)) ;
#78199 = CARTESIAN_POINT('Ctrl Pts',(3.07434158440252,0.762,7.64111756647598)) ;
#78200 = CARTESIAN_POINT('Ctrl Pts',(3.12354729023977,0.762,7.60523285051226)) ;
#78201 = CARTESIAN_POINT('Ctrl Pts',(3.1930870265562,0.762,7.51957043397612)) ;
#78202 = CARTESIAN_POINT('Ctrl Pts',(3.21546217517793,0.762,7.41298214194023)) ;
#78203 = CARTESIAN_POINT('Ctrl Pts',(3.21546217517793,0.762,7.36730649953872)) ;
#78204 = CARTESIAN_POINT('Origin',(0.353968116746258,0.854554628096494,8.8138)) ;
#78205 = CARTESIAN_POINT('',(1.13746140899458,0.340348049204384,6.81085442572523)) ;
#78206 = CARTESIAN_POINT('',(0.286908573456264,0.692658569199241,6.81085442572523)) ;
#78207 = CARTESIAN_POINT('',(1.14058797599861,0.356066362978515,6.99051557427477)) ;
#78208 = CARTESIAN_POINT('',(1.17226904966379,0.515337875768437,8.81099729580349)) ;
#78209 = CARTESIAN_POINT('',(4.49267557623886,-1.03241378330366,6.99051557427477)) ;
#78210 = CARTESIAN_POINT('Origin',(1.17871069663557,0.448102752174838,6.9818)) ;
#78211 = CARTESIAN_POINT('Origin',(1.17871069663557,0.448102752174838,6.9818)) ;
#78212 = CARTESIAN_POINT('Origin',(1.17871069663557,0.448102752174838,6.9818)) ;
#78213 = CARTESIAN_POINT('Origin',(4.53079829687583,-0.940377394107333,6.9818)) ;
#78214 = CARTESIAN_POINT('Origin',(1.21039177030075,0.60737426496476,8.80228172152873)) ;
#78215 = CARTESIAN_POINT('Origin',(1.17558412963154,0.432384438400707,6.80213885145047)) ;
#78216 = CARTESIAN_POINT('Ctrl Pts',(1.13746140899458,0.340348049204384,6.81085442572523)) ;
#78217 = CARTESIAN_POINT('Ctrl Pts',(1.13739615091639,0.335710036450627,6.7615916062195)) ;
#78218 = CARTESIAN_POINT('Ctrl Pts',(1.136701792954,0.286360727148731,6.71957)) ;
#78219 = CARTESIAN_POINT('Ctrl Pts',(1.13595304047785,0.233145498782358,6.71957)) ;
#78220 = CARTESIAN_POINT('Ctrl Pts',(1.14951407564648,0.33537699353815,6.81107958928014)) ;
#78221 = CARTESIAN_POINT('Ctrl Pts',(1.14898571310985,0.331172502747832,6.76307285057327)) ;
#78222 = CARTESIAN_POINT('Ctrl Pts',(1.14300981851451,0.285105982850998,6.71957)) ;
#78223 = CARTESIAN_POINT('Ctrl Pts',(1.13595304047785,0.233145498782358,6.71957)) ;
#78224 = CARTESIAN_POINT('Ctrl Pts',(1.16254657695484,0.332784667850026,6.81107958928014)) ;
#78225 = CARTESIAN_POINT('Ctrl Pts',(1.16142573132119,0.328698029275168,6.76307285057327)) ;
#78226 = CARTESIAN_POINT('Ctrl Pts',(1.14931784407503,0.283851238553264,6.71957)) ;
#78227 = CARTESIAN_POINT('Ctrl Pts',(1.13595304047785,0.233145498782358,6.71957)) ;
#78228 = CARTESIAN_POINT('Ctrl Pts',(1.17558412963154,0.332764968591532,6.81085442572523)) ;
#78229 = CARTESIAN_POINT('Ctrl Pts',(1.17386952959436,0.328455030351457,6.7615916062195)) ;
#78230 = CARTESIAN_POINT('Ctrl Pts',(1.15562586963554,0.282596494255531,6.71957)) ;
#78231 = CARTESIAN_POINT('Ctrl Pts',(1.13595304047785,0.233145498782358,6.71957)) ;
#78232 = CARTESIAN_POINT('',(1.13595304047785,0.233145498782358,6.71957)) ;
#78233 = CARTESIAN_POINT('Origin',(1.13595304047785,0.233145498782358,6.81957)) ;
#78234 = CARTESIAN_POINT('Origin',(1.13595304047785,0.233145498782358,6.81957)) ;
#78235 = CARTESIAN_POINT('Origin',(0.,0.233145498782358,6.81957)) ;
#78236 = CARTESIAN_POINT('',(0.,0.233145498782358,6.71957)) ;
#78237 = CARTESIAN_POINT('Origin',(0.248785852819299,0.600622180002918,6.81957)) ;
#78238 = CARTESIAN_POINT('',(0.248785852819299,0.600622180002918,6.71957)) ;
#78239 = CARTESIAN_POINT('Origin',(-5.2341907152369E-16,7.49419702465636E-15,
6.81957)) ;
#78240 = CARTESIAN_POINT('Origin',(-5.2341907152369E-16,7.49419702465636E-15,
6.71957)) ;
#78241 = CARTESIAN_POINT('Origin',(-1.38777878078145E-16,7.18180894821816E-15,
6.79368809548975)) ;
#78242 = CARTESIAN_POINT('Origin',(-4.22508734431004E-15,1.88057342394262E-15,
6.81957)) ;
#78243 = CARTESIAN_POINT('Origin',(-4.22508734431004E-15,1.88057342394262E-15,
6.71957)) ;
#78244 = CARTESIAN_POINT('Origin',(-4.65139692566778E-15,2.35922392732846E-15,
6.79368809548975)) ;
#78245 = CARTESIAN_POINT('Origin',(0.,0.,6.81957)) ;
#78246 = CARTESIAN_POINT('Origin',(0.,0.,6.71957)) ;
#78247 = CARTESIAN_POINT('Origin',(0.,-7.43633015083647E-17,6.79368809548975)) ;
#78248 = CARTESIAN_POINT('Origin',(-0.854554628096486,0.353968116746271,8.8138)) ;
#78249 = CARTESIAN_POINT('Origin',(-0.415843288169369,0.172247929781578,3.38615128096072)) ;
#78250 = CARTESIAN_POINT('Origin',(0.,0.,8.8138)) ;
#78251 = CARTESIAN_POINT('Origin',(0.,0.,6.71957)) ;
#78252 = CARTESIAN_POINT('Origin',(0.,-0.862,3.42553041237115)) ;
#78253 = CARTESIAN_POINT('',(3.13247669898886,-0.878300227999278,7.72083338058589)) ;
#78254 = CARTESIAN_POINT('Origin',(0.,-0.878300227999278,3.42553041237115)) ;
#78255 = CARTESIAN_POINT('Origin',(3.07434158440252,-0.862,7.64111756647598)) ;
#78256 = CARTESIAN_POINT('Ctrl Pts',(3.13247669898886,-0.878300227999278,
7.72083338058588)) ;
#78257 = CARTESIAN_POINT('Ctrl Pts',(3.24194772411599,-0.884393761686983,
7.63975239746791)) ;
#78258 = CARTESIAN_POINT('Ctrl Pts',(3.31205160669424,-0.887893661760288,
7.50491108098797)) ;
#78259 = CARTESIAN_POINT('Ctrl Pts',(3.31205160669424,-0.887893661760288,
7.36730649953872)) ;
#78260 = CARTESIAN_POINT('Ctrl Pts',(3.13406331600289,-0.862001836852293,
7.72300897562607)) ;
#78261 = CARTESIAN_POINT('Ctrl Pts',(3.24484531401722,-0.867681983706699,
7.64234029129293)) ;
#78262 = CARTESIAN_POINT('Ctrl Pts',(3.3165712033995,-0.871034506014564,7.50637222518225)) ;
#78263 = CARTESIAN_POINT('Ctrl Pts',(3.3165712033995,-0.871034506014564,7.36730649953872)) ;
#78264 = CARTESIAN_POINT('Ctrl Pts',(3.13236709785152,-0.828113890360543,
7.7206830937248)) ;
#78265 = CARTESIAN_POINT('Ctrl Pts',(3.24344041373217,-0.832362489170559,
7.64188726219099)) ;
#78266 = CARTESIAN_POINT('Ctrl Pts',(3.31655021571401,-0.83498349586979,7.50636187808678)) ;
#78267 = CARTESIAN_POINT('Ctrl Pts',(3.31655021571401,-0.83498349586979,7.36730649953871)) ;
#78268 = CARTESIAN_POINT('Ctrl Pts',(3.11315074038068,-0.778100046144805,
7.69433331199796)) ;
#78269 = CARTESIAN_POINT('Ctrl Pts',(3.21661438879145,-0.779302983062094,
7.62174351094937)) ;
#78270 = CARTESIAN_POINT('Ctrl Pts',(3.28499976832129,-0.780067219187875,
7.49621911028266)) ;
#78271 = CARTESIAN_POINT('Ctrl Pts',(3.28499976832129,-0.780067219187875,
7.36730649953872)) ;
#78272 = CARTESIAN_POINT('Ctrl Pts',(3.08894215024221,-0.762,7.66113809968827)) ;
#78273 = CARTESIAN_POINT('Ctrl Pts',(3.18160442136363,-0.761976718953809,
7.59466385085047)) ;
#78274 = CARTESIAN_POINT('Ctrl Pts',(3.24164385284348,-0.762,7.48231337878088)) ;
#78275 = CARTESIAN_POINT('Ctrl Pts',(3.24164385284348,-0.762,7.36730649953872)) ;
#78276 = CARTESIAN_POINT('Ctrl Pts',(3.07434158440252,-0.762,7.64111756647598)) ;
#78277 = CARTESIAN_POINT('Ctrl Pts',(3.16045156961772,-0.762,7.57831931353947)) ;
#78278 = CARTESIAN_POINT('Ctrl Pts',(3.21546217517793,-0.762,7.47388299847558)) ;
#78279 = CARTESIAN_POINT('Ctrl Pts',(3.21546217517793,-0.762,7.36730649953872)) ;
#78280 = CARTESIAN_POINT('Ctrl Pts',(3.13247669898886,-0.878300227999278,
7.72083338058588)) ;
#78281 = CARTESIAN_POINT('Ctrl Pts',(3.24194772411599,-0.884393761686983,
7.63975239746791)) ;
#78282 = CARTESIAN_POINT('Ctrl Pts',(3.31205160669424,-0.887893661760288,
7.50491108098797)) ;
#78283 = CARTESIAN_POINT('Ctrl Pts',(3.31205160669424,-0.887893661760288,
7.36730649953872)) ;
#78284 = CARTESIAN_POINT('Origin',(0.507879677365692,-0.21037065041854,3.37743570668596)) ;
#78285 = CARTESIAN_POINT('Origin',(0.51748356894024,-0.214348712560278,3.376526246514)) ;
#78286 = CARTESIAN_POINT('Origin',(-4.22508734431003E-15,3.18503882869472E-15,
8.18016875778516)) ;
#78287 = CARTESIAN_POINT('Origin',(-4.3836885553672E-15,3.19189119579733E-15,
8.20605066229541)) ;
#78288 = CARTESIAN_POINT('Origin',(-4.30498280490066E-15,3.24526720351407E-15,
8.27007790985519)) ;
#78289 = CARTESIAN_POINT('Origin',(-3.21546217517793,-0.862,0.)) ;
#78290 = CARTESIAN_POINT('',(-3.31205160669424,-0.887893661760289,7.36730649953872)) ;
#78291 = CARTESIAN_POINT('',(-3.31205160669424,-0.887893661760288,0.)) ;
#78292 = CARTESIAN_POINT('Origin',(-3.21546217517793,-0.862,7.36730649953872)) ;
#78293 = CARTESIAN_POINT('Ctrl Pts',(-3.31205160669424,-0.887893661760288,
7.36730649953872)) ;
#78294 = CARTESIAN_POINT('Ctrl Pts',(-3.31205160669424,-0.887893661760288,
7.50491119623589)) ;
#78295 = CARTESIAN_POINT('Ctrl Pts',(-3.24194781580122,-0.884393766790498,
7.63975232956018)) ;
#78296 = CARTESIAN_POINT('Ctrl Pts',(-3.13247669898886,-0.878300227999278,
7.72083338058588)) ;
#78297 = CARTESIAN_POINT('Ctrl Pts',(-3.3165712033995,-0.871034506014564,
7.36730649953872)) ;
#78298 = CARTESIAN_POINT('Ctrl Pts',(-3.3165712033995,-0.871034506014564,
7.50637234165392)) ;
#78299 = CARTESIAN_POINT('Ctrl Pts',(-3.24484540680043,-0.867681988463991,
7.64234022373052)) ;
#78300 = CARTESIAN_POINT('Ctrl Pts',(-3.13406331600289,-0.862001836852293,
7.72300897562607)) ;
#78301 = CARTESIAN_POINT('Ctrl Pts',(-3.31655021571397,-0.834983495869826,
7.36730649953871)) ;
#78302 = CARTESIAN_POINT('Ctrl Pts',(-3.31655021571397,-0.834983495869826,
7.50636199454979)) ;
#78303 = CARTESIAN_POINT('Ctrl Pts',(-3.24344050675935,-0.832362492728917,
7.64188719619712)) ;
#78304 = CARTESIAN_POINT('Ctrl Pts',(-3.13236709785151,-0.828113890360574,
7.72068309372478)) ;
#78305 = CARTESIAN_POINT('Ctrl Pts',(-3.28499976832123,-0.780067219188007,
7.36730649953872)) ;
#78306 = CARTESIAN_POINT('Ctrl Pts',(-3.28499976832123,-0.780067219188007,
7.49621921825079)) ;
#78307 = CARTESIAN_POINT('Ctrl Pts',(-3.2166144754453,-0.779302984069696,
7.62174345015321)) ;
#78308 = CARTESIAN_POINT('Ctrl Pts',(-3.11315074038065,-0.778100046144912,
7.69433331199791)) ;
#78309 = CARTESIAN_POINT('Ctrl Pts',(-3.24164385284348,-0.762,7.36730649953872)) ;
#78310 = CARTESIAN_POINT('Ctrl Pts',(-3.24164385284348,-0.762,7.48231347510255)) ;
#78311 = CARTESIAN_POINT('Ctrl Pts',(-3.18160449897102,-0.761976718934311,
7.59466379517632)) ;
#78312 = CARTESIAN_POINT('Ctrl Pts',(-3.08894215024221,-0.762,7.66113809968827)) ;
#78313 = CARTESIAN_POINT('Ctrl Pts',(-3.21546217517793,-0.762,7.36730649953872)) ;
#78314 = CARTESIAN_POINT('Ctrl Pts',(-3.21546217517793,-0.762,7.47388308773656)) ;
#78315 = CARTESIAN_POINT('Ctrl Pts',(-3.16045164173738,-0.762,7.57831926094407)) ;
#78316 = CARTESIAN_POINT('Ctrl Pts',(-3.07434158440252,-0.762,7.64111756647598)) ;
#78317 = CARTESIAN_POINT('Ctrl Pts',(-3.31205160669424,-0.887893661760288,
7.36730649953872)) ;
#78318 = CARTESIAN_POINT('Ctrl Pts',(-3.31205160669424,-0.887893661760288,
7.50491119623589)) ;
#78319 = CARTESIAN_POINT('Ctrl Pts',(-3.24194781580122,-0.884393766790498,
7.63975232956018)) ;
#78320 = CARTESIAN_POINT('Ctrl Pts',(-3.13247669898886,-0.878300227999278,
7.72083338058588)) ;
#78321 = CARTESIAN_POINT('Origin',(0.,0.,3.42553041237115)) ;
#78322 = CARTESIAN_POINT('Origin',(0.,-5.74654389008192E-16,7.72083338058588)) ;
#78323 = CARTESIAN_POINT('Origin',(0.,-8.67361737988404E-16,7.36730649953872)) ;
#78324 = CARTESIAN_POINT('Origin',(0.,-7.44125213282148E-16,7.36730649953872)) ;
#78325 = CARTESIAN_POINT('Origin',(0.,0.,0.)) ;
#78326 = CARTESIAN_POINT('Ctrl Pts',(-3.21546217517793,0.762,7.36730649953872)) ;
#78327 = CARTESIAN_POINT('Ctrl Pts',(-3.21546217517793,0.762,7.41298218019493)) ;
#78328 = CARTESIAN_POINT('Ctrl Pts',(-3.19308177554602,0.762,7.51957930543031)) ;
#78329 = CARTESIAN_POINT('Ctrl Pts',(-3.12354733145101,0.762,7.60523282045775)) ;
#78330 = CARTESIAN_POINT('Ctrl Pts',(-3.07434158440252,0.762,7.64111756647598)) ;
#78331 = CARTESIAN_POINT('Ctrl Pts',(-3.23291662695496,0.762,7.36730649953872)) ;
#78332 = CARTESIAN_POINT('Ctrl Pts',(-3.23291662695496,0.762,7.41538680927401)) ;
#78333 = CARTESIAN_POINT('Ctrl Pts',(-3.20919044530172,0.7619991985266,7.52759091140272)) ;
#78334 = CARTESIAN_POINT('Ctrl Pts',(-3.1357727028504,0.761998534434387,7.61717961816928)) ;
#78335 = CARTESIAN_POINT('Ctrl Pts',(-3.08407529496231,0.762,7.65446458861751)) ;
#78336 = CARTESIAN_POINT('Ctrl Pts',(-3.26773265822935,0.771355198514182,
7.36730649953871)) ;
#78337 = CARTESIAN_POINT('Ctrl Pts',(-3.26773265822935,0.771355198514182,
7.42018495670109)) ;
#78338 = CARTESIAN_POINT('Ctrl Pts',(-3.24132584545736,0.771198194794288,
7.54357471788814)) ;
#78339 = CARTESIAN_POINT('Ctrl Pts',(-3.16016819309997,0.770710393590129,
7.6410163084456)) ;
#78340 = CARTESIAN_POINT('Ctrl Pts',(-3.10349960406018,0.770364006601212,
7.6810995169956)) ;
#78341 = CARTESIAN_POINT('Ctrl Pts',(-3.31260641155451,0.816049431227016,
7.36730649953872)) ;
#78342 = CARTESIAN_POINT('Ctrl Pts',(-3.31260641155451,0.816049431227016,
7.42635027754646)) ;
#78343 = CARTESIAN_POINT('Ctrl Pts',(-3.28302099203104,0.815206773658776,
7.56414693052081)) ;
#78344 = CARTESIAN_POINT('Ctrl Pts',(-3.19241201477822,0.812575144026894,
7.67241987682184)) ;
#78345 = CARTESIAN_POINT('Ctrl Pts',(-3.12944289962309,0.81069277169432,7.71667338558099)) ;
#78346 = CARTESIAN_POINT('Ctrl Pts',(-3.31883100175212,0.862604928141702,
7.36730649953872)) ;
#78347 = CARTESIAN_POINT('Ctrl Pts',(-3.31883100175212,0.862604928141702,
7.42724277748668)) ;
#78348 = CARTESIAN_POINT('Ctrl Pts',(-3.2893920752126,0.861258395620179,7.56706915453154)) ;
#78349 = CARTESIAN_POINT('Ctrl Pts',(-3.19856097674223,0.856983205993464,
7.67811414352739)) ;
#78350 = CARTESIAN_POINT('Ctrl Pts',(-3.13485662450991,0.853852641278801,
7.72409677314616)) ;
#78351 = CARTESIAN_POINT('Ctrl Pts',(-3.31205160669424,0.887893661760288,
7.36730649953872)) ;
#78352 = CARTESIAN_POINT('Ctrl Pts',(-3.31205160669424,0.887893661760288,
7.42627994098036)) ;
#78353 = CARTESIAN_POINT('Ctrl Pts',(-3.28354207485051,0.886445036569108,
7.56391115375268)) ;
#78354 = CARTESIAN_POINT('Ctrl Pts',(-3.19503162288163,0.881782250165689,
7.67450135142834)) ;
#78355 = CARTESIAN_POINT('Ctrl Pts',(-3.13247669898886,0.878300227999278,
7.72083338058589)) ;
#78356 = CARTESIAN_POINT('',(-3.13247669898886,0.878300227999279,7.72083338058589)) ;
#78357 = CARTESIAN_POINT('Origin',(-3.07434158440252,0.862,7.64111756647598)) ;
#78358 = CARTESIAN_POINT('Ctrl Pts',(-3.13247669898886,0.878300227999278,
7.72083338058589)) ;
#78359 = CARTESIAN_POINT('Ctrl Pts',(-3.15125721360594,0.879345616021897,
7.7069233748392)) ;
#78360 = CARTESIAN_POINT('Ctrl Pts',(-3.16898822142431,0.880324705415051,
7.69152912899859)) ;
#78361 = CARTESIAN_POINT('Ctrl Pts',(-3.20181219242865,0.882115453804949,
7.65815848336878)) ;
#78362 = CARTESIAN_POINT('Ctrl Pts',(-3.21691237399404,0.882927612145381,
7.6401903396444)) ;
#78363 = CARTESIAN_POINT('Ctrl Pts',(-3.24406613551655,0.88436959350386,7.60211786955277)) ;
#78364 = CARTESIAN_POINT('Ctrl Pts',(-3.25612892273065,0.885000021482306,
7.5820210842502)) ;
#78365 = CARTESIAN_POINT('Ctrl Pts',(-3.27008056843648,0.885725501365387,
7.55390876065276)) ;
#78366 = CARTESIAN_POINT('Ctrl Pts',(-3.2734427045829,0.885900005481902,7.54664209868898)) ;
#78367 = CARTESIAN_POINT('Ctrl Pts',(-3.28536345129656,0.886519241337546,
7.51890596267789)) ;
#78368 = CARTESIAN_POINT('Ctrl Pts',(-3.29258331858232,0.886895069252813,
7.49782797698803)) ;
#78369 = CARTESIAN_POINT('Ctrl Pts',(-3.30372575706298,0.887471400743178,
7.45480156534341)) ;
#78370 = CARTESIAN_POINT('Ctrl Pts',(-3.30765080218502,0.887672045043684,
7.43285457715974)) ;
#78371 = CARTESIAN_POINT('Ctrl Pts',(-3.31132435060191,0.887857745113204,
7.39630625236233)) ;
#78372 = CARTESIAN_POINT('Ctrl Pts',(-3.31205160669424,0.887893661760288,
7.38180486361516)) ;
#78373 = CARTESIAN_POINT('Ctrl Pts',(-3.31205160669424,0.887893661760288,
7.36730649953872)) ;
#78374 = CARTESIAN_POINT('Origin',(0.,0.862,3.42553041237115)) ;
#78375 = CARTESIAN_POINT('Origin',(0.,0.878300227999278,3.42553041237115)) ;
#78376 = CARTESIAN_POINT('Origin',(-0.507879677365692,0.210370650418544,3.37743570668596)) ;
#78377 = CARTESIAN_POINT('Origin',(-0.51748356894024,0.214348712560283,3.376526246514)) ;
#78378 = CARTESIAN_POINT('Origin',(-0.135929041739323,1.4180803283024E-15,
3.41363816217501)) ;
#78379 = CARTESIAN_POINT('Origin',(-0.138499429641961,1.44489591144929E-15,
3.41341328237267)) ;
#78380 = CARTESIAN_POINT('Ctrl Pts',(3.07434158440252,0.762,7.64111756647598)) ;
#78381 = CARTESIAN_POINT('Ctrl Pts',(3.12354729023977,0.762,7.60523285051226)) ;
#78382 = CARTESIAN_POINT('Ctrl Pts',(3.1930870265562,0.762,7.51957043397612)) ;
#78383 = CARTESIAN_POINT('Ctrl Pts',(3.21546217517793,0.762,7.41298214194023)) ;
#78384 = CARTESIAN_POINT('Ctrl Pts',(3.21546217517793,0.762,7.36730649953872)) ;
#78385 = CARTESIAN_POINT('Ctrl Pts',(3.08407529496231,0.762,7.65446458861751)) ;
#78386 = CARTESIAN_POINT('Ctrl Pts',(3.13577265955232,0.761998534435614,7.61717964939652)) ;
#78387 = CARTESIAN_POINT('Ctrl Pts',(3.20919599213541,0.761999198366373,7.52758160791742)) ;
#78388 = CARTESIAN_POINT('Ctrl Pts',(3.23291662695496,0.762,7.41538676900536)) ;
#78389 = CARTESIAN_POINT('Ctrl Pts',(3.23291662695496,0.762,7.36730649953872)) ;
#78390 = CARTESIAN_POINT('Ctrl Pts',(3.10349960406021,0.770364006601186,7.68109951699563)) ;
#78391 = CARTESIAN_POINT('Ctrl Pts',(3.1601681456384,0.770710393299994,7.64101634201648)) ;
#78392 = CARTESIAN_POINT('Ctrl Pts',(3.24133198224179,0.771198231737204,7.54356455202267)) ;
#78393 = CARTESIAN_POINT('Ctrl Pts',(3.2677326582294,0.771355198514153,7.42018491241385)) ;
#78394 = CARTESIAN_POINT('Ctrl Pts',(3.2677326582294,0.771355198514153,7.36730649953871)) ;
#78395 = CARTESIAN_POINT('Ctrl Pts',(3.12944289962316,0.810692771694295,7.71667338558108)) ;
#78396 = CARTESIAN_POINT('Ctrl Pts',(3.19241196203983,0.812575142450328,7.67241991388553)) ;
#78397 = CARTESIAN_POINT('Ctrl Pts',(3.28302784295196,0.815206972212267,7.56413561454693)) ;
#78398 = CARTESIAN_POINT('Ctrl Pts',(3.31260641155465,0.816049431226997,7.42635022809559)) ;
#78399 = CARTESIAN_POINT('Ctrl Pts',(3.31260641155465,0.816049431226997,7.36730649953872)) ;
#78400 = CARTESIAN_POINT('Ctrl Pts',(3.13485662450991,0.853852641278801,7.72409677314616)) ;
#78401 = CARTESIAN_POINT('Ctrl Pts',(3.19856092338799,0.856983203371525,7.67811418203917)) ;
#78402 = CARTESIAN_POINT('Ctrl Pts',(3.28939894471721,0.861258718801572,7.56705759107582)) ;
#78403 = CARTESIAN_POINT('Ctrl Pts',(3.31883100175212,0.862604928141702,7.42724272728831)) ;
#78404 = CARTESIAN_POINT('Ctrl Pts',(3.31883100175212,0.862604928141702,7.36730649953872)) ;
#78405 = CARTESIAN_POINT('Ctrl Pts',(3.13247669898886,0.878300227999278,7.72083338058588)) ;
#78406 = CARTESIAN_POINT('Ctrl Pts',(3.19503157049007,0.881782247249395,7.67450139023276)) ;
#78407 = CARTESIAN_POINT('Ctrl Pts',(3.2835487590593,0.886445388078747,7.56389969951321)) ;
#78408 = CARTESIAN_POINT('Ctrl Pts',(3.31205160669424,0.887893661760288,7.42627989158839)) ;
#78409 = CARTESIAN_POINT('Ctrl Pts',(3.31205160669424,0.887893661760288,7.36730649953872)) ;
#78410 = CARTESIAN_POINT('',(3.31205160669424,0.887893661760288,7.36730649953872)) ;
#78411 = CARTESIAN_POINT('Origin',(3.21546217517793,0.862,7.36730649953872)) ;
#78412 = CARTESIAN_POINT('Ctrl Pts',(3.31205160669424,0.887893661760288,7.36730649953872)) ;
#78413 = CARTESIAN_POINT('Ctrl Pts',(3.31205160669424,0.887893661760288,7.38956143771478)) ;
#78414 = CARTESIAN_POINT('Ctrl Pts',(3.31033560020008,0.887808601466395,7.41182249790195)) ;
#78415 = CARTESIAN_POINT('Ctrl Pts',(3.30351690635115,0.887460286770387,7.45583467472282)) ;
#78416 = CARTESIAN_POINT('Ctrl Pts',(3.29841004269922,0.887196799265865,7.47758437086555)) ;
#78417 = CARTESIAN_POINT('Ctrl Pts',(3.28732603928197,0.886621411389359,7.5125396219205)) ;
#78418 = CARTESIAN_POINT('Ctrl Pts',(3.28228994385203,0.886359400067986,7.52605670555331)) ;
#78419 = CARTESIAN_POINT('Ctrl Pts',(3.26737490624966,0.885584721481954,7.56076103741013)) ;
#78420 = CARTESIAN_POINT('Ctrl Pts',(3.25642579234752,0.885016920148674,7.58148532526352)) ;
#78421 = CARTESIAN_POINT('Ctrl Pts',(3.23139243072244,0.883699376658414,7.62095135160198)) ;
#78422 = CARTESIAN_POINT('Ctrl Pts',(3.21730269907916,0.882949261558222,7.63968874680989)) ;
#78423 = CARTESIAN_POINT('Ctrl Pts',(3.18634388333276,0.881275273044124,7.67476016953305)) ;
#78424 = CARTESIAN_POINT('Ctrl Pts',(3.16946465452307,0.88035071777546,7.69108408662551)) ;
#78425 = CARTESIAN_POINT('Ctrl Pts',(3.14525705790316,0.879010759195164,7.71110108522053)) ;
#78426 = CARTESIAN_POINT('Ctrl Pts',(3.13892867704792,0.878659367283939,7.71605464828228)) ;
#78427 = CARTESIAN_POINT('Ctrl Pts',(3.13247669898886,0.878300227999279,7.72083338058589)) ;
#78428 = CARTESIAN_POINT('Origin',(3.21546217517793,0.861999999999999,0.)) ;
#78429 = CARTESIAN_POINT('',(3.31205160669424,0.887893661760288,0.)) ;
#78430 = CARTESIAN_POINT('Origin',(0.,0.,3.42553041237115)) ;
#78431 = CARTESIAN_POINT('Origin',(0.,-5.74654389008192E-16,7.72083338058588)) ;
#78432 = CARTESIAN_POINT('Origin',(0.,-8.67361737988404E-16,7.36730649953872)) ;
#78433 = CARTESIAN_POINT('Origin',(0.,-7.44125213282148E-16,7.36730649953872)) ;
#78434 = CARTESIAN_POINT('Origin',(0.,0.,0.)) ;
#78435 = CARTESIAN_POINT('Origin',(0.,0.,0.5953125)) ;
#78436 = CARTESIAN_POINT('',(-1.56389349909515,6.20727076724186E-13,0.406605999095151)) ;
#78437 = CARTESIAN_POINT('Ctrl Pts',(-1.56389349909515,1.24170639048682E-12,
0.40660599909515)) ;
#78438 = CARTESIAN_POINT('Ctrl Pts',(-1.56745804029789,-0.0734174872881957,
0.410170540297885)) ;
#78439 = CARTESIAN_POINT('Ctrl Pts',(-1.56574208917974,-0.143162522998449,
0.413636286609932)) ;
#78440 = CARTESIAN_POINT('Ctrl Pts',(-1.55193928496058,-0.310682384668358,
0.422105828519627)) ;
#78441 = CARTESIAN_POINT('Ctrl Pts',(-1.53358392757052,-0.412143684651979,
0.427385555715839)) ;
#78442 = CARTESIAN_POINT('Ctrl Pts',(-1.447702417125,-0.715662399845767,0.443633913138531)) ;
#78443 = CARTESIAN_POINT('Ctrl Pts',(-1.34947303687865,-0.906569448029718,
0.454496467611271)) ;
#78444 = CARTESIAN_POINT('Ctrl Pts',(-1.15133056045185,-1.15429653660643,
0.469686241696881)) ;
#78445 = CARTESIAN_POINT('Ctrl Pts',(-1.07768308713858,-1.22969696342727,
0.474530087857337)) ;
#78446 = CARTESIAN_POINT('Ctrl Pts',(-0.836867957885233,-1.43446115704913,
0.489835648281197)) ;
#78447 = CARTESIAN_POINT('Ctrl Pts',(-0.650095663570034,-1.53964452624183,
0.500458351416618)) ;
#78448 = CARTESIAN_POINT('Ctrl Pts',(-0.216304224148064,-1.68393625033617,
0.522791960259464)) ;
#78449 = CARTESIAN_POINT('Ctrl Pts',(0.00797445504568436,-1.70157489439822,
0.532602184785555)) ;
#78450 = CARTESIAN_POINT('Ctrl Pts',(0.39442070359125,-1.67235506214807,0.550645164261604)) ;
#78451 = CARTESIAN_POINT('Ctrl Pts',(0.578381302744751,-1.62749177136662,
0.559673597083784)) ;
#78452 = CARTESIAN_POINT('Ctrl Pts',(0.838857844667483,-1.51645723159726,
0.57311954012989)) ;
#78453 = CARTESIAN_POINT('Ctrl Pts',(0.923066437402856,-1.47199035969867,
0.577586656827061)) ;
#78454 = CARTESIAN_POINT('Ctrl Pts',(1.11065896487304,-1.35208673309619,0.587837823942977)) ;
#78455 = CARTESIAN_POINT('Ctrl Pts',(1.18850492238163,-1.2858292868164,0.592330998254932)) ;
#78456 = CARTESIAN_POINT('Ctrl Pts',(1.23927534453555,-1.23927534486525,0.5953124999899)) ;
#78457 = CARTESIAN_POINT('',(-1.1572875,-1.41726843256824E-16,6.93889390390723E-17)) ;
#78458 = CARTESIAN_POINT('',(-1.7526,-2.14631598018565E-16,0.5953125)) ;
#78459 = CARTESIAN_POINT('Origin',(0.,0.,0.)) ;
#78460 = CARTESIAN_POINT('Ctrl Pts',(0.726199640324296,-1.00145522282725,
0.0797567518095781)) ;
#78461 = CARTESIAN_POINT('Ctrl Pts',(0.85827032683805,-0.91812330569503,0.0898263199638132)) ;
#78462 = CARTESIAN_POINT('Ctrl Pts',(0.966230127421333,-0.81477793631574,
0.0985476242080515)) ;
#78463 = CARTESIAN_POINT('Ctrl Pts',(1.14142047749138,-0.584869602376768,
0.116935473138185)) ;
#78464 = CARTESIAN_POINT('Ctrl Pts',(1.20940238333913,-0.45431006970221,0.126370642327099)) ;
#78465 = CARTESIAN_POINT('Ctrl Pts',(1.31992804059758,-0.108087210236051,
0.14918186937396)) ;
#78466 = CARTESIAN_POINT('Ctrl Pts',(1.320127313916,0.0729480435983187,0.159158271321901)) ;
#78467 = CARTESIAN_POINT('Ctrl Pts',(1.29419866014635,0.367183226884352,0.176917483314036)) ;
#78468 = CARTESIAN_POINT('Ctrl Pts',(1.24602456229177,0.534537805855587,0.187567821710453)) ;
#78469 = CARTESIAN_POINT('Ctrl Pts',(1.06285410240392,0.89276995042693,0.211685938535209)) ;
#78470 = CARTESIAN_POINT('Ctrl Pts',(0.928597035203795,1.02719764559811,0.221685613693348)) ;
#78471 = CARTESIAN_POINT('Ctrl Pts',(0.693985903348748,1.22533564983316,0.239291466200409)) ;
#78472 = CARTESIAN_POINT('Ctrl Pts',(0.534496651620149,1.31426473081559,0.249960727937322)) ;
#78473 = CARTESIAN_POINT('Ctrl Pts',(0.140400650614174,1.44310966165732,0.273743112836897)) ;
#78474 = CARTESIAN_POINT('Ctrl Pts',(-0.0567292878068117,1.44660339865736,
0.283709043024783)) ;
#78475 = CARTESIAN_POINT('Ctrl Pts',(-0.384490687238328,1.42007491780602,
0.301724326338965)) ;
#78476 = CARTESIAN_POINT('Ctrl Pts',(-0.568439624563353,1.36843547863331,
0.312409905281157)) ;
#78477 = CARTESIAN_POINT('Ctrl Pts',(-0.943592421571356,1.17947003346788,
0.335505788342169)) ;
#78478 = CARTESIAN_POINT('Ctrl Pts',(-1.09490202949618,1.04247043391369,0.345447089068427)) ;
#78479 = CARTESIAN_POINT('Ctrl Pts',(-1.32988994898806,0.765621603495837,
0.364510040364269)) ;
#78480 = CARTESIAN_POINT('Ctrl Pts',(-1.42735349524037,0.59169431681732,0.375202747150079)) ;
#78481 = CARTESIAN_POINT('Ctrl Pts',(-1.53569636645461,0.262270120156304,
0.393498668676532)) ;
#78482 = CARTESIAN_POINT('Ctrl Pts',(-1.5577870170388,0.125772867603548,0.400499517038806)) ;
#78483 = CARTESIAN_POINT('Ctrl Pts',(-1.56389349909515,1.24143750834804E-12,
0.406605999095151)) ;
#78484 = CARTESIAN_POINT('Origin',(-4.22508734431003E-15,3.79252875187005E-15,
8.8138)) ;
#78485 = CARTESIAN_POINT('Origin',(4.32558592440026E-16,8.45017468862007E-15,
8.8138)) ;
#78486 = CARTESIAN_POINT('Origin',(0.,0.,0.)) ;
#78487 = CARTESIAN_POINT('Ctrl Pts',(0.,1.23704425180958,-0.396875000000002)) ;
#78488 = CARTESIAN_POINT('Ctrl Pts',(-0.512400506355204,1.23704425180958,
-0.347265625000002)) ;
#78489 = CARTESIAN_POINT('Ctrl Pts',(-0.874722379082389,0.874722379082389,
-0.297656250000002)) ;
#78490 = CARTESIAN_POINT('Ctrl Pts',(-1.23704425180958,0.512400506355204,
-0.248046875000002)) ;
#78491 = CARTESIAN_POINT('Ctrl Pts',(-1.23704425180958,7.57471141691114E-17,
-0.198437500000002)) ;
#78492 = CARTESIAN_POINT('Ctrl Pts',(-1.23704425180958,-0.512400506355204,
-0.148828125000002)) ;
#78493 = CARTESIAN_POINT('Ctrl Pts',(-0.874722379082389,-0.874722379082389,
-0.0992187500000016)) ;
#78494 = CARTESIAN_POINT('Ctrl Pts',(-0.512400506355204,-1.23704425180958,
-0.0496093750000016)) ;
#78495 = CARTESIAN_POINT('Ctrl Pts',(-1.51494228338223E-16,-1.23704425180958,
-1.62630325872826E-15)) ;
#78496 = CARTESIAN_POINT('Ctrl Pts',(0.512400506355204,-1.23704425180958,
0.0496093749999984)) ;
#78497 = CARTESIAN_POINT('Ctrl Pts',(0.874722379082389,-0.87472237908239,
0.0992187499999984)) ;
#78498 = CARTESIAN_POINT('Ctrl Pts',(1.23704425180957,-0.512400506355205,
0.148828124999998)) ;
#78499 = CARTESIAN_POINT('Ctrl Pts',(1.23704425180958,-2.27241342507334E-16,
0.198437499999998)) ;
#78500 = CARTESIAN_POINT('Ctrl Pts',(1.23704425180957,0.512400506355204,0.248046874999998)) ;
#78501 = CARTESIAN_POINT('Ctrl Pts',(0.87472237908239,0.874722379082389,0.297656249999998)) ;
#78502 = CARTESIAN_POINT('Ctrl Pts',(0.512400506355205,1.23704425180957,0.347265624999998)) ;
#78503 = CARTESIAN_POINT('Ctrl Pts',(0.,1.23704425180958,0.396874999999998)) ;
#78504 = CARTESIAN_POINT('Ctrl Pts',(-0.512400506355204,1.23704425180958,
0.446484374999998)) ;
#78505 = CARTESIAN_POINT('Ctrl Pts',(-0.874722379082389,0.874722379082389,
0.496093749999998)) ;
#78506 = CARTESIAN_POINT('Ctrl Pts',(-1.23704425180958,0.512400506355204,
0.545703124999998)) ;
#78507 = CARTESIAN_POINT('Ctrl Pts',(-1.23704425180958,7.57471141691114E-17,
0.595312499999998)) ;
#78508 = CARTESIAN_POINT('Ctrl Pts',(-1.23704425180958,-0.512400506355204,
0.644921874999998)) ;
#78509 = CARTESIAN_POINT('Ctrl Pts',(-0.874722379082389,-0.874722379082389,
0.694531249999998)) ;
#78510 = CARTESIAN_POINT('Ctrl Pts',(-0.512400506355204,-1.23704425180958,
0.744140624999998)) ;
#78511 = CARTESIAN_POINT('Ctrl Pts',(-1.51494228338223E-16,-1.23704425180958,
0.793749999999998)) ;
#78512 = CARTESIAN_POINT('Ctrl Pts',(0.512400506355204,-1.23704425180958,
0.843359374999998)) ;
#78513 = CARTESIAN_POINT('Ctrl Pts',(0.874722379082389,-0.87472237908239,
0.892968749999998)) ;
#78514 = CARTESIAN_POINT('Ctrl Pts',(1.23704425180957,-0.512400506355205,
0.942578124999999)) ;
#78515 = CARTESIAN_POINT('Ctrl Pts',(1.23704425180958,-2.27241342507334E-16,
0.992187499999998)) ;
#78516 = CARTESIAN_POINT('Ctrl Pts',(1.23704425180957,0.512400506355204,1.041796875)) ;
#78517 = CARTESIAN_POINT('Ctrl Pts',(0.87472237908239,0.874722379082389,1.09140625)) ;
#78518 = CARTESIAN_POINT('Ctrl Pts',(0.512400506355205,1.23704425180957,1.141015625)) ;
#78519 = CARTESIAN_POINT('Ctrl Pts',(0.,1.23704425180958,1.190625)) ;
#78520 = CARTESIAN_POINT('Ctrl Pts',(-0.512400506355204,1.23704425180958,
1.240234375)) ;
#78521 = CARTESIAN_POINT('Ctrl Pts',(-0.874722379082389,0.874722379082389,
1.28984375)) ;
#78522 = CARTESIAN_POINT('Ctrl Pts',(-1.23704425180958,0.512400506355204,
1.339453125)) ;
#78523 = CARTESIAN_POINT('Ctrl Pts',(-1.23704425180958,7.57471141691114E-17,
1.3890625)) ;
#78524 = CARTESIAN_POINT('Ctrl Pts',(-1.23704425180958,-0.512400506355204,
1.438671875)) ;
#78525 = CARTESIAN_POINT('Ctrl Pts',(-0.874722379082389,-0.874722379082389,
1.48828125)) ;
#78526 = CARTESIAN_POINT('Ctrl Pts',(-0.512400506355204,-1.23704425180958,
1.537890625)) ;
#78527 = CARTESIAN_POINT('Ctrl Pts',(-1.51494228338223E-16,-1.23704425180958,
1.5875)) ;
#78528 = CARTESIAN_POINT('Ctrl Pts',(0.512400506355204,-1.23704425180958,
1.637109375)) ;
#78529 = CARTESIAN_POINT('Ctrl Pts',(0.874722379082389,-0.87472237908239,
1.68671875)) ;
#78530 = CARTESIAN_POINT('Ctrl Pts',(1.23704425180957,-0.512400506355205,
1.736328125)) ;
#78531 = CARTESIAN_POINT('Ctrl Pts',(1.23704425180958,-2.27241342507334E-16,
1.7859375)) ;
#78532 = CARTESIAN_POINT('Ctrl Pts',(1.23704425180957,0.512400506355204,1.835546875)) ;
#78533 = CARTESIAN_POINT('Ctrl Pts',(0.87472237908239,0.874722379082389,1.88515625)) ;
#78534 = CARTESIAN_POINT('Ctrl Pts',(0.512400506355205,1.23704425180957,1.934765625)) ;
#78535 = CARTESIAN_POINT('Ctrl Pts',(0.,1.23704425180958,1.984375)) ;
#78536 = CARTESIAN_POINT('Ctrl Pts',(-0.512400506355204,1.23704425180958,
2.033984375)) ;
#78537 = CARTESIAN_POINT('Ctrl Pts',(-0.874722379082389,0.874722379082389,
2.08359375)) ;
#78538 = CARTESIAN_POINT('Ctrl Pts',(-1.23704425180958,0.512400506355204,
2.133203125)) ;
#78539 = CARTESIAN_POINT('Ctrl Pts',(-1.23704425180958,7.57471141691114E-17,
2.1828125)) ;
#78540 = CARTESIAN_POINT('Ctrl Pts',(-1.23704425180958,-0.512400506355204,
2.232421875)) ;
#78541 = CARTESIAN_POINT('Ctrl Pts',(-0.874722379082389,-0.874722379082389,
2.28203125)) ;
#78542 = CARTESIAN_POINT('Ctrl Pts',(-0.512400506355204,-1.23704425180958,
2.331640625)) ;
#78543 = CARTESIAN_POINT('Ctrl Pts',(-1.51494228338223E-16,-1.23704425180958,
2.38125)) ;
#78544 = CARTESIAN_POINT('Ctrl Pts',(0.512400506355204,-1.23704425180958,
2.430859375)) ;
#78545 = CARTESIAN_POINT('Ctrl Pts',(0.874722379082389,-0.87472237908239,
2.48046875)) ;
#78546 = CARTESIAN_POINT('Ctrl Pts',(1.23704425180957,-0.512400506355205,
2.530078125)) ;
#78547 = CARTESIAN_POINT('Ctrl Pts',(1.23704425180958,-2.27241342507334E-16,
2.5796875)) ;
#78548 = CARTESIAN_POINT('Ctrl Pts',(1.23704425180957,0.512400506355204,2.629296875)) ;
#78549 = CARTESIAN_POINT('Ctrl Pts',(0.87472237908239,0.874722379082389,2.67890625)) ;
#78550 = CARTESIAN_POINT('Ctrl Pts',(0.512400506355205,1.23704425180957,2.728515625)) ;
#78551 = CARTESIAN_POINT('Ctrl Pts',(0.,1.23704425180958,2.778125)) ;
#78552 = CARTESIAN_POINT('Ctrl Pts',(-0.512400506355204,1.23704425180958,
2.827734375)) ;
#78553 = CARTESIAN_POINT('Ctrl Pts',(-0.874722379082389,0.874722379082389,
2.87734375)) ;
#78554 = CARTESIAN_POINT('Ctrl Pts',(-1.23704425180958,0.512400506355204,
2.926953125)) ;
#78555 = CARTESIAN_POINT('Ctrl Pts',(-1.23704425180958,7.57471141691114E-17,
2.9765625)) ;
#78556 = CARTESIAN_POINT('Ctrl Pts',(-1.23704425180958,-0.512400506355204,
3.026171875)) ;
#78557 = CARTESIAN_POINT('Ctrl Pts',(-0.874722379082389,-0.874722379082389,
3.07578125)) ;
#78558 = CARTESIAN_POINT('Ctrl Pts',(-0.512400506355204,-1.23704425180958,
3.125390625)) ;
#78559 = CARTESIAN_POINT('Ctrl Pts',(-1.51494228338223E-16,-1.23704425180958,
3.175)) ;
#78560 = CARTESIAN_POINT('Ctrl Pts',(0.512400506355204,-1.23704425180958,
3.224609375)) ;
#78561 = CARTESIAN_POINT('Ctrl Pts',(0.874722379082389,-0.87472237908239,
3.27421875)) ;
#78562 = CARTESIAN_POINT('Ctrl Pts',(1.23704425180957,-0.512400506355205,
3.323828125)) ;
#78563 = CARTESIAN_POINT('Ctrl Pts',(1.23704425180958,-2.27241342507334E-16,
3.3734375)) ;
#78564 = CARTESIAN_POINT('Ctrl Pts',(1.23704425180957,0.512400506355204,3.423046875)) ;
#78565 = CARTESIAN_POINT('Ctrl Pts',(0.87472237908239,0.874722379082389,3.47265625)) ;
#78566 = CARTESIAN_POINT('Ctrl Pts',(0.512400506355205,1.23704425180957,3.522265625)) ;
#78567 = CARTESIAN_POINT('Ctrl Pts',(0.,1.23704425180958,3.571875)) ;
#78568 = CARTESIAN_POINT('Ctrl Pts',(-0.512400506355204,1.23704425180958,
3.621484375)) ;
#78569 = CARTESIAN_POINT('Ctrl Pts',(-0.874722379082389,0.874722379082389,
3.67109375)) ;
#78570 = CARTESIAN_POINT('Ctrl Pts',(-1.23704425180958,0.512400506355204,
3.720703125)) ;
#78571 = CARTESIAN_POINT('Ctrl Pts',(-1.23704425180958,7.57471141691114E-17,
3.7703125)) ;
#78572 = CARTESIAN_POINT('Ctrl Pts',(-1.23704425180958,-0.512400506355204,
3.819921875)) ;
#78573 = CARTESIAN_POINT('Ctrl Pts',(-0.874722379082389,-0.874722379082389,
3.86953125)) ;
#78574 = CARTESIAN_POINT('Ctrl Pts',(-0.512400506355204,-1.23704425180958,
3.919140625)) ;
#78575 = CARTESIAN_POINT('Ctrl Pts',(-1.51494228338223E-16,-1.23704425180958,
3.96875)) ;
#78576 = CARTESIAN_POINT('Ctrl Pts',(0.512400506355204,-1.23704425180958,
4.018359375)) ;
#78577 = CARTESIAN_POINT('Ctrl Pts',(0.874722379082389,-0.87472237908239,
4.06796875)) ;
#78578 = CARTESIAN_POINT('Ctrl Pts',(1.23704425180957,-0.512400506355205,
4.117578125)) ;
#78579 = CARTESIAN_POINT('Ctrl Pts',(1.23704425180958,-2.27241342507334E-16,
4.1671875)) ;
#78580 = CARTESIAN_POINT('Ctrl Pts',(1.23704425180957,0.512400506355204,4.216796875)) ;
#78581 = CARTESIAN_POINT('Ctrl Pts',(0.87472237908239,0.874722379082389,4.26640625)) ;
#78582 = CARTESIAN_POINT('Ctrl Pts',(0.512400506355205,1.23704425180957,4.316015625)) ;
#78583 = CARTESIAN_POINT('Ctrl Pts',(0.,1.23704425180958,4.365625)) ;
#78584 = CARTESIAN_POINT('Ctrl Pts',(-0.512400506355204,1.23704425180958,
4.415234375)) ;
#78585 = CARTESIAN_POINT('Ctrl Pts',(-0.874722379082389,0.874722379082389,
4.46484375)) ;
#78586 = CARTESIAN_POINT('Ctrl Pts',(-1.23704425180958,0.512400506355204,
4.514453125)) ;
#78587 = CARTESIAN_POINT('Ctrl Pts',(-1.23704425180958,7.57471141691114E-17,
4.5640625)) ;
#78588 = CARTESIAN_POINT('Ctrl Pts',(-1.23704425180958,-0.512400506355204,
4.613671875)) ;
#78589 = CARTESIAN_POINT('Ctrl Pts',(-0.874722379082389,-0.874722379082389,
4.66328125)) ;
#78590 = CARTESIAN_POINT('Ctrl Pts',(-0.512400506355204,-1.23704425180958,
4.712890625)) ;
#78591 = CARTESIAN_POINT('Ctrl Pts',(-1.51494228338223E-16,-1.23704425180958,
4.7625)) ;
#78592 = CARTESIAN_POINT('Ctrl Pts',(0.512400506355204,-1.23704425180958,
4.812109375)) ;
#78593 = CARTESIAN_POINT('Ctrl Pts',(0.874722379082389,-0.87472237908239,
4.86171875)) ;
#78594 = CARTESIAN_POINT('Ctrl Pts',(1.23704425180957,-0.512400506355205,
4.911328125)) ;
#78595 = CARTESIAN_POINT('Ctrl Pts',(1.23704425180958,-2.27241342507334E-16,
4.9609375)) ;
#78596 = CARTESIAN_POINT('Ctrl Pts',(1.23704425180957,0.512400506355204,5.010546875)) ;
#78597 = CARTESIAN_POINT('Ctrl Pts',(0.87472237908239,0.874722379082389,5.06015625)) ;
#78598 = CARTESIAN_POINT('Ctrl Pts',(0.512400506355205,1.23704425180957,5.109765625)) ;
#78599 = CARTESIAN_POINT('Ctrl Pts',(0.,1.23704425180958,5.159375)) ;
#78600 = CARTESIAN_POINT('Ctrl Pts',(-0.512400506355204,1.23704425180958,
5.208984375)) ;
#78601 = CARTESIAN_POINT('Ctrl Pts',(-0.874722379082389,0.874722379082389,
5.25859375)) ;
#78602 = CARTESIAN_POINT('Ctrl Pts',(-1.23704425180958,0.512400506355204,
5.308203125)) ;
#78603 = CARTESIAN_POINT('Ctrl Pts',(-1.23704425180958,7.57471141691114E-17,
5.3578125)) ;
#78604 = CARTESIAN_POINT('Ctrl Pts',(-1.23704425180958,-0.512400506355204,
5.407421875)) ;
#78605 = CARTESIAN_POINT('Ctrl Pts',(-0.874722379082389,-0.874722379082389,
5.45703125)) ;
#78606 = CARTESIAN_POINT('Ctrl Pts',(-0.512400506355204,-1.23704425180958,
5.506640625)) ;
#78607 = CARTESIAN_POINT('Ctrl Pts',(-1.51494228338223E-16,-1.23704425180958,
5.55625)) ;
#78608 = CARTESIAN_POINT('Ctrl Pts',(0.512400506355204,-1.23704425180958,
5.605859375)) ;
#78609 = CARTESIAN_POINT('Ctrl Pts',(0.874722379082389,-0.87472237908239,
5.65546875)) ;
#78610 = CARTESIAN_POINT('Ctrl Pts',(1.23704425180957,-0.512400506355205,
5.705078125)) ;
#78611 = CARTESIAN_POINT('Ctrl Pts',(1.23704425180958,-2.27241342507334E-16,
5.7546875)) ;
#78612 = CARTESIAN_POINT('Ctrl Pts',(1.23704425180957,0.512400506355204,5.804296875)) ;
#78613 = CARTESIAN_POINT('Ctrl Pts',(0.87472237908239,0.874722379082389,5.85390625)) ;
#78614 = CARTESIAN_POINT('Ctrl Pts',(0.512400506355205,1.23704425180957,5.903515625)) ;
#78615 = CARTESIAN_POINT('Ctrl Pts',(0.,1.23704425180958,5.953125)) ;
#78616 = CARTESIAN_POINT('Ctrl Pts',(-0.512400506355204,1.23704425180958,
6.002734375)) ;
#78617 = CARTESIAN_POINT('Ctrl Pts',(-0.874722379082389,0.874722379082389,
6.05234375)) ;
#78618 = CARTESIAN_POINT('Ctrl Pts',(-1.23704425180958,0.512400506355204,
6.101953125)) ;
#78619 = CARTESIAN_POINT('Ctrl Pts',(-1.23704425180958,7.57471141691114E-17,
6.1515625)) ;
#78620 = CARTESIAN_POINT('Ctrl Pts',(-1.23704425180958,-0.512400506355204,
6.201171875)) ;
#78621 = CARTESIAN_POINT('Ctrl Pts',(-0.874722379082389,-0.874722379082389,
6.25078125)) ;
#78622 = CARTESIAN_POINT('Ctrl Pts',(-0.512400506355204,-1.23704425180958,
6.300390625)) ;
#78623 = CARTESIAN_POINT('Ctrl Pts',(-1.51494228338223E-16,-1.23704425180958,
6.35)) ;
#78624 = CARTESIAN_POINT('Ctrl Pts',(0.512400506355204,-1.23704425180958,
6.399609375)) ;
#78625 = CARTESIAN_POINT('Ctrl Pts',(0.874722379082389,-0.87472237908239,
6.44921875)) ;
#78626 = CARTESIAN_POINT('Ctrl Pts',(1.23704425180957,-0.512400506355205,
6.498828125)) ;
#78627 = CARTESIAN_POINT('Ctrl Pts',(1.23704425180958,-2.27241342507334E-16,
6.5484375)) ;
#78628 = CARTESIAN_POINT('Ctrl Pts',(1.23704425180957,0.512400506355204,6.598046875)) ;
#78629 = CARTESIAN_POINT('Ctrl Pts',(0.87472237908239,0.874722379082389,6.64765625)) ;
#78630 = CARTESIAN_POINT('Ctrl Pts',(0.512400506355205,1.23704425180957,6.697265625)) ;
#78631 = CARTESIAN_POINT('Ctrl Pts',(0.,1.23704425180958,6.746875)) ;
#78632 = CARTESIAN_POINT('Ctrl Pts',(0.,1.75262906179543,-0.694548028835418)) ;
#78633 = CARTESIAN_POINT('Ctrl Pts',(-0.725962727204902,1.75262906179543,
-0.644938653835418)) ;
#78634 = CARTESIAN_POINT('Ctrl Pts',(-1.23929589450017,1.23929589450017,-0.595329278835418)) ;
#78635 = CARTESIAN_POINT('Ctrl Pts',(-1.75262906179543,0.725962727204902,
-0.545719903835418)) ;
#78636 = CARTESIAN_POINT('Ctrl Pts',(-1.75262906179543,1.0731757853102E-16,
-0.496110528835418)) ;
#78637 = CARTESIAN_POINT('Ctrl Pts',(-1.75262906179543,-0.725962727204902,
-0.446501153835418)) ;
#78638 = CARTESIAN_POINT('Ctrl Pts',(-1.23929589450017,-1.23929589450017,
-0.396891778835418)) ;
#78639 = CARTESIAN_POINT('Ctrl Pts',(-0.725962727204902,-1.75262906179543,
-0.347282403835418)) ;
#78640 = CARTESIAN_POINT('Ctrl Pts',(-2.14635157062041E-16,-1.75262906179543,
-0.297673028835418)) ;
#78641 = CARTESIAN_POINT('Ctrl Pts',(0.725962727204902,-1.75262906179543,
-0.248063653835418)) ;
#78642 = CARTESIAN_POINT('Ctrl Pts',(1.23929589450017,-1.23929589450017,-0.198454278835418)) ;
#78643 = CARTESIAN_POINT('Ctrl Pts',(1.75262906179543,-0.725962727204903,
-0.148844903835418)) ;
#78644 = CARTESIAN_POINT('Ctrl Pts',(1.75262906179543,-3.21952735593061E-16,
-0.0992355288354184)) ;
#78645 = CARTESIAN_POINT('Ctrl Pts',(1.75262906179543,0.725962727204903,-0.0496261538354183)) ;
#78646 = CARTESIAN_POINT('Ctrl Pts',(1.23929589450017,1.23929589450017,-1.67788354183017E-5)) ;
#78647 = CARTESIAN_POINT('Ctrl Pts',(0.725962727204903,1.75262906179543,0.0495925961645818)) ;
#78648 = CARTESIAN_POINT('Ctrl Pts',(0.,1.75262906179543,0.0992019711645818)) ;
#78649 = CARTESIAN_POINT('Ctrl Pts',(-0.725962727204902,1.75262906179543,
0.148811346164582)) ;
#78650 = CARTESIAN_POINT('Ctrl Pts',(-1.23929589450017,1.23929589450017,0.198420721164582)) ;
#78651 = CARTESIAN_POINT('Ctrl Pts',(-1.75262906179543,0.725962727204902,
0.248030096164582)) ;
#78652 = CARTESIAN_POINT('Ctrl Pts',(-1.75262906179543,1.0731757853102E-16,
0.297639471164582)) ;
#78653 = CARTESIAN_POINT('Ctrl Pts',(-1.75262906179543,-0.725962727204902,
0.347248846164582)) ;
#78654 = CARTESIAN_POINT('Ctrl Pts',(-1.23929589450017,-1.23929589450017,
0.396858221164582)) ;
#78655 = CARTESIAN_POINT('Ctrl Pts',(-0.725962727204902,-1.75262906179543,
0.446467596164582)) ;
#78656 = CARTESIAN_POINT('Ctrl Pts',(-2.14635157062041E-16,-1.75262906179543,
0.496076971164582)) ;
#78657 = CARTESIAN_POINT('Ctrl Pts',(0.725962727204902,-1.75262906179543,
0.545686346164582)) ;
#78658 = CARTESIAN_POINT('Ctrl Pts',(1.23929589450017,-1.23929589450017,0.595295721164582)) ;
#78659 = CARTESIAN_POINT('Ctrl Pts',(1.75262906179543,-0.725962727204903,
0.644905096164582)) ;
#78660 = CARTESIAN_POINT('Ctrl Pts',(1.75262906179543,-3.21952735593061E-16,
0.694514471164582)) ;
#78661 = CARTESIAN_POINT('Ctrl Pts',(1.75262906179543,0.725962727204903,0.744123846164582)) ;
#78662 = CARTESIAN_POINT('Ctrl Pts',(1.23929589450017,1.23929589450017,0.793733221164582)) ;
#78663 = CARTESIAN_POINT('Ctrl Pts',(0.725962727204903,1.75262906179543,0.843342596164582)) ;
#78664 = CARTESIAN_POINT('Ctrl Pts',(0.,1.75262906179543,0.892951971164582)) ;
#78665 = CARTESIAN_POINT('Ctrl Pts',(-0.725962727204902,1.75262906179543,
0.942561346164582)) ;
#78666 = CARTESIAN_POINT('Ctrl Pts',(-1.23929589450017,1.23929589450017,0.992170721164582)) ;
#78667 = CARTESIAN_POINT('Ctrl Pts',(-1.75262906179543,0.725962727204902,
1.04178009616459)) ;
#78668 = CARTESIAN_POINT('Ctrl Pts',(-1.75262906179543,1.0731757853102E-16,
1.09138947116459)) ;
#78669 = CARTESIAN_POINT('Ctrl Pts',(-1.75262906179543,-0.725962727204902,
1.14099884616459)) ;
#78670 = CARTESIAN_POINT('Ctrl Pts',(-1.23929589450017,-1.23929589450017,
1.19060822116459)) ;
#78671 = CARTESIAN_POINT('Ctrl Pts',(-0.725962727204902,-1.75262906179543,
1.24021759616459)) ;
#78672 = CARTESIAN_POINT('Ctrl Pts',(-2.14635157062041E-16,-1.75262906179543,
1.28982697116459)) ;
#78673 = CARTESIAN_POINT('Ctrl Pts',(0.725962727204902,-1.75262906179543,
1.33943634616459)) ;
#78674 = CARTESIAN_POINT('Ctrl Pts',(1.23929589450017,-1.23929589450017,1.38904572116459)) ;
#78675 = CARTESIAN_POINT('Ctrl Pts',(1.75262906179543,-0.725962727204903,
1.43865509616459)) ;
#78676 = CARTESIAN_POINT('Ctrl Pts',(1.75262906179543,-3.21952735593061E-16,
1.48826447116459)) ;
#78677 = CARTESIAN_POINT('Ctrl Pts',(1.75262906179543,0.725962727204903,1.53787384616459)) ;
#78678 = CARTESIAN_POINT('Ctrl Pts',(1.23929589450017,1.23929589450017,1.58748322116459)) ;
#78679 = CARTESIAN_POINT('Ctrl Pts',(0.725962727204903,1.75262906179543,1.63709259616459)) ;
#78680 = CARTESIAN_POINT('Ctrl Pts',(0.,1.75262906179543,1.68670197116459)) ;
#78681 = CARTESIAN_POINT('Ctrl Pts',(-0.725962727204902,1.75262906179543,
1.73631134616459)) ;
#78682 = CARTESIAN_POINT('Ctrl Pts',(-1.23929589450017,1.23929589450017,1.78592072116459)) ;
#78683 = CARTESIAN_POINT('Ctrl Pts',(-1.75262906179543,0.725962727204902,
1.83553009616459)) ;
#78684 = CARTESIAN_POINT('Ctrl Pts',(-1.75262906179543,1.0731757853102E-16,
1.88513947116459)) ;
#78685 = CARTESIAN_POINT('Ctrl Pts',(-1.75262906179543,-0.725962727204902,
1.93474884616459)) ;
#78686 = CARTESIAN_POINT('Ctrl Pts',(-1.23929589450017,-1.23929589450017,
1.98435822116459)) ;
#78687 = CARTESIAN_POINT('Ctrl Pts',(-0.725962727204902,-1.75262906179543,
2.03396759616459)) ;
#78688 = CARTESIAN_POINT('Ctrl Pts',(-2.14635157062041E-16,-1.75262906179543,
2.08357697116459)) ;
#78689 = CARTESIAN_POINT('Ctrl Pts',(0.725962727204902,-1.75262906179543,
2.13318634616459)) ;
#78690 = CARTESIAN_POINT('Ctrl Pts',(1.23929589450017,-1.23929589450017,2.18279572116459)) ;
#78691 = CARTESIAN_POINT('Ctrl Pts',(1.75262906179543,-0.725962727204903,
2.23240509616459)) ;
#78692 = CARTESIAN_POINT('Ctrl Pts',(1.75262906179543,-3.21952735593061E-16,
2.28201447116459)) ;
#78693 = CARTESIAN_POINT('Ctrl Pts',(1.75262906179543,0.725962727204903,2.33162384616459)) ;
#78694 = CARTESIAN_POINT('Ctrl Pts',(1.23929589450017,1.23929589450017,2.38123322116459)) ;
#78695 = CARTESIAN_POINT('Ctrl Pts',(0.725962727204903,1.75262906179543,2.43084259616459)) ;
#78696 = CARTESIAN_POINT('Ctrl Pts',(0.,1.75262906179543,2.48045197116459)) ;
#78697 = CARTESIAN_POINT('Ctrl Pts',(-0.725962727204902,1.75262906179543,
2.53006134616459)) ;
#78698 = CARTESIAN_POINT('Ctrl Pts',(-1.23929589450017,1.23929589450017,2.57967072116459)) ;
#78699 = CARTESIAN_POINT('Ctrl Pts',(-1.75262906179543,0.725962727204902,
2.62928009616459)) ;
#78700 = CARTESIAN_POINT('Ctrl Pts',(-1.75262906179543,1.0731757853102E-16,
2.67888947116459)) ;
#78701 = CARTESIAN_POINT('Ctrl Pts',(-1.75262906179543,-0.725962727204902,
2.72849884616459)) ;
#78702 = CARTESIAN_POINT('Ctrl Pts',(-1.23929589450017,-1.23929589450017,
2.77810822116459)) ;
#78703 = CARTESIAN_POINT('Ctrl Pts',(-0.725962727204902,-1.75262906179543,
2.82771759616459)) ;
#78704 = CARTESIAN_POINT('Ctrl Pts',(-2.14635157062041E-16,-1.75262906179543,
2.87732697116459)) ;
#78705 = CARTESIAN_POINT('Ctrl Pts',(0.725962727204902,-1.75262906179543,
2.92693634616458)) ;
#78706 = CARTESIAN_POINT('Ctrl Pts',(1.23929589450017,-1.23929589450017,2.97654572116459)) ;
#78707 = CARTESIAN_POINT('Ctrl Pts',(1.75262906179543,-0.725962727204903,
3.02615509616459)) ;
#78708 = CARTESIAN_POINT('Ctrl Pts',(1.75262906179543,-3.21952735593061E-16,
3.07576447116459)) ;
#78709 = CARTESIAN_POINT('Ctrl Pts',(1.75262906179543,0.725962727204903,3.12537384616459)) ;
#78710 = CARTESIAN_POINT('Ctrl Pts',(1.23929589450017,1.23929589450017,3.17498322116459)) ;
#78711 = CARTESIAN_POINT('Ctrl Pts',(0.725962727204903,1.75262906179543,3.22459259616459)) ;
#78712 = CARTESIAN_POINT('Ctrl Pts',(0.,1.75262906179543,3.27420197116459)) ;
#78713 = CARTESIAN_POINT('Ctrl Pts',(-0.725962727204902,1.75262906179543,
3.32381134616459)) ;
#78714 = CARTESIAN_POINT('Ctrl Pts',(-1.23929589450017,1.23929589450017,3.37342072116459)) ;
#78715 = CARTESIAN_POINT('Ctrl Pts',(-1.75262906179543,0.725962727204902,
3.42303009616459)) ;
#78716 = CARTESIAN_POINT('Ctrl Pts',(-1.75262906179543,1.0731757853102E-16,
3.47263947116459)) ;
#78717 = CARTESIAN_POINT('Ctrl Pts',(-1.75262906179543,-0.725962727204902,
3.52224884616459)) ;
#78718 = CARTESIAN_POINT('Ctrl Pts',(-1.23929589450017,-1.23929589450017,
3.57185822116459)) ;
#78719 = CARTESIAN_POINT('Ctrl Pts',(-0.725962727204902,-1.75262906179543,
3.62146759616459)) ;
#78720 = CARTESIAN_POINT('Ctrl Pts',(-2.14635157062041E-16,-1.75262906179543,
3.67107697116459)) ;
#78721 = CARTESIAN_POINT('Ctrl Pts',(0.725962727204902,-1.75262906179543,
3.72068634616459)) ;
#78722 = CARTESIAN_POINT('Ctrl Pts',(1.23929589450017,-1.23929589450017,3.77029572116459)) ;
#78723 = CARTESIAN_POINT('Ctrl Pts',(1.75262906179543,-0.725962727204903,
3.81990509616459)) ;
#78724 = CARTESIAN_POINT('Ctrl Pts',(1.75262906179543,-3.21952735593061E-16,
3.86951447116459)) ;
#78725 = CARTESIAN_POINT('Ctrl Pts',(1.75262906179543,0.725962727204903,3.91912384616459)) ;
#78726 = CARTESIAN_POINT('Ctrl Pts',(1.23929589450017,1.23929589450017,3.96873322116459)) ;
#78727 = CARTESIAN_POINT('Ctrl Pts',(0.725962727204903,1.75262906179543,4.01834259616459)) ;
#78728 = CARTESIAN_POINT('Ctrl Pts',(0.,1.75262906179543,4.06795197116459)) ;
#78729 = CARTESIAN_POINT('Ctrl Pts',(-0.725962727204902,1.75262906179543,
4.11756134616459)) ;
#78730 = CARTESIAN_POINT('Ctrl Pts',(-1.23929589450017,1.23929589450017,4.16717072116459)) ;
#78731 = CARTESIAN_POINT('Ctrl Pts',(-1.75262906179543,0.725962727204902,
4.21678009616459)) ;
#78732 = CARTESIAN_POINT('Ctrl Pts',(-1.75262906179543,1.0731757853102E-16,
4.26638947116459)) ;
#78733 = CARTESIAN_POINT('Ctrl Pts',(-1.75262906179543,-0.725962727204902,
4.31599884616459)) ;
#78734 = CARTESIAN_POINT('Ctrl Pts',(-1.23929589450017,-1.23929589450017,
4.36560822116459)) ;
#78735 = CARTESIAN_POINT('Ctrl Pts',(-0.725962727204902,-1.75262906179543,
4.41521759616459)) ;
#78736 = CARTESIAN_POINT('Ctrl Pts',(-2.14635157062041E-16,-1.75262906179543,
4.46482697116459)) ;
#78737 = CARTESIAN_POINT('Ctrl Pts',(0.725962727204902,-1.75262906179543,
4.51443634616459)) ;
#78738 = CARTESIAN_POINT('Ctrl Pts',(1.23929589450017,-1.23929589450017,4.56404572116459)) ;
#78739 = CARTESIAN_POINT('Ctrl Pts',(1.75262906179543,-0.725962727204903,
4.61365509616459)) ;
#78740 = CARTESIAN_POINT('Ctrl Pts',(1.75262906179543,-3.21952735593061E-16,
4.66326447116459)) ;
#78741 = CARTESIAN_POINT('Ctrl Pts',(1.75262906179543,0.725962727204903,4.71287384616459)) ;
#78742 = CARTESIAN_POINT('Ctrl Pts',(1.23929589450017,1.23929589450017,4.76248322116459)) ;
#78743 = CARTESIAN_POINT('Ctrl Pts',(0.725962727204903,1.75262906179543,4.81209259616459)) ;
#78744 = CARTESIAN_POINT('Ctrl Pts',(0.,1.75262906179543,4.86170197116459)) ;
#78745 = CARTESIAN_POINT('Ctrl Pts',(-0.725962727204902,1.75262906179543,
4.91131134616459)) ;
#78746 = CARTESIAN_POINT('Ctrl Pts',(-1.23929589450017,1.23929589450017,4.96092072116459)) ;
#78747 = CARTESIAN_POINT('Ctrl Pts',(-1.75262906179543,0.725962727204902,
5.01053009616459)) ;
#78748 = CARTESIAN_POINT('Ctrl Pts',(-1.75262906179543,1.0731757853102E-16,
5.06013947116459)) ;
#78749 = CARTESIAN_POINT('Ctrl Pts',(-1.75262906179543,-0.725962727204902,
5.10974884616459)) ;
#78750 = CARTESIAN_POINT('Ctrl Pts',(-1.23929589450017,-1.23929589450017,
5.15935822116457)) ;
#78751 = CARTESIAN_POINT('Ctrl Pts',(-0.725962727204902,-1.75262906179543,
5.20896759616459)) ;
#78752 = CARTESIAN_POINT('Ctrl Pts',(-2.14635157062041E-16,-1.75262906179543,
5.25857697116458)) ;
#78753 = CARTESIAN_POINT('Ctrl Pts',(0.725962727204902,-1.75262906179543,
5.30818634616459)) ;
#78754 = CARTESIAN_POINT('Ctrl Pts',(1.23929589450017,-1.23929589450017,5.35779572116459)) ;
#78755 = CARTESIAN_POINT('Ctrl Pts',(1.75262906179543,-0.725962727204903,
5.40740509616459)) ;
#78756 = CARTESIAN_POINT('Ctrl Pts',(1.75262906179543,-3.21952735593061E-16,
5.45701447116459)) ;
#78757 = CARTESIAN_POINT('Ctrl Pts',(1.75262906179543,0.725962727204903,5.50662384616459)) ;
#78758 = CARTESIAN_POINT('Ctrl Pts',(1.23929589450017,1.23929589450017,5.55623322116459)) ;
#78759 = CARTESIAN_POINT('Ctrl Pts',(0.725962727204903,1.75262906179543,5.60584259616459)) ;
#78760 = CARTESIAN_POINT('Ctrl Pts',(0.,1.75262906179543,5.65545197116459)) ;
#78761 = CARTESIAN_POINT('Ctrl Pts',(-0.725962727204902,1.75262906179543,
5.70506134616459)) ;
#78762 = CARTESIAN_POINT('Ctrl Pts',(-1.23929589450017,1.23929589450017,5.75467072116458)) ;
#78763 = CARTESIAN_POINT('Ctrl Pts',(-1.75262906179543,0.725962727204902,
5.80428009616459)) ;
#78764 = CARTESIAN_POINT('Ctrl Pts',(-1.75262906179543,1.0731757853102E-16,
5.85388947116459)) ;
#78765 = CARTESIAN_POINT('Ctrl Pts',(-1.75262906179543,-0.725962727204902,
5.90349884616459)) ;
#78766 = CARTESIAN_POINT('Ctrl Pts',(-1.23929589450017,-1.23929589450017,
5.95310822116459)) ;
#78767 = CARTESIAN_POINT('Ctrl Pts',(-0.725962727204902,-1.75262906179543,
6.00271759616459)) ;
#78768 = CARTESIAN_POINT('Ctrl Pts',(-2.14635157062041E-16,-1.75262906179543,
6.05232697116459)) ;
#78769 = CARTESIAN_POINT('Ctrl Pts',(0.725962727204902,-1.75262906179543,
6.10193634616459)) ;
#78770 = CARTESIAN_POINT('Ctrl Pts',(1.23929589450017,-1.23929589450017,6.15154572116459)) ;
#78771 = CARTESIAN_POINT('Ctrl Pts',(1.75262906179543,-0.725962727204903,
6.20115509616459)) ;
#78772 = CARTESIAN_POINT('Ctrl Pts',(1.75262906179543,-3.21952735593061E-16,
6.25076447116458)) ;
#78773 = CARTESIAN_POINT('Ctrl Pts',(1.75262906179543,0.725962727204903,6.30037384616459)) ;
#78774 = CARTESIAN_POINT('Ctrl Pts',(1.23929589450017,1.23929589450017,6.34998322116458)) ;
#78775 = CARTESIAN_POINT('Ctrl Pts',(0.725962727204903,1.75262906179543,6.39959259616457)) ;
#78776 = CARTESIAN_POINT('Ctrl Pts',(0.,1.75262906179543,6.44920197116459)) ;
#78777 = CARTESIAN_POINT('',(205.838527625407,531.472556589211,-39.3721601717608)) ;
#78778 = CARTESIAN_POINT('',(205.838527625415,578.972556589211,-39.3721601717608)) ;
#78779 = CARTESIAN_POINT('',(205.838527625412,559.972556589211,-39.3721601717608)) ;
#78780 = CARTESIAN_POINT('',(205.838527625414,569.472556589211,-39.3721601717608)) ;
#78781 = CARTESIAN_POINT('',(205.838527625409,540.972556589211,-39.3721601717608)) ;
#78782 = CARTESIAN_POINT('',(205.838527625411,550.472556589211,-39.3721601717608)) ;
#78783 = CARTESIAN_POINT('',(205.83852762542,607.472556589211,-39.3721601717608)) ;
#78784 = CARTESIAN_POINT('',(205.838527625417,588.472556589211,-39.3721601717608)) ;
#78785 = CARTESIAN_POINT('',(205.838527625419,597.972556589211,-39.3721601717608)) ;
#78786 = CARTESIAN_POINT('',(0.,0.,0.)) ;
#78787 = CARTESIAN_POINT('',(0.,0.,0.)) ;
#78788 = CARTESIAN_POINT('Origin',(130.842036869422,-80.5295274127545,-200.900005310181)) ;
#78789 = CARTESIAN_POINT('',(130.842036869422,-75.5685899127545,-202.652605310181)) ;
#78790 = CARTESIAN_POINT('',(130.842036869422,-75.4693711627547,-202.652605310181)) ;
#78791 = CARTESIAN_POINT('',(130.842036869422,-80.5295274127545,-202.652605310181)) ;
#78792 = CARTESIAN_POINT('',(129.538783258268,-75.178136333852,-199.72819611709)) ;
#78793 = CARTESIAN_POINT('Ctrl Pts',(130.842036869422,-75.4693711627547,-202.652605310181)) ;
#78794 = CARTESIAN_POINT('Ctrl Pts',(130.711623674148,-75.4604591013659,-202.652605310181)) ;
#78795 = CARTESIAN_POINT('Ctrl Pts',(130.581350458606,-75.45114469441,-202.638053305016)) ;
#78796 = CARTESIAN_POINT('Ctrl Pts',(130.229646191826,-75.424847544527,-202.558116804753)) ;
#78797 = CARTESIAN_POINT('Ctrl Pts',(130.017854402449,-75.4077012196374,-202.463682049367)) ;
#78798 = CARTESIAN_POINT('Ctrl Pts',(129.645404195784,-75.3747957460244,-202.200371817811)) ;
#78799 = CARTESIAN_POINT('Ctrl Pts',(129.487601874771,-75.3597717165059,-202.035077120023)) ;
#78800 = CARTESIAN_POINT('Ctrl Pts',(129.241759961654,-75.3265456678467,-201.650700216346)) ;
#78801 = CARTESIAN_POINT('Ctrl Pts',(129.157209481383,-75.309384599292,-201.434598477145)) ;
#78802 = CARTESIAN_POINT('Ctrl Pts',(129.076967738613,-75.2764311561231,-200.985616864913)) ;
#78803 = CARTESIAN_POINT('Ctrl Pts',(129.080663347727,-75.261430802899,-200.757312650326)) ;
#78804 = CARTESIAN_POINT('Ctrl Pts',(129.159604564136,-75.2337894460306,-200.385525890022)) ;
#78805 = CARTESIAN_POINT('Ctrl Pts',(129.2112220981,-75.222378340329,-200.239924020435)) ;
#78806 = CARTESIAN_POINT('Ctrl Pts',(129.350395585309,-75.1998143561719,-199.967385188184)) ;
#78807 = CARTESIAN_POINT('Ctrl Pts',(129.436986777276,-75.1887546024267,-199.841411333558)) ;
#78808 = CARTESIAN_POINT('Ctrl Pts',(129.538783258269,-75.1781363338561,-199.728196117089)) ;
#78809 = CARTESIAN_POINT('',(130.749091630179,-75.1781363338479,-199.14987161743)) ;
#78810 = CARTESIAN_POINT('Origin',(130.842036869422,-75.1781363338479,-200.900005310181)) ;
#78811 = CARTESIAN_POINT('Ctrl Pts',(130.749091630179,-75.1781363338479,-199.14987161743)) ;
#78812 = CARTESIAN_POINT('Ctrl Pts',(130.583254486741,-75.1897184635544,-199.158678814867)) ;
#78813 = CARTESIAN_POINT('Ctrl Pts',(130.419542420933,-75.2018212127873,-199.191008850173)) ;
#78814 = CARTESIAN_POINT('Ctrl Pts',(130.104891265179,-75.2264421770496,-199.301183187997)) ;
#78815 = CARTESIAN_POINT('Ctrl Pts',(129.955658398848,-75.238838371062,-199.378835920221)) ;
#78816 = CARTESIAN_POINT('Ctrl Pts',(129.636699798695,-75.2671190344011,-199.607901016349)) ;
#78817 = CARTESIAN_POINT('Ctrl Pts',(129.480768268154,-75.2820839842016,-199.77336511249)) ;
#78818 = CARTESIAN_POINT('Ctrl Pts',(129.237096602546,-75.3153352420707,-200.15900985697)) ;
#78819 = CARTESIAN_POINT('Ctrl Pts',(129.153543957048,-75.3325729348049,-200.376646180286)) ;
#78820 = CARTESIAN_POINT('Ctrl Pts',(129.076532892538,-75.3654879406052,-200.826403516307)) ;
#78821 = CARTESIAN_POINT('Ctrl Pts',(129.081706866303,-75.3804449144316,-201.053820825158)) ;
#78822 = CARTESIAN_POINT('Ctrl Pts',(129.179055347663,-75.4136531396854,-201.499444906297)) ;
#78823 = CARTESIAN_POINT('Ctrl Pts',(129.272321466205,-75.4308815313005,-201.712921670936)) ;
#78824 = CARTESIAN_POINT('Ctrl Pts',(129.533230085197,-75.4638459969484,-202.08722990841)) ;
#78825 = CARTESIAN_POINT('Ctrl Pts',(129.696689211027,-75.4787997245241,-202.245611390901)) ;
#78826 = CARTESIAN_POINT('Ctrl Pts',(130.078901162208,-75.5119638302814,-202.494491642853)) ;
#78827 = CARTESIAN_POINT('Ctrl Pts',(130.295049123513,-75.5291820177327,-202.580948429471)) ;
#78828 = CARTESIAN_POINT('Ctrl Pts',(130.627614758952,-75.553658530876,-202.64277021834)) ;
#78829 = CARTESIAN_POINT('Ctrl Pts',(130.73482723915,-75.5612635160318,-202.652605310181)) ;
#78830 = CARTESIAN_POINT('Ctrl Pts',(130.842036869422,-75.5685899127545,-202.652605310181)) ;
#78831 = CARTESIAN_POINT('Origin',(130.842036869422,-80.5295274127545,-200.900005310181)) ;
#78832 = CARTESIAN_POINT('',(130.842036869422,-76.3623399127545,-202.652605310181)) ;
#78833 = CARTESIAN_POINT('',(130.842036869422,-76.2631211627547,-202.652605310181)) ;
#78834 = CARTESIAN_POINT('',(130.842036869422,-80.5295274127545,-202.652605310181)) ;
#78835 = CARTESIAN_POINT('Ctrl Pts',(130.842036869423,-76.2631211627547,-202.652605310181)) ;
#78836 = CARTESIAN_POINT('Ctrl Pts',(130.680530862958,-76.2520843083839,-202.652605310181)) ;
#78837 = CARTESIAN_POINT('Ctrl Pts',(130.519524607284,-76.240449888059,-202.630287995016)) ;
#78838 = CARTESIAN_POINT('Ctrl Pts',(130.143742521215,-76.2117513287222,-202.523643499451)) ;
#78839 = CARTESIAN_POINT('Ctrl Pts',(129.938218404822,-76.1947406166118,-202.418868171205)) ;
#78840 = CARTESIAN_POINT('Ctrl Pts',(129.579230443517,-76.1622165224726,-202.136530578372)) ;
#78841 = CARTESIAN_POINT('Ctrl Pts',(129.429150307446,-76.1468603032157,-201.961809848165)) ;
#78842 = CARTESIAN_POINT('Ctrl Pts',(129.204152299825,-76.1133229218017,-201.564243279102)) ;
#78843 = CARTESIAN_POINT('Ctrl Pts',(129.131552208418,-76.09629426262,-201.345129117699)) ;
#78844 = CARTESIAN_POINT('Ctrl Pts',(129.074692618702,-76.063724019615,-200.89206979759)) ;
#78845 = CARTESIAN_POINT('Ctrl Pts',(129.090700039042,-76.0484202449793,-200.662540463456)) ;
#78846 = CARTESIAN_POINT('Ctrl Pts',(129.209927517257,-76.0149164496177,-200.22165378263)) ;
#78847 = CARTESIAN_POINT('Ctrl Pts',(129.312316492737,-75.997869967443,-200.01461777116)) ;
#78848 = CARTESIAN_POINT('Ctrl Pts',(129.590225701037,-75.9652528792995,-199.652434700344)) ;
#78849 = CARTESIAN_POINT('Ctrl Pts',(129.762719252203,-75.9499991490224,-199.500527579452)) ;
#78850 = CARTESIAN_POINT('Ctrl Pts',(130.157227417958,-75.9165305241439,-199.270574963972)) ;
#78851 = CARTESIAN_POINT('Ctrl Pts',(130.375689145037,-75.8994664234005,-199.195147677286)) ;
#78852 = CARTESIAN_POINT('Ctrl Pts',(130.827837753823,-75.8668019164062,-199.132759277728)) ;
#78853 = CARTESIAN_POINT('Ctrl Pts',(131.057076696894,-75.8515954494147,-199.145833643124)) ;
#78854 = CARTESIAN_POINT('Ctrl Pts',(131.499315712216,-75.8181635650319,-199.259255825996)) ;
#78855 = CARTESIAN_POINT('Ctrl Pts',(131.707911547695,-75.8010821313174,-199.359113821189)) ;
#78856 = CARTESIAN_POINT('Ctrl Pts',(132.073423739357,-75.7683697617454,-199.632351923101)) ;
#78857 = CARTESIAN_POINT('Ctrl Pts',(132.227237627881,-75.7532074074886,-199.80251847069)) ;
#78858 = CARTESIAN_POINT('Ctrl Pts',(132.462347492692,-75.7198138065936,-200.193792582609)) ;
#78859 = CARTESIAN_POINT('Ctrl Pts',(132.540726942963,-75.7027154063227,-200.41153340003)) ;
#78860 = CARTESIAN_POINT('Ctrl Pts',(132.60888938881,-75.6699548665787,-200.862695600096)) ;
#78861 = CARTESIAN_POINT('Ctrl Pts',(132.598863206262,-75.6548331230282,-201.091631358305)) ;
#78862 = CARTESIAN_POINT('Ctrl Pts',(132.491490612412,-75.6214793083452,-201.535233775242)) ;
#78863 = CARTESIAN_POINT('Ctrl Pts',(132.394291290212,-75.6043643871491,-201.74542090273)) ;
#78864 = CARTESIAN_POINT('Ctrl Pts',(132.125933368952,-75.5715555104706,-202.114366752397)) ;
#78865 = CARTESIAN_POINT('Ctrl Pts',(131.958174035764,-75.556470548808,-202.270151684134)) ;
#78866 = CARTESIAN_POINT('Ctrl Pts',(131.570286632123,-75.5231579691041,-202.51057546937)) ;
#78867 = CARTESIAN_POINT('Ctrl Pts',(131.353333758772,-75.5060270489619,-202.592006046919)) ;
#78868 = CARTESIAN_POINT('Ctrl Pts',(131.032490736109,-75.4826057764187,-202.644849186622)) ;
#78869 = CARTESIAN_POINT('Ctrl Pts',(130.937241579496,-75.4758771778776,-202.652605310181)) ;
#78870 = CARTESIAN_POINT('Ctrl Pts',(130.842036869422,-75.4693711627547,-202.652605310181)) ;
#78871 = CARTESIAN_POINT('Ctrl Pts',(130.842036869422,-75.5685899127545,-202.652605310181)) ;
#78872 = CARTESIAN_POINT('Ctrl Pts',(130.959477744642,-75.5766154832293,-202.652605310181)) ;
#78873 = CARTESIAN_POINT('Ctrl Pts',(131.076869305746,-75.5849717373026,-202.640803865211)) ;
#78874 = CARTESIAN_POINT('Ctrl Pts',(131.41821150113,-75.6102698116508,-202.571146452148)) ;
#78875 = CARTESIAN_POINT('Ctrl Pts',(131.632673993324,-75.6274769034568,-202.481012570103)) ;
#78876 = CARTESIAN_POINT('Ctrl Pts',(132.010645484719,-75.6605387180287,-202.225508685628)) ;
#78877 = CARTESIAN_POINT('Ctrl Pts',(132.171518155561,-75.6755006059372,-202.064086384525)) ;
#78878 = CARTESIAN_POINT('Ctrl Pts',(132.425641905301,-75.7085736307167,-201.685379179858)) ;
#78879 = CARTESIAN_POINT('Ctrl Pts',(132.515009981141,-75.725768754759,-201.470774608662)) ;
#78880 = CARTESIAN_POINT('Ctrl Pts',(132.604827890813,-75.7588782129851,-201.023476553771)) ;
#78881 = CARTESIAN_POINT('Ctrl Pts',(132.606049116628,-75.7738515041829,-200.795418974851)) ;
#78882 = CARTESIAN_POINT('Ctrl Pts',(132.521055612484,-75.8068778545833,-200.347338730559)) ;
#78883 = CARTESIAN_POINT('Ctrl Pts',(132.43408062645,-75.8240601663205,-200.131930395886)) ;
#78884 = CARTESIAN_POINT('Ctrl Pts',(132.184038144773,-75.8572163801247,-199.750315341626)) ;
#78885 = CARTESIAN_POINT('Ctrl Pts',(132.024665724764,-75.8722059667016,-199.586938734511)) ;
#78886 = CARTESIAN_POINT('Ctrl Pts',(131.649496464221,-75.9051850367174,-199.32759286598)) ;
#78887 = CARTESIAN_POINT('Ctrl Pts',(131.436473815438,-75.9223537365705,-199.235339205358)) ;
#78888 = CARTESIAN_POINT('Ctrl Pts',(130.990483732311,-75.9555556730147,-199.139096502026)) ;
#78889 = CARTESIAN_POINT('Ctrl Pts',(130.762105493726,-75.9705663911608,-199.134658928056)) ;
#78890 = CARTESIAN_POINT('Ctrl Pts',(130.312859003515,-76.0034976947888,-199.213479053113)) ;
#78891 = CARTESIAN_POINT('Ctrl Pts',(130.0965551513,-76.0206520317887,-199.297303777041)) ;
#78892 = CARTESIAN_POINT('Ctrl Pts',(129.711357293294,-76.0538985433324,-199.541886643868)) ;
#78893 = CARTESIAN_POINT('Ctrl Pts',(129.545488935552,-76.0689350880305,-199.699219419944)) ;
#78894 = CARTESIAN_POINT('Ctrl Pts',(129.280999183371,-76.1018182804073,-200.070855004335)) ;
#78895 = CARTESIAN_POINT('Ctrl Pts',(129.185917130932,-76.1189575601195,-200.28227558004)) ;
#78896 = CARTESIAN_POINT('Ctrl Pts',(129.083328343325,-76.1522473970365,-200.726923306207)) ;
#78897 = CARTESIAN_POINT('Ctrl Pts',(129.075707100053,-76.1673142726,-200.955619260857)) ;
#78898 = CARTESIAN_POINT('Ctrl Pts',(129.148444787698,-76.2001491530251,-201.405974185939)) ;
#78899 = CARTESIAN_POINT('Ctrl Pts',(129.22916264484,-76.2172727445578,-201.623115035738)) ;
#78900 = CARTESIAN_POINT('Ctrl Pts',(129.468346539637,-76.2506045681308,-202.01179762083)) ;
#78901 = CARTESIAN_POINT('Ctrl Pts',(129.623670940997,-76.2657060428676,-202.180119503146)) ;
#78902 = CARTESIAN_POINT('Ctrl Pts',(129.991815319861,-76.2984925560701,-202.449622289195)) ;
#78903 = CARTESIAN_POINT('Ctrl Pts',(130.201632658185,-76.3155998980288,-202.547446602108)) ;
#78904 = CARTESIAN_POINT('Ctrl Pts',(130.561330991605,-76.3426794053451,-202.635722841674)) ;
#78905 = CARTESIAN_POINT('Ctrl Pts',(130.701567106792,-76.3527406145762,-202.652605310181)) ;
#78906 = CARTESIAN_POINT('Ctrl Pts',(130.842036869422,-76.3623399127545,-202.652605310181)) ;
#78907 = CARTESIAN_POINT('Origin',(130.842036869422,-80.5295274127545,-200.900005310181)) ;
#78908 = CARTESIAN_POINT('',(130.842036869422,-77.1560899127545,-202.652605310181)) ;
#78909 = CARTESIAN_POINT('',(130.842036869422,-77.0568711627547,-202.652605310181)) ;
#78910 = CARTESIAN_POINT('',(130.842036869422,-80.5295274127545,-202.652605310181)) ;
#78911 = CARTESIAN_POINT('Ctrl Pts',(130.842036869423,-77.0568711627547,-202.652605310181)) ;
#78912 = CARTESIAN_POINT('Ctrl Pts',(130.660862359968,-77.0444902196534,-202.652605310181)) ;
#78913 = CARTESIAN_POINT('Ctrl Pts',(130.480554613838,-77.0313735225802,-202.62452004209)) ;
#78914 = CARTESIAN_POINT('Ctrl Pts',(130.085697399116,-77.000810765977,-202.498068619796)) ;
#78915 = CARTESIAN_POINT('Ctrl Pts',(129.880224218456,-76.983526713373,-202.383513748854)) ;
#78916 = CARTESIAN_POINT('Ctrl Pts',(129.532288465508,-76.9513296806648,-202.086048190946)) ;
#78917 = CARTESIAN_POINT('Ctrl Pts',(129.391113123426,-76.9358875977997,-201.908456427025)) ;
#78918 = CARTESIAN_POINT('Ctrl Pts',(129.179864391872,-76.9021655650029,-201.502492655479)) ;
#78919 = CARTESIAN_POINT('Ctrl Pts',(129.114605521132,-76.8848805664655,-201.276586560807)) ;
#78920 = CARTESIAN_POINT('Ctrl Pts',(129.07687057682,-76.8526447943419,-200.82049997823)) ;
#78921 = CARTESIAN_POINT('Ctrl Pts',(129.101600837785,-76.8372461483228,-200.594999757667)) ;
#78922 = CARTESIAN_POINT('Ctrl Pts',(129.237269162886,-76.8035468524068,-200.158062273154)) ;
#78923 = CARTESIAN_POINT('Ctrl Pts',(129.349858198285,-76.786261223496,-199.951751750124)) ;
#78924 = CARTESIAN_POINT('Ctrl Pts',(129.643953164324,-76.7539853070896,-199.601265520593)) ;
#78925 = CARTESIAN_POINT('Ctrl Pts',(129.820211604413,-76.7386299006385,-199.458473588984)) ;
#78926 = CARTESIAN_POINT('Ctrl Pts',(130.223983964321,-76.7049546806224,-199.243588123652)) ;
#78927 = CARTESIAN_POINT('Ctrl Pts',(130.449047202455,-76.6876687850883,-199.176262728122)) ;
#78928 = CARTESIAN_POINT('Ctrl Pts',(130.909073090394,-76.6550281376619,-199.133734673547)) ;
#78929 = CARTESIAN_POINT('Ctrl Pts',(131.139374153986,-76.6393870344989,-199.157648888211)) ;
#78930 = CARTESIAN_POINT('Ctrl Pts',(131.576419558745,-76.6057052246166,-199.292438924183)) ;
#78931 = CARTESIAN_POINT('Ctrl Pts',(131.77911781247,-76.5887660217225,-199.401510210809)) ;
#78932 = CARTESIAN_POINT('Ctrl Pts',(132.132208948266,-76.5564174246657,-199.691884038837)) ;
#78933 = CARTESIAN_POINT('Ctrl Pts',(132.278922193298,-76.5408350866697,-199.870700004851)) ;
#78934 = CARTESIAN_POINT('Ctrl Pts',(132.494762704611,-76.5071791018237,-200.273795297035)) ;
#78935 = CARTESIAN_POINT('Ctrl Pts',(132.562162396617,-76.490222206561,-200.494013388806)) ;
#78936 = CARTESIAN_POINT('Ctrl Pts',(132.608849707334,-76.4578312887575,-200.948662078778)) ;
#78937 = CARTESIAN_POINT('Ctrl Pts',(132.587407092316,-76.4423071791597,-201.178724080473)) ;
#78938 = CARTESIAN_POINT('Ctrl Pts',(132.457467252682,-76.408678519364,-201.617000739225)) ;
#78939 = CARTESIAN_POINT('Ctrl Pts',(132.350462124597,-76.3917037628473,-201.821075091975)) ;
#78940 = CARTESIAN_POINT('Ctrl Pts',(132.063964068573,-76.3592694308844,-202.177026212854)) ;
#78941 = CARTESIAN_POINT('Ctrl Pts',(131.887131888661,-76.3438026630912,-202.325371835702)) ;
#78942 = CARTESIAN_POINT('Ctrl Pts',(131.486699375041,-76.3102028625554,-202.545655983835)) ;
#78943 = CARTESIAN_POINT('Ctrl Pts',(131.267000568947,-76.293210143172,-202.615574936906)) ;
#78944 = CARTESIAN_POINT('Ctrl Pts',(130.974192440467,-76.2722579522,-202.648872584618)) ;
#78945 = CARTESIAN_POINT('Ctrl Pts',(130.908080100251,-76.2676343665469,-202.652605310181)) ;
#78946 = CARTESIAN_POINT('Ctrl Pts',(130.842036869423,-76.2631211627547,-202.652605310181)) ;
#78947 = CARTESIAN_POINT('Ctrl Pts',(130.842036869422,-76.3623399127545,-202.652605310181)) ;
#78948 = CARTESIAN_POINT('Ctrl Pts',(130.927732020547,-76.3681960720637,-202.652605310181)) ;
#78949 = CARTESIAN_POINT('Ctrl Pts',(131.013489712243,-76.3742343886244,-202.646321045107)) ;
#78950 = CARTESIAN_POINT('Ctrl Pts',(131.325323374,-76.396850595793,-202.600168733674)) ;
#78951 = CARTESIAN_POINT('Ctrl Pts',(131.543236919714,-76.4139412010658,-202.52248166809)) ;
#78952 = CARTESIAN_POINT('Ctrl Pts',(131.935273278315,-76.4473526944659,-202.288579923138)) ;
#78953 = CARTESIAN_POINT('Ctrl Pts',(132.105985750161,-76.4625350327593,-202.135213217096)) ;
#78954 = CARTESIAN_POINT('Ctrl Pts',(132.380323796131,-76.4952252232096,-201.770481191732)) ;
#78955 = CARTESIAN_POINT('Ctrl Pts',(132.480779023794,-76.5122986825163,-201.562249430233)) ;
#78956 = CARTESIAN_POINT('Ctrl Pts',(132.595566916625,-76.545747750087,-201.120324663123)) ;
#78957 = CARTESIAN_POINT('Ctrl Pts',(132.609330561055,-76.56097570292,-200.891017337064)) ;
#78958 = CARTESIAN_POINT('Ctrl Pts',(132.548243878357,-76.5936182194001,-200.438651334102)) ;
#78959 = CARTESIAN_POINT('Ctrl Pts',(132.473482223509,-76.6106742035755,-200.22003266576)) ;
#78960 = CARTESIAN_POINT('Ctrl Pts',(132.244694692041,-76.6441592882175,-199.824801045146)) ;
#78961 = CARTESIAN_POINT('Ctrl Pts',(132.093217587578,-76.6594358371184,-199.651783035504)) ;
#78962 = CARTESIAN_POINT('Ctrl Pts',(131.729342273886,-76.6922515818963,-199.370941121313)) ;
#78963 = CARTESIAN_POINT('Ctrl Pts',(131.519544627757,-76.7095273473052,-199.267119203586)) ;
#78964 = CARTESIAN_POINT('Ctrl Pts',(131.078444100614,-76.7430165317484,-199.148924170579)) ;
#78965 = CARTESIAN_POINT('Ctrl Pts',(130.852083649157,-76.7581224862258,-199.133067137667)) ;
#78966 = CARTESIAN_POINT('Ctrl Pts',(130.398646477582,-76.7906817392251,-199.188626258328)) ;
#78967 = CARTESIAN_POINT('Ctrl Pts',(130.176299310019,-76.8079607520649,-199.262265676444)) ;
#78968 = CARTESIAN_POINT('Ctrl Pts',(129.779379757525,-76.841483184078,-199.488297587811)) ;
#78969 = CARTESIAN_POINT('Ctrl Pts',(129.607247921277,-76.8566236548969,-199.636101837318)) ;
#78970 = CARTESIAN_POINT('Ctrl Pts',(129.323693542478,-76.8891354594,-199.994405950988)) ;
#78971 = CARTESIAN_POINT('Ctrl Pts',(129.217251752075,-76.9064170276745,-200.203203325608)) ;
#78972 = CARTESIAN_POINT('Ctrl Pts',(129.093852777237,-76.9399712233906,-200.643099641315)) ;
#78973 = CARTESIAN_POINT('Ctrl Pts',(129.075346457736,-76.9551485249676,-200.869201516679)) ;
#78974 = CARTESIAN_POINT('Ctrl Pts',(129.125582008963,-76.9876137783497,-201.323468254862)) ;
#78975 = CARTESIAN_POINT('Ctrl Pts',(129.196731061098,-77.0048972601188,-201.54691236114)) ;
#78976 = CARTESIAN_POINT('Ctrl Pts',(129.418359724146,-77.0384817382174,-201.946563740064)) ;
#78977 = CARTESIAN_POINT('Ctrl Pts',(129.564173231869,-77.0536978199423,-202.120333179967)) ;
#78978 = CARTESIAN_POINT('Ctrl Pts',(129.919389102757,-77.0861175319037,-202.408089791066)) ;
#78979 = CARTESIAN_POINT('Ctrl Pts',(130.127218863722,-77.1034023371828,-202.516981964381)) ;
#78980 = CARTESIAN_POINT('Ctrl Pts',(130.510261782241,-77.1327485220846,-202.628976575734)) ;
#78981 = CARTESIAN_POINT('Ctrl Pts',(130.675853792087,-77.1447334408586,-202.652605310181)) ;
#78982 = CARTESIAN_POINT('Ctrl Pts',(130.842036869423,-77.1560899127545,-202.652605310181)) ;
#78983 = CARTESIAN_POINT('Origin',(130.842036869422,-80.5295274127545,-200.900005310181)) ;
#78984 = CARTESIAN_POINT('',(130.842036869422,-77.9498399127545,-202.652605310181)) ;
#78985 = CARTESIAN_POINT('',(130.842036869422,-77.8506211627547,-202.652605310181)) ;
#78986 = CARTESIAN_POINT('',(130.842036869422,-80.5295274127545,-202.652605310181)) ;
#78987 = CARTESIAN_POINT('',(132.582591005309,-78.1626363340786,-200.694875936254)) ;
#78988 = CARTESIAN_POINT('Ctrl Pts',(130.842036869422,-77.9498399127545,-202.652605310181)) ;
#78989 = CARTESIAN_POINT('Ctrl Pts',(130.878973335089,-77.9523640442185,-202.652605310181)) ;
#78990 = CARTESIAN_POINT('Ctrl Pts',(130.915944065332,-77.9549235685973,-202.651437671282)) ;
#78991 = CARTESIAN_POINT('Ctrl Pts',(131.185735954615,-77.9738443881084,-202.63433819772)) ;
#78992 = CARTESIAN_POINT('Ctrl Pts',(131.413270636545,-77.9911230002116,-202.57323670437)) ;
#78993 = CARTESIAN_POINT('Ctrl Pts',(131.823569757904,-78.0249345862475,-202.369290696316)) ;
#78994 = CARTESIAN_POINT('Ctrl Pts',(132.00382073611,-78.0405744142742,-202.231335498657)) ;
#78995 = CARTESIAN_POINT('Ctrl Pts',(132.307955670742,-78.0726103610347,-201.88851951691)) ;
#78996 = CARTESIAN_POINT('Ctrl Pts',(132.426398965465,-78.0898871114286,-201.684763829815)) ;
#78997 = CARTESIAN_POINT('Ctrl Pts',(132.543724247562,-78.1168050533483,-201.339462244637)) ;
#78998 = CARTESIAN_POINT('Ctrl Pts',(132.571871931176,-78.1264000599994,-201.210714433672)) ;
#78999 = CARTESIAN_POINT('Ctrl Pts',(132.598595450617,-78.1448420342225,-200.951916059058)) ;
#79000 = CARTESIAN_POINT('Ctrl Pts',(132.597664960051,-78.1534690027399,-200.822780749546)) ;
#79001 = CARTESIAN_POINT('Ctrl Pts',(132.582591005311,-78.1626363343082,-200.69487593627)) ;
#79002 = CARTESIAN_POINT('',(131.927746207111,-78.1626363319089,-199.524199363257)) ;
#79003 = CARTESIAN_POINT('Origin',(130.842036869422,-78.162636333848,-200.900005310181)) ;
#79004 = CARTESIAN_POINT('Ctrl Pts',(131.92774620522,-78.1626363275436,-199.524199365231)) ;
#79005 = CARTESIAN_POINT('Ctrl Pts',(132.032870635821,-78.1531041953848,-199.607157704045)) ;
#79006 = CARTESIAN_POINT('Ctrl Pts',(132.128113721767,-78.1441417575876,-199.70186258093)) ;
#79007 = CARTESIAN_POINT('Ctrl Pts',(132.296967822098,-78.1249092162616,-199.913357175936)) ;
#79008 = CARTESIAN_POINT('Ctrl Pts',(132.369466681103,-78.1148993723112,-200.029804582434)) ;
#79009 = CARTESIAN_POINT('Ctrl Pts',(132.527258877092,-78.0875293201199,-200.364960104891)) ;
#79010 = CARTESIAN_POINT('Ctrl Pts',(132.583533118867,-78.0702656353602,-200.594275863051)) ;
#79011 = CARTESIAN_POINT('Ctrl Pts',(132.602412482054,-78.038398844302,-201.052773258879)) ;
#79012 = CARTESIAN_POINT('Ctrl Pts',(132.568271995862,-78.0225237872543,-201.277378390298)) ;
#79013 = CARTESIAN_POINT('Ctrl Pts',(132.413961440197,-77.9886262611793,-201.709494778747)) ;
#79014 = CARTESIAN_POINT('Ctrl Pts',(132.29212573684,-77.9713604947043,-201.911684552793)) ;
#79015 = CARTESIAN_POINT('Ctrl Pts',(131.982167398814,-77.9394706930005,-202.249949812049)) ;
#79016 = CARTESIAN_POINT('Ctrl Pts',(131.799570632373,-77.9236291961254,-202.385068504199)) ;
#79017 = CARTESIAN_POINT('Ctrl Pts',(131.385487786747,-77.889742898508,-202.582519204571)) ;
#79018 = CARTESIAN_POINT('Ctrl Pts',(131.156575821523,-77.8724750331792,-202.639915979879)) ;
#79019 = CARTESIAN_POINT('Ctrl Pts',(130.896087871841,-77.8543325329972,-202.651980685353)) ;
#79020 = CARTESIAN_POINT('Ctrl Pts',(130.869052052766,-77.8524673024178,-202.652605310181)) ;
#79021 = CARTESIAN_POINT('Ctrl Pts',(130.842036869422,-77.8506211627547,-202.652605310181)) ;
#79022 = CARTESIAN_POINT('Origin',(130.842036869422,-75.6433781549656,-200.900005310181)) ;
#79023 = CARTESIAN_POINT('',(130.842036869422,-75.7204074847575,-199.400005310181)) ;
#79024 = CARTESIAN_POINT('',(130.842036869422,-75.3175535907516,-199.400005310181)) ;
#79025 = CARTESIAN_POINT('',(130.842036869422,-75.6433781549656,-199.400005310181)) ;
#79026 = CARTESIAN_POINT('',(132.182528457453,-75.1781363338479,-200.226891425003)) ;
#79027 = CARTESIAN_POINT('Ctrl Pts',(130.842036869422,-75.3175535907516,-199.400005310181)) ;
#79028 = CARTESIAN_POINT('Ctrl Pts',(130.923497640682,-75.3110493486307,-199.400005310181)) ;
#79029 = CARTESIAN_POINT('Ctrl Pts',(131.00499096693,-75.304323094454,-199.40663952094)) ;
#79030 = CARTESIAN_POINT('Ctrl Pts',(131.281007794349,-75.2807814784863,-199.452085443423)) ;
#79031 = CARTESIAN_POINT('Ctrl Pts',(131.467996781686,-75.2635202774295,-199.522567574949)) ;
#79032 = CARTESIAN_POINT('Ctrl Pts',(131.751702866556,-75.2350150020201,-199.699532289036)) ;
#79033 = CARTESIAN_POINT('Ctrl Pts',(131.857062122586,-75.2240076020635,-199.787200645029)) ;
#79034 = CARTESIAN_POINT('Ctrl Pts',(132.042145181341,-75.2017219599688,-199.989647742754)) ;
#79035 = CARTESIAN_POINT('Ctrl Pts',(132.120680804841,-75.1900161952267,-200.103723176819)) ;
#79036 = CARTESIAN_POINT('Ctrl Pts',(132.182528457453,-75.1781363338479,-200.226891425003)) ;
#79037 = CARTESIAN_POINT('',(129.471900051694,-75.1781363338479,-201.5105174728)) ;
#79038 = CARTESIAN_POINT('Origin',(130.842036869422,-75.1781363338479,-200.900005310181)) ;
#79039 = CARTESIAN_POINT('Ctrl Pts',(129.471900051693,-75.1781363338479,-201.510517472799)) ;
#79040 = CARTESIAN_POINT('Ctrl Pts',(129.523145180104,-75.1890138594523,-201.62552392388)) ;
#79041 = CARTESIAN_POINT('Ctrl Pts',(129.588668562329,-75.1998125962201,-201.733629357294)) ;
#79042 = CARTESIAN_POINT('Ctrl Pts',(129.743608209588,-75.2205300543474,-201.928921932756)) ;
#79043 = CARTESIAN_POINT('Ctrl Pts',(129.831872765876,-75.2301658928566,-202.015704331718)) ;
#79044 = CARTESIAN_POINT('Ctrl Pts',(130.085406381744,-75.256833387257,-202.209944277907)) ;
#79045 = CARTESIAN_POINT('Ctrl Pts',(130.262879102329,-75.2738994471159,-202.297500377412)) ;
#79046 = CARTESIAN_POINT('Ctrl Pts',(130.640660017268,-75.3074266408475,-202.399192190453)) ;
#79047 = CARTESIAN_POINT('Ctrl Pts',(130.837245993353,-75.3227318075518,-202.41264856471)) ;
#79048 = CARTESIAN_POINT('Ctrl Pts',(131.225288586058,-75.3553440832905,-202.363394295449)) ;
#79049 = CARTESIAN_POINT('Ctrl Pts',(131.412936549342,-75.3723944027559,-202.30087933489)) ;
#79050 = CARTESIAN_POINT('Ctrl Pts',(131.75312498777,-75.4059516029996,-202.107523971697)) ;
#79051 = CARTESIAN_POINT('Ctrl Pts',(131.902486230923,-75.4213026058212,-201.978721156193)) ;
#79052 = CARTESIAN_POINT('Ctrl Pts',(132.143713490584,-75.453873769828,-201.670711273436)) ;
#79053 = CARTESIAN_POINT('Ctrl Pts',(132.233094454037,-75.4709082764385,-201.494389617103)) ;
#79054 = CARTESIAN_POINT('Ctrl Pts',(132.338999307863,-75.5044941579365,-201.117618780385)) ;
#79055 = CARTESIAN_POINT('Ctrl Pts',(132.354589568972,-75.5198925313956,-200.920824362433)) ;
#79056 = CARTESIAN_POINT('Ctrl Pts',(132.309343323413,-75.5524233019008,-200.532142384087)) ;
#79057 = CARTESIAN_POINT('Ctrl Pts',(132.248877081164,-75.5694419833218,-200.344042056749)) ;
#79058 = CARTESIAN_POINT('Ctrl Pts',(132.059122564365,-75.6030552274161,-200.00166019157)) ;
#79059 = CARTESIAN_POINT('Ctrl Pts',(131.931645903337,-75.6185022127119,-199.850686675688)) ;
#79060 = CARTESIAN_POINT('Ctrl Pts',(131.625957549094,-75.6509933889424,-199.606273278445)) ;
#79061 = CARTESIAN_POINT('Ctrl Pts',(131.450740290742,-75.6679962906386,-199.515181675565)) ;
#79062 = CARTESIAN_POINT('Ctrl Pts',(131.125990033399,-75.6970664972799,-199.420224974047)) ;
#79063 = CARTESIAN_POINT('Ctrl Pts',(130.98426630219,-75.7090511637559,-199.400005310181)) ;
#79064 = CARTESIAN_POINT('Ctrl Pts',(130.842036869421,-75.7204074847575,-199.400005310181)) ;
#79065 = CARTESIAN_POINT('Origin',(130.842036869422,-75.6433781549656,-200.900005310181)) ;
#79066 = CARTESIAN_POINT('',(130.842036869422,-76.5141574847575,-199.400005310181)) ;
#79067 = CARTESIAN_POINT('',(130.842036869422,-76.1113035907516,-199.400005310181)) ;
#79068 = CARTESIAN_POINT('',(130.842036869422,-75.6433781549656,-199.400005310181)) ;
#79069 = CARTESIAN_POINT('Ctrl Pts',(130.842036869422,-76.1113035907516,-199.400005310181)) ;
#79070 = CARTESIAN_POINT('Ctrl Pts',(130.949133951451,-76.1027524152448,-199.400005310181)) ;
#79071 = CARTESIAN_POINT('Ctrl Pts',(131.056137952684,-76.0938294801729,-199.411470631266)) ;
#79072 = CARTESIAN_POINT('Ctrl Pts',(131.35367248696,-76.0679295416266,-199.476274975455)) ;
#79073 = CARTESIAN_POINT('Ctrl Pts',(131.535967499815,-76.0507484264606,-199.555667869188)) ;
#79074 = CARTESIAN_POINT('Ctrl Pts',(131.856884803169,-76.0177530719082,-199.778559777848)) ;
#79075 = CARTESIAN_POINT('Ctrl Pts',(131.993103698459,-76.0027441261626,-199.918882943764)) ;
#79076 = CARTESIAN_POINT('Ctrl Pts',(132.206435794837,-75.9695406232978,-200.246366953058)) ;
#79077 = CARTESIAN_POINT('Ctrl Pts',(132.280411469569,-75.9523470991235,-200.431061265048)) ;
#79078 = CARTESIAN_POINT('Ctrl Pts',(132.352103988871,-75.9193090849539,-200.815141685916)) ;
#79079 = CARTESIAN_POINT('Ctrl Pts',(132.350440326257,-75.9043164329487,-201.010564209893)) ;
#79080 = CARTESIAN_POINT('Ctrl Pts',(132.272196408425,-75.8711545191446,-201.393482702957)) ;
#79081 = CARTESIAN_POINT('Ctrl Pts',(132.195018141393,-75.8539492166687,-201.576997972207)) ;
#79082 = CARTESIAN_POINT('Ctrl Pts',(131.976138215843,-75.8208689999167,-201.900639928999)) ;
#79083 = CARTESIAN_POINT('Ctrl Pts',(131.837740354137,-75.8058886898989,-202.038438444838)) ;
#79084 = CARTESIAN_POINT('Ctrl Pts',(131.513051259311,-75.7727691594772,-202.255979052327)) ;
#79085 = CARTESIAN_POINT('Ctrl Pts',(131.329077594801,-75.7555527454817,-202.33238662566)) ;
#79086 = CARTESIAN_POINT('Ctrl Pts',(130.945923266647,-75.7224308342911,-202.408851659376)) ;
#79087 = CARTESIAN_POINT('Ctrl Pts',(130.750746000305,-75.7074589752768,-202.409666134416)) ;
#79088 = CARTESIAN_POINT('Ctrl Pts',(130.366844379053,-75.6743824609859,-202.336377856499)) ;
#79089 = CARTESIAN_POINT('Ctrl Pts',(130.182132440041,-75.65715563652,-202.261437862205)) ;
#79090 = CARTESIAN_POINT('Ctrl Pts',(129.85578178882,-75.6239926625053,-202.046595036644)) ;
#79091 = CARTESIAN_POINT('Ctrl Pts',(129.716409296074,-75.6090253037173,-201.910119156804)) ;
#79092 = CARTESIAN_POINT('Ctrl Pts',(129.494688502418,-75.5759923565716,-201.588245942602)) ;
#79093 = CARTESIAN_POINT('Ctrl Pts',(129.415861126859,-75.5587558370719,-201.405022786578)) ;
#79094 = CARTESIAN_POINT('Ctrl Pts',(129.334640315407,-75.5255525576802,-201.022819290159)) ;
#79095 = CARTESIAN_POINT('Ctrl Pts',(129.331365796756,-75.5105857242824,-200.827887032132)) ;
#79096 = CARTESIAN_POINT('Ctrl Pts',(129.399727674285,-75.4775968060397,-200.44304190406)) ;
#79097 = CARTESIAN_POINT('Ctrl Pts',(129.472428123445,-75.460351321514,-200.257168611777)) ;
#79098 = CARTESIAN_POINT('Ctrl Pts',(129.683247340528,-75.4271085811011,-199.928152312836)) ;
#79099 = CARTESIAN_POINT('Ctrl Pts',(129.817824620494,-75.412138369452,-199.787224430205)) ;
#79100 = CARTESIAN_POINT('Ctrl Pts',(130.136887807839,-75.3791938198857,-199.561392440293)) ;
#79101 = CARTESIAN_POINT('Ctrl Pts',(130.319338815088,-75.3619401079321,-199.480181097861)) ;
#79102 = CARTESIAN_POINT('Ctrl Pts',(130.620752245873,-75.3356272410693,-199.412255846619)) ;
#79103 = CARTESIAN_POINT('Ctrl Pts',(130.731332038619,-75.3263928272623,-199.400005310181)) ;
#79104 = CARTESIAN_POINT('Ctrl Pts',(130.842036869422,-75.3175535907516,-199.400005310181)) ;
#79105 = CARTESIAN_POINT('Ctrl Pts',(130.842036869421,-75.7204074847575,-199.400005310181)) ;
#79106 = CARTESIAN_POINT('Ctrl Pts',(130.789053275896,-75.7246379642313,-199.400005310181)) ;
#79107 = CARTESIAN_POINT('Ctrl Pts',(130.736014303355,-75.7289657007846,-199.402812299913)) ;
#79108 = CARTESIAN_POINT('Ctrl Pts',(130.488691675152,-75.7495845976627,-199.429160168525)) ;
#79109 = CARTESIAN_POINT('Ctrl Pts',(130.300185846525,-75.7665718200039,-199.487696240402)) ;
#79110 = CARTESIAN_POINT('Ctrl Pts',(129.955758181003,-75.800235894582,-199.674048679986)) ;
#79111 = CARTESIAN_POINT('Ctrl Pts',(129.803265972982,-75.8157826860376,-199.800274398092)) ;
#79112 = CARTESIAN_POINT('Ctrl Pts',(129.555874234132,-75.8481973565873,-200.103770906374)) ;
#79113 = CARTESIAN_POINT('Ctrl Pts',(129.463190942205,-75.8651690514804,-200.277938023653)) ;
#79114 = CARTESIAN_POINT('Ctrl Pts',(129.349584642592,-75.898856639705,-200.65279261781)) ;
#79115 = CARTESIAN_POINT('Ctrl Pts',(129.330079232436,-75.9144540804814,-200.849965531322)) ;
#79116 = CARTESIAN_POINT('Ctrl Pts',(129.368016288118,-75.9468319620272,-201.2397602553)) ;
#79117 = CARTESIAN_POINT('Ctrl Pts',(129.424747760915,-75.963788329165,-201.428627134975)) ;
#79118 = CARTESIAN_POINT('Ctrl Pts',(129.607910594488,-75.9974982023313,-201.774949571655)) ;
#79119 = CARTESIAN_POINT('Ctrl Pts',(129.73296496394,-76.01314644887,-201.928861605832)) ;
#79120 = CARTESIAN_POINT('Ctrl Pts',(130.034407896328,-76.045488585227,-202.179017955619)) ;
#79121 = CARTESIAN_POINT('Ctrl Pts',(130.207584873293,-76.0624298680528,-202.273172111748)) ;
#79122 = CARTESIAN_POINT('Ctrl Pts',(130.581547837697,-76.0961608319643,-202.390242512836)) ;
#79123 = CARTESIAN_POINT('Ctrl Pts',(130.77888951949,-76.111859804738,-202.411515470159)) ;
#79124 = CARTESIAN_POINT('Ctrl Pts',(131.169161293525,-76.1441672804533,-202.376858921408)) ;
#79125 = CARTESIAN_POINT('Ctrl Pts',(131.35834777257,-76.1610937619284,-202.321802659239)) ;
#79126 = CARTESIAN_POINT('Ctrl Pts',(131.706413790785,-76.1948446602018,-202.141608759678)) ;
#79127 = CARTESIAN_POINT('Ctrl Pts',(131.861643938923,-76.2105940614007,-202.017643661455)) ;
#79128 = CARTESIAN_POINT('Ctrl Pts',(132.114349873871,-76.2428679937785,-201.718111005681)) ;
#79129 = CARTESIAN_POINT('Ctrl Pts',(132.20985468799,-76.2597799920395,-201.545860256861)) ;
#79130 = CARTESIAN_POINT('Ctrl Pts',(132.330125403464,-76.2935497087167,-201.172737556653)) ;
#79131 = CARTESIAN_POINT('Ctrl Pts',(132.353035129703,-76.3093490409428,-200.975240991203)) ;
#79132 = CARTESIAN_POINT('Ctrl Pts',(132.321405445704,-76.3415905723374,-200.584541352067)) ;
#79133 = CARTESIAN_POINT('Ctrl Pts',(132.267894073625,-76.3584884363231,-200.395073371258)) ;
#79134 = CARTESIAN_POINT('Ctrl Pts',(132.090445274992,-76.3922758978451,-200.045412367649)) ;
#79135 = CARTESIAN_POINT('Ctrl Pts',(131.96748662106,-76.4081244833936,-199.888966462595)) ;
#79136 = CARTESIAN_POINT('Ctrl Pts',(131.669719158122,-76.4403347738487,-199.63392326637)) ;
#79137 = CARTESIAN_POINT('Ctrl Pts',(131.498328538328,-76.4572188789652,-199.537185300362)) ;
#79138 = CARTESIAN_POINT('Ctrl Pts',(131.161010070314,-76.4878437443242,-199.425563939749)) ;
#79139 = CARTESIAN_POINT('Ctrl Pts',(131.001940017472,-76.5013900044752,-199.400005310181)) ;
#79140 = CARTESIAN_POINT('Ctrl Pts',(130.842036869421,-76.5141574847575,-199.400005310181)) ;
#79141 = CARTESIAN_POINT('Origin',(130.842036869422,-75.6433781549656,-200.900005310181)) ;
#79142 = CARTESIAN_POINT('',(130.842036869422,-77.3079074847574,-199.400005310181)) ;
#79143 = CARTESIAN_POINT('',(130.842036869422,-76.9050535907517,-199.400005310181)) ;
#79144 = CARTESIAN_POINT('',(130.842036869422,-75.6433781549656,-199.400005310181)) ;
#79145 = CARTESIAN_POINT('Ctrl Pts',(130.842036869422,-76.9050535907517,-199.400005310181)) ;
#79146 = CARTESIAN_POINT('Ctrl Pts',(130.973277756236,-76.8945746511246,-199.400005310181)) ;
#79147 = CARTESIAN_POINT('Ctrl Pts',(131.104164513265,-76.883554604073,-199.417221298495)) ;
#79148 = CARTESIAN_POINT('Ctrl Pts',(131.42316821846,-76.8552478784647,-199.502966623318)) ;
#79149 = CARTESIAN_POINT('Ctrl Pts',(131.602820838047,-76.8379560643228,-199.592085937357)) ;
#79150 = CARTESIAN_POINT('Ctrl Pts',(131.912295362626,-76.8053273979256,-199.831515893817)) ;
#79151 = CARTESIAN_POINT('Ctrl Pts',(132.040530630802,-76.7902332168997,-199.97765127425)) ;
#79152 = CARTESIAN_POINT('Ctrl Pts',(132.237649557133,-76.756738893529,-200.315493307942)) ;
#79153 = CARTESIAN_POINT('Ctrl Pts',(132.302667737018,-76.7394503735366,-200.505087687405)) ;
#79154 = CARTESIAN_POINT('Ctrl Pts',(132.354348630853,-76.7067785325167,-200.892871149926)) ;
#79155 = CARTESIAN_POINT('Ctrl Pts',(132.342762418159,-76.6917106911163,-201.086984832368)) ;
#79156 = CARTESIAN_POINT('Ctrl Pts',(132.2458886052,-76.6584315923737,-201.463654223975)) ;
#79157 = CARTESIAN_POINT('Ctrl Pts',(132.160197310018,-76.6413355443219,-201.642274951503)) ;
#79158 = CARTESIAN_POINT('Ctrl Pts',(131.925793584997,-76.6085994180286,-201.955177264194)) ;
#79159 = CARTESIAN_POINT('Ctrl Pts',(131.77984294802,-76.5934170441698,-202.086780793741)) ;
#79160 = CARTESIAN_POINT('Ctrl Pts',(131.444367472244,-76.5599854470804,-202.28771649062)) ;
#79161 = CARTESIAN_POINT('Ctrl Pts',(131.257750790847,-76.5428742303957,-202.354562487653)) ;
#79162 = CARTESIAN_POINT('Ctrl Pts',(130.871128061817,-76.5100950834768,-202.412290164846)) ;
#79163 = CARTESIAN_POINT('Ctrl Pts',(130.674983186419,-76.4949496843938,-202.403316448077)) ;
#79164 = CARTESIAN_POINT('Ctrl Pts',(130.29516011843,-76.4615532102009,-202.310507293421)) ;
#79165 = CARTESIAN_POINT('Ctrl Pts',(130.115325229674,-76.4444271428584,-202.22683957285)) ;
#79166 = CARTESIAN_POINT('Ctrl Pts',(129.799803199283,-76.4116047496094,-201.99615201914)) ;
#79167 = CARTESIAN_POINT('Ctrl Pts',(129.666695505079,-76.3964933948748,-201.852035070149)) ;
#79168 = CARTESIAN_POINT('Ctrl Pts',(129.461705145776,-76.363133274824,-201.519134287027)) ;
#79169 = CARTESIAN_POINT('Ctrl Pts',(129.392533140982,-76.3459927355846,-201.333113826507)) ;
#79170 = CARTESIAN_POINT('Ctrl Pts',(129.330252747718,-76.3131269832385,-200.947292225973)) ;
#79171 = CARTESIAN_POINT('Ctrl Pts',(129.336833153221,-76.2980465000572,-200.751383852506)) ;
#79172 = CARTESIAN_POINT('Ctrl Pts',(129.424883567968,-76.264723917436,-200.370515086616)) ;
#79173 = CARTESIAN_POINT('Ctrl Pts',(129.506446128229,-76.2475693434764,-200.189451187835)) ;
#79174 = CARTESIAN_POINT('Ctrl Pts',(129.733285788991,-76.2146602341759,-199.871249254266)) ;
#79175 = CARTESIAN_POINT('Ctrl Pts',(129.875521313557,-76.1996072313484,-199.736598692578)) ;
#79176 = CARTESIAN_POINT('Ctrl Pts',(130.205750886396,-76.1663233112515,-199.527463459781)) ;
#79177 = CARTESIAN_POINT('Ctrl Pts',(130.391129269758,-76.1491551949364,-199.455907517061)) ;
#79178 = CARTESIAN_POINT('Ctrl Pts',(130.670105432118,-76.1252757574679,-199.407391615755)) ;
#79179 = CARTESIAN_POINT('Ctrl Pts',(130.756081559722,-76.1181666996718,-199.400005310181)) ;
#79180 = CARTESIAN_POINT('Ctrl Pts',(130.842036869422,-76.1113035907516,-199.400005310181)) ;
#79181 = CARTESIAN_POINT('Ctrl Pts',(130.842036869421,-76.5141574847575,-199.400005310181)) ;
#79182 = CARTESIAN_POINT('Ctrl Pts',(130.805260101874,-76.5170939288503,-199.400005310181)) ;
#79183 = CARTESIAN_POINT('Ctrl Pts',(130.768446344966,-76.5200780567153,-199.401357787018)) ;
#79184 = CARTESIAN_POINT('Ctrl Pts',(130.537271994658,-76.5391002762126,-199.418413557827)) ;
#79185 = CARTESIAN_POINT('Ctrl Pts',(130.347557096745,-76.5559710200978,-199.470508809946)) ;
#79186 = CARTESIAN_POINT('Ctrl Pts',(129.996444879957,-76.5897909265991,-199.645435083595)) ;
#79187 = CARTESIAN_POINT('Ctrl Pts',(129.838884319023,-76.6057353618368,-199.767469352618)) ;
#79188 = CARTESIAN_POINT('Ctrl Pts',(129.581710192247,-76.6378866870249,-200.063615659322)) ;
#79189 = CARTESIAN_POINT('Ctrl Pts',(129.48385222616,-76.6547444854666,-200.234212888455)) ;
#79190 = CARTESIAN_POINT('Ctrl Pts',(129.359505721472,-76.6881636884534,-200.601257419495)) ;
#79191 = CARTESIAN_POINT('Ctrl Pts',(129.333434136973,-76.7038450753353,-200.793982602854)) ;
#79192 = CARTESIAN_POINT('Ctrl Pts',(129.356031997873,-76.7358905682875,-201.18596811064)) ;
#79193 = CARTESIAN_POINT('Ctrl Pts',(129.407341104038,-76.7531804135556,-201.381257572453)) ;
#79194 = CARTESIAN_POINT('Ctrl Pts',(129.580292633447,-76.7870465825427,-201.733767158146)) ;
#79195 = CARTESIAN_POINT('Ctrl Pts',(129.697743348234,-76.8027593414652,-201.888803616562)) ;
#79196 = CARTESIAN_POINT('Ctrl Pts',(129.990270832118,-76.8347813779517,-202.150805152778)) ;
#79197 = CARTESIAN_POINT('Ctrl Pts',(130.164427716409,-76.8520696019562,-202.253083793321)) ;
#79198 = CARTESIAN_POINT('Ctrl Pts',(130.535734909097,-76.8859472142279,-202.380999886652)) ;
#79199 = CARTESIAN_POINT('Ctrl Pts',(130.728367360873,-76.9016902851713,-202.408055647389)) ;
#79200 = CARTESIAN_POINT('Ctrl Pts',(131.120596328859,-76.9336900193736,-202.387429123056)) ;
#79201 = CARTESIAN_POINT('Ctrl Pts',(131.316234964971,-76.9509766065318,-202.337061511149)) ;
#79202 = CARTESIAN_POINT('Ctrl Pts',(131.669706269178,-76.9848649572559,-202.165761083734)) ;
#79203 = CARTESIAN_POINT('Ctrl Pts',(131.825339272788,-77.0006372432278,-202.049030903486)) ;
#79204 = CARTESIAN_POINT('Ctrl Pts',(132.088820735292,-77.0326157990592,-201.757660987844)) ;
#79205 = CARTESIAN_POINT('Ctrl Pts',(132.19196169619,-77.0499007470333,-201.58390231817)) ;
#79206 = CARTESIAN_POINT('Ctrl Pts',(132.321624870104,-77.0837991688935,-201.21305816541)) ;
#79207 = CARTESIAN_POINT('Ctrl Pts',(132.34956107743,-77.0995995474399,-201.020508531354)) ;
#79208 = CARTESIAN_POINT('Ctrl Pts',(132.330697244536,-77.1315580160005,-200.628066253989)) ;
#79209 = CARTESIAN_POINT('Ctrl Pts',(132.28117262879,-77.1488413339024,-200.432119382427)) ;
#79210 = CARTESIAN_POINT('Ctrl Pts',(132.111349949548,-77.1827491959449,-200.077791610206)) ;
#79211 = CARTESIAN_POINT('Ctrl Pts',(131.995263067737,-77.1985765294972,-199.921625849429)) ;
#79212 = CARTESIAN_POINT('Ctrl Pts',(131.704929039509,-77.2305159670289,-199.656826323022)) ;
#79213 = CARTESIAN_POINT('Ctrl Pts',(131.531529005047,-77.2477976737595,-199.552917543089)) ;
#79214 = CARTESIAN_POINT('Ctrl Pts',(131.181874606249,-77.2798123464763,-199.429055232196)) ;
#79215 = CARTESIAN_POINT('Ctrl Pts',(131.012501544664,-77.2942967184498,-199.400005310181)) ;
#79216 = CARTESIAN_POINT('Ctrl Pts',(130.842036869422,-77.3079074847575,-199.400005310181)) ;
#79217 = CARTESIAN_POINT('Origin',(130.842036869422,-75.6433781549656,-200.900005310181)) ;
#79218 = CARTESIAN_POINT('',(130.842036869422,-78.1016574847575,-199.400005310181)) ;
#79219 = CARTESIAN_POINT('',(130.842036869422,-77.6988035907517,-199.400005310181)) ;
#79220 = CARTESIAN_POINT('',(130.842036869422,-75.6433781549656,-199.400005310181)) ;
#79221 = CARTESIAN_POINT('',(130.148682626495,-78.162636333848,-199.569870018636)) ;
#79222 = CARTESIAN_POINT('Ctrl Pts',(130.842036869422,-78.1016574847575,-199.400005310181)) ;
#79223 = CARTESIAN_POINT('Ctrl Pts',(130.826012984664,-78.1029369131814,-199.400005310181)) ;
#79224 = CARTESIAN_POINT('Ctrl Pts',(130.809980207002,-78.1042255435838,-199.40026207386)) ;
#79225 = CARTESIAN_POINT('Ctrl Pts',(130.682617796906,-78.1145299262998,-199.404347603704)) ;
#79226 = CARTESIAN_POINT('Ctrl Pts',(130.572056402493,-78.12388553057,-199.420306899202)) ;
#79227 = CARTESIAN_POINT('Ctrl Pts',(130.354846362033,-78.1430979579179,-199.476826662743)) ;
#79228 = CARTESIAN_POINT('Ctrl Pts',(130.248972434197,-78.1528997109598,-199.517592356254)) ;
#79229 = CARTESIAN_POINT('Ctrl Pts',(130.148682626494,-78.1626363338481,-199.569870018636)) ;
#79230 = CARTESIAN_POINT('',(131.596354821607,-78.162636333848,-202.196540858098)) ;
#79231 = CARTESIAN_POINT('Origin',(130.842036869422,-78.162636333848,-200.900005310181)) ;
#79232 = CARTESIAN_POINT('Ctrl Pts',(131.596354821608,-78.1626363338481,-202.196540858097)) ;
#79233 = CARTESIAN_POINT('Ctrl Pts',(131.49689101871,-78.1527807895855,-202.254408405376)) ;
#79234 = CARTESIAN_POINT('Ctrl Pts',(131.39110873996,-78.1428057769923,-202.300634073335)) ;
#79235 = CARTESIAN_POINT('Ctrl Pts',(131.172260974558,-78.1231163253183,-202.367623431803)) ;
#79236 = CARTESIAN_POINT('Ctrl Pts',(131.059986449382,-78.1134630724344,-202.388446632887)) ;
#79237 = CARTESIAN_POINT('Ctrl Pts',(130.754280448219,-78.0883486428074,-202.409772490022)) ;
#79238 = CARTESIAN_POINT('Ctrl Pts',(130.561333404588,-78.0728041866019,-202.38604789494)) ;
#79239 = CARTESIAN_POINT('Ctrl Pts',(130.188312935722,-78.0390081124059,-202.264733419426)) ;
#79240 = CARTESIAN_POINT('Ctrl Pts',(130.012689248877,-78.0217109294338,-202.165725068183)) ;
#79241 = CARTESIAN_POINT('Ctrl Pts',(129.715826498257,-77.9895282788732,-201.90933342916)) ;
#79242 = CARTESIAN_POINT('Ctrl Pts',(129.595660741605,-77.974019492826,-201.756542963972)) ;
#79243 = CARTESIAN_POINT('Ctrl Pts',(129.416527173312,-77.9402399793395,-201.407679358008)) ;
#79244 = CARTESIAN_POINT('Ctrl Pts',(129.361697254571,-77.9229416709976,-201.213742270841)) ;
#79245 = CARTESIAN_POINT('Ctrl Pts',(129.331700777835,-77.8907281445107,-200.822716875643)) ;
#79246 = CARTESIAN_POINT('Ctrl Pts',(129.35408257953,-77.8752555553349,-200.629642407692)) ;
#79247 = CARTESIAN_POINT('Ctrl Pts',(129.472740133472,-77.8414935896882,-200.255948589964)) ;
#79248 = CARTESIAN_POINT('Ctrl Pts',(129.570427250837,-77.8241943253707,-200.079751562834)) ;
#79249 = CARTESIAN_POINT('Ctrl Pts',(129.824553178997,-77.7919486768708,-199.781161321941)) ;
#79250 = CARTESIAN_POINT('Ctrl Pts',(129.976443198279,-77.7765126636698,-199.659905991275)) ;
#79251 = CARTESIAN_POINT('Ctrl Pts',(130.323834208348,-77.7427692720935,-199.478309452035)) ;
#79252 = CARTESIAN_POINT('Ctrl Pts',(130.517212622459,-77.7254692521619,-199.422079025222)) ;
#79253 = CARTESIAN_POINT('Ctrl Pts',(130.757947644041,-77.7055761044962,-199.401771180552)) ;
#79254 = CARTESIAN_POINT('Ctrl Pts',(130.800013424201,-77.7021589562638,-199.400005310181)) ;
#79255 = CARTESIAN_POINT('Ctrl Pts',(130.842036869421,-77.6988035907517,-199.400005310181)) ;
#79256 = CARTESIAN_POINT('Origin',(130.842036869422,-75.6433781549656,-200.900005310181)) ;
#79257 = CARTESIAN_POINT('Ctrl Pts',(130.842036869421,-77.6988035907517,-199.400005310181)) ;
#79258 = CARTESIAN_POINT('Ctrl Pts',(130.992008831122,-77.6868290668776,-199.400005310181)) ;
#79259 = CARTESIAN_POINT('Ctrl Pts',(131.141323533336,-77.6741634905891,-199.422486888103)) ;
#79260 = CARTESIAN_POINT('Ctrl Pts',(131.475469354102,-77.6440672695971,-199.525783489103)) ;
#79261 = CARTESIAN_POINT('Ctrl Pts',(131.652283192623,-77.6267667275403,-199.622020126052)) ;
#79262 = CARTESIAN_POINT('Ctrl Pts',(131.952754395999,-77.5944531510418,-199.873658895021)) ;
#79263 = CARTESIAN_POINT('Ctrl Pts',(132.075201405575,-77.5790907454146,-200.024564717812)) ;
#79264 = CARTESIAN_POINT('Ctrl Pts',(132.259479675576,-77.5453877295651,-200.370339242824)) ;
#79265 = CARTESIAN_POINT('Ctrl Pts',(132.317233347614,-77.5280869339979,-200.56309642236)) ;
#79266 = CARTESIAN_POINT('Ctrl Pts',(132.353408227123,-77.4957375987893,-200.95326354207)) ;
#79267 = CARTESIAN_POINT('Ctrl Pts',(132.334104045199,-77.4804118388597,-201.146631517833)) ;
#79268 = CARTESIAN_POINT('Ctrl Pts',(132.22152570243,-77.4467306937986,-201.521831209849)) ;
#79269 = CARTESIAN_POINT('Ctrl Pts',(132.126871825135,-77.4294299502341,-201.699303172619)) ;
#79270 = CARTESIAN_POINT('Ctrl Pts',(131.877947072605,-77.3970437056544,-202.001808671817)) ;
#79271 = CARTESIAN_POINT('Ctrl Pts',(131.728110265776,-77.3817541999581,-202.125551001611)) ;
#79272 = CARTESIAN_POINT('Ctrl Pts',(131.384099552374,-77.3480960890395,-202.312729734136)) ;
#79273 = CARTESIAN_POINT('Ctrl Pts',(131.192029511511,-77.3307957413689,-202.372128762973)) ;
#79274 = CARTESIAN_POINT('Ctrl Pts',(130.802370384407,-77.2983714823411,-202.411795458234)) ;
#79275 = CARTESIAN_POINT('Ctrl Pts',(130.608835675341,-77.2831176049036,-202.394229680283)) ;
#79276 = CARTESIAN_POINT('Ctrl Pts',(130.232808390015,-77.2494837181064,-202.285078235795)) ;
#79277 = CARTESIAN_POINT('Ctrl Pts',(130.054640466163,-77.2321841497198,-202.192140090124)) ;
#79278 = CARTESIAN_POINT('Ctrl Pts',(129.749950823865,-77.1997208259819,-201.94615774307)) ;
#79279 = CARTESIAN_POINT('Ctrl Pts',(129.624809896354,-77.1845017022962,-201.79747424918)) ;
#79280 = CARTESIAN_POINT('Ctrl Pts',(129.434516675332,-77.1508932519114,-201.455375560225)) ;
#79281 = CARTESIAN_POINT('Ctrl Pts',(129.373353578203,-77.1335948863862,-201.26406104526)) ;
#79282 = CARTESIAN_POINT('Ctrl Pts',(129.329930478591,-77.1010915117849,-200.874967008356)) ;
#79283 = CARTESIAN_POINT('Ctrl Pts',(129.345626577679,-77.0859060069524,-200.68125218463)) ;
#79284 = CARTESIAN_POINT('Ctrl Pts',(129.451098485901,-77.0523242226114,-200.304353329801)) ;
#79285 = CARTESIAN_POINT('Ctrl Pts',(129.542190023052,-77.0350275239044,-200.125456456248)) ;
#79286 = CARTESIAN_POINT('Ctrl Pts',(129.785004660559,-77.0024831856076,-199.818440058895)) ;
#79287 = CARTESIAN_POINT('Ctrl Pts',(129.932452894176,-76.9873298951115,-199.691799819314)) ;
#79288 = CARTESIAN_POINT('Ctrl Pts',(130.272493493307,-76.9537760181528,-199.498188024059)) ;
#79289 = CARTESIAN_POINT('Ctrl Pts',(130.46298275716,-76.9364814902319,-199.435148629158)) ;
#79290 = CARTESIAN_POINT('Ctrl Pts',(130.720672404424,-76.9148656030244,-199.403683739152)) ;
#79291 = CARTESIAN_POINT('Ctrl Pts',(130.781382737284,-76.9098965250249,-199.400005310181)) ;
#79292 = CARTESIAN_POINT('Ctrl Pts',(130.842036869422,-76.9050535907517,-199.400005310181)) ;
#79293 = CARTESIAN_POINT('Ctrl Pts',(130.842036869422,-77.3079074847574,-199.400005310181)) ;
#79294 = CARTESIAN_POINT('Ctrl Pts',(130.820046030699,-77.3096633451218,-199.400005310181)) ;
#79295 = CARTESIAN_POINT('Ctrl Pts',(130.798039539999,-77.3114364490101,-199.400488901959)) ;
#79296 = CARTESIAN_POINT('Ctrl Pts',(130.575996418083,-77.3294889515356,-199.410268832037)) ;
#79297 = CARTESIAN_POINT('Ctrl Pts',(130.379778101036,-77.3467690742638,-199.459041510435)) ;
#79298 = CARTESIAN_POINT('Ctrl Pts',(130.024690032456,-77.3806940629399,-199.62754651657)) ;
#79299 = CARTESIAN_POINT('Ctrl Pts',(129.86805013415,-77.3965718782909,-199.743061024941)) ;
#79300 = CARTESIAN_POINT('Ctrl Pts',(129.602080452281,-77.428476275587,-200.032471506143)) ;
#79301 = CARTESIAN_POINT('Ctrl Pts',(129.497490180716,-77.4457548483642,-200.205550007105)) ;
#79302 = CARTESIAN_POINT('Ctrl Pts',(129.364884363641,-77.4796875897104,-200.575605103068)) ;
#79303 = CARTESIAN_POINT('Ctrl Pts',(129.335466147829,-77.4955889433358,-200.768015612496)) ;
#79304 = CARTESIAN_POINT('Ctrl Pts',(129.351364949874,-77.5274772554681,-201.160807389023)) ;
#79305 = CARTESIAN_POINT('Ctrl Pts',(129.399469184275,-77.5447543179783,-201.357264257698)) ;
#79306 = CARTESIAN_POINT('Ctrl Pts',(129.566803157659,-77.5786943134002,-201.713025332201)) ;
#79307 = CARTESIAN_POINT('Ctrl Pts',(129.681809956479,-77.5946180886615,-201.87008589028)) ;
#79308 = CARTESIAN_POINT('Ctrl Pts',(129.970399781909,-77.6264912206868,-202.137091466825)) ;
#79309 = CARTESIAN_POINT('Ctrl Pts',(130.143191170662,-77.6437668171255,-202.242284895348)) ;
#79310 = CARTESIAN_POINT('Ctrl Pts',(130.512913843575,-77.6777135976496,-202.376117744342)) ;
#79311 = CARTESIAN_POINT('Ctrl Pts',(130.705266466733,-77.6936586984264,-202.406153605062)) ;
#79312 = CARTESIAN_POINT('Ctrl Pts',(131.098200371139,-77.7255175164878,-202.391489719301)) ;
#79313 = CARTESIAN_POINT('Ctrl Pts',(131.294866508558,-77.7427916945635,-202.343977918736)) ;
#79314 = CARTESIAN_POINT('Ctrl Pts',(131.651221821218,-77.7767448194291,-202.177681578418)) ;
#79315 = CARTESIAN_POINT('Ctrl Pts',(131.808654563925,-77.7927101744347,-202.063123903972)) ;
#79316 = CARTESIAN_POINT('Ctrl Pts',(132.07657487055,-77.8245555059074,-201.775261153286)) ;
#79317 = CARTESIAN_POINT('Ctrl Pts',(132.182300787846,-77.8418283159611,-201.602725225993)) ;
#79318 = CARTESIAN_POINT('Ctrl Pts',(132.317218105444,-77.8757873712274,-201.233298022712)) ;
#79319 = CARTESIAN_POINT('Ctrl Pts',(132.347799699357,-77.8917719375526,-201.040996502765)) ;
#79320 = CARTESIAN_POINT('Ctrl Pts',(132.334226538529,-77.9236045714227,-200.647938742724)) ;
#79321 = CARTESIAN_POINT('Ctrl Pts',(132.287238405253,-77.9408760656535,-200.451089308365)) ;
#79322 = CARTESIAN_POINT('Ctrl Pts',(132.121859081654,-77.9748406628289,-200.094210472838)) ;
#79323 = CARTESIAN_POINT('Ctrl Pts',(132.007697746346,-77.9908434287853,-199.936449239791)) ;
#79324 = CARTESIAN_POINT('Ctrl Pts',(131.720477474982,-78.0226641162253,-199.667722993288)) ;
#79325 = CARTESIAN_POINT('Ctrl Pts',(131.548168129765,-78.0399343480179,-199.561528015344)) ;
#79326 = CARTESIAN_POINT('Ctrl Pts',(131.194068406748,-78.0725178154868,-199.431199462941)) ;
#79327 = CARTESIAN_POINT('Ctrl Pts',(131.018673974061,-78.0875538803064,-199.400005310181)) ;
#79328 = CARTESIAN_POINT('Ctrl Pts',(130.842036869422,-78.1016574847574,-199.400005310181)) ;
#79329 = CARTESIAN_POINT('Origin',(130.842036869422,-80.5295274127545,-200.900005310181)) ;
#79330 = CARTESIAN_POINT('Ctrl Pts',(130.842036869422,-77.8506211627547,-202.652605310181)) ;
#79331 = CARTESIAN_POINT('Ctrl Pts',(130.644451329195,-77.8371187371731,-202.652605310181)) ;
#79332 = CARTESIAN_POINT('Ctrl Pts',(130.448097214639,-77.8227548518017,-202.619198734178)) ;
#79333 = CARTESIAN_POINT('Ctrl Pts',(130.040901161784,-77.7908800902098,-202.476185390008)) ;
#79334 = CARTESIAN_POINT('Ctrl Pts',(129.838174909486,-77.7736101243252,-202.355496502983)) ;
#79335 = CARTESIAN_POINT('Ctrl Pts',(129.498362301134,-77.7416703239782,-202.047507444084)) ;
#79336 = CARTESIAN_POINT('Ctrl Pts',(129.362281696203,-77.7259000849022,-201.865706510437)) ;
#79337 = CARTESIAN_POINT('Ctrl Pts',(129.162621889232,-77.6920386786955,-201.452902951119)) ;
#79338 = CARTESIAN_POINT('Ctrl Pts',(129.103964484698,-77.6747666285661,-201.224451918021)) ;
#79339 = CARTESIAN_POINT('Ctrl Pts',(129.080106017582,-77.642799764517,-200.766552532796)) ;
#79340 = CARTESIAN_POINT('Ctrl Pts',(129.111757813305,-77.6270671276914,-200.541712232754)) ;
#79341 = CARTESIAN_POINT('Ctrl Pts',(129.261129496703,-77.5932194816432,-200.108280007658)) ;
#79342 = CARTESIAN_POINT('Ctrl Pts',(129.380527623304,-77.5759453843576,-199.904958648707)) ;
#79343 = CARTESIAN_POINT('Ctrl Pts',(129.686301058074,-77.5439500369427,-199.563415459841)) ;
#79344 = CARTESIAN_POINT('Ctrl Pts',(129.867209754028,-77.528256224698,-199.426255935562)) ;
#79345 = CARTESIAN_POINT('Ctrl Pts',(130.278573687824,-77.4944232819949,-199.224126123784)) ;
#79346 = CARTESIAN_POINT('Ctrl Pts',(130.506500212819,-77.4771471983583,-199.164059948942)) ;
#79347 = CARTESIAN_POINT('Ctrl Pts',(130.964032215596,-77.4451219218751,-199.137250947671)) ;
#79348 = CARTESIAN_POINT('Ctrl Pts',(131.189012232965,-77.4294680618709,-199.167429429727)) ;
#79349 = CARTESIAN_POINT('Ctrl Pts',(131.62320958988,-77.3956508170102,-199.313879908351)) ;
#79350 = CARTESIAN_POINT('Ctrl Pts',(131.827186768078,-77.3783728346266,-199.431831999971)) ;
#79351 = CARTESIAN_POINT('Ctrl Pts',(132.170655099965,-77.3463161635726,-199.735124169881)) ;
#79352 = CARTESIAN_POINT('Ctrl Pts',(132.309018835436,-77.3307032671394,-199.915037539806)) ;
#79353 = CARTESIAN_POINT('Ctrl Pts',(132.513895580475,-77.2969027664325,-200.324788921932)) ;
#79354 = CARTESIAN_POINT('Ctrl Pts',(132.575527443354,-77.2796230028992,-200.552120766877)) ;
#79355 = CARTESIAN_POINT('Ctrl Pts',(132.605622241063,-77.2475334590931,-201.009232193585)) ;
#79356 = CARTESIAN_POINT('Ctrl Pts',(132.577083364891,-77.2319623982045,-201.234368161112)) ;
#79357 = CARTESIAN_POINT('Ctrl Pts',(132.433881243309,-77.1981797398566,-201.669404915484)) ;
#79358 = CARTESIAN_POINT('Ctrl Pts',(132.317540721715,-77.1808983460219,-201.874099548761)) ;
#79359 = CARTESIAN_POINT('Ctrl Pts',(132.017012961559,-77.1487744466078,-202.219696711894)) ;
#79360 = CARTESIAN_POINT('Ctrl Pts',(131.838203763758,-77.1332459297227,-202.359397169411)) ;
#79361 = CARTESIAN_POINT('Ctrl Pts',(131.430249263693,-77.0994822634179,-202.567310685746)) ;
#79362 = CARTESIAN_POINT('Ctrl Pts',(131.203588819781,-77.0821994266498,-202.630672025349)) ;
#79363 = CARTESIAN_POINT('Ctrl Pts',(130.928130107247,-77.0627993718329,-202.651021002246)) ;
#79364 = CARTESIAN_POINT('Ctrl Pts',(130.885062091297,-77.0598113822456,-202.652605310181)) ;
#79365 = CARTESIAN_POINT('Ctrl Pts',(130.842036869423,-77.0568711627547,-202.652605310181)) ;
#79366 = CARTESIAN_POINT('Ctrl Pts',(130.842036869423,-77.1560899127545,-202.652605310181)) ;
#79367 = CARTESIAN_POINT('Ctrl Pts',(130.899863916809,-77.1600416462823,-202.652605310181)) ;
#79368 = CARTESIAN_POINT('Ctrl Pts',(130.957751472884,-77.1640785216738,-202.649743499313)) ;
#79369 = CARTESIAN_POINT('Ctrl Pts',(131.24683297456,-77.1846473603666,-202.620992047951)) ;
#79370 = CARTESIAN_POINT('Ctrl Pts',(131.471277230816,-77.2019329520754,-202.552183031522)) ;
#79371 = CARTESIAN_POINT('Ctrl Pts',(131.873460958087,-77.2355736049585,-202.334683455417)) ;
#79372 = CARTESIAN_POINT('Ctrl Pts',(132.048757131248,-77.2508716670637,-202.19072395006)) ;
#79373 = CARTESIAN_POINT('Ctrl Pts',(132.34040870828,-77.2832037156893,-201.838404233993)) ;
#79374 = CARTESIAN_POINT('Ctrl Pts',(132.451572590196,-77.3004896097301,-201.631499513322)) ;
#79375 = CARTESIAN_POINT('Ctrl Pts',(132.584388495721,-77.3341562011185,-201.1938590943)) ;
#79376 = CARTESIAN_POINT('Ctrl Pts',(132.607674330953,-77.3494967795872,-200.968219965905)) ;
#79377 = CARTESIAN_POINT('Ctrl Pts',(132.567039602767,-77.3817868708411,-200.512539643014)) ;
#79378 = CARTESIAN_POINT('Ctrl Pts',(132.500409317965,-77.399072635403,-200.287190397148)) ;
#79379 = CARTESIAN_POINT('Ctrl Pts',(132.28674768475,-77.4327637742788,-199.882678163347)) ;
#79380 = CARTESIAN_POINT('Ctrl Pts',(132.144500759557,-77.4481474585741,-199.705970343403)) ;
#79381 = CARTESIAN_POINT('Ctrl Pts',(131.794872857357,-77.4803969309762,-199.410737405653)) ;
#79382 = CARTESIAN_POINT('Ctrl Pts',(131.588842742789,-77.4976821851599,-199.297484642701)) ;
#79383 = CARTESIAN_POINT('Ctrl Pts',(131.15223619477,-77.5313965183911,-199.160486127959)) ;
#79384 = CARTESIAN_POINT('Ctrl Pts',(130.926800560358,-77.5468236025095,-199.135082754097)) ;
#79385 = CARTESIAN_POINT('Ctrl Pts',(130.470527967021,-77.5790338459698,-199.17146675209)) ;
#79386 = CARTESIAN_POINT('Ctrl Pts',(130.244365397702,-77.5963182578483,-199.236085712784)) ;
#79387 = CARTESIAN_POINT('Ctrl Pts',(129.83772801225,-77.6300544744548,-199.446209282137)) ;
#79388 = CARTESIAN_POINT('Ctrl Pts',(129.659724973282,-77.645524979993,-199.5868862514)) ;
#79389 = CARTESIAN_POINT('Ctrl Pts',(129.361223280434,-77.6776974239309,-199.934033007447)) ;
#79390 = CARTESIAN_POINT('Ctrl Pts',(129.246064167252,-77.6949807081504,-200.139244658745)) ;
#79391 = CARTESIAN_POINT('Ctrl Pts',(129.105238669955,-77.7287375427082,-200.57488795491)) ;
#79392 = CARTESIAN_POINT('Ctrl Pts',(129.077900326764,-77.7442512433349,-200.800138432473)) ;
#79393 = CARTESIAN_POINT('Ctrl Pts',(129.110402356064,-77.7763873453171,-201.256934052676)) ;
#79394 = CARTESIAN_POINT('Ctrl Pts',(129.173179088576,-77.7936692603424,-201.4838231606)) ;
#79395 = CARTESIAN_POINT('Ctrl Pts',(129.380065789546,-77.8274454955802,-201.892386906941)) ;
#79396 = CARTESIAN_POINT('Ctrl Pts',(129.519313614305,-77.8430019422771,-202.071569910934)) ;
#79397 = CARTESIAN_POINT('Ctrl Pts',(129.864190902294,-77.8751031773022,-202.37303491588)) ;
#79398 = CARTESIAN_POINT('Ctrl Pts',(130.068643846436,-77.8923835224096,-202.48992187722)) ;
#79399 = CARTESIAN_POINT('Ctrl Pts',(130.468250156428,-77.923445898564,-202.622558528809)) ;
#79400 = CARTESIAN_POINT('Ctrl Pts',(130.654644951822,-77.9370340899242,-202.652605310181)) ;
#79401 = CARTESIAN_POINT('Ctrl Pts',(130.842036869422,-77.9498399127545,-202.652605310181)) ;
#79402 = CARTESIAN_POINT('Origin',(128.967036869422,-80.3871372990547,-194.819931163313)) ;
#79403 = CARTESIAN_POINT('',(128.842036869421,-80.3871372990547,-205.37875531018)) ;
#79404 = CARTESIAN_POINT('',(128.967036869421,-80.5121372990547,-205.37875531018)) ;
#79405 = CARTESIAN_POINT('Origin',(128.967036869421,-80.3871372990547,-205.37875531018)) ;
#79406 = CARTESIAN_POINT('',(128.967036869421,-80.5121372990547,-204.676255310181)) ;
#79407 = CARTESIAN_POINT('',(128.967036869422,-80.5121372990547,-194.819931163313)) ;
#79408 = CARTESIAN_POINT('',(128.842036869421,-80.3871372990547,-204.676255310181)) ;
#79409 = CARTESIAN_POINT('Origin',(128.967036869421,-80.3871372990547,-204.676255310181)) ;
#79410 = CARTESIAN_POINT('',(128.842036869422,-80.3871372990547,-194.819931163313)) ;
#79411 = CARTESIAN_POINT('Origin',(131.540536869422,-80.5756372990547,-204.676255310181)) ;
#79412 = CARTESIAN_POINT('',(131.540536869422,-80.5121372990547,-204.676255310181)) ;
#79413 = CARTESIAN_POINT('',(131.477036869422,-80.5756372990547,-204.676255310181)) ;
#79414 = CARTESIAN_POINT('Origin',(131.540536869422,-80.5756372990547,-204.676255310181)) ;
#79415 = CARTESIAN_POINT('',(131.540536869422,-80.3871372990547,-204.551255310181)) ;
#79416 = CARTESIAN_POINT('Origin',(131.540536869422,-80.3871372990547,-204.676255310181)) ;
#79417 = CARTESIAN_POINT('',(131.352036869423,-80.5756372990547,-204.551255310181)) ;
#79418 = CARTESIAN_POINT('Origin',(131.540536869422,-80.5756372990547,-204.551255310181)) ;
#79419 = CARTESIAN_POINT('Origin',(131.352036869422,-80.5756372990547,-204.676255310181)) ;
#79420 = CARTESIAN_POINT('Origin',(128.857661869421,-80.3871372990547,-204.676255310181)) ;
#79421 = CARTESIAN_POINT('',(132.717036869422,-80.5121372990547,-204.676255310181)) ;
#79422 = CARTESIAN_POINT('',(132.717036869422,-80.3871372990547,-204.551255310181)) ;
#79423 = CARTESIAN_POINT('Origin',(132.717036869422,-80.3871372990547,-204.676255310181)) ;
#79424 = CARTESIAN_POINT('',(128.857661869421,-80.3871372990547,-204.551255310181)) ;
#79425 = CARTESIAN_POINT('',(128.857661869421,-80.5121372990547,-204.676255310181)) ;
#79426 = CARTESIAN_POINT('Origin',(131.540536869422,-80.5756372990547,-205.378755310181)) ;
#79427 = CARTESIAN_POINT('',(131.477036869422,-80.5756372990547,-205.378755310181)) ;
#79428 = CARTESIAN_POINT('',(131.540536869422,-80.5121372990547,-205.378755310181)) ;
#79429 = CARTESIAN_POINT('Origin',(131.540536869422,-80.5756372990547,-205.378755310181)) ;
#79430 = CARTESIAN_POINT('',(131.352036869422,-80.5756372990547,-205.503755310181)) ;
#79431 = CARTESIAN_POINT('Origin',(131.352036869422,-80.5756372990547,-205.378755310181)) ;
#79432 = CARTESIAN_POINT('',(131.540536869422,-80.3871372990547,-205.503755310181)) ;
#79433 = CARTESIAN_POINT('Origin',(131.540536869422,-80.5756372990547,-205.503755310181)) ;
#79434 = CARTESIAN_POINT('Origin',(131.540536869422,-80.3871372990547,-205.378755310181)) ;
#79435 = CARTESIAN_POINT('Origin',(130.143536869423,-80.5756372990547,-204.676255310181)) ;
#79436 = CARTESIAN_POINT('',(130.207036869423,-80.5756372990547,-204.676255310181)) ;
#79437 = CARTESIAN_POINT('',(130.143536869423,-80.5121372990547,-204.676255310181)) ;
#79438 = CARTESIAN_POINT('Origin',(130.143536869423,-80.5756372990547,-204.676255310181)) ;
#79439 = CARTESIAN_POINT('',(130.332036869423,-80.5756372990547,-204.551255310181)) ;
#79440 = CARTESIAN_POINT('Origin',(130.332036869423,-80.5756372990547,-204.676255310181)) ;
#79441 = CARTESIAN_POINT('',(130.143536869423,-80.3871372990547,-204.551255310181)) ;
#79442 = CARTESIAN_POINT('Origin',(130.143536869423,-80.5756372990547,-204.551255310181)) ;
#79443 = CARTESIAN_POINT('Origin',(130.143536869423,-80.3871372990547,-204.676255310181)) ;
#79444 = CARTESIAN_POINT('Origin',(130.332036869423,-78.8018322834461,-204.676255310181)) ;
#79445 = CARTESIAN_POINT('',(130.207036869423,-84.5845282330442,-204.676255310181)) ;
#79446 = CARTESIAN_POINT('',(130.332036869423,-84.5845282330442,-204.551255310181)) ;
#79447 = CARTESIAN_POINT('Origin',(130.332036869423,-84.5845282330442,-204.676255310181)) ;
#79448 = CARTESIAN_POINT('',(130.332036869423,-78.8018322834461,-204.551255310181)) ;
#79449 = CARTESIAN_POINT('',(130.207036869423,-78.8018322834461,-204.676255310181)) ;
#79450 = CARTESIAN_POINT('Origin',(130.842036869423,-84.5845282330442,-204.676255310181)) ;
#79451 = CARTESIAN_POINT('',(131.477036869423,-84.5845282330442,-204.676255310181)) ;
#79452 = CARTESIAN_POINT('',(131.352036869423,-84.5845282330442,-204.551255310181)) ;
#79453 = CARTESIAN_POINT('Origin',(131.352036869423,-84.5845282330442,-204.676255310181)) ;
#79454 = CARTESIAN_POINT('Origin',(130.842036869423,-84.5845282330442,-204.551255310181)) ;
#79455 = CARTESIAN_POINT('Origin',(130.842036869423,-84.5845282330442,-204.676255310181)) ;
#79456 = CARTESIAN_POINT('Origin',(131.352036869422,-81.0243322834461,-204.676255310181)) ;
#79457 = CARTESIAN_POINT('',(131.352036869423,-81.0243322834461,-204.551255310181)) ;
#79458 = CARTESIAN_POINT('',(131.477036869422,-81.0243322834461,-204.676255310181)) ;
#79459 = CARTESIAN_POINT('Origin',(128.857661869421,-80.3871372990547,-204.676255310181)) ;
#79460 = CARTESIAN_POINT('',(128.967036869421,-80.3871372990547,-204.551255310181)) ;
#79461 = CARTESIAN_POINT('Origin',(128.967036869421,-80.3871372990547,-204.676255310181)) ;
#79462 = CARTESIAN_POINT('',(128.857661869421,-80.5121372990547,-204.676255310181)) ;
#79463 = CARTESIAN_POINT('',(128.857661869421,-80.3871372990547,-204.551255310181)) ;
#79464 = CARTESIAN_POINT('Origin',(130.143536869422,-80.5756372990547,-205.37875531018)) ;
#79465 = CARTESIAN_POINT('',(130.143536869422,-80.5121372990547,-205.37875531018)) ;
#79466 = CARTESIAN_POINT('',(130.207036869422,-80.5756372990547,-205.37875531018)) ;
#79467 = CARTESIAN_POINT('Origin',(130.143536869422,-80.5756372990547,-205.37875531018)) ;
#79468 = CARTESIAN_POINT('',(130.143536869422,-80.3871372990547,-205.50375531018)) ;
#79469 = CARTESIAN_POINT('Origin',(130.143536869422,-80.3871372990547,-205.37875531018)) ;
#79470 = CARTESIAN_POINT('',(130.332036869422,-80.5756372990547,-205.50375531018)) ;
#79471 = CARTESIAN_POINT('Origin',(130.143536869422,-80.5756372990547,-205.50375531018)) ;
#79472 = CARTESIAN_POINT('Origin',(130.332036869422,-80.5756372990547,-205.37875531018)) ;
#79473 = CARTESIAN_POINT('Origin',(128.857661869421,-80.3871372990547,-205.37875531018)) ;
#79474 = CARTESIAN_POINT('',(128.967036869421,-80.3871372990547,-205.50375531018)) ;
#79475 = CARTESIAN_POINT('Origin',(128.967036869421,-80.3871372990547,-205.37875531018)) ;
#79476 = CARTESIAN_POINT('',(128.857661869421,-80.3871372990547,-205.50375531018)) ;
#79477 = CARTESIAN_POINT('',(128.857661869421,-80.5121372990547,-205.37875531018)) ;
#79478 = CARTESIAN_POINT('Origin',(131.352036869422,-85.691582283446,-205.378755310181)) ;
#79479 = CARTESIAN_POINT('',(131.477036869422,-84.5845282330442,-205.378755310181)) ;
#79480 = CARTESIAN_POINT('',(131.352036869422,-84.5845282330442,-205.503755310181)) ;
#79481 = CARTESIAN_POINT('Origin',(131.352036869422,-84.5845282330442,-205.378755310181)) ;
#79482 = CARTESIAN_POINT('',(131.352036869422,-85.691582283446,-205.503755310181)) ;
#79483 = CARTESIAN_POINT('',(131.477036869422,-85.691582283446,-205.378755310181)) ;
#79484 = CARTESIAN_POINT('Origin',(130.842036869423,-84.5845282330442,-205.37875531018)) ;
#79485 = CARTESIAN_POINT('',(130.207036869422,-84.5845282330442,-205.37875531018)) ;
#79486 = CARTESIAN_POINT('',(130.332036869423,-84.5845282330442,-205.50375531018)) ;
#79487 = CARTESIAN_POINT('Origin',(130.332036869423,-84.5845282330442,-205.37875531018)) ;
#79488 = CARTESIAN_POINT('Origin',(130.842036869423,-84.5845282330442,-205.50375531018)) ;
#79489 = CARTESIAN_POINT('Origin',(130.842036869423,-84.5845282330442,-205.37875531018)) ;
#79490 = CARTESIAN_POINT('Origin',(130.332036869422,-83.469082283446,-205.37875531018)) ;
#79491 = CARTESIAN_POINT('',(130.332036869422,-83.469082283446,-205.50375531018)) ;
#79492 = CARTESIAN_POINT('',(130.207036869422,-83.469082283446,-205.37875531018)) ;
#79493 = CARTESIAN_POINT('Origin',(130.143536869425,-80.5756372990547,-187.914255310181)) ;
#79494 = CARTESIAN_POINT('',(130.207036869425,-80.5756372990547,-187.914255310181)) ;
#79495 = CARTESIAN_POINT('',(130.143536869425,-80.5121372990547,-187.914255310181)) ;
#79496 = CARTESIAN_POINT('Origin',(128.857661869421,-80.3871372990547,-205.37875531018)) ;
#79497 = CARTESIAN_POINT('',(132.717036869421,-80.3871372990547,-205.503755310181)) ;
#79498 = CARTESIAN_POINT('',(132.717036869421,-80.5121372990547,-205.378755310181)) ;
#79499 = CARTESIAN_POINT('Origin',(132.717036869421,-80.3871372990547,-205.378755310181)) ;
#79500 = CARTESIAN_POINT('',(128.857661869421,-80.5121372990547,-205.37875531018)) ;
#79501 = CARTESIAN_POINT('',(128.857661869421,-80.3871372990547,-205.50375531018)) ;
#79502 = CARTESIAN_POINT('Origin',(131.540536869425,-80.5756372990547,-188.739755310182)) ;
#79503 = CARTESIAN_POINT('',(131.477036869425,-80.5756372990547,-188.739755310182)) ;
#79504 = CARTESIAN_POINT('',(131.540536869425,-80.5121372990547,-188.739755310182)) ;
#79505 = CARTESIAN_POINT('Origin',(128.967036869421,-80.3871372990547,-205.37875531018)) ;
#79506 = CARTESIAN_POINT('Origin',(128.967036869421,-80.3871372990547,-205.37875531018)) ;
#79507 = CARTESIAN_POINT('Origin',(128.967036869421,-80.3871372990547,-204.676255310181)) ;
#79508 = CARTESIAN_POINT('Origin',(128.967036869421,-80.3871372990547,-204.676255310181)) ;
#79509 = CARTESIAN_POINT('Origin',(132.717036869422,-80.3871372990547,-199.185505310181)) ;
#79510 = CARTESIAN_POINT('',(132.842036869421,-80.3871372990547,-205.378755310181)) ;
#79511 = CARTESIAN_POINT('Origin',(132.717036869421,-80.3871372990547,-205.378755310181)) ;
#79512 = CARTESIAN_POINT('',(132.842036869422,-80.3871372990547,-204.676255310181)) ;
#79513 = CARTESIAN_POINT('',(132.842036869422,-80.3871372990547,-199.185505310181)) ;
#79514 = CARTESIAN_POINT('Origin',(132.717036869422,-80.3871372990547,-204.676255310181)) ;
#79515 = CARTESIAN_POINT('',(132.717036869422,-80.5121372990547,-199.185505310181)) ;
#79516 = CARTESIAN_POINT('Origin',(132.717036869421,-80.3871372990547,-205.378755310181)) ;
#79517 = CARTESIAN_POINT('Origin',(132.717036869421,-80.3871372990547,-205.378755310181)) ;
#79518 = CARTESIAN_POINT('Origin',(132.717036869422,-80.3871372990547,-204.676255310181)) ;
#79519 = CARTESIAN_POINT('Origin',(132.717036869422,-80.3871372990547,-204.676255310181)) ;
#79520 = CARTESIAN_POINT('Origin',(130.207036869425,-82.6795282330441,-187.088755310182)) ;
#79521 = CARTESIAN_POINT('',(130.207036869422,-84.5845282330442,-205.503755310182)) ;
#79522 = CARTESIAN_POINT('Origin',(128.967036869421,-77.019821262485,-204.676255310181)) ;
#79523 = CARTESIAN_POINT('',(128.967036869421,-76.2556363338479,-204.551255310181)) ;
#79524 = CARTESIAN_POINT('',(128.967036869421,-77.019821262485,-204.551255310181)) ;
#79525 = CARTESIAN_POINT('',(128.842036869421,-76.2556363338479,-204.676255310181)) ;
#79526 = CARTESIAN_POINT('Origin',(128.967036869421,-76.2556363338479,-204.676255310181)) ;
#79527 = CARTESIAN_POINT('',(128.842036869421,-77.019821262485,-204.676255310181)) ;
#79528 = CARTESIAN_POINT('Origin',(126.238286869421,-74.924136333848,-204.55125531018)) ;
#79529 = CARTESIAN_POINT('',(132.717036869422,-76.2556363338479,-204.551255310181)) ;
#79530 = CARTESIAN_POINT('',(132.717036869422,-75.051136333848,-204.551255310181)) ;
#79531 = CARTESIAN_POINT('',(132.651420178853,-76.194136333848,-204.551255310181)) ;
#79532 = CARTESIAN_POINT('Ctrl Pts',(132.717036869422,-76.2556363338479,-204.551255310181)) ;
#79533 = CARTESIAN_POINT('Ctrl Pts',(132.697172914594,-76.2357723790203,-204.551255310181)) ;
#79534 = CARTESIAN_POINT('Ctrl Pts',(132.675045468123,-76.2135667892559,-204.551255310181)) ;
#79535 = CARTESIAN_POINT('Ctrl Pts',(132.651420178853,-76.194136333848,-204.551255310181)) ;
#79536 = CARTESIAN_POINT('',(129.03265355999,-76.194136333848,-204.551255310181)) ;
#79537 = CARTESIAN_POINT('',(126.492286869421,-76.194136333848,-204.55125531018)) ;
#79538 = CARTESIAN_POINT('Ctrl Pts',(129.03265355999,-76.1941363338481,-204.551255310181)) ;
#79539 = CARTESIAN_POINT('Ctrl Pts',(129.009028270719,-76.2135667892559,-204.551255310181)) ;
#79540 = CARTESIAN_POINT('Ctrl Pts',(128.986900824248,-76.2357723790203,-204.551255310181)) ;
#79541 = CARTESIAN_POINT('Ctrl Pts',(128.967036869421,-76.2556363338479,-204.551255310181)) ;
#79542 = CARTESIAN_POINT('Origin',(132.717036869422,-75.051136333848,-204.676255310181)) ;
#79543 = CARTESIAN_POINT('',(132.842036869422,-76.2556363338479,-204.676255310181)) ;
#79544 = CARTESIAN_POINT('',(132.842036869422,-75.051136333848,-204.676255310181)) ;
#79545 = CARTESIAN_POINT('Origin',(132.717036869422,-76.2556363338479,-204.676255310181)) ;
#79546 = CARTESIAN_POINT('Origin',(132.842036869421,-75.178136333848,-209.631255310181)) ;
#79547 = CARTESIAN_POINT('',(132.842036869421,-76.2556363338479,-205.378755310181)) ;
#79548 = CARTESIAN_POINT('',(132.842036869421,-79.7183863338479,-205.378755310181)) ;
#79549 = CARTESIAN_POINT('',(132.842036869421,-76.2556363338479,-205.265630310181)) ;
#79550 = CARTESIAN_POINT('Origin',(131.477036869424,-80.5121372990547,-188.739755310181)) ;
#79551 = CARTESIAN_POINT('Origin',(131.477036869424,-80.5121372990547,-188.739755310181)) ;
#79552 = CARTESIAN_POINT('Origin',(131.477036869425,-87.1245282330441,-188.739755310182)) ;
#79553 = CARTESIAN_POINT('',(131.477036869422,-84.5845282330442,-205.503755310182)) ;
#79554 = CARTESIAN_POINT('Origin',(130.842036869423,-84.5845282330442,-200.106255310182)) ;
#79555 = CARTESIAN_POINT('Origin',(132.717036869421,-79.7183863338479,-205.378755310181)) ;
#79556 = CARTESIAN_POINT('',(132.717036869421,-76.2556363338479,-205.503755310181)) ;
#79557 = CARTESIAN_POINT('',(132.717036869421,-79.7183863338479,-205.503755310181)) ;
#79558 = CARTESIAN_POINT('Origin',(132.717036869421,-76.2556363338479,-205.378755310181)) ;
#79559 = CARTESIAN_POINT('Origin',(128.967036869421,-81.687071262485,-205.37875531018)) ;
#79560 = CARTESIAN_POINT('',(128.842036869421,-76.2556363338479,-205.37875531018)) ;
#79561 = CARTESIAN_POINT('',(128.842036869421,-81.687071262485,-205.37875531018)) ;
#79562 = CARTESIAN_POINT('',(128.967036869421,-76.2556363338479,-205.50375531018)) ;
#79563 = CARTESIAN_POINT('Origin',(128.967036869421,-76.2556363338479,-205.37875531018)) ;
#79564 = CARTESIAN_POINT('',(128.967036869421,-81.687071262485,-205.50375531018)) ;
#79565 = CARTESIAN_POINT('Origin',(126.238286869421,-84.2586363338479,-205.50375531018)) ;
#79566 = CARTESIAN_POINT('',(128.717036869421,-76.0056363338479,-205.50375531018)) ;
#79567 = CARTESIAN_POINT('Origin',(128.717036869421,-76.2556363338479,-205.50375531018)) ;
#79568 = CARTESIAN_POINT('',(126.96703686942,-76.0056363338479,-205.50375531018)) ;
#79569 = CARTESIAN_POINT('',(126.238286869421,-76.0056363338479,-205.50375531018)) ;
#79570 = CARTESIAN_POINT('',(126.96703686942,-75.8766363338479,-205.50375531018)) ;
#79571 = CARTESIAN_POINT('',(126.96703686942,-81.6870712624849,-205.50375531018)) ;
#79572 = CARTESIAN_POINT('',(134.717036869421,-75.8766363338479,-205.503755310181)) ;
#79573 = CARTESIAN_POINT('',(126.492286869421,-75.8766363338479,-205.50375531018)) ;
#79574 = CARTESIAN_POINT('',(134.717036869421,-76.0056363338479,-205.503755310181)) ;
#79575 = CARTESIAN_POINT('',(134.717036869421,-79.7183863338479,-205.503755310181)) ;
#79576 = CARTESIAN_POINT('',(132.967036869421,-76.0056363338479,-205.503755310181)) ;
#79577 = CARTESIAN_POINT('',(126.238286869421,-76.0056363338479,-205.50375531018)) ;
#79578 = CARTESIAN_POINT('Origin',(132.967036869421,-76.2556363338479,-205.503755310181)) ;
#79579 = CARTESIAN_POINT('Origin',(128.842036869421,-79.1155061911221,-200.900107016445)) ;
#79580 = CARTESIAN_POINT('',(128.842036869421,-76.2556363338479,-200.900056163313)) ;
#79581 = CARTESIAN_POINT('Origin',(126.238286869423,-84.2586363338479,-197.24875531018)) ;
#79582 = CARTESIAN_POINT('',(128.967036869422,-80.3871363338479,-197.248755310181)) ;
#79583 = CARTESIAN_POINT('',(132.717036869423,-80.3871363338479,-197.248755310181)) ;
#79584 = CARTESIAN_POINT('',(128.857661869423,-80.3871363338479,-197.248755310181)) ;
#79585 = CARTESIAN_POINT('',(128.967036869422,-76.2556363338479,-197.248755310181)) ;
#79586 = CARTESIAN_POINT('',(128.967036869422,-81.687071262485,-197.248755310181)) ;
#79587 = CARTESIAN_POINT('',(129.032653559991,-76.194136333848,-197.248755310181)) ;
#79588 = CARTESIAN_POINT('Ctrl Pts',(128.967036869422,-76.2556363338479,-197.248755310181)) ;
#79589 = CARTESIAN_POINT('Ctrl Pts',(128.98690082425,-76.2357723790203,-197.248755310181)) ;
#79590 = CARTESIAN_POINT('Ctrl Pts',(129.00902827072,-76.2135667892558,-197.248755310181)) ;
#79591 = CARTESIAN_POINT('Ctrl Pts',(129.032653559991,-76.1941363338479,-197.248755310181)) ;
#79592 = CARTESIAN_POINT('',(132.651420178854,-76.194136333848,-197.248755310181)) ;
#79593 = CARTESIAN_POINT('',(126.492286869423,-76.194136333848,-197.24875531018)) ;
#79594 = CARTESIAN_POINT('',(132.717036869423,-76.2556363338479,-197.248755310181)) ;
#79595 = CARTESIAN_POINT('Ctrl Pts',(132.651420178854,-76.194136333848,-197.248755310181)) ;
#79596 = CARTESIAN_POINT('Ctrl Pts',(132.675045468124,-76.2135667892558,-197.248755310181)) ;
#79597 = CARTESIAN_POINT('Ctrl Pts',(132.697172914595,-76.2357723790203,-197.248755310181)) ;
#79598 = CARTESIAN_POINT('Ctrl Pts',(132.717036869423,-76.2556363338479,-197.248755310181)) ;
#79599 = CARTESIAN_POINT('',(132.717036869423,-79.7183863338479,-197.248755310181)) ;
#79600 = CARTESIAN_POINT('Origin',(131.477036869424,-80.5121363338479,-188.739755310181)) ;
#79601 = CARTESIAN_POINT('',(132.717036869423,-80.5121363338479,-197.123755310181)) ;
#79602 = CARTESIAN_POINT('',(128.967036869422,-80.512136333848,-197.123755310181)) ;
#79603 = CARTESIAN_POINT('',(128.857661869423,-80.512136333848,-197.123755310181)) ;
#79604 = CARTESIAN_POINT('',(132.717036869423,-80.5121363338479,-196.421255310181)) ;
#79605 = CARTESIAN_POINT('',(132.717036869422,-80.512136333848,-199.185505310181)) ;
#79606 = CARTESIAN_POINT('',(128.967036869422,-80.512136333848,-196.42125531018)) ;
#79607 = CARTESIAN_POINT('',(128.857661869422,-80.512136333848,-196.42125531018)) ;
#79608 = CARTESIAN_POINT('',(128.967036869422,-80.512136333848,-194.819931163313)) ;
#79609 = CARTESIAN_POINT('Origin',(126.238286869422,-74.6066363338479,-196.29625531018)) ;
#79610 = CARTESIAN_POINT('',(132.717036869423,-80.3871363338479,-196.296255310181)) ;
#79611 = CARTESIAN_POINT('',(128.967036869422,-80.3871363338479,-196.29625531018)) ;
#79612 = CARTESIAN_POINT('',(128.857661869422,-80.3871363338479,-196.29625531018)) ;
#79613 = CARTESIAN_POINT('',(132.717036869423,-76.2556363338479,-196.296255310181)) ;
#79614 = CARTESIAN_POINT('',(132.717036869423,-74.8923863338479,-196.296255310181)) ;
#79615 = CARTESIAN_POINT('',(132.967036869423,-76.0056363338479,-196.296255310181)) ;
#79616 = CARTESIAN_POINT('Origin',(132.967036869423,-76.2556363338479,-196.296255310181)) ;
#79617 = CARTESIAN_POINT('',(134.717036869422,-76.0056363338479,-196.296255310181)) ;
#79618 = CARTESIAN_POINT('',(126.238286869422,-76.0056363338479,-196.29625531018)) ;
#79619 = CARTESIAN_POINT('',(134.717036869422,-75.8766363338479,-196.296255310181)) ;
#79620 = CARTESIAN_POINT('',(134.717036869422,-74.8923863338479,-196.296255310181)) ;
#79621 = CARTESIAN_POINT('',(126.967036869422,-75.8766363338479,-196.29625531018)) ;
#79622 = CARTESIAN_POINT('',(126.492286869422,-75.8766363338479,-196.29625531018)) ;
#79623 = CARTESIAN_POINT('',(126.967036869422,-76.0056363338479,-196.29625531018)) ;
#79624 = CARTESIAN_POINT('',(126.967036869422,-76.8610712624849,-196.29625531018)) ;
#79625 = CARTESIAN_POINT('',(128.717036869422,-76.0056363338479,-196.29625531018)) ;
#79626 = CARTESIAN_POINT('',(126.238286869422,-76.0056363338479,-196.29625531018)) ;
#79627 = CARTESIAN_POINT('',(128.967036869422,-76.2556363338479,-196.29625531018)) ;
#79628 = CARTESIAN_POINT('Origin',(128.717036869422,-76.2556363338479,-196.29625531018)) ;
#79629 = CARTESIAN_POINT('',(128.967036869422,-76.861071262485,-196.29625531018)) ;
#79630 = CARTESIAN_POINT('Origin',(126.238286869422,-75.1781363338479,-200.90000531018)) ;
#79631 = CARTESIAN_POINT('',(126.967036869421,-75.1781363338479,-196.99475531018)) ;
#79632 = CARTESIAN_POINT('',(126.96703686942,-75.1781363338479,-204.80525531018)) ;
#79633 = CARTESIAN_POINT('',(126.967036869421,-75.1781363338479,-200.900056163312)) ;
#79634 = CARTESIAN_POINT('',(134.717036869422,-75.1781363338479,-196.994755310181)) ;
#79635 = CARTESIAN_POINT('',(126.492286869422,-75.1781363338479,-196.99475531018)) ;
#79636 = CARTESIAN_POINT('',(134.717036869421,-75.1781363338479,-204.805255310181)) ;
#79637 = CARTESIAN_POINT('',(134.717036869421,-75.1781363338479,-205.265630310181)) ;
#79638 = CARTESIAN_POINT('',(126.492286869421,-75.1781363338479,-204.80525531018)) ;
#79639 = CARTESIAN_POINT('Ctrl Pts',(129.538783258279,-75.1781363338479,-199.728196117098)) ;
#79640 = CARTESIAN_POINT('Ctrl Pts',(129.45800656813,-75.1781363338479,-199.843248165079)) ;
#79641 = CARTESIAN_POINT('Ctrl Pts',(129.392083038491,-75.1781363338479,-199.968013747906)) ;
#79642 = CARTESIAN_POINT('Ctrl Pts',(129.295765628632,-75.1781363338479,-200.224210513459)) ;
#79643 = CARTESIAN_POINT('Ctrl Pts',(129.264039116857,-75.1781363336273,-200.353975535856)) ;
#79644 = CARTESIAN_POINT('Ctrl Pts',(129.237141221678,-75.1781363336273,-200.577407440569)) ;
#79645 = CARTESIAN_POINT('Ctrl Pts',(129.233742341553,-75.1781363339454,-200.669408192917)) ;
#79646 = CARTESIAN_POINT('Ctrl Pts',(129.246388555036,-75.1781363339454,-200.944817520171)) ;
#79647 = CARTESIAN_POINT('Ctrl Pts',(129.28319680131,-75.1781363338479,-201.083489158714)) ;
#79648 = CARTESIAN_POINT('Ctrl Pts',(129.349105122886,-75.1781363338479,-201.28766056179)) ;
#79649 = CARTESIAN_POINT('Ctrl Pts',(129.403482219833,-75.1781363338479,-201.403236625849)) ;
#79650 = CARTESIAN_POINT('Ctrl Pts',(129.471900051694,-75.1781363338479,-201.5105174728)) ;
#79651 = CARTESIAN_POINT('Ctrl Pts',(132.182528457453,-75.1781363338479,-200.226891425003)) ;
#79652 = CARTESIAN_POINT('Ctrl Pts',(132.131574767273,-75.1781363338479,-200.071657123996)) ;
#79653 = CARTESIAN_POINT('Ctrl Pts',(132.055096968141,-75.1781363338479,-199.926049956735)) ;
#79654 = CARTESIAN_POINT('Ctrl Pts',(131.886671256346,-75.1781363338479,-199.704076104489)) ;
#79655 = CARTESIAN_POINT('Ctrl Pts',(131.769830068204,-75.1781363338479,-199.569294695449)) ;
#79656 = CARTESIAN_POINT('Ctrl Pts',(131.470525930309,-75.1781363338479,-199.36014270823)) ;
#79657 = CARTESIAN_POINT('Ctrl Pts',(131.341077459766,-75.1781363338479,-199.293181639218)) ;
#79658 = CARTESIAN_POINT('Ctrl Pts',(131.057089712392,-75.1781363338479,-199.191077475863)) ;
#79659 = CARTESIAN_POINT('Ctrl Pts',(130.90605206945,-75.1781363338479,-199.160428444176)) ;
#79660 = CARTESIAN_POINT('Ctrl Pts',(130.749091630179,-75.1781363338479,-199.14987161743)) ;
#79661 = CARTESIAN_POINT('Origin',(126.238286869422,-75.8766363338479,-196.99475531018)) ;
#79662 = CARTESIAN_POINT('Origin',(126.967036869421,-75.8766363338479,-196.99475531018)) ;
#79663 = CARTESIAN_POINT('Origin',(134.717036869422,-75.8766363338479,-196.994755310181)) ;
#79664 = CARTESIAN_POINT('Origin',(126.238286869421,-75.8766363338479,-204.80525531018)) ;
#79665 = CARTESIAN_POINT('Origin',(126.96703686942,-75.8766363338479,-204.80525531018)) ;
#79666 = CARTESIAN_POINT('Origin',(134.717036869421,-75.8766363338479,-204.805255310181)) ;
#79667 = CARTESIAN_POINT('Origin',(126.238286869423,-76.194136333848,-197.31225531018)) ;
#79668 = CARTESIAN_POINT('',(132.552818265117,-76.1306363338479,-197.312255310181)) ;
#79669 = CARTESIAN_POINT('Ctrl Pts',(132.552818265118,-76.1306363338479,-197.312255310181)) ;
#79670 = CARTESIAN_POINT('Ctrl Pts',(132.553235902517,-76.1306363338479,-197.311832627558)) ;
#79671 = CARTESIAN_POINT('Ctrl Pts',(132.553653540005,-76.1306405541772,-197.311409957672)) ;
#79672 = CARTESIAN_POINT('Ctrl Pts',(132.561306890963,-76.1307952165411,-197.303665859274)) ;
#79673 = CARTESIAN_POINT('Ctrl Pts',(132.568504138283,-76.1322072351016,-197.296404775943)) ;
#79674 = CARTESIAN_POINT('Ctrl Pts',(132.582932569029,-76.137491469148,-197.282617198858)) ;
#79675 = CARTESIAN_POINT('Ctrl Pts',(132.590067314198,-76.141343967398,-197.276182188304)) ;
#79676 = CARTESIAN_POINT('Ctrl Pts',(132.60894050488,-76.1543405140709,-197.261267814067)) ;
#79677 = CARTESIAN_POINT('Ctrl Pts',(132.619689006199,-76.1646337439611,-197.254884983358)) ;
#79678 = CARTESIAN_POINT('Ctrl Pts',(132.637807265837,-76.1820606916733,-197.24953905352)) ;
#79679 = CARTESIAN_POINT('Ctrl Pts',(132.644422115438,-76.1883808250967,-197.248755310181)) ;
#79680 = CARTESIAN_POINT('Ctrl Pts',(132.651420178854,-76.194136333848,-197.248755310181)) ;
#79681 = CARTESIAN_POINT('',(129.131255473727,-76.1306363338479,-197.312255310181)) ;
#79682 = CARTESIAN_POINT('Ctrl Pts',(129.032653559991,-76.1941363338485,-197.24875531018)) ;
#79683 = CARTESIAN_POINT('Ctrl Pts',(129.039651623408,-76.1883808250969,-197.24875531018)) ;
#79684 = CARTESIAN_POINT('Ctrl Pts',(129.046266473008,-76.1820606916736,-197.24953905352)) ;
#79685 = CARTESIAN_POINT('Ctrl Pts',(129.064384732645,-76.1646337439627,-197.254884983357)) ;
#79686 = CARTESIAN_POINT('Ctrl Pts',(129.075133233964,-76.1543405140722,-197.261267814065)) ;
#79687 = CARTESIAN_POINT('Ctrl Pts',(129.094006424647,-76.1413439673982,-197.276182188303)) ;
#79688 = CARTESIAN_POINT('Ctrl Pts',(129.101141169816,-76.1374914691481,-197.282617198857)) ;
#79689 = CARTESIAN_POINT('Ctrl Pts',(129.115569600563,-76.1322072351016,-197.296404775943)) ;
#79690 = CARTESIAN_POINT('Ctrl Pts',(129.122766847883,-76.130795216541,-197.303665859274)) ;
#79691 = CARTESIAN_POINT('Ctrl Pts',(129.13042019884,-76.1306405541772,-197.311409957671)) ;
#79692 = CARTESIAN_POINT('Ctrl Pts',(129.130837836329,-76.1306363338479,-197.311832627557)) ;
#79693 = CARTESIAN_POINT('Ctrl Pts',(129.131255473728,-76.1306363338479,-197.31225531018)) ;
#79694 = CARTESIAN_POINT('',(126.238286869423,-76.1306363338479,-197.31225531018)) ;
#79695 = CARTESIAN_POINT('Origin',(126.238286869421,-76.194136333848,-204.48775531018)) ;
#79696 = CARTESIAN_POINT('',(132.552818265116,-76.1306363338479,-204.487755310181)) ;
#79697 = CARTESIAN_POINT('Ctrl Pts',(132.651420178853,-76.1941363338479,-204.551255310181)) ;
#79698 = CARTESIAN_POINT('Ctrl Pts',(132.644422115437,-76.1883808250966,-204.551255310181)) ;
#79699 = CARTESIAN_POINT('Ctrl Pts',(132.637807265836,-76.1820606916732,-204.550471566842)) ;
#79700 = CARTESIAN_POINT('Ctrl Pts',(132.619689006197,-76.1646337439608,-204.545125637004)) ;
#79701 = CARTESIAN_POINT('Ctrl Pts',(132.608940504879,-76.1543405140707,-204.538742806295)) ;
#79702 = CARTESIAN_POINT('Ctrl Pts',(132.590067314197,-76.1413439673978,-204.523828432057)) ;
#79703 = CARTESIAN_POINT('Ctrl Pts',(132.582932569028,-76.1374914691479,-204.517393421504)) ;
#79704 = CARTESIAN_POINT('Ctrl Pts',(132.568504138281,-76.1322072351013,-204.503605844418)) ;
#79705 = CARTESIAN_POINT('Ctrl Pts',(132.561306890966,-76.1307952165411,-204.496344761088)) ;
#79706 = CARTESIAN_POINT('Ctrl Pts',(132.553653540003,-76.1306405541772,-204.48860066269)) ;
#79707 = CARTESIAN_POINT('Ctrl Pts',(132.553235902516,-76.1306363338479,-204.488177992805)) ;
#79708 = CARTESIAN_POINT('Ctrl Pts',(132.552818265117,-76.1306363338479,-204.487755310181)) ;
#79709 = CARTESIAN_POINT('',(129.131255473726,-76.1306363338479,-204.487755310181)) ;
#79710 = CARTESIAN_POINT('',(126.238286869421,-76.1306363338479,-204.48775531018)) ;
#79711 = CARTESIAN_POINT('Ctrl Pts',(129.131255473726,-76.1306363338479,-204.487755310181)) ;
#79712 = CARTESIAN_POINT('Ctrl Pts',(129.130837836326,-76.1306363338479,-204.488177992804)) ;
#79713 = CARTESIAN_POINT('Ctrl Pts',(129.130420198838,-76.1306405541772,-204.48860066269)) ;
#79714 = CARTESIAN_POINT('Ctrl Pts',(129.122766847881,-76.1307952165411,-204.496344761087)) ;
#79715 = CARTESIAN_POINT('Ctrl Pts',(129.115569600561,-76.1322072351016,-204.503605844418)) ;
#79716 = CARTESIAN_POINT('Ctrl Pts',(129.101141169815,-76.1374914691477,-204.517393421503)) ;
#79717 = CARTESIAN_POINT('Ctrl Pts',(129.094006424646,-76.1413439673975,-204.523828432056)) ;
#79718 = CARTESIAN_POINT('Ctrl Pts',(129.075133233963,-76.1543405140709,-204.538742806295)) ;
#79719 = CARTESIAN_POINT('Ctrl Pts',(129.064384732644,-76.1646337439613,-204.545125637003)) ;
#79720 = CARTESIAN_POINT('Ctrl Pts',(129.046266473007,-76.1820606916719,-204.550471566841)) ;
#79721 = CARTESIAN_POINT('Ctrl Pts',(129.039651623407,-76.1883808250955,-204.55125531018)) ;
#79722 = CARTESIAN_POINT('Ctrl Pts',(129.03265355999,-76.1941363338474,-204.55125531018)) ;
#79723 = CARTESIAN_POINT('Origin',(132.842036869421,-75.178136333848,-209.631255310181)) ;
#79724 = CARTESIAN_POINT('',(132.842036869423,-80.3871363338479,-197.123755310181)) ;
#79725 = CARTESIAN_POINT('',(132.842036869423,-80.3871363338479,-196.421255310181)) ;
#79726 = CARTESIAN_POINT('',(132.842036869422,-80.3871363338479,-199.185505310181)) ;
#79727 = CARTESIAN_POINT('',(132.842036869423,-76.2556363338479,-197.123755310181)) ;
#79728 = CARTESIAN_POINT('',(132.842036869423,-79.7183863338479,-197.123755310181)) ;
#79729 = CARTESIAN_POINT('',(132.842036869423,-76.2556363338479,-196.421255310181)) ;
#79730 = CARTESIAN_POINT('',(132.842036869421,-76.2556363338479,-205.265630310181)) ;
#79731 = CARTESIAN_POINT('',(132.842036869423,-74.8923863338479,-196.421255310181)) ;
#79732 = CARTESIAN_POINT('Origin',(132.717036869423,-79.7183863338479,-197.123755310181)) ;
#79733 = CARTESIAN_POINT('Origin',(132.717036869423,-80.3871363338479,-197.123755310181)) ;
#79734 = CARTESIAN_POINT('Origin',(132.717036869423,-76.2556363338479,-197.123755310181)) ;
#79735 = CARTESIAN_POINT('Origin',(134.84203686942,-75.1781363338479,-209.631255310181)) ;
#79736 = CARTESIAN_POINT('',(134.842036869421,-76.0056363338479,-205.378755310181)) ;
#79737 = CARTESIAN_POINT('',(134.842036869422,-76.0056363338479,-196.421255310181)) ;
#79738 = CARTESIAN_POINT('',(134.842036869421,-76.0056363338479,-205.265630310181)) ;
#79739 = CARTESIAN_POINT('',(134.842036869421,-75.8766363338479,-205.378755310181)) ;
#79740 = CARTESIAN_POINT('',(134.842036869421,-79.7183863338479,-205.378755310181)) ;
#79741 = CARTESIAN_POINT('',(134.842036869421,-75.3031363338479,-204.805255310181)) ;
#79742 = CARTESIAN_POINT('Origin',(134.842036869421,-75.8766363338479,-204.805255310181)) ;
#79743 = CARTESIAN_POINT('',(134.842036869422,-75.3031363338479,-196.994755310181)) ;
#79744 = CARTESIAN_POINT('',(134.842036869421,-75.3031363338479,-205.265630310181)) ;
#79745 = CARTESIAN_POINT('',(134.842036869422,-75.8766363338479,-196.421255310181)) ;
#79746 = CARTESIAN_POINT('Origin',(134.842036869422,-75.8766363338479,-196.994755310181)) ;
#79747 = CARTESIAN_POINT('',(134.842036869422,-74.8923863338479,-196.421255310181)) ;
#79748 = CARTESIAN_POINT('Origin',(126.842036869421,-79.115506191122,-200.900107016444)) ;
#79749 = CARTESIAN_POINT('',(126.842036869422,-75.8766363338479,-196.42125531018)) ;
#79750 = CARTESIAN_POINT('',(126.842036869422,-76.0056363338479,-196.42125531018)) ;
#79751 = CARTESIAN_POINT('',(126.842036869422,-76.8610712624849,-196.42125531018)) ;
#79752 = CARTESIAN_POINT('',(126.842036869421,-75.3031363338479,-196.99475531018)) ;
#79753 = CARTESIAN_POINT('Origin',(126.842036869421,-75.8766363338479,-196.99475531018)) ;
#79754 = CARTESIAN_POINT('',(126.84203686942,-75.3031363338479,-204.80525531018)) ;
#79755 = CARTESIAN_POINT('',(126.842036869421,-75.3031363338479,-200.900056163312)) ;
#79756 = CARTESIAN_POINT('',(126.84203686942,-75.8766363338479,-205.37875531018)) ;
#79757 = CARTESIAN_POINT('Origin',(126.84203686942,-75.8766363338479,-204.80525531018)) ;
#79758 = CARTESIAN_POINT('',(126.84203686942,-76.0056363338479,-205.37875531018)) ;
#79759 = CARTESIAN_POINT('',(126.84203686942,-81.6870712624849,-205.37875531018)) ;
#79760 = CARTESIAN_POINT('',(126.842036869421,-76.0056363338479,-200.900056163312)) ;
#79761 = CARTESIAN_POINT('Origin',(128.967036869422,-81.687071262485,-197.123755310181)) ;
#79762 = CARTESIAN_POINT('',(128.842036869422,-80.3871363338479,-197.123755310181)) ;
#79763 = CARTESIAN_POINT('Origin',(128.967036869422,-80.3871363338479,-197.123755310181)) ;
#79764 = CARTESIAN_POINT('',(128.842036869422,-76.2556363338479,-197.123755310181)) ;
#79765 = CARTESIAN_POINT('',(128.842036869422,-81.687071262485,-197.123755310181)) ;
#79766 = CARTESIAN_POINT('Origin',(128.967036869422,-76.2556363338479,-197.123755310181)) ;
#79767 = CARTESIAN_POINT('Origin',(128.842036869421,-79.1155061911221,-200.900107016445)) ;
#79768 = CARTESIAN_POINT('',(128.842036869422,-80.3871363338479,-196.42125531018)) ;
#79769 = CARTESIAN_POINT('',(128.842036869422,-80.3871363338479,-194.819931163313)) ;
#79770 = CARTESIAN_POINT('',(128.842036869422,-76.2556363338479,-196.42125531018)) ;
#79771 = CARTESIAN_POINT('',(128.842036869422,-76.861071262485,-196.42125531018)) ;
#79772 = CARTESIAN_POINT('',(128.842036869421,-76.2556363338479,-200.900056163313)) ;
#79773 = CARTESIAN_POINT('Origin',(132.717036869422,-76.2556363338479,-204.676255310181)) ;
#79774 = CARTESIAN_POINT('',(132.967036869422,-76.1306363338479,-204.676255310181)) ;
#79775 = CARTESIAN_POINT('Origin',(132.967036869422,-76.2556363338479,-204.676255310181)) ;
#79776 = CARTESIAN_POINT('Origin',(132.717036869422,-76.1306363338479,-204.676255310181)) ;
#79777 = CARTESIAN_POINT('Origin',(128.967036869421,-76.2556363338479,-204.676255310181)) ;
#79778 = CARTESIAN_POINT('',(128.717036869421,-76.1306363338479,-204.676255310181)) ;
#79779 = CARTESIAN_POINT('Origin',(128.967036869421,-76.1306363338479,-204.676255310181)) ;
#79780 = CARTESIAN_POINT('Origin',(128.717036869421,-76.2556363338479,-204.676255310181)) ;
#79781 = CARTESIAN_POINT('Origin',(132.717036869423,-76.2556363338479,-197.123755310181)) ;
#79782 = CARTESIAN_POINT('',(132.967036869423,-76.1306363338479,-197.123755310181)) ;
#79783 = CARTESIAN_POINT('Origin',(132.717036869423,-76.1306363338479,-197.123755310181)) ;
#79784 = CARTESIAN_POINT('Origin',(132.967036869423,-76.2556363338479,-197.123755310181)) ;
#79785 = CARTESIAN_POINT('Origin',(128.967036869422,-80.3871363338479,-197.123755310181)) ;
#79786 = CARTESIAN_POINT('Origin',(128.967036869422,-80.3871363338479,-197.123755310181)) ;
#79787 = CARTESIAN_POINT('Origin',(128.967036869422,-80.3871363338479,-197.123755310181)) ;
#79788 = CARTESIAN_POINT('Origin',(128.967036869422,-76.2556363338479,-197.123755310181)) ;
#79789 = CARTESIAN_POINT('',(128.717036869422,-76.1306363338479,-197.123755310181)) ;
#79790 = CARTESIAN_POINT('Origin',(128.717036869422,-76.2556363338479,-197.123755310181)) ;
#79791 = CARTESIAN_POINT('Origin',(128.967036869422,-76.1306363338479,-197.123755310181)) ;
#79792 = CARTESIAN_POINT('Origin',(132.717036869423,-80.3871363338479,-197.123755310181)) ;
#79793 = CARTESIAN_POINT('Origin',(132.717036869423,-80.3871363338479,-197.123755310181)) ;
#79794 = CARTESIAN_POINT('Origin',(132.717036869423,-80.3871363338479,-197.123755310181)) ;
#79795 = CARTESIAN_POINT('Origin',(128.857661869423,-80.3871363338479,-197.123755310181)) ;
#79796 = CARTESIAN_POINT('Origin',(132.967036869421,-76.2556363338479,-205.265630310181)) ;
#79797 = CARTESIAN_POINT('',(132.967036869421,-76.1306363338479,-205.378755310181)) ;
#79798 = CARTESIAN_POINT('Origin',(132.967036869421,-76.2556363338479,-205.378755310181)) ;
#79799 = CARTESIAN_POINT('',(132.967036869421,-76.1306363338479,-205.265630310181)) ;
#79800 = CARTESIAN_POINT('Origin',(128.717036869421,-76.2556363338479,-200.900056163313)) ;
#79801 = CARTESIAN_POINT('',(128.717036869421,-76.1306363338479,-205.37875531018)) ;
#79802 = CARTESIAN_POINT('',(128.717036869421,-76.1306363338479,-200.900056163313)) ;
#79803 = CARTESIAN_POINT('Origin',(128.717036869421,-76.2556363338479,-205.37875531018)) ;
#79804 = CARTESIAN_POINT('Origin',(126.238286869421,-76.0056363338479,-205.37875531018)) ;
#79805 = CARTESIAN_POINT('',(134.717036869421,-76.1306363338479,-205.378755310181)) ;
#79806 = CARTESIAN_POINT('Origin',(134.717036869421,-76.0056363338479,-205.378755310181)) ;
#79807 = CARTESIAN_POINT('',(126.238286869421,-76.1306363338479,-205.37875531018)) ;
#79808 = CARTESIAN_POINT('Origin',(132.967036869421,-76.0056363338479,-205.378755310181)) ;
#79809 = CARTESIAN_POINT('Origin',(126.238286869421,-76.0056363338479,-205.37875531018)) ;
#79810 = CARTESIAN_POINT('Origin',(128.717036869421,-76.0056363338479,-205.37875531018)) ;
#79811 = CARTESIAN_POINT('',(126.96703686942,-76.1306363338479,-205.37875531018)) ;
#79812 = CARTESIAN_POINT('',(126.238286869421,-76.1306363338479,-205.37875531018)) ;
#79813 = CARTESIAN_POINT('Origin',(126.96703686942,-76.0056363338479,-205.37875531018)) ;
#79814 = CARTESIAN_POINT('Origin',(134.717036869422,-74.8923863338479,-196.421255310181)) ;
#79815 = CARTESIAN_POINT('Origin',(134.717036869422,-76.0056363338479,-196.421255310181)) ;
#79816 = CARTESIAN_POINT('Origin',(134.717036869422,-75.8766363338479,-196.421255310181)) ;
#79817 = CARTESIAN_POINT('Origin',(134.717036869422,-75.8766363338479,-196.994755310181)) ;
#79818 = CARTESIAN_POINT('Origin',(134.717036869422,-75.3031363338479,-196.994755310181)) ;
#79819 = CARTESIAN_POINT('Origin',(134.717036869421,-75.3031363338479,-205.265630310181)) ;
#79820 = CARTESIAN_POINT('Origin',(134.717036869421,-75.3031363338479,-204.805255310181)) ;
#79821 = CARTESIAN_POINT('Origin',(134.717036869421,-75.8766363338479,-204.805255310181)) ;
#79822 = CARTESIAN_POINT('Origin',(134.717036869421,-75.8766363338479,-205.378755310181)) ;
#79823 = CARTESIAN_POINT('Origin',(134.717036869421,-79.7183863338479,-205.378755310181)) ;
#79824 = CARTESIAN_POINT('Origin',(134.717036869421,-76.0056363338479,-205.378755310181)) ;
#79825 = CARTESIAN_POINT('Origin',(134.717036869421,-76.0056363338479,-205.265630310181)) ;
#79826 = CARTESIAN_POINT('',(134.717036869422,-76.1306363338479,-196.421255310181)) ;
#79827 = CARTESIAN_POINT('Origin',(134.717036869422,-76.0056363338479,-196.421255310181)) ;
#79828 = CARTESIAN_POINT('',(134.717036869421,-76.1306363338479,-205.265630310181)) ;
#79829 = CARTESIAN_POINT('Origin',(134.717036869421,-76.0056363338479,-205.378755310181)) ;
#79830 = CARTESIAN_POINT('Origin',(126.967036869421,-76.0056363338479,-200.900056163312)) ;
#79831 = CARTESIAN_POINT('Origin',(126.96703686942,-76.0056363338479,-205.37875531018)) ;
#79832 = CARTESIAN_POINT('',(126.967036869422,-76.1306363338479,-196.42125531018)) ;
#79833 = CARTESIAN_POINT('',(126.967036869421,-76.1306363338479,-200.900056163312)) ;
#79834 = CARTESIAN_POINT('Origin',(126.967036869422,-76.0056363338479,-196.42125531018)) ;
#79835 = CARTESIAN_POINT('Origin',(126.96703686942,-81.6870712624849,-205.37875531018)) ;
#79836 = CARTESIAN_POINT('Origin',(126.96703686942,-76.0056363338479,-205.37875531018)) ;
#79837 = CARTESIAN_POINT('Origin',(126.96703686942,-75.8766363338479,-205.37875531018)) ;
#79838 = CARTESIAN_POINT('Origin',(126.96703686942,-75.8766363338479,-204.80525531018)) ;
#79839 = CARTESIAN_POINT('Origin',(126.96703686942,-75.3031363338479,-204.80525531018)) ;
#79840 = CARTESIAN_POINT('Origin',(126.967036869421,-75.3031363338479,-200.900056163312)) ;
#79841 = CARTESIAN_POINT('Origin',(126.967036869421,-75.3031363338479,-196.99475531018)) ;
#79842 = CARTESIAN_POINT('Origin',(126.967036869421,-75.8766363338479,-196.99475531018)) ;
#79843 = CARTESIAN_POINT('Origin',(126.967036869422,-75.8766363338479,-196.42125531018)) ;
#79844 = CARTESIAN_POINT('Origin',(126.967036869422,-76.8610712624849,-196.42125531018)) ;
#79845 = CARTESIAN_POINT('Origin',(126.967036869422,-76.0056363338479,-196.42125531018)) ;
#79846 = CARTESIAN_POINT('Origin',(132.967036869421,-76.2556363338479,-205.265630310181)) ;
#79847 = CARTESIAN_POINT('',(132.967036869423,-76.1306363338479,-196.421255310181)) ;
#79848 = CARTESIAN_POINT('',(132.967036869421,-76.1306363338479,-205.265630310181)) ;
#79849 = CARTESIAN_POINT('Origin',(132.967036869423,-76.2556363338479,-196.421255310181)) ;
#79850 = CARTESIAN_POINT('Origin',(132.717036869423,-74.8923863338479,-196.421255310181)) ;
#79851 = CARTESIAN_POINT('Origin',(132.717036869423,-80.3871363338479,-196.421255310181)) ;
#79852 = CARTESIAN_POINT('Origin',(132.717036869423,-76.2556363338479,-196.421255310181)) ;
#79853 = CARTESIAN_POINT('Origin',(132.717036869422,-80.3871363338479,-199.185505310181)) ;
#79854 = CARTESIAN_POINT('Origin',(132.717036869423,-80.3871363338479,-196.421255310181)) ;
#79855 = CARTESIAN_POINT('Origin',(128.967036869422,-80.3871363338479,-194.819931163313)) ;
#79856 = CARTESIAN_POINT('Origin',(128.967036869422,-80.3871363338479,-196.42125531018)) ;
#79857 = CARTESIAN_POINT('Origin',(128.967036869422,-76.861071262485,-196.42125531018)) ;
#79858 = CARTESIAN_POINT('Origin',(128.967036869422,-76.2556363338479,-196.42125531018)) ;
#79859 = CARTESIAN_POINT('Origin',(128.967036869422,-80.3871363338479,-196.42125531018)) ;
#79860 = CARTESIAN_POINT('Origin',(128.857661869422,-80.3871363338479,-196.42125531018)) ;
#79861 = CARTESIAN_POINT('Origin',(132.717036869423,-80.3871363338479,-196.421255310181)) ;
#79862 = CARTESIAN_POINT('Origin',(128.967036869422,-80.3871363338479,-196.42125531018)) ;
#79863 = CARTESIAN_POINT('Origin',(128.967036869422,-80.3871363338479,-196.42125531018)) ;
#79864 = CARTESIAN_POINT('Origin',(132.717036869423,-80.3871363338479,-196.421255310181)) ;
#79865 = CARTESIAN_POINT('Origin',(128.717036869421,-76.2556363338479,-200.900056163313)) ;
#79866 = CARTESIAN_POINT('',(128.717036869422,-76.1306363338479,-196.42125531018)) ;
#79867 = CARTESIAN_POINT('Origin',(128.717036869422,-76.2556363338479,-196.42125531018)) ;
#79868 = CARTESIAN_POINT('',(128.717036869421,-76.1306363338479,-200.900056163313)) ;
#79869 = CARTESIAN_POINT('Origin',(126.238286869422,-76.0056363338479,-196.42125531018)) ;
#79870 = CARTESIAN_POINT('Origin',(126.967036869422,-76.0056363338479,-196.42125531018)) ;
#79871 = CARTESIAN_POINT('',(126.238286869422,-76.1306363338479,-196.42125531018)) ;
#79872 = CARTESIAN_POINT('Origin',(128.717036869422,-76.0056363338479,-196.42125531018)) ;
#79873 = CARTESIAN_POINT('Origin',(128.717036869422,-76.2556363338479,-196.42125531018)) ;
#79874 = CARTESIAN_POINT('Origin',(126.238286869422,-76.0056363338479,-196.42125531018)) ;
#79875 = CARTESIAN_POINT('Origin',(132.967036869423,-76.0056363338479,-196.421255310181)) ;
#79876 = CARTESIAN_POINT('',(126.238286869422,-76.1306363338479,-196.42125531018)) ;
#79877 = CARTESIAN_POINT('Origin',(134.717036869422,-76.0056363338479,-196.421255310181)) ;
#79878 = CARTESIAN_POINT('Origin',(132.967036869423,-76.2556363338479,-196.421255310181)) ;
#79879 = CARTESIAN_POINT('Origin',(126.967036869422,-76.0056363338479,-196.42125531018)) ;
#79880 = CARTESIAN_POINT('Origin',(134.717036869422,-76.0056363338479,-196.421255310181)) ;
#79881 = CARTESIAN_POINT('Origin',(126.96703686942,-76.0056363338479,-205.37875531018)) ;
#79882 = CARTESIAN_POINT('Origin',(134.717036869421,-76.0056363338479,-205.378755310181)) ;
#79883 = CARTESIAN_POINT('Origin',(128.717036869421,-76.2556363338479,-205.37875531018)) ;
#79884 = CARTESIAN_POINT('Origin',(132.967036869421,-76.2556363338479,-205.378755310181)) ;
#79885 = CARTESIAN_POINT('Origin',(130.842036869422,-78.037636333848,-200.900005310181)) ;
#79886 = CARTESIAN_POINT('',(130.842036869423,-78.162636333848,-198.167505310181)) ;
#79887 = CARTESIAN_POINT('Origin',(130.842036869422,-78.162636333848,-200.900005310181)) ;
#79888 = CARTESIAN_POINT('',(130.842036869423,-78.037636333848,-198.042505310181)) ;
#79889 = CARTESIAN_POINT('Origin',(130.842036869422,-78.037636333848,-198.167505310181)) ;
#79890 = CARTESIAN_POINT('Origin',(130.842036869422,-78.037636333848,-200.900005310181)) ;
#79891 = CARTESIAN_POINT('Origin',(126.238286869422,-76.1306363338479,-200.90000531018)) ;
#79892 = CARTESIAN_POINT('',(130.842036869422,-76.1306363338479,-203.882505310181)) ;
#79893 = CARTESIAN_POINT('Origin',(130.842036869422,-76.1306363338479,-200.900005310181)) ;
#79894 = CARTESIAN_POINT('Origin',(130.842036869422,-76.130636333848,-200.900005310181)) ;
#79895 = CARTESIAN_POINT('',(130.842036869422,-76.2556363338479,-203.757505310181)) ;
#79896 = CARTESIAN_POINT('',(130.842036869422,-76.2556363338479,-198.042505310181)) ;
#79897 = CARTESIAN_POINT('Origin',(130.842036869422,-76.2556363338479,-200.900005310181)) ;
#79898 = CARTESIAN_POINT('Origin',(130.842036869422,-76.2556363338479,-200.900005310181)) ;
#79899 = CARTESIAN_POINT('',(130.842036869422,-76.130636333848,-198.042505310181)) ;
#79900 = CARTESIAN_POINT('Origin',(130.842036869422,-76.2556363338479,-200.900005310181)) ;
#79901 = CARTESIAN_POINT('Origin',(130.842036869422,-76.2556363338479,-203.882505310181)) ;
#79902 = CARTESIAN_POINT('Origin',(134.413911869422,-78.162636333848,-204.471880310181)) ;
#79903 = CARTESIAN_POINT('Ctrl Pts',(130.148682626495,-78.162636333848,-199.569870018636)) ;
#79904 = CARTESIAN_POINT('Ctrl Pts',(130.287989560911,-78.162636333848,-199.468610877589)) ;
#79905 = CARTESIAN_POINT('Ctrl Pts',(130.443609984945,-78.162636333848,-199.392079607406)) ;
#79906 = CARTESIAN_POINT('Ctrl Pts',(130.818610624952,-78.162636333848,-199.281692556162)) ;
#79907 = CARTESIAN_POINT('Ctrl Pts',(131.013241952139,-78.162636333848,-199.274293448841)) ;
#79908 = CARTESIAN_POINT('Ctrl Pts',(131.29629180081,-78.162636333848,-199.292439790627)) ;
#79909 = CARTESIAN_POINT('Ctrl Pts',(131.426707517184,-78.162636333848,-199.316460614013)) ;
#79910 = CARTESIAN_POINT('Ctrl Pts',(131.684331081807,-78.162636333848,-199.396206322493)) ;
#79911 = CARTESIAN_POINT('Ctrl Pts',(131.810182908812,-78.162636333848,-199.452859887612)) ;
#79912 = CARTESIAN_POINT('Ctrl Pts',(131.927746211475,-78.162636333848,-199.52419935635)) ;
#79913 = CARTESIAN_POINT('Ctrl Pts',(132.582591006102,-78.162636333848,-200.694875936258)) ;
#79914 = CARTESIAN_POINT('Ctrl Pts',(132.581738268888,-78.162636333848,-200.854045453659)) ;
#79915 = CARTESIAN_POINT('Ctrl Pts',(132.560263297441,-78.162636333848,-201.03274583285)) ;
#79916 = CARTESIAN_POINT('Ctrl Pts',(132.446670912049,-78.162636333848,-201.375601546739)) ;
#79917 = CARTESIAN_POINT('Ctrl Pts',(132.371376067505,-78.1626363339111,-201.523340523348)) ;
#79918 = CARTESIAN_POINT('Ctrl Pts',(132.188297852137,-78.1626363339111,-201.778075291675)) ;
#79919 = CARTESIAN_POINT('Ctrl Pts',(132.085318536322,-78.162636333848,-201.886377279636)) ;
#79920 = CARTESIAN_POINT('Ctrl Pts',(131.895362496131,-78.162636333848,-202.038032714918)) ;
#79921 = CARTESIAN_POINT('Ctrl Pts',(131.770997671067,-78.162636333848,-202.126855902566)) ;
#79922 = CARTESIAN_POINT('Ctrl Pts',(131.596354821607,-78.162636333848,-202.196540858098)) ;
#79923 = CARTESIAN_POINT('Ctrl Pts',(135.341831707641,-78.9434337333926,-200.900005310181)) ;
#79924 = CARTESIAN_POINT('Ctrl Pts',(135.341831707641,-78.8938243583926,-202.763881360068)) ;
#79925 = CARTESIAN_POINT('Ctrl Pts',(134.023872313475,-78.8442149833926,-204.081840754234)) ;
#79926 = CARTESIAN_POINT('Ctrl Pts',(132.705912919309,-78.7946056083926,-205.3998001484)) ;
#79927 = CARTESIAN_POINT('Ctrl Pts',(130.842036869423,-78.7449962333926,-205.3998001484)) ;
#79928 = CARTESIAN_POINT('Ctrl Pts',(128.978160819536,-78.6953868583926,-205.3998001484)) ;
#79929 = CARTESIAN_POINT('Ctrl Pts',(127.66020142537,-78.6457774833926,-204.081840754234)) ;
#79930 = CARTESIAN_POINT('Ctrl Pts',(126.342242031204,-78.5961681083926,-202.763881360068)) ;
#79931 = CARTESIAN_POINT('Ctrl Pts',(126.342242031204,-78.5465587333926,-200.900005310181)) ;
#79932 = CARTESIAN_POINT('Ctrl Pts',(126.342242031204,-78.4969493583926,-199.036129260295)) ;
#79933 = CARTESIAN_POINT('Ctrl Pts',(127.66020142537,-78.4473399833926,-197.718169866129)) ;
#79934 = CARTESIAN_POINT('Ctrl Pts',(128.978160819536,-78.3977306083926,-196.400210471963)) ;
#79935 = CARTESIAN_POINT('Ctrl Pts',(130.842036869422,-78.3481212333926,-196.400210471963)) ;
#79936 = CARTESIAN_POINT('Ctrl Pts',(132.705912919309,-78.2985118583926,-196.400210471962)) ;
#79937 = CARTESIAN_POINT('Ctrl Pts',(134.023872313475,-78.2489024833926,-197.718169866128)) ;
#79938 = CARTESIAN_POINT('Ctrl Pts',(135.341831707641,-78.1992931083926,-199.036129260294)) ;
#79939 = CARTESIAN_POINT('Ctrl Pts',(135.341831707641,-78.1496837333926,-200.900005310181)) ;
#79940 = CARTESIAN_POINT('Ctrl Pts',(135.341831707641,-78.1000743583926,-202.763881360068)) ;
#79941 = CARTESIAN_POINT('Ctrl Pts',(134.023872313475,-78.0504649833926,-204.081840754234)) ;
#79942 = CARTESIAN_POINT('Ctrl Pts',(132.705912919309,-78.0008556083926,-205.3998001484)) ;
#79943 = CARTESIAN_POINT('Ctrl Pts',(130.842036869423,-77.9512462333926,-205.3998001484)) ;
#79944 = CARTESIAN_POINT('Ctrl Pts',(128.978160819536,-77.9016368583926,-205.3998001484)) ;
#79945 = CARTESIAN_POINT('Ctrl Pts',(127.66020142537,-77.8520274833926,-204.081840754234)) ;
#79946 = CARTESIAN_POINT('Ctrl Pts',(126.342242031204,-77.8024181083926,-202.763881360068)) ;
#79947 = CARTESIAN_POINT('Ctrl Pts',(126.342242031204,-77.7528087333926,-200.900005310181)) ;
#79948 = CARTESIAN_POINT('Ctrl Pts',(126.342242031204,-77.7031993583927,-199.036129260295)) ;
#79949 = CARTESIAN_POINT('Ctrl Pts',(127.66020142537,-77.6535899833926,-197.718169866129)) ;
#79950 = CARTESIAN_POINT('Ctrl Pts',(128.978160819536,-77.6039806083926,-196.400210471963)) ;
#79951 = CARTESIAN_POINT('Ctrl Pts',(130.842036869422,-77.5543712333926,-196.400210471963)) ;
#79952 = CARTESIAN_POINT('Ctrl Pts',(132.705912919309,-77.5047618583926,-196.400210471962)) ;
#79953 = CARTESIAN_POINT('Ctrl Pts',(134.023872313475,-77.4551524833926,-197.718169866128)) ;
#79954 = CARTESIAN_POINT('Ctrl Pts',(135.341831707641,-77.4055431083926,-199.036129260294)) ;
#79955 = CARTESIAN_POINT('Ctrl Pts',(135.341831707641,-77.3559337333926,-200.900005310181)) ;
#79956 = CARTESIAN_POINT('Ctrl Pts',(135.341831707641,-77.3063243583926,-202.763881360068)) ;
#79957 = CARTESIAN_POINT('Ctrl Pts',(134.023872313475,-77.2567149833926,-204.081840754234)) ;
#79958 = CARTESIAN_POINT('Ctrl Pts',(132.705912919309,-77.2071056083926,-205.3998001484)) ;
#79959 = CARTESIAN_POINT('Ctrl Pts',(130.842036869423,-77.1574962333926,-205.3998001484)) ;
#79960 = CARTESIAN_POINT('Ctrl Pts',(128.978160819536,-77.1078868583926,-205.3998001484)) ;
#79961 = CARTESIAN_POINT('Ctrl Pts',(127.66020142537,-77.0582774833926,-204.081840754234)) ;
#79962 = CARTESIAN_POINT('Ctrl Pts',(126.342242031204,-77.0086681083926,-202.763881360068)) ;
#79963 = CARTESIAN_POINT('Ctrl Pts',(126.342242031204,-76.9590587333926,-200.900005310181)) ;
#79964 = CARTESIAN_POINT('Ctrl Pts',(126.342242031204,-76.9094493583926,-199.036129260295)) ;
#79965 = CARTESIAN_POINT('Ctrl Pts',(127.66020142537,-76.8598399833926,-197.718169866129)) ;
#79966 = CARTESIAN_POINT('Ctrl Pts',(128.978160819536,-76.8102306083926,-196.400210471963)) ;
#79967 = CARTESIAN_POINT('Ctrl Pts',(130.842036869422,-76.7606212333926,-196.400210471963)) ;
#79968 = CARTESIAN_POINT('Ctrl Pts',(132.705912919309,-76.7110118583926,-196.400210471962)) ;
#79969 = CARTESIAN_POINT('Ctrl Pts',(134.023872313475,-76.6614024833926,-197.718169866128)) ;
#79970 = CARTESIAN_POINT('Ctrl Pts',(135.341831707641,-76.6117931083926,-199.036129260294)) ;
#79971 = CARTESIAN_POINT('Ctrl Pts',(135.341831707641,-76.5621837333926,-200.900005310181)) ;
#79972 = CARTESIAN_POINT('Ctrl Pts',(135.341831707641,-76.5125743583926,-202.763881360068)) ;
#79973 = CARTESIAN_POINT('Ctrl Pts',(134.023872313475,-76.4629649833926,-204.081840754234)) ;
#79974 = CARTESIAN_POINT('Ctrl Pts',(132.705912919309,-76.4133556083926,-205.3998001484)) ;
#79975 = CARTESIAN_POINT('Ctrl Pts',(130.842036869423,-76.3637462333926,-205.3998001484)) ;
#79976 = CARTESIAN_POINT('Ctrl Pts',(128.978160819536,-76.3141368583926,-205.3998001484)) ;
#79977 = CARTESIAN_POINT('Ctrl Pts',(127.66020142537,-76.2645274833926,-204.081840754234)) ;
#79978 = CARTESIAN_POINT('Ctrl Pts',(126.342242031204,-76.2149181083926,-202.763881360068)) ;
#79979 = CARTESIAN_POINT('Ctrl Pts',(126.342242031204,-76.1653087333926,-200.900005310181)) ;
#79980 = CARTESIAN_POINT('Ctrl Pts',(126.342242031204,-76.1156993583926,-199.036129260295)) ;
#79981 = CARTESIAN_POINT('Ctrl Pts',(127.66020142537,-76.0660899833926,-197.718169866129)) ;
#79982 = CARTESIAN_POINT('Ctrl Pts',(128.978160819536,-76.0164806083926,-196.400210471963)) ;
#79983 = CARTESIAN_POINT('Ctrl Pts',(130.842036869422,-75.9668712333926,-196.400210471963)) ;
#79984 = CARTESIAN_POINT('Ctrl Pts',(132.705912919309,-75.9172618583926,-196.400210471962)) ;
#79985 = CARTESIAN_POINT('Ctrl Pts',(134.023872313475,-75.8676524833926,-197.718169866128)) ;
#79986 = CARTESIAN_POINT('Ctrl Pts',(135.341831707641,-75.8180431083926,-199.036129260294)) ;
#79987 = CARTESIAN_POINT('Ctrl Pts',(135.341831707641,-75.7684337333926,-200.900005310181)) ;
#79988 = CARTESIAN_POINT('Ctrl Pts',(135.341831707641,-75.7188243583926,-202.763881360068)) ;
#79989 = CARTESIAN_POINT('Ctrl Pts',(134.023872313475,-75.6692149833926,-204.081840754234)) ;
#79990 = CARTESIAN_POINT('Ctrl Pts',(132.705912919309,-75.6196056083926,-205.3998001484)) ;
#79991 = CARTESIAN_POINT('Ctrl Pts',(130.842036869422,-75.5699962333926,-205.3998001484)) ;
#79992 = CARTESIAN_POINT('Ctrl Pts',(128.978160819536,-75.5203868583926,-205.3998001484)) ;
#79993 = CARTESIAN_POINT('Ctrl Pts',(127.66020142537,-75.4707774833926,-204.081840754234)) ;
#79994 = CARTESIAN_POINT('Ctrl Pts',(126.342242031204,-75.4211681083926,-202.763881360068)) ;
#79995 = CARTESIAN_POINT('Ctrl Pts',(126.342242031204,-75.3715587333926,-200.900005310181)) ;
#79996 = CARTESIAN_POINT('Ctrl Pts',(126.342242031204,-75.3219493583926,-199.036129260295)) ;
#79997 = CARTESIAN_POINT('Ctrl Pts',(127.66020142537,-75.2723399833926,-197.718169866129)) ;
#79998 = CARTESIAN_POINT('Ctrl Pts',(128.978160819536,-75.2227306083926,-196.400210471963)) ;
#79999 = CARTESIAN_POINT('Ctrl Pts',(130.842036869422,-75.1731212333926,-196.400210471963)) ;
#80000 = CARTESIAN_POINT('Ctrl Pts',(132.705912919309,-75.1235118583926,-196.400210471962)) ;
#80001 = CARTESIAN_POINT('Ctrl Pts',(134.023872313475,-75.0739024833926,-197.718169866128)) ;
#80002 = CARTESIAN_POINT('Ctrl Pts',(135.341831707641,-75.0242931083926,-199.036129260294)) ;
#80003 = CARTESIAN_POINT('Ctrl Pts',(135.341831707641,-74.9746837333926,-200.900005310181)) ;
#80004 = CARTESIAN_POINT('Ctrl Pts',(135.341831707641,-74.9250743583926,-202.763881360068)) ;
#80005 = CARTESIAN_POINT('Ctrl Pts',(134.023872313475,-74.8754649833926,-204.081840754234)) ;
#80006 = CARTESIAN_POINT('Ctrl Pts',(132.705912919309,-74.8258556083926,-205.3998001484)) ;
#80007 = CARTESIAN_POINT('Ctrl Pts',(130.842036869422,-74.7762462333926,-205.3998001484)) ;
#80008 = CARTESIAN_POINT('Ctrl Pts',(128.978160819536,-74.7266368583926,-205.3998001484)) ;
#80009 = CARTESIAN_POINT('Ctrl Pts',(127.66020142537,-74.6770274833926,-204.081840754234)) ;
#80010 = CARTESIAN_POINT('Ctrl Pts',(126.342242031204,-74.6274181083926,-202.763881360068)) ;
#80011 = CARTESIAN_POINT('Ctrl Pts',(126.342242031204,-74.5778087333926,-200.900005310181)) ;
#80012 = CARTESIAN_POINT('Ctrl Pts',(126.342242031204,-74.5281993583926,-199.036129260295)) ;
#80013 = CARTESIAN_POINT('Ctrl Pts',(127.66020142537,-74.4785899833926,-197.718169866129)) ;
#80014 = CARTESIAN_POINT('Ctrl Pts',(128.978160819536,-74.4289806083926,-196.400210471963)) ;
#80015 = CARTESIAN_POINT('Ctrl Pts',(130.842036869422,-74.3793712333926,-196.400210471963)) ;
#80016 = CARTESIAN_POINT('Ctrl Pts',(132.705912919309,-74.3297618583926,-196.400210471962)) ;
#80017 = CARTESIAN_POINT('Ctrl Pts',(134.023872313475,-74.2801524833926,-197.718169866128)) ;
#80018 = CARTESIAN_POINT('Ctrl Pts',(135.341831707641,-74.2305431083926,-199.036129260294)) ;
#80019 = CARTESIAN_POINT('Ctrl Pts',(135.341831707641,-74.1809337333926,-200.900005310181)) ;
#80020 = CARTESIAN_POINT('Ctrl Pts',(135.341831707641,-74.1313243583926,-202.763881360068)) ;
#80021 = CARTESIAN_POINT('Ctrl Pts',(134.023872313475,-74.0817149833926,-204.081840754234)) ;
#80022 = CARTESIAN_POINT('Ctrl Pts',(132.705912919309,-74.0321056083926,-205.3998001484)) ;
#80023 = CARTESIAN_POINT('Ctrl Pts',(130.842036869422,-73.9824962333926,-205.3998001484)) ;
#80024 = CARTESIAN_POINT('Ctrl Pts',(128.978160819536,-73.9328868583926,-205.3998001484)) ;
#80025 = CARTESIAN_POINT('Ctrl Pts',(127.66020142537,-73.8832774833926,-204.081840754234)) ;
#80026 = CARTESIAN_POINT('Ctrl Pts',(126.342242031204,-73.8336681083926,-202.763881360068)) ;
#80027 = CARTESIAN_POINT('Ctrl Pts',(126.342242031204,-73.7840587333926,-200.900005310181)) ;
#80028 = CARTESIAN_POINT('Ctrl Pts',(126.342242031204,-73.7344493583927,-199.036129260295)) ;
#80029 = CARTESIAN_POINT('Ctrl Pts',(127.66020142537,-73.6848399833926,-197.718169866129)) ;
#80030 = CARTESIAN_POINT('Ctrl Pts',(128.978160819536,-73.6352306083926,-196.400210471963)) ;
#80031 = CARTESIAN_POINT('Ctrl Pts',(130.842036869422,-73.5856212333926,-196.400210471963)) ;
#80032 = CARTESIAN_POINT('Ctrl Pts',(132.705912919309,-73.5360118583926,-196.400210471962)) ;
#80033 = CARTESIAN_POINT('Ctrl Pts',(134.023872313475,-73.4864024833926,-197.718169866128)) ;
#80034 = CARTESIAN_POINT('Ctrl Pts',(135.341831707641,-73.4367931083926,-199.036129260294)) ;
#80035 = CARTESIAN_POINT('Ctrl Pts',(135.341831707641,-73.3871837333926,-200.900005310181)) ;
#80036 = CARTESIAN_POINT('Ctrl Pts',(135.341831707641,-73.3375743583926,-202.763881360068)) ;
#80037 = CARTESIAN_POINT('Ctrl Pts',(134.023872313475,-73.2879649833926,-204.081840754234)) ;
#80038 = CARTESIAN_POINT('Ctrl Pts',(132.705912919309,-73.2383556083926,-205.3998001484)) ;
#80039 = CARTESIAN_POINT('Ctrl Pts',(130.842036869422,-73.1887462333926,-205.3998001484)) ;
#80040 = CARTESIAN_POINT('Ctrl Pts',(128.978160819536,-73.1391368583926,-205.3998001484)) ;
#80041 = CARTESIAN_POINT('Ctrl Pts',(127.66020142537,-73.0895274833926,-204.081840754234)) ;
#80042 = CARTESIAN_POINT('Ctrl Pts',(126.342242031204,-73.0399181083926,-202.763881360068)) ;
#80043 = CARTESIAN_POINT('Ctrl Pts',(126.342242031204,-72.9903087333926,-200.900005310181)) ;
#80044 = CARTESIAN_POINT('Ctrl Pts',(126.342242031204,-72.9406993583926,-199.036129260295)) ;
#80045 = CARTESIAN_POINT('Ctrl Pts',(127.66020142537,-72.8910899833926,-197.718169866129)) ;
#80046 = CARTESIAN_POINT('Ctrl Pts',(128.978160819536,-72.8414806083926,-196.400210471963)) ;
#80047 = CARTESIAN_POINT('Ctrl Pts',(130.842036869422,-72.7918712333926,-196.400210471963)) ;
#80048 = CARTESIAN_POINT('Ctrl Pts',(132.705912919309,-72.7422618583926,-196.400210471962)) ;
#80049 = CARTESIAN_POINT('Ctrl Pts',(134.023872313475,-72.6926524833926,-197.718169866128)) ;
#80050 = CARTESIAN_POINT('Ctrl Pts',(135.341831707641,-72.6430431083926,-199.036129260294)) ;
#80051 = CARTESIAN_POINT('Ctrl Pts',(135.341831707641,-72.5934337333926,-200.900005310181)) ;
#80052 = CARTESIAN_POINT('Ctrl Pts',(135.341831707641,-72.5438243583926,-202.763881360068)) ;
#80053 = CARTESIAN_POINT('Ctrl Pts',(134.023872313475,-72.4942149833926,-204.081840754234)) ;
#80054 = CARTESIAN_POINT('Ctrl Pts',(132.705912919309,-72.4446056083926,-205.3998001484)) ;
#80055 = CARTESIAN_POINT('Ctrl Pts',(130.842036869422,-72.3949962333926,-205.3998001484)) ;
#80056 = CARTESIAN_POINT('Ctrl Pts',(128.978160819536,-72.3453868583926,-205.3998001484)) ;
#80057 = CARTESIAN_POINT('Ctrl Pts',(127.66020142537,-72.2957774833926,-204.081840754234)) ;
#80058 = CARTESIAN_POINT('Ctrl Pts',(126.342242031204,-72.2461681083926,-202.763881360068)) ;
#80059 = CARTESIAN_POINT('Ctrl Pts',(126.342242031204,-72.1965587333926,-200.900005310181)) ;
#80060 = CARTESIAN_POINT('Ctrl Pts',(126.342242031204,-72.1469493583926,-199.036129260295)) ;
#80061 = CARTESIAN_POINT('Ctrl Pts',(127.66020142537,-72.0973399833926,-197.718169866129)) ;
#80062 = CARTESIAN_POINT('Ctrl Pts',(128.978160819536,-72.0477306083926,-196.400210471963)) ;
#80063 = CARTESIAN_POINT('Ctrl Pts',(130.842036869422,-71.9981212333926,-196.400210471963)) ;
#80064 = CARTESIAN_POINT('Ctrl Pts',(132.705912919309,-71.9485118583926,-196.400210471962)) ;
#80065 = CARTESIAN_POINT('Ctrl Pts',(134.023872313475,-71.8989024833926,-197.718169866128)) ;
#80066 = CARTESIAN_POINT('Ctrl Pts',(135.341831707641,-71.8492931083926,-199.036129260294)) ;
#80067 = CARTESIAN_POINT('Ctrl Pts',(135.341831707641,-71.7996837333926,-200.900005310181)) ;
#80068 = CARTESIAN_POINT('Ctrl Pts',(132.594636869422,-80.5295274127545,-200.900005310181)) ;
#80069 = CARTESIAN_POINT('Ctrl Pts',(132.594636869422,-80.4799180377545,-201.625955999596)) ;
#80070 = CARTESIAN_POINT('Ctrl Pts',(132.08131221413,-80.4303086627545,-202.139280654889)) ;
#80071 = CARTESIAN_POINT('Ctrl Pts',(131.567987558838,-80.3806992877545,-202.652605310181)) ;
#80072 = CARTESIAN_POINT('Ctrl Pts',(130.842036869422,-80.3310899127545,-202.652605310181)) ;
#80073 = CARTESIAN_POINT('Ctrl Pts',(130.116086180007,-80.2814805377545,-202.652605310181)) ;
#80074 = CARTESIAN_POINT('Ctrl Pts',(129.602761524715,-80.2318711627545,-202.139280654889)) ;
#80075 = CARTESIAN_POINT('Ctrl Pts',(129.089436869422,-80.1822617877545,-201.625955999596)) ;
#80076 = CARTESIAN_POINT('Ctrl Pts',(129.089436869422,-80.1326524127545,-200.900005310181)) ;
#80077 = CARTESIAN_POINT('Ctrl Pts',(129.089436869422,-80.0830430377545,-200.174054620766)) ;
#80078 = CARTESIAN_POINT('Ctrl Pts',(129.602761524715,-80.0334336627545,-199.660729965474)) ;
#80079 = CARTESIAN_POINT('Ctrl Pts',(130.116086180007,-79.9838242877545,-199.147405310181)) ;
#80080 = CARTESIAN_POINT('Ctrl Pts',(130.842036869422,-79.9342149127545,-199.147405310181)) ;
#80081 = CARTESIAN_POINT('Ctrl Pts',(131.567987558837,-79.8846055377545,-199.147405310181)) ;
#80082 = CARTESIAN_POINT('Ctrl Pts',(132.08131221413,-79.8349961627545,-199.660729965474)) ;
#80083 = CARTESIAN_POINT('Ctrl Pts',(132.594636869422,-79.7853867877545,-200.174054620766)) ;
#80084 = CARTESIAN_POINT('Ctrl Pts',(132.594636869422,-79.7357774127545,-200.900005310181)) ;
#80085 = CARTESIAN_POINT('Ctrl Pts',(132.594636869422,-79.6861680377545,-201.625955999596)) ;
#80086 = CARTESIAN_POINT('Ctrl Pts',(132.08131221413,-79.6365586627545,-202.139280654889)) ;
#80087 = CARTESIAN_POINT('Ctrl Pts',(131.567987558838,-79.5869492877545,-202.652605310181)) ;
#80088 = CARTESIAN_POINT('Ctrl Pts',(130.842036869422,-79.5373399127545,-202.652605310181)) ;
#80089 = CARTESIAN_POINT('Ctrl Pts',(130.116086180007,-79.4877305377545,-202.652605310181)) ;
#80090 = CARTESIAN_POINT('Ctrl Pts',(129.602761524715,-79.4381211627545,-202.139280654889)) ;
#80091 = CARTESIAN_POINT('Ctrl Pts',(129.089436869422,-79.3885117877545,-201.625955999596)) ;
#80092 = CARTESIAN_POINT('Ctrl Pts',(129.089436869422,-79.3389024127545,-200.900005310181)) ;
#80093 = CARTESIAN_POINT('Ctrl Pts',(129.089436869422,-79.2892930377545,-200.174054620766)) ;
#80094 = CARTESIAN_POINT('Ctrl Pts',(129.602761524715,-79.2396836627545,-199.660729965474)) ;
#80095 = CARTESIAN_POINT('Ctrl Pts',(130.116086180007,-79.1900742877545,-199.147405310181)) ;
#80096 = CARTESIAN_POINT('Ctrl Pts',(130.842036869422,-79.1404649127545,-199.147405310181)) ;
#80097 = CARTESIAN_POINT('Ctrl Pts',(131.567987558837,-79.0908555377545,-199.147405310181)) ;
#80098 = CARTESIAN_POINT('Ctrl Pts',(132.08131221413,-79.0412461627545,-199.660729965474)) ;
#80099 = CARTESIAN_POINT('Ctrl Pts',(132.594636869422,-78.9916367877545,-200.174054620766)) ;
#80100 = CARTESIAN_POINT('Ctrl Pts',(132.594636869422,-78.9420274127545,-200.900005310181)) ;
#80101 = CARTESIAN_POINT('Ctrl Pts',(132.594636869422,-78.8924180377545,-201.625955999596)) ;
#80102 = CARTESIAN_POINT('Ctrl Pts',(132.08131221413,-78.8428086627545,-202.139280654889)) ;
#80103 = CARTESIAN_POINT('Ctrl Pts',(131.567987558838,-78.7931992877545,-202.652605310181)) ;
#80104 = CARTESIAN_POINT('Ctrl Pts',(130.842036869422,-78.7435899127545,-202.652605310181)) ;
#80105 = CARTESIAN_POINT('Ctrl Pts',(130.116086180007,-78.6939805377545,-202.652605310181)) ;
#80106 = CARTESIAN_POINT('Ctrl Pts',(129.602761524715,-78.6443711627545,-202.139280654889)) ;
#80107 = CARTESIAN_POINT('Ctrl Pts',(129.089436869422,-78.5947617877545,-201.625955999596)) ;
#80108 = CARTESIAN_POINT('Ctrl Pts',(129.089436869422,-78.5451524127545,-200.900005310181)) ;
#80109 = CARTESIAN_POINT('Ctrl Pts',(129.089436869422,-78.4955430377545,-200.174054620766)) ;
#80110 = CARTESIAN_POINT('Ctrl Pts',(129.602761524715,-78.4459336627545,-199.660729965474)) ;
#80111 = CARTESIAN_POINT('Ctrl Pts',(130.116086180007,-78.3963242877545,-199.147405310181)) ;
#80112 = CARTESIAN_POINT('Ctrl Pts',(130.842036869422,-78.3467149127545,-199.147405310181)) ;
#80113 = CARTESIAN_POINT('Ctrl Pts',(131.567987558837,-78.2971055377545,-199.147405310181)) ;
#80114 = CARTESIAN_POINT('Ctrl Pts',(132.08131221413,-78.2474961627545,-199.660729965474)) ;
#80115 = CARTESIAN_POINT('Ctrl Pts',(132.594636869422,-78.1978867877545,-200.174054620766)) ;
#80116 = CARTESIAN_POINT('Ctrl Pts',(132.594636869422,-78.1482774127545,-200.900005310181)) ;
#80117 = CARTESIAN_POINT('Ctrl Pts',(132.594636869422,-78.0986680377545,-201.625955999596)) ;
#80118 = CARTESIAN_POINT('Ctrl Pts',(132.08131221413,-78.0490586627545,-202.139280654889)) ;
#80119 = CARTESIAN_POINT('Ctrl Pts',(131.567987558838,-77.9994492877545,-202.652605310181)) ;
#80120 = CARTESIAN_POINT('Ctrl Pts',(130.842036869422,-77.9498399127545,-202.652605310181)) ;
#80121 = CARTESIAN_POINT('Ctrl Pts',(130.116086180007,-77.9002305377545,-202.652605310181)) ;
#80122 = CARTESIAN_POINT('Ctrl Pts',(129.602761524715,-77.8506211627545,-202.139280654889)) ;
#80123 = CARTESIAN_POINT('Ctrl Pts',(129.089436869422,-77.8010117877545,-201.625955999596)) ;
#80124 = CARTESIAN_POINT('Ctrl Pts',(129.089436869422,-77.7514024127545,-200.900005310181)) ;
#80125 = CARTESIAN_POINT('Ctrl Pts',(129.089436869422,-77.7017930377545,-200.174054620766)) ;
#80126 = CARTESIAN_POINT('Ctrl Pts',(129.602761524715,-77.6521836627545,-199.660729965474)) ;
#80127 = CARTESIAN_POINT('Ctrl Pts',(130.116086180007,-77.6025742877545,-199.147405310181)) ;
#80128 = CARTESIAN_POINT('Ctrl Pts',(130.842036869422,-77.5529649127545,-199.147405310181)) ;
#80129 = CARTESIAN_POINT('Ctrl Pts',(131.567987558837,-77.5033555377545,-199.147405310181)) ;
#80130 = CARTESIAN_POINT('Ctrl Pts',(132.08131221413,-77.4537461627545,-199.660729965474)) ;
#80131 = CARTESIAN_POINT('Ctrl Pts',(132.594636869422,-77.4041367877545,-200.174054620766)) ;
#80132 = CARTESIAN_POINT('Ctrl Pts',(132.594636869422,-77.3545274127545,-200.900005310181)) ;
#80133 = CARTESIAN_POINT('Ctrl Pts',(132.594636869422,-77.3049180377545,-201.625955999596)) ;
#80134 = CARTESIAN_POINT('Ctrl Pts',(132.08131221413,-77.2553086627545,-202.139280654889)) ;
#80135 = CARTESIAN_POINT('Ctrl Pts',(131.567987558838,-77.2056992877545,-202.652605310181)) ;
#80136 = CARTESIAN_POINT('Ctrl Pts',(130.842036869422,-77.1560899127545,-202.652605310181)) ;
#80137 = CARTESIAN_POINT('Ctrl Pts',(130.116086180007,-77.1064805377545,-202.652605310181)) ;
#80138 = CARTESIAN_POINT('Ctrl Pts',(129.602761524715,-77.0568711627545,-202.139280654889)) ;
#80139 = CARTESIAN_POINT('Ctrl Pts',(129.089436869422,-77.0072617877545,-201.625955999596)) ;
#80140 = CARTESIAN_POINT('Ctrl Pts',(129.089436869422,-76.9576524127545,-200.900005310181)) ;
#80141 = CARTESIAN_POINT('Ctrl Pts',(129.089436869422,-76.9080430377545,-200.174054620766)) ;
#80142 = CARTESIAN_POINT('Ctrl Pts',(129.602761524715,-76.8584336627545,-199.660729965474)) ;
#80143 = CARTESIAN_POINT('Ctrl Pts',(130.116086180007,-76.8088242877545,-199.147405310181)) ;
#80144 = CARTESIAN_POINT('Ctrl Pts',(130.842036869422,-76.7592149127545,-199.147405310181)) ;
#80145 = CARTESIAN_POINT('Ctrl Pts',(131.567987558837,-76.7096055377545,-199.147405310181)) ;
#80146 = CARTESIAN_POINT('Ctrl Pts',(132.08131221413,-76.6599961627545,-199.660729965474)) ;
#80147 = CARTESIAN_POINT('Ctrl Pts',(132.594636869422,-76.6103867877545,-200.174054620766)) ;
#80148 = CARTESIAN_POINT('Ctrl Pts',(132.594636869422,-76.5607774127545,-200.900005310181)) ;
#80149 = CARTESIAN_POINT('Ctrl Pts',(132.594636869422,-76.5111680377545,-201.625955999596)) ;
#80150 = CARTESIAN_POINT('Ctrl Pts',(132.08131221413,-76.4615586627545,-202.139280654889)) ;
#80151 = CARTESIAN_POINT('Ctrl Pts',(131.567987558838,-76.4119492877545,-202.652605310181)) ;
#80152 = CARTESIAN_POINT('Ctrl Pts',(130.842036869422,-76.3623399127545,-202.652605310181)) ;
#80153 = CARTESIAN_POINT('Ctrl Pts',(130.116086180007,-76.3127305377545,-202.652605310181)) ;
#80154 = CARTESIAN_POINT('Ctrl Pts',(129.602761524715,-76.2631211627545,-202.139280654889)) ;
#80155 = CARTESIAN_POINT('Ctrl Pts',(129.089436869422,-76.2135117877545,-201.625955999596)) ;
#80156 = CARTESIAN_POINT('Ctrl Pts',(129.089436869422,-76.1639024127545,-200.900005310181)) ;
#80157 = CARTESIAN_POINT('Ctrl Pts',(129.089436869422,-76.1142930377545,-200.174054620766)) ;
#80158 = CARTESIAN_POINT('Ctrl Pts',(129.602761524715,-76.0646836627545,-199.660729965474)) ;
#80159 = CARTESIAN_POINT('Ctrl Pts',(130.116086180007,-76.0150742877545,-199.147405310181)) ;
#80160 = CARTESIAN_POINT('Ctrl Pts',(130.842036869422,-75.9654649127545,-199.147405310181)) ;
#80161 = CARTESIAN_POINT('Ctrl Pts',(131.567987558837,-75.9158555377545,-199.147405310181)) ;
#80162 = CARTESIAN_POINT('Ctrl Pts',(132.08131221413,-75.8662461627545,-199.660729965474)) ;
#80163 = CARTESIAN_POINT('Ctrl Pts',(132.594636869422,-75.8166367877545,-200.174054620766)) ;
#80164 = CARTESIAN_POINT('Ctrl Pts',(132.594636869422,-75.7670274127545,-200.900005310181)) ;
#80165 = CARTESIAN_POINT('Ctrl Pts',(132.594636869422,-75.7174180377545,-201.625955999596)) ;
#80166 = CARTESIAN_POINT('Ctrl Pts',(132.08131221413,-75.6678086627545,-202.139280654889)) ;
#80167 = CARTESIAN_POINT('Ctrl Pts',(131.567987558837,-75.6181992877545,-202.652605310181)) ;
#80168 = CARTESIAN_POINT('Ctrl Pts',(130.842036869422,-75.5685899127545,-202.652605310181)) ;
#80169 = CARTESIAN_POINT('Ctrl Pts',(130.116086180007,-75.5189805377545,-202.652605310181)) ;
#80170 = CARTESIAN_POINT('Ctrl Pts',(129.602761524715,-75.4693711627545,-202.139280654889)) ;
#80171 = CARTESIAN_POINT('Ctrl Pts',(129.089436869422,-75.4197617877545,-201.625955999596)) ;
#80172 = CARTESIAN_POINT('Ctrl Pts',(129.089436869422,-75.3701524127545,-200.900005310181)) ;
#80173 = CARTESIAN_POINT('Ctrl Pts',(129.089436869422,-75.3205430377545,-200.174054620766)) ;
#80174 = CARTESIAN_POINT('Ctrl Pts',(129.602761524715,-75.2709336627545,-199.660729965474)) ;
#80175 = CARTESIAN_POINT('Ctrl Pts',(130.116086180007,-75.2213242877545,-199.147405310181)) ;
#80176 = CARTESIAN_POINT('Ctrl Pts',(130.842036869422,-75.1717149127545,-199.147405310181)) ;
#80177 = CARTESIAN_POINT('Ctrl Pts',(131.567987558837,-75.1221055377545,-199.147405310181)) ;
#80178 = CARTESIAN_POINT('Ctrl Pts',(132.08131221413,-75.0724961627545,-199.660729965474)) ;
#80179 = CARTESIAN_POINT('Ctrl Pts',(132.594636869422,-75.0228867877545,-200.174054620766)) ;
#80180 = CARTESIAN_POINT('Ctrl Pts',(132.594636869422,-74.9732774127545,-200.900005310181)) ;
#80181 = CARTESIAN_POINT('Ctrl Pts',(132.594636869422,-74.9236680377545,-201.625955999596)) ;
#80182 = CARTESIAN_POINT('Ctrl Pts',(132.08131221413,-74.8740586627545,-202.139280654889)) ;
#80183 = CARTESIAN_POINT('Ctrl Pts',(131.567987558837,-74.8244492877545,-202.652605310181)) ;
#80184 = CARTESIAN_POINT('Ctrl Pts',(130.842036869422,-74.7748399127545,-202.652605310181)) ;
#80185 = CARTESIAN_POINT('Ctrl Pts',(130.116086180007,-74.7252305377545,-202.652605310181)) ;
#80186 = CARTESIAN_POINT('Ctrl Pts',(129.602761524715,-74.6756211627545,-202.139280654889)) ;
#80187 = CARTESIAN_POINT('Ctrl Pts',(129.089436869422,-74.6260117877545,-201.625955999596)) ;
#80188 = CARTESIAN_POINT('Ctrl Pts',(129.089436869422,-74.5764024127545,-200.900005310181)) ;
#80189 = CARTESIAN_POINT('Ctrl Pts',(129.089436869422,-74.5267930377545,-200.174054620766)) ;
#80190 = CARTESIAN_POINT('Ctrl Pts',(129.602761524715,-74.4771836627545,-199.660729965474)) ;
#80191 = CARTESIAN_POINT('Ctrl Pts',(130.116086180007,-74.4275742877545,-199.147405310181)) ;
#80192 = CARTESIAN_POINT('Ctrl Pts',(130.842036869422,-74.3779649127545,-199.147405310181)) ;
#80193 = CARTESIAN_POINT('Ctrl Pts',(131.567987558837,-74.3283555377545,-199.147405310181)) ;
#80194 = CARTESIAN_POINT('Ctrl Pts',(132.08131221413,-74.2787461627545,-199.660729965474)) ;
#80195 = CARTESIAN_POINT('Ctrl Pts',(132.594636869422,-74.2291367877545,-200.174054620766)) ;
#80196 = CARTESIAN_POINT('Ctrl Pts',(132.594636869422,-74.1795274127545,-200.900005310181)) ;
#80197 = CARTESIAN_POINT('Ctrl Pts',(132.594636869422,-74.1299180377545,-201.625955999596)) ;
#80198 = CARTESIAN_POINT('Ctrl Pts',(132.08131221413,-74.0803086627545,-202.139280654889)) ;
#80199 = CARTESIAN_POINT('Ctrl Pts',(131.567987558837,-74.0306992877545,-202.652605310181)) ;
#80200 = CARTESIAN_POINT('Ctrl Pts',(130.842036869422,-73.9810899127545,-202.652605310181)) ;
#80201 = CARTESIAN_POINT('Ctrl Pts',(130.116086180007,-73.9314805377545,-202.652605310181)) ;
#80202 = CARTESIAN_POINT('Ctrl Pts',(129.602761524715,-73.8818711627545,-202.139280654889)) ;
#80203 = CARTESIAN_POINT('Ctrl Pts',(129.089436869422,-73.8322617877545,-201.625955999596)) ;
#80204 = CARTESIAN_POINT('Ctrl Pts',(129.089436869422,-73.7826524127545,-200.900005310181)) ;
#80205 = CARTESIAN_POINT('Ctrl Pts',(129.089436869422,-73.7330430377545,-200.174054620766)) ;
#80206 = CARTESIAN_POINT('Ctrl Pts',(129.602761524715,-73.6834336627545,-199.660729965474)) ;
#80207 = CARTESIAN_POINT('Ctrl Pts',(130.116086180007,-73.6338242877545,-199.147405310181)) ;
#80208 = CARTESIAN_POINT('Ctrl Pts',(130.842036869422,-73.5842149127545,-199.147405310181)) ;
#80209 = CARTESIAN_POINT('Ctrl Pts',(131.567987558837,-73.5346055377545,-199.147405310181)) ;
#80210 = CARTESIAN_POINT('Ctrl Pts',(132.08131221413,-73.4849961627545,-199.660729965474)) ;
#80211 = CARTESIAN_POINT('Ctrl Pts',(132.594636869422,-73.4353867877545,-200.174054620766)) ;
#80212 = CARTESIAN_POINT('Ctrl Pts',(132.594636869422,-73.3857774127545,-200.900005310181)) ;
#80213 = CARTESIAN_POINT('Ctrl Pts',(132.079081121232,-80.8271836627545,-200.900005310181)) ;
#80214 = CARTESIAN_POINT('Ctrl Pts',(132.079081121232,-80.7775742877545,-201.412405816536)) ;
#80215 = CARTESIAN_POINT('Ctrl Pts',(131.716759248505,-80.7279649127545,-201.774727689263)) ;
#80216 = CARTESIAN_POINT('Ctrl Pts',(131.354437375778,-80.6783555377545,-202.137049561991)) ;
#80217 = CARTESIAN_POINT('Ctrl Pts',(130.842036869422,-80.6287461627545,-202.137049561991)) ;
#80218 = CARTESIAN_POINT('Ctrl Pts',(130.329636363067,-80.5791367877545,-202.137049561991)) ;
#80219 = CARTESIAN_POINT('Ctrl Pts',(129.96731449034,-80.5295274127545,-201.774727689264)) ;
#80220 = CARTESIAN_POINT('Ctrl Pts',(129.604992617613,-80.4799180377545,-201.412405816536)) ;
#80221 = CARTESIAN_POINT('Ctrl Pts',(129.604992617613,-80.4303086627545,-200.900005310181)) ;
#80222 = CARTESIAN_POINT('Ctrl Pts',(129.604992617613,-80.3806992877545,-200.387604803826)) ;
#80223 = CARTESIAN_POINT('Ctrl Pts',(129.96731449034,-80.3310899127545,-200.025282931099)) ;
#80224 = CARTESIAN_POINT('Ctrl Pts',(130.329636363067,-80.2814805377545,-199.662961058372)) ;
#80225 = CARTESIAN_POINT('Ctrl Pts',(130.842036869422,-80.2318711627545,-199.662961058372)) ;
#80226 = CARTESIAN_POINT('Ctrl Pts',(131.354437375778,-80.1822617877545,-199.662961058371)) ;
#80227 = CARTESIAN_POINT('Ctrl Pts',(131.716759248505,-80.1326524127545,-200.025282931099)) ;
#80228 = CARTESIAN_POINT('Ctrl Pts',(132.079081121232,-80.0830430377545,-200.387604803826)) ;
#80229 = CARTESIAN_POINT('Ctrl Pts',(132.079081121232,-80.0334336627545,-200.900005310181)) ;
#80230 = CARTESIAN_POINT('Ctrl Pts',(132.079081121232,-79.9838242877545,-201.412405816536)) ;
#80231 = CARTESIAN_POINT('Ctrl Pts',(131.716759248505,-79.9342149127545,-201.774727689263)) ;
#80232 = CARTESIAN_POINT('Ctrl Pts',(131.354437375778,-79.8846055377545,-202.137049561991)) ;
#80233 = CARTESIAN_POINT('Ctrl Pts',(130.842036869422,-79.8349961627545,-202.137049561991)) ;
#80234 = CARTESIAN_POINT('Ctrl Pts',(130.329636363067,-79.7853867877545,-202.137049561991)) ;
#80235 = CARTESIAN_POINT('Ctrl Pts',(129.96731449034,-79.7357774127545,-201.774727689264)) ;
#80236 = CARTESIAN_POINT('Ctrl Pts',(129.604992617613,-79.6861680377545,-201.412405816536)) ;
#80237 = CARTESIAN_POINT('Ctrl Pts',(129.604992617613,-79.6365586627545,-200.900005310181)) ;
#80238 = CARTESIAN_POINT('Ctrl Pts',(129.604992617613,-79.5869492877545,-200.387604803826)) ;
#80239 = CARTESIAN_POINT('Ctrl Pts',(129.96731449034,-79.5373399127545,-200.025282931099)) ;
#80240 = CARTESIAN_POINT('Ctrl Pts',(130.329636363067,-79.4877305377545,-199.662961058372)) ;
#80241 = CARTESIAN_POINT('Ctrl Pts',(130.842036869422,-79.4381211627545,-199.662961058372)) ;
#80242 = CARTESIAN_POINT('Ctrl Pts',(131.354437375778,-79.3885117877545,-199.662961058371)) ;
#80243 = CARTESIAN_POINT('Ctrl Pts',(131.716759248505,-79.3389024127545,-200.025282931099)) ;
#80244 = CARTESIAN_POINT('Ctrl Pts',(132.079081121232,-79.2892930377545,-200.387604803826)) ;
#80245 = CARTESIAN_POINT('Ctrl Pts',(132.079081121232,-79.2396836627545,-200.900005310181)) ;
#80246 = CARTESIAN_POINT('Ctrl Pts',(132.079081121232,-79.1900742877545,-201.412405816536)) ;
#80247 = CARTESIAN_POINT('Ctrl Pts',(131.716759248505,-79.1404649127545,-201.774727689263)) ;
#80248 = CARTESIAN_POINT('Ctrl Pts',(131.354437375778,-79.0908555377545,-202.137049561991)) ;
#80249 = CARTESIAN_POINT('Ctrl Pts',(130.842036869422,-79.0412461627545,-202.137049561991)) ;
#80250 = CARTESIAN_POINT('Ctrl Pts',(130.329636363067,-78.9916367877545,-202.137049561991)) ;
#80251 = CARTESIAN_POINT('Ctrl Pts',(129.96731449034,-78.9420274127545,-201.774727689264)) ;
#80252 = CARTESIAN_POINT('Ctrl Pts',(129.604992617613,-78.8924180377545,-201.412405816536)) ;
#80253 = CARTESIAN_POINT('Ctrl Pts',(129.604992617613,-78.8428086627545,-200.900005310181)) ;
#80254 = CARTESIAN_POINT('Ctrl Pts',(129.604992617613,-78.7931992877545,-200.387604803826)) ;
#80255 = CARTESIAN_POINT('Ctrl Pts',(129.96731449034,-78.7435899127545,-200.025282931099)) ;
#80256 = CARTESIAN_POINT('Ctrl Pts',(130.329636363067,-78.6939805377545,-199.662961058372)) ;
#80257 = CARTESIAN_POINT('Ctrl Pts',(130.842036869422,-78.6443711627545,-199.662961058372)) ;
#80258 = CARTESIAN_POINT('Ctrl Pts',(131.354437375778,-78.5947617877545,-199.662961058371)) ;
#80259 = CARTESIAN_POINT('Ctrl Pts',(131.716759248505,-78.5451524127545,-200.025282931099)) ;
#80260 = CARTESIAN_POINT('Ctrl Pts',(132.079081121232,-78.4955430377545,-200.387604803826)) ;
#80261 = CARTESIAN_POINT('Ctrl Pts',(132.079081121232,-78.4459336627545,-200.900005310181)) ;
#80262 = CARTESIAN_POINT('Ctrl Pts',(132.079081121232,-78.3963242877545,-201.412405816536)) ;
#80263 = CARTESIAN_POINT('Ctrl Pts',(131.716759248505,-78.3467149127545,-201.774727689263)) ;
#80264 = CARTESIAN_POINT('Ctrl Pts',(131.354437375778,-78.2971055377545,-202.137049561991)) ;
#80265 = CARTESIAN_POINT('Ctrl Pts',(130.842036869422,-78.2474961627545,-202.137049561991)) ;
#80266 = CARTESIAN_POINT('Ctrl Pts',(130.329636363067,-78.1978867877545,-202.137049561991)) ;
#80267 = CARTESIAN_POINT('Ctrl Pts',(129.96731449034,-78.1482774127545,-201.774727689264)) ;
#80268 = CARTESIAN_POINT('Ctrl Pts',(129.604992617613,-78.0986680377545,-201.412405816536)) ;
#80269 = CARTESIAN_POINT('Ctrl Pts',(129.604992617613,-78.0490586627545,-200.900005310181)) ;
#80270 = CARTESIAN_POINT('Ctrl Pts',(129.604992617613,-77.9994492877545,-200.387604803826)) ;
#80271 = CARTESIAN_POINT('Ctrl Pts',(129.96731449034,-77.9498399127545,-200.025282931099)) ;
#80272 = CARTESIAN_POINT('Ctrl Pts',(130.329636363067,-77.9002305377545,-199.662961058372)) ;
#80273 = CARTESIAN_POINT('Ctrl Pts',(130.842036869422,-77.8506211627545,-199.662961058372)) ;
#80274 = CARTESIAN_POINT('Ctrl Pts',(131.354437375778,-77.8010117877545,-199.662961058371)) ;
#80275 = CARTESIAN_POINT('Ctrl Pts',(131.716759248505,-77.7514024127545,-200.025282931099)) ;
#80276 = CARTESIAN_POINT('Ctrl Pts',(132.079081121232,-77.7017930377545,-200.387604803826)) ;
#80277 = CARTESIAN_POINT('Ctrl Pts',(132.079081121232,-77.6521836627545,-200.900005310181)) ;
#80278 = CARTESIAN_POINT('Ctrl Pts',(132.079081121232,-77.6025742877545,-201.412405816536)) ;
#80279 = CARTESIAN_POINT('Ctrl Pts',(131.716759248505,-77.5529649127545,-201.774727689263)) ;
#80280 = CARTESIAN_POINT('Ctrl Pts',(131.354437375778,-77.5033555377545,-202.137049561991)) ;
#80281 = CARTESIAN_POINT('Ctrl Pts',(130.842036869422,-77.4537461627545,-202.137049561991)) ;
#80282 = CARTESIAN_POINT('Ctrl Pts',(130.329636363067,-77.4041367877545,-202.137049561991)) ;
#80283 = CARTESIAN_POINT('Ctrl Pts',(129.96731449034,-77.3545274127545,-201.774727689264)) ;
#80284 = CARTESIAN_POINT('Ctrl Pts',(129.604992617613,-77.3049180377545,-201.412405816536)) ;
#80285 = CARTESIAN_POINT('Ctrl Pts',(129.604992617613,-77.2553086627545,-200.900005310181)) ;
#80286 = CARTESIAN_POINT('Ctrl Pts',(129.604992617613,-77.2056992877545,-200.387604803826)) ;
#80287 = CARTESIAN_POINT('Ctrl Pts',(129.96731449034,-77.1560899127545,-200.025282931099)) ;
#80288 = CARTESIAN_POINT('Ctrl Pts',(130.329636363067,-77.1064805377545,-199.662961058372)) ;
#80289 = CARTESIAN_POINT('Ctrl Pts',(130.842036869422,-77.0568711627545,-199.662961058372)) ;
#80290 = CARTESIAN_POINT('Ctrl Pts',(131.354437375778,-77.0072617877545,-199.662961058371)) ;
#80291 = CARTESIAN_POINT('Ctrl Pts',(131.716759248505,-76.9576524127545,-200.025282931099)) ;
#80292 = CARTESIAN_POINT('Ctrl Pts',(132.079081121232,-76.9080430377545,-200.387604803826)) ;
#80293 = CARTESIAN_POINT('Ctrl Pts',(132.079081121232,-76.8584336627545,-200.900005310181)) ;
#80294 = CARTESIAN_POINT('Ctrl Pts',(132.079081121232,-76.8088242877545,-201.412405816536)) ;
#80295 = CARTESIAN_POINT('Ctrl Pts',(131.716759248505,-76.7592149127545,-201.774727689263)) ;
#80296 = CARTESIAN_POINT('Ctrl Pts',(131.354437375778,-76.7096055377545,-202.137049561991)) ;
#80297 = CARTESIAN_POINT('Ctrl Pts',(130.842036869422,-76.6599961627545,-202.137049561991)) ;
#80298 = CARTESIAN_POINT('Ctrl Pts',(130.329636363067,-76.6103867877545,-202.137049561991)) ;
#80299 = CARTESIAN_POINT('Ctrl Pts',(129.96731449034,-76.5607774127545,-201.774727689264)) ;
#80300 = CARTESIAN_POINT('Ctrl Pts',(129.604992617613,-76.5111680377545,-201.412405816536)) ;
#80301 = CARTESIAN_POINT('Ctrl Pts',(129.604992617613,-76.4615586627545,-200.900005310181)) ;
#80302 = CARTESIAN_POINT('Ctrl Pts',(129.604992617613,-76.4119492877545,-200.387604803826)) ;
#80303 = CARTESIAN_POINT('Ctrl Pts',(129.96731449034,-76.3623399127545,-200.025282931099)) ;
#80304 = CARTESIAN_POINT('Ctrl Pts',(130.329636363067,-76.3127305377545,-199.662961058372)) ;
#80305 = CARTESIAN_POINT('Ctrl Pts',(130.842036869422,-76.2631211627545,-199.662961058372)) ;
#80306 = CARTESIAN_POINT('Ctrl Pts',(131.354437375778,-76.2135117877545,-199.662961058371)) ;
#80307 = CARTESIAN_POINT('Ctrl Pts',(131.716759248505,-76.1639024127545,-200.025282931099)) ;
#80308 = CARTESIAN_POINT('Ctrl Pts',(132.079081121232,-76.1142930377545,-200.387604803826)) ;
#80309 = CARTESIAN_POINT('Ctrl Pts',(132.079081121232,-76.0646836627545,-200.900005310181)) ;
#80310 = CARTESIAN_POINT('Ctrl Pts',(132.079081121232,-76.0150742877545,-201.412405816536)) ;
#80311 = CARTESIAN_POINT('Ctrl Pts',(131.716759248505,-75.9654649127545,-201.774727689263)) ;
#80312 = CARTESIAN_POINT('Ctrl Pts',(131.354437375778,-75.9158555377545,-202.137049561991)) ;
#80313 = CARTESIAN_POINT('Ctrl Pts',(130.842036869422,-75.8662461627545,-202.137049561991)) ;
#80314 = CARTESIAN_POINT('Ctrl Pts',(130.329636363067,-75.8166367877545,-202.137049561991)) ;
#80315 = CARTESIAN_POINT('Ctrl Pts',(129.96731449034,-75.7670274127545,-201.774727689264)) ;
#80316 = CARTESIAN_POINT('Ctrl Pts',(129.604992617613,-75.7174180377545,-201.412405816536)) ;
#80317 = CARTESIAN_POINT('Ctrl Pts',(129.604992617613,-75.6678086627545,-200.900005310181)) ;
#80318 = CARTESIAN_POINT('Ctrl Pts',(129.604992617613,-75.6181992877545,-200.387604803826)) ;
#80319 = CARTESIAN_POINT('Ctrl Pts',(129.96731449034,-75.5685899127545,-200.025282931099)) ;
#80320 = CARTESIAN_POINT('Ctrl Pts',(130.329636363067,-75.5189805377545,-199.662961058372)) ;
#80321 = CARTESIAN_POINT('Ctrl Pts',(130.842036869422,-75.4693711627545,-199.662961058372)) ;
#80322 = CARTESIAN_POINT('Ctrl Pts',(131.354437375778,-75.4197617877545,-199.662961058371)) ;
#80323 = CARTESIAN_POINT('Ctrl Pts',(131.716759248505,-75.3701524127545,-200.025282931099)) ;
#80324 = CARTESIAN_POINT('Ctrl Pts',(132.079081121232,-75.3205430377545,-200.387604803826)) ;
#80325 = CARTESIAN_POINT('Ctrl Pts',(132.079081121232,-75.2709336627545,-200.900005310181)) ;
#80326 = CARTESIAN_POINT('Ctrl Pts',(132.079081121232,-75.2213242877545,-201.412405816536)) ;
#80327 = CARTESIAN_POINT('Ctrl Pts',(131.716759248505,-75.1717149127545,-201.774727689263)) ;
#80328 = CARTESIAN_POINT('Ctrl Pts',(131.354437375778,-75.1221055377545,-202.137049561991)) ;
#80329 = CARTESIAN_POINT('Ctrl Pts',(130.842036869422,-75.0724961627545,-202.137049561991)) ;
#80330 = CARTESIAN_POINT('Ctrl Pts',(130.329636363067,-75.0228867877545,-202.137049561991)) ;
#80331 = CARTESIAN_POINT('Ctrl Pts',(129.96731449034,-74.9732774127545,-201.774727689264)) ;
#80332 = CARTESIAN_POINT('Ctrl Pts',(129.604992617613,-74.9236680377545,-201.412405816536)) ;
#80333 = CARTESIAN_POINT('Ctrl Pts',(129.604992617613,-74.8740586627545,-200.900005310181)) ;
#80334 = CARTESIAN_POINT('Ctrl Pts',(129.604992617613,-74.8244492877545,-200.387604803826)) ;
#80335 = CARTESIAN_POINT('Ctrl Pts',(129.96731449034,-74.7748399127545,-200.025282931099)) ;
#80336 = CARTESIAN_POINT('Ctrl Pts',(130.329636363067,-74.7252305377545,-199.662961058372)) ;
#80337 = CARTESIAN_POINT('Ctrl Pts',(130.842036869422,-74.6756211627545,-199.662961058372)) ;
#80338 = CARTESIAN_POINT('Ctrl Pts',(131.354437375778,-74.6260117877545,-199.662961058371)) ;
#80339 = CARTESIAN_POINT('Ctrl Pts',(131.716759248505,-74.5764024127545,-200.025282931099)) ;
#80340 = CARTESIAN_POINT('Ctrl Pts',(132.079081121232,-74.5267930377545,-200.387604803826)) ;
#80341 = CARTESIAN_POINT('Ctrl Pts',(132.079081121232,-74.4771836627545,-200.900005310181)) ;
#80342 = CARTESIAN_POINT('Ctrl Pts',(132.079081121232,-74.4275742877545,-201.412405816536)) ;
#80343 = CARTESIAN_POINT('Ctrl Pts',(131.716759248505,-74.3779649127545,-201.774727689263)) ;
#80344 = CARTESIAN_POINT('Ctrl Pts',(131.354437375778,-74.3283555377545,-202.137049561991)) ;
#80345 = CARTESIAN_POINT('Ctrl Pts',(130.842036869422,-74.2787461627545,-202.137049561991)) ;
#80346 = CARTESIAN_POINT('Ctrl Pts',(130.329636363067,-74.2291367877545,-202.137049561991)) ;
#80347 = CARTESIAN_POINT('Ctrl Pts',(129.96731449034,-74.1795274127545,-201.774727689264)) ;
#80348 = CARTESIAN_POINT('Ctrl Pts',(129.604992617613,-74.1299180377545,-201.412405816536)) ;
#80349 = CARTESIAN_POINT('Ctrl Pts',(129.604992617613,-74.0803086627545,-200.900005310181)) ;
#80350 = CARTESIAN_POINT('Ctrl Pts',(129.604992617613,-74.0306992877545,-200.387604803826)) ;
#80351 = CARTESIAN_POINT('Ctrl Pts',(129.96731449034,-73.9810899127545,-200.025282931099)) ;
#80352 = CARTESIAN_POINT('Ctrl Pts',(130.329636363067,-73.9314805377545,-199.662961058372)) ;
#80353 = CARTESIAN_POINT('Ctrl Pts',(130.842036869422,-73.8818711627545,-199.662961058372)) ;
#80354 = CARTESIAN_POINT('Ctrl Pts',(131.354437375778,-73.8322617877545,-199.662961058371)) ;
#80355 = CARTESIAN_POINT('Ctrl Pts',(131.716759248505,-73.7826524127545,-200.025282931099)) ;
#80356 = CARTESIAN_POINT('Ctrl Pts',(132.079081121232,-73.7330430377545,-200.387604803826)) ;
#80357 = CARTESIAN_POINT('Ctrl Pts',(132.079081121232,-73.6834336627545,-200.900005310181)) ;
#80358 = CARTESIAN_POINT('Ctrl Pts',(131.259739170827,-81.3002309583791,-200.900005310181)) ;
#80359 = CARTESIAN_POINT('Ctrl Pts',(131.259739170827,-81.2506215833791,-201.073023268457)) ;
#80360 = CARTESIAN_POINT('Ctrl Pts',(131.137396999263,-81.2010122083791,-201.195365440022)) ;
#80361 = CARTESIAN_POINT('Ctrl Pts',(131.015054827699,-81.1514028333791,-201.317707611586)) ;
#80362 = CARTESIAN_POINT('Ctrl Pts',(130.842036869422,-81.1017934583791,-201.317707611586)) ;
#80363 = CARTESIAN_POINT('Ctrl Pts',(130.669018911146,-81.0521840833791,-201.317707611586)) ;
#80364 = CARTESIAN_POINT('Ctrl Pts',(130.546676739582,-81.0025747083791,-201.195365440022)) ;
#80365 = CARTESIAN_POINT('Ctrl Pts',(130.424334568018,-80.9529653333791,-201.073023268457)) ;
#80366 = CARTESIAN_POINT('Ctrl Pts',(130.424334568018,-80.9033559583791,-200.900005310181)) ;
#80367 = CARTESIAN_POINT('Ctrl Pts',(130.424334568018,-80.8537465833791,-200.726987351905)) ;
#80368 = CARTESIAN_POINT('Ctrl Pts',(130.546676739582,-80.8041372083791,-200.604645180341)) ;
#80369 = CARTESIAN_POINT('Ctrl Pts',(130.669018911146,-80.7545278333791,-200.482303008776)) ;
#80370 = CARTESIAN_POINT('Ctrl Pts',(130.842036869422,-80.7049184583791,-200.482303008776)) ;
#80371 = CARTESIAN_POINT('Ctrl Pts',(131.015054827699,-80.6553090833791,-200.482303008776)) ;
#80372 = CARTESIAN_POINT('Ctrl Pts',(131.137396999263,-80.6056997083791,-200.604645180341)) ;
#80373 = CARTESIAN_POINT('Ctrl Pts',(131.259739170827,-80.5560903333791,-200.726987351905)) ;
#80374 = CARTESIAN_POINT('Ctrl Pts',(131.259739170827,-80.5064809583791,-200.900005310181)) ;
#80375 = CARTESIAN_POINT('Ctrl Pts',(131.259739170827,-80.4568715833791,-201.073023268457)) ;
#80376 = CARTESIAN_POINT('Ctrl Pts',(131.137396999263,-80.4072622083791,-201.195365440022)) ;
#80377 = CARTESIAN_POINT('Ctrl Pts',(131.015054827699,-80.3576528333791,-201.317707611586)) ;
#80378 = CARTESIAN_POINT('Ctrl Pts',(130.842036869422,-80.3080434583791,-201.317707611586)) ;
#80379 = CARTESIAN_POINT('Ctrl Pts',(130.669018911146,-80.2584340833791,-201.317707611586)) ;
#80380 = CARTESIAN_POINT('Ctrl Pts',(130.546676739582,-80.2088247083791,-201.195365440022)) ;
#80381 = CARTESIAN_POINT('Ctrl Pts',(130.424334568018,-80.1592153333791,-201.073023268457)) ;
#80382 = CARTESIAN_POINT('Ctrl Pts',(130.424334568018,-80.1096059583791,-200.900005310181)) ;
#80383 = CARTESIAN_POINT('Ctrl Pts',(130.424334568018,-80.0599965833791,-200.726987351905)) ;
#80384 = CARTESIAN_POINT('Ctrl Pts',(130.546676739582,-80.0103872083791,-200.604645180341)) ;
#80385 = CARTESIAN_POINT('Ctrl Pts',(130.669018911146,-79.9607778333791,-200.482303008776)) ;
#80386 = CARTESIAN_POINT('Ctrl Pts',(130.842036869422,-79.9111684583791,-200.482303008776)) ;
#80387 = CARTESIAN_POINT('Ctrl Pts',(131.015054827699,-79.8615590833791,-200.482303008776)) ;
#80388 = CARTESIAN_POINT('Ctrl Pts',(131.137396999263,-79.8119497083791,-200.604645180341)) ;
#80389 = CARTESIAN_POINT('Ctrl Pts',(131.259739170827,-79.7623403333791,-200.726987351905)) ;
#80390 = CARTESIAN_POINT('Ctrl Pts',(131.259739170827,-79.7127309583791,-200.900005310181)) ;
#80391 = CARTESIAN_POINT('Ctrl Pts',(131.259739170827,-79.6631215833791,-201.073023268457)) ;
#80392 = CARTESIAN_POINT('Ctrl Pts',(131.137396999263,-79.6135122083791,-201.195365440022)) ;
#80393 = CARTESIAN_POINT('Ctrl Pts',(131.015054827699,-79.5639028333791,-201.317707611586)) ;
#80394 = CARTESIAN_POINT('Ctrl Pts',(130.842036869422,-79.5142934583791,-201.317707611586)) ;
#80395 = CARTESIAN_POINT('Ctrl Pts',(130.669018911146,-79.4646840833791,-201.317707611586)) ;
#80396 = CARTESIAN_POINT('Ctrl Pts',(130.546676739582,-79.4150747083791,-201.195365440022)) ;
#80397 = CARTESIAN_POINT('Ctrl Pts',(130.424334568018,-79.3654653333791,-201.073023268457)) ;
#80398 = CARTESIAN_POINT('Ctrl Pts',(130.424334568018,-79.3158559583791,-200.900005310181)) ;
#80399 = CARTESIAN_POINT('Ctrl Pts',(130.424334568018,-79.2662465833791,-200.726987351905)) ;
#80400 = CARTESIAN_POINT('Ctrl Pts',(130.546676739582,-79.2166372083791,-200.604645180341)) ;
#80401 = CARTESIAN_POINT('Ctrl Pts',(130.669018911146,-79.1670278333791,-200.482303008776)) ;
#80402 = CARTESIAN_POINT('Ctrl Pts',(130.842036869422,-79.1174184583791,-200.482303008776)) ;
#80403 = CARTESIAN_POINT('Ctrl Pts',(131.015054827699,-79.0678090833791,-200.482303008776)) ;
#80404 = CARTESIAN_POINT('Ctrl Pts',(131.137396999263,-79.0181997083791,-200.604645180341)) ;
#80405 = CARTESIAN_POINT('Ctrl Pts',(131.259739170827,-78.9685903333791,-200.726987351905)) ;
#80406 = CARTESIAN_POINT('Ctrl Pts',(131.259739170827,-78.9189809583791,-200.900005310181)) ;
#80407 = CARTESIAN_POINT('Ctrl Pts',(131.259739170827,-78.8693715833791,-201.073023268457)) ;
#80408 = CARTESIAN_POINT('Ctrl Pts',(131.137396999263,-78.8197622083791,-201.195365440022)) ;
#80409 = CARTESIAN_POINT('Ctrl Pts',(131.015054827699,-78.7701528333791,-201.317707611586)) ;
#80410 = CARTESIAN_POINT('Ctrl Pts',(130.842036869422,-78.7205434583791,-201.317707611586)) ;
#80411 = CARTESIAN_POINT('Ctrl Pts',(130.669018911146,-78.6709340833791,-201.317707611586)) ;
#80412 = CARTESIAN_POINT('Ctrl Pts',(130.546676739582,-78.6213247083791,-201.195365440022)) ;
#80413 = CARTESIAN_POINT('Ctrl Pts',(130.424334568018,-78.5717153333791,-201.073023268457)) ;
#80414 = CARTESIAN_POINT('Ctrl Pts',(130.424334568018,-78.5221059583791,-200.900005310181)) ;
#80415 = CARTESIAN_POINT('Ctrl Pts',(130.424334568018,-78.4724965833791,-200.726987351905)) ;
#80416 = CARTESIAN_POINT('Ctrl Pts',(130.546676739582,-78.4228872083791,-200.604645180341)) ;
#80417 = CARTESIAN_POINT('Ctrl Pts',(130.669018911146,-78.3732778333791,-200.482303008776)) ;
#80418 = CARTESIAN_POINT('Ctrl Pts',(130.842036869422,-78.3236684583791,-200.482303008776)) ;
#80419 = CARTESIAN_POINT('Ctrl Pts',(131.015054827699,-78.2740590833791,-200.482303008776)) ;
#80420 = CARTESIAN_POINT('Ctrl Pts',(131.137396999263,-78.2244497083791,-200.604645180341)) ;
#80421 = CARTESIAN_POINT('Ctrl Pts',(131.259739170827,-78.1748403333791,-200.726987351905)) ;
#80422 = CARTESIAN_POINT('Ctrl Pts',(131.259739170827,-78.1252309583791,-200.900005310181)) ;
#80423 = CARTESIAN_POINT('Ctrl Pts',(131.259739170827,-78.0756215833791,-201.073023268457)) ;
#80424 = CARTESIAN_POINT('Ctrl Pts',(131.137396999263,-78.0260122083791,-201.195365440022)) ;
#80425 = CARTESIAN_POINT('Ctrl Pts',(131.015054827699,-77.9764028333791,-201.317707611586)) ;
#80426 = CARTESIAN_POINT('Ctrl Pts',(130.842036869422,-77.9267934583791,-201.317707611586)) ;
#80427 = CARTESIAN_POINT('Ctrl Pts',(130.669018911146,-77.8771840833791,-201.317707611586)) ;
#80428 = CARTESIAN_POINT('Ctrl Pts',(130.546676739582,-77.8275747083791,-201.195365440022)) ;
#80429 = CARTESIAN_POINT('Ctrl Pts',(130.424334568018,-77.7779653333791,-201.073023268457)) ;
#80430 = CARTESIAN_POINT('Ctrl Pts',(130.424334568018,-77.7283559583791,-200.900005310181)) ;
#80431 = CARTESIAN_POINT('Ctrl Pts',(130.424334568018,-77.6787465833791,-200.726987351905)) ;
#80432 = CARTESIAN_POINT('Ctrl Pts',(130.546676739582,-77.6291372083791,-200.604645180341)) ;
#80433 = CARTESIAN_POINT('Ctrl Pts',(130.669018911146,-77.5795278333791,-200.482303008776)) ;
#80434 = CARTESIAN_POINT('Ctrl Pts',(130.842036869422,-77.5299184583791,-200.482303008776)) ;
#80435 = CARTESIAN_POINT('Ctrl Pts',(131.015054827699,-77.4803090833791,-200.482303008776)) ;
#80436 = CARTESIAN_POINT('Ctrl Pts',(131.137396999263,-77.4306997083791,-200.604645180341)) ;
#80437 = CARTESIAN_POINT('Ctrl Pts',(131.259739170827,-77.3810903333791,-200.726987351905)) ;
#80438 = CARTESIAN_POINT('Ctrl Pts',(131.259739170827,-77.3314809583791,-200.900005310181)) ;
#80439 = CARTESIAN_POINT('Ctrl Pts',(131.259739170827,-77.2818715833791,-201.073023268457)) ;
#80440 = CARTESIAN_POINT('Ctrl Pts',(131.137396999263,-77.2322622083791,-201.195365440022)) ;
#80441 = CARTESIAN_POINT('Ctrl Pts',(131.015054827699,-77.1826528333791,-201.317707611586)) ;
#80442 = CARTESIAN_POINT('Ctrl Pts',(130.842036869422,-77.1330434583791,-201.317707611586)) ;
#80443 = CARTESIAN_POINT('Ctrl Pts',(130.669018911146,-77.0834340833791,-201.317707611586)) ;
#80444 = CARTESIAN_POINT('Ctrl Pts',(130.546676739582,-77.0338247083791,-201.195365440022)) ;
#80445 = CARTESIAN_POINT('Ctrl Pts',(130.424334568018,-76.9842153333791,-201.073023268457)) ;
#80446 = CARTESIAN_POINT('Ctrl Pts',(130.424334568018,-76.9346059583791,-200.900005310181)) ;
#80447 = CARTESIAN_POINT('Ctrl Pts',(130.424334568018,-76.8849965833791,-200.726987351905)) ;
#80448 = CARTESIAN_POINT('Ctrl Pts',(130.546676739582,-76.8353872083791,-200.604645180341)) ;
#80449 = CARTESIAN_POINT('Ctrl Pts',(130.669018911146,-76.7857778333791,-200.482303008776)) ;
#80450 = CARTESIAN_POINT('Ctrl Pts',(130.842036869422,-76.7361684583791,-200.482303008776)) ;
#80451 = CARTESIAN_POINT('Ctrl Pts',(131.015054827699,-76.6865590833791,-200.482303008776)) ;
#80452 = CARTESIAN_POINT('Ctrl Pts',(131.137396999263,-76.6369497083791,-200.604645180341)) ;
#80453 = CARTESIAN_POINT('Ctrl Pts',(131.259739170827,-76.5873403333791,-200.726987351905)) ;
#80454 = CARTESIAN_POINT('Ctrl Pts',(131.259739170827,-76.5377309583791,-200.900005310181)) ;
#80455 = CARTESIAN_POINT('Ctrl Pts',(131.259739170827,-76.4881215833791,-201.073023268457)) ;
#80456 = CARTESIAN_POINT('Ctrl Pts',(131.137396999263,-76.4385122083791,-201.195365440022)) ;
#80457 = CARTESIAN_POINT('Ctrl Pts',(131.015054827699,-76.3889028333791,-201.317707611586)) ;
#80458 = CARTESIAN_POINT('Ctrl Pts',(130.842036869422,-76.3392934583791,-201.317707611586)) ;
#80459 = CARTESIAN_POINT('Ctrl Pts',(130.669018911146,-76.2896840833791,-201.317707611586)) ;
#80460 = CARTESIAN_POINT('Ctrl Pts',(130.546676739582,-76.2400747083791,-201.195365440022)) ;
#80461 = CARTESIAN_POINT('Ctrl Pts',(130.424334568018,-76.1904653333791,-201.073023268457)) ;
#80462 = CARTESIAN_POINT('Ctrl Pts',(130.424334568018,-76.1408559583791,-200.900005310181)) ;
#80463 = CARTESIAN_POINT('Ctrl Pts',(130.424334568018,-76.0912465833791,-200.726987351905)) ;
#80464 = CARTESIAN_POINT('Ctrl Pts',(130.546676739582,-76.0416372083791,-200.604645180341)) ;
#80465 = CARTESIAN_POINT('Ctrl Pts',(130.669018911146,-75.9920278333791,-200.482303008776)) ;
#80466 = CARTESIAN_POINT('Ctrl Pts',(130.842036869422,-75.9424184583791,-200.482303008776)) ;
#80467 = CARTESIAN_POINT('Ctrl Pts',(131.015054827699,-75.8928090833791,-200.482303008776)) ;
#80468 = CARTESIAN_POINT('Ctrl Pts',(131.137396999263,-75.8431997083791,-200.604645180341)) ;
#80469 = CARTESIAN_POINT('Ctrl Pts',(131.259739170827,-75.7935903333791,-200.726987351905)) ;
#80470 = CARTESIAN_POINT('Ctrl Pts',(131.259739170827,-75.7439809583791,-200.900005310181)) ;
#80471 = CARTESIAN_POINT('Ctrl Pts',(131.259739170827,-75.6943715833791,-201.073023268457)) ;
#80472 = CARTESIAN_POINT('Ctrl Pts',(131.137396999263,-75.6447622083791,-201.195365440022)) ;
#80473 = CARTESIAN_POINT('Ctrl Pts',(131.015054827699,-75.5951528333791,-201.317707611586)) ;
#80474 = CARTESIAN_POINT('Ctrl Pts',(130.842036869422,-75.5455434583791,-201.317707611586)) ;
#80475 = CARTESIAN_POINT('Ctrl Pts',(130.669018911146,-75.4959340833791,-201.317707611586)) ;
#80476 = CARTESIAN_POINT('Ctrl Pts',(130.546676739582,-75.4463247083791,-201.195365440022)) ;
#80477 = CARTESIAN_POINT('Ctrl Pts',(130.424334568018,-75.3967153333791,-201.073023268457)) ;
#80478 = CARTESIAN_POINT('Ctrl Pts',(130.424334568018,-75.3471059583791,-200.900005310181)) ;
#80479 = CARTESIAN_POINT('Ctrl Pts',(130.424334568018,-75.2974965833791,-200.726987351905)) ;
#80480 = CARTESIAN_POINT('Ctrl Pts',(130.546676739582,-75.2478872083791,-200.604645180341)) ;
#80481 = CARTESIAN_POINT('Ctrl Pts',(130.669018911146,-75.1982778333791,-200.482303008776)) ;
#80482 = CARTESIAN_POINT('Ctrl Pts',(130.842036869422,-75.1486684583791,-200.482303008776)) ;
#80483 = CARTESIAN_POINT('Ctrl Pts',(131.015054827699,-75.0990590833791,-200.482303008776)) ;
#80484 = CARTESIAN_POINT('Ctrl Pts',(131.137396999263,-75.0494497083791,-200.604645180341)) ;
#80485 = CARTESIAN_POINT('Ctrl Pts',(131.259739170827,-74.9998403333791,-200.726987351905)) ;
#80486 = CARTESIAN_POINT('Ctrl Pts',(131.259739170827,-74.9502309583791,-200.900005310181)) ;
#80487 = CARTESIAN_POINT('Ctrl Pts',(131.259739170827,-74.9006215833791,-201.073023268457)) ;
#80488 = CARTESIAN_POINT('Ctrl Pts',(131.137396999263,-74.8510122083791,-201.195365440022)) ;
#80489 = CARTESIAN_POINT('Ctrl Pts',(131.015054827699,-74.8014028333791,-201.317707611586)) ;
#80490 = CARTESIAN_POINT('Ctrl Pts',(130.842036869422,-74.7517934583791,-201.317707611586)) ;
#80491 = CARTESIAN_POINT('Ctrl Pts',(130.669018911146,-74.7021840833791,-201.317707611586)) ;
#80492 = CARTESIAN_POINT('Ctrl Pts',(130.546676739582,-74.6525747083791,-201.195365440022)) ;
#80493 = CARTESIAN_POINT('Ctrl Pts',(130.424334568018,-74.6029653333791,-201.073023268457)) ;
#80494 = CARTESIAN_POINT('Ctrl Pts',(130.424334568018,-74.5533559583791,-200.900005310181)) ;
#80495 = CARTESIAN_POINT('Ctrl Pts',(130.424334568018,-74.5037465833791,-200.726987351905)) ;
#80496 = CARTESIAN_POINT('Ctrl Pts',(130.546676739582,-74.4541372083791,-200.604645180341)) ;
#80497 = CARTESIAN_POINT('Ctrl Pts',(130.669018911146,-74.4045278333791,-200.482303008776)) ;
#80498 = CARTESIAN_POINT('Ctrl Pts',(130.842036869422,-74.3549184583791,-200.482303008776)) ;
#80499 = CARTESIAN_POINT('Ctrl Pts',(131.015054827699,-74.3053090833791,-200.482303008776)) ;
#80500 = CARTESIAN_POINT('Ctrl Pts',(131.137396999263,-74.2556997083791,-200.604645180341)) ;
#80501 = CARTESIAN_POINT('Ctrl Pts',(131.259739170827,-74.2060903333791,-200.726987351905)) ;
#80502 = CARTESIAN_POINT('Ctrl Pts',(131.259739170827,-74.1564809583791,-200.900005310181)) ;
#80503 = CARTESIAN_POINT('Ctrl Pts',(132.079081121232,-80.9264024127545,-200.900005310181)) ;
#80504 = CARTESIAN_POINT('Ctrl Pts',(132.079081121232,-80.8767930377545,-201.412405816536)) ;
#80505 = CARTESIAN_POINT('Ctrl Pts',(131.716759248505,-80.8271836627545,-201.774727689263)) ;
#80506 = CARTESIAN_POINT('Ctrl Pts',(131.354437375778,-80.7775742877545,-202.137049561991)) ;
#80507 = CARTESIAN_POINT('Ctrl Pts',(130.842036869422,-80.7279649127545,-202.137049561991)) ;
#80508 = CARTESIAN_POINT('Ctrl Pts',(130.329636363067,-80.6783555377545,-202.137049561991)) ;
#80509 = CARTESIAN_POINT('Ctrl Pts',(129.96731449034,-80.6287461627545,-201.774727689264)) ;
#80510 = CARTESIAN_POINT('Ctrl Pts',(129.604992617613,-80.5791367877545,-201.412405816536)) ;
#80511 = CARTESIAN_POINT('Ctrl Pts',(129.604992617613,-80.5295274127545,-200.900005310181)) ;
#80512 = CARTESIAN_POINT('Ctrl Pts',(129.604992617613,-80.4799180377545,-200.387604803826)) ;
#80513 = CARTESIAN_POINT('Ctrl Pts',(129.96731449034,-80.4303086627545,-200.025282931099)) ;
#80514 = CARTESIAN_POINT('Ctrl Pts',(130.329636363067,-80.3806992877545,-199.662961058372)) ;
#80515 = CARTESIAN_POINT('Ctrl Pts',(130.842036869422,-80.3310899127545,-199.662961058372)) ;
#80516 = CARTESIAN_POINT('Ctrl Pts',(131.354437375778,-80.2814805377545,-199.662961058371)) ;
#80517 = CARTESIAN_POINT('Ctrl Pts',(131.716759248505,-80.2318711627545,-200.025282931099)) ;
#80518 = CARTESIAN_POINT('Ctrl Pts',(132.079081121232,-80.1822617877545,-200.387604803826)) ;
#80519 = CARTESIAN_POINT('Ctrl Pts',(132.079081121232,-80.1326524127545,-200.900005310181)) ;
#80520 = CARTESIAN_POINT('Ctrl Pts',(132.079081121232,-80.0830430377545,-201.412405816536)) ;
#80521 = CARTESIAN_POINT('Ctrl Pts',(131.716759248505,-80.0334336627545,-201.774727689263)) ;
#80522 = CARTESIAN_POINT('Ctrl Pts',(131.354437375778,-79.9838242877545,-202.137049561991)) ;
#80523 = CARTESIAN_POINT('Ctrl Pts',(130.842036869422,-79.9342149127545,-202.137049561991)) ;
#80524 = CARTESIAN_POINT('Ctrl Pts',(130.329636363067,-79.8846055377545,-202.137049561991)) ;
#80525 = CARTESIAN_POINT('Ctrl Pts',(129.96731449034,-79.8349961627545,-201.774727689264)) ;
#80526 = CARTESIAN_POINT('Ctrl Pts',(129.604992617613,-79.7853867877545,-201.412405816536)) ;
#80527 = CARTESIAN_POINT('Ctrl Pts',(129.604992617613,-79.7357774127545,-200.900005310181)) ;
#80528 = CARTESIAN_POINT('Ctrl Pts',(129.604992617613,-79.6861680377545,-200.387604803826)) ;
#80529 = CARTESIAN_POINT('Ctrl Pts',(129.96731449034,-79.6365586627545,-200.025282931099)) ;
#80530 = CARTESIAN_POINT('Ctrl Pts',(130.329636363067,-79.5869492877545,-199.662961058372)) ;
#80531 = CARTESIAN_POINT('Ctrl Pts',(130.842036869422,-79.5373399127545,-199.662961058372)) ;
#80532 = CARTESIAN_POINT('Ctrl Pts',(131.354437375778,-79.4877305377545,-199.662961058371)) ;
#80533 = CARTESIAN_POINT('Ctrl Pts',(131.716759248505,-79.4381211627545,-200.025282931099)) ;
#80534 = CARTESIAN_POINT('Ctrl Pts',(132.079081121232,-79.3885117877545,-200.387604803826)) ;
#80535 = CARTESIAN_POINT('Ctrl Pts',(132.079081121232,-79.3389024127545,-200.900005310181)) ;
#80536 = CARTESIAN_POINT('Ctrl Pts',(132.079081121232,-79.2892930377545,-201.412405816536)) ;
#80537 = CARTESIAN_POINT('Ctrl Pts',(131.716759248505,-79.2396836627545,-201.774727689263)) ;
#80538 = CARTESIAN_POINT('Ctrl Pts',(131.354437375778,-79.1900742877545,-202.137049561991)) ;
#80539 = CARTESIAN_POINT('Ctrl Pts',(130.842036869422,-79.1404649127545,-202.137049561991)) ;
#80540 = CARTESIAN_POINT('Ctrl Pts',(130.329636363067,-79.0908555377545,-202.137049561991)) ;
#80541 = CARTESIAN_POINT('Ctrl Pts',(129.96731449034,-79.0412461627545,-201.774727689264)) ;
#80542 = CARTESIAN_POINT('Ctrl Pts',(129.604992617613,-78.9916367877545,-201.412405816536)) ;
#80543 = CARTESIAN_POINT('Ctrl Pts',(129.604992617613,-78.9420274127545,-200.900005310181)) ;
#80544 = CARTESIAN_POINT('Ctrl Pts',(129.604992617613,-78.8924180377545,-200.387604803826)) ;
#80545 = CARTESIAN_POINT('Ctrl Pts',(129.96731449034,-78.8428086627545,-200.025282931099)) ;
#80546 = CARTESIAN_POINT('Ctrl Pts',(130.329636363067,-78.7931992877545,-199.662961058372)) ;
#80547 = CARTESIAN_POINT('Ctrl Pts',(130.842036869422,-78.7435899127545,-199.662961058372)) ;
#80548 = CARTESIAN_POINT('Ctrl Pts',(131.354437375778,-78.6939805377545,-199.662961058371)) ;
#80549 = CARTESIAN_POINT('Ctrl Pts',(131.716759248505,-78.6443711627545,-200.025282931099)) ;
#80550 = CARTESIAN_POINT('Ctrl Pts',(132.079081121232,-78.5947617877545,-200.387604803826)) ;
#80551 = CARTESIAN_POINT('Ctrl Pts',(132.079081121232,-78.5451524127545,-200.900005310181)) ;
#80552 = CARTESIAN_POINT('Ctrl Pts',(132.079081121232,-78.4955430377545,-201.412405816536)) ;
#80553 = CARTESIAN_POINT('Ctrl Pts',(131.716759248505,-78.4459336627545,-201.774727689263)) ;
#80554 = CARTESIAN_POINT('Ctrl Pts',(131.354437375778,-78.3963242877545,-202.137049561991)) ;
#80555 = CARTESIAN_POINT('Ctrl Pts',(130.842036869422,-78.3467149127545,-202.137049561991)) ;
#80556 = CARTESIAN_POINT('Ctrl Pts',(130.329636363067,-78.2971055377545,-202.137049561991)) ;
#80557 = CARTESIAN_POINT('Ctrl Pts',(129.96731449034,-78.2474961627545,-201.774727689264)) ;
#80558 = CARTESIAN_POINT('Ctrl Pts',(129.604992617613,-78.1978867877545,-201.412405816536)) ;
#80559 = CARTESIAN_POINT('Ctrl Pts',(129.604992617613,-78.1482774127545,-200.900005310181)) ;
#80560 = CARTESIAN_POINT('Ctrl Pts',(129.604992617613,-78.0986680377545,-200.387604803826)) ;
#80561 = CARTESIAN_POINT('Ctrl Pts',(129.96731449034,-78.0490586627545,-200.025282931099)) ;
#80562 = CARTESIAN_POINT('Ctrl Pts',(130.329636363067,-77.9994492877545,-199.662961058372)) ;
#80563 = CARTESIAN_POINT('Ctrl Pts',(130.842036869422,-77.9498399127545,-199.662961058372)) ;
#80564 = CARTESIAN_POINT('Ctrl Pts',(131.354437375778,-77.9002305377545,-199.662961058371)) ;
#80565 = CARTESIAN_POINT('Ctrl Pts',(131.716759248505,-77.8506211627545,-200.025282931099)) ;
#80566 = CARTESIAN_POINT('Ctrl Pts',(132.079081121232,-77.8010117877545,-200.387604803826)) ;
#80567 = CARTESIAN_POINT('Ctrl Pts',(132.079081121232,-77.7514024127545,-200.900005310181)) ;
#80568 = CARTESIAN_POINT('Ctrl Pts',(132.079081121232,-77.7017930377545,-201.412405816536)) ;
#80569 = CARTESIAN_POINT('Ctrl Pts',(131.716759248505,-77.6521836627545,-201.774727689263)) ;
#80570 = CARTESIAN_POINT('Ctrl Pts',(131.354437375778,-77.6025742877545,-202.137049561991)) ;
#80571 = CARTESIAN_POINT('Ctrl Pts',(130.842036869422,-77.5529649127545,-202.137049561991)) ;
#80572 = CARTESIAN_POINT('Ctrl Pts',(130.329636363067,-77.5033555377545,-202.137049561991)) ;
#80573 = CARTESIAN_POINT('Ctrl Pts',(129.96731449034,-77.4537461627545,-201.774727689264)) ;
#80574 = CARTESIAN_POINT('Ctrl Pts',(129.604992617613,-77.4041367877545,-201.412405816536)) ;
#80575 = CARTESIAN_POINT('Ctrl Pts',(129.604992617613,-77.3545274127545,-200.900005310181)) ;
#80576 = CARTESIAN_POINT('Ctrl Pts',(129.604992617613,-77.3049180377545,-200.387604803826)) ;
#80577 = CARTESIAN_POINT('Ctrl Pts',(129.96731449034,-77.2553086627545,-200.025282931099)) ;
#80578 = CARTESIAN_POINT('Ctrl Pts',(130.329636363067,-77.2056992877545,-199.662961058372)) ;
#80579 = CARTESIAN_POINT('Ctrl Pts',(130.842036869422,-77.1560899127545,-199.662961058372)) ;
#80580 = CARTESIAN_POINT('Ctrl Pts',(131.354437375778,-77.1064805377545,-199.662961058371)) ;
#80581 = CARTESIAN_POINT('Ctrl Pts',(131.716759248505,-77.0568711627545,-200.025282931099)) ;
#80582 = CARTESIAN_POINT('Ctrl Pts',(132.079081121232,-77.0072617877545,-200.387604803826)) ;
#80583 = CARTESIAN_POINT('Ctrl Pts',(132.079081121232,-76.9576524127545,-200.900005310181)) ;
#80584 = CARTESIAN_POINT('Ctrl Pts',(132.079081121232,-76.9080430377545,-201.412405816536)) ;
#80585 = CARTESIAN_POINT('Ctrl Pts',(131.716759248505,-76.8584336627545,-201.774727689263)) ;
#80586 = CARTESIAN_POINT('Ctrl Pts',(131.354437375778,-76.8088242877545,-202.137049561991)) ;
#80587 = CARTESIAN_POINT('Ctrl Pts',(130.842036869422,-76.7592149127545,-202.137049561991)) ;
#80588 = CARTESIAN_POINT('Ctrl Pts',(130.329636363067,-76.7096055377545,-202.137049561991)) ;
#80589 = CARTESIAN_POINT('Ctrl Pts',(129.96731449034,-76.6599961627545,-201.774727689264)) ;
#80590 = CARTESIAN_POINT('Ctrl Pts',(129.604992617613,-76.6103867877545,-201.412405816536)) ;
#80591 = CARTESIAN_POINT('Ctrl Pts',(129.604992617613,-76.5607774127545,-200.900005310181)) ;
#80592 = CARTESIAN_POINT('Ctrl Pts',(129.604992617613,-76.5111680377545,-200.387604803826)) ;
#80593 = CARTESIAN_POINT('Ctrl Pts',(129.96731449034,-76.4615586627545,-200.025282931099)) ;
#80594 = CARTESIAN_POINT('Ctrl Pts',(130.329636363067,-76.4119492877545,-199.662961058372)) ;
#80595 = CARTESIAN_POINT('Ctrl Pts',(130.842036869422,-76.3623399127545,-199.662961058372)) ;
#80596 = CARTESIAN_POINT('Ctrl Pts',(131.354437375778,-76.3127305377545,-199.662961058371)) ;
#80597 = CARTESIAN_POINT('Ctrl Pts',(131.716759248505,-76.2631211627545,-200.025282931099)) ;
#80598 = CARTESIAN_POINT('Ctrl Pts',(132.079081121232,-76.2135117877545,-200.387604803826)) ;
#80599 = CARTESIAN_POINT('Ctrl Pts',(132.079081121232,-76.1639024127545,-200.900005310181)) ;
#80600 = CARTESIAN_POINT('Ctrl Pts',(132.079081121232,-76.1142930377545,-201.412405816536)) ;
#80601 = CARTESIAN_POINT('Ctrl Pts',(131.716759248505,-76.0646836627545,-201.774727689263)) ;
#80602 = CARTESIAN_POINT('Ctrl Pts',(131.354437375778,-76.0150742877545,-202.137049561991)) ;
#80603 = CARTESIAN_POINT('Ctrl Pts',(130.842036869422,-75.9654649127545,-202.137049561991)) ;
#80604 = CARTESIAN_POINT('Ctrl Pts',(130.329636363067,-75.9158555377545,-202.137049561991)) ;
#80605 = CARTESIAN_POINT('Ctrl Pts',(129.96731449034,-75.8662461627545,-201.774727689264)) ;
#80606 = CARTESIAN_POINT('Ctrl Pts',(129.604992617613,-75.8166367877545,-201.412405816536)) ;
#80607 = CARTESIAN_POINT('Ctrl Pts',(129.604992617613,-75.7670274127545,-200.900005310181)) ;
#80608 = CARTESIAN_POINT('Ctrl Pts',(129.604992617613,-75.7174180377545,-200.387604803826)) ;
#80609 = CARTESIAN_POINT('Ctrl Pts',(129.96731449034,-75.6678086627545,-200.025282931099)) ;
#80610 = CARTESIAN_POINT('Ctrl Pts',(130.329636363067,-75.6181992877545,-199.662961058372)) ;
#80611 = CARTESIAN_POINT('Ctrl Pts',(130.842036869422,-75.5685899127545,-199.662961058372)) ;
#80612 = CARTESIAN_POINT('Ctrl Pts',(131.354437375778,-75.5189805377545,-199.662961058371)) ;
#80613 = CARTESIAN_POINT('Ctrl Pts',(131.716759248505,-75.4693711627545,-200.025282931099)) ;
#80614 = CARTESIAN_POINT('Ctrl Pts',(132.079081121232,-75.4197617877545,-200.387604803826)) ;
#80615 = CARTESIAN_POINT('Ctrl Pts',(132.079081121232,-75.3701524127545,-200.900005310181)) ;
#80616 = CARTESIAN_POINT('Ctrl Pts',(132.079081121232,-75.3205430377545,-201.412405816536)) ;
#80617 = CARTESIAN_POINT('Ctrl Pts',(131.716759248505,-75.2709336627545,-201.774727689263)) ;
#80618 = CARTESIAN_POINT('Ctrl Pts',(131.354437375778,-75.2213242877545,-202.137049561991)) ;
#80619 = CARTESIAN_POINT('Ctrl Pts',(130.842036869422,-75.1717149127545,-202.137049561991)) ;
#80620 = CARTESIAN_POINT('Ctrl Pts',(130.329636363067,-75.1221055377545,-202.137049561991)) ;
#80621 = CARTESIAN_POINT('Ctrl Pts',(129.96731449034,-75.0724961627545,-201.774727689264)) ;
#80622 = CARTESIAN_POINT('Ctrl Pts',(129.604992617613,-75.0228867877545,-201.412405816536)) ;
#80623 = CARTESIAN_POINT('Ctrl Pts',(129.604992617613,-74.9732774127545,-200.900005310181)) ;
#80624 = CARTESIAN_POINT('Ctrl Pts',(129.604992617613,-74.9236680377545,-200.387604803826)) ;
#80625 = CARTESIAN_POINT('Ctrl Pts',(129.96731449034,-74.8740586627545,-200.025282931099)) ;
#80626 = CARTESIAN_POINT('Ctrl Pts',(130.329636363067,-74.8244492877545,-199.662961058372)) ;
#80627 = CARTESIAN_POINT('Ctrl Pts',(130.842036869422,-74.7748399127545,-199.662961058372)) ;
#80628 = CARTESIAN_POINT('Ctrl Pts',(131.354437375778,-74.7252305377545,-199.662961058371)) ;
#80629 = CARTESIAN_POINT('Ctrl Pts',(131.716759248505,-74.6756211627545,-200.025282931099)) ;
#80630 = CARTESIAN_POINT('Ctrl Pts',(132.079081121232,-74.6260117877545,-200.387604803826)) ;
#80631 = CARTESIAN_POINT('Ctrl Pts',(132.079081121232,-74.5764024127545,-200.900005310181)) ;
#80632 = CARTESIAN_POINT('Ctrl Pts',(132.079081121232,-74.5267930377545,-201.412405816536)) ;
#80633 = CARTESIAN_POINT('Ctrl Pts',(131.716759248505,-74.4771836627545,-201.774727689263)) ;
#80634 = CARTESIAN_POINT('Ctrl Pts',(131.354437375778,-74.4275742877545,-202.137049561991)) ;
#80635 = CARTESIAN_POINT('Ctrl Pts',(130.842036869422,-74.3779649127545,-202.137049561991)) ;
#80636 = CARTESIAN_POINT('Ctrl Pts',(130.329636363067,-74.3283555377545,-202.137049561991)) ;
#80637 = CARTESIAN_POINT('Ctrl Pts',(129.96731449034,-74.2787461627545,-201.774727689264)) ;
#80638 = CARTESIAN_POINT('Ctrl Pts',(129.604992617613,-74.2291367877545,-201.412405816536)) ;
#80639 = CARTESIAN_POINT('Ctrl Pts',(129.604992617613,-74.1795274127545,-200.900005310181)) ;
#80640 = CARTESIAN_POINT('Ctrl Pts',(129.604992617613,-74.1299180377545,-200.387604803826)) ;
#80641 = CARTESIAN_POINT('Ctrl Pts',(129.96731449034,-74.0803086627545,-200.025282931099)) ;
#80642 = CARTESIAN_POINT('Ctrl Pts',(130.329636363067,-74.0306992877545,-199.662961058372)) ;
#80643 = CARTESIAN_POINT('Ctrl Pts',(130.842036869422,-73.9810899127545,-199.662961058372)) ;
#80644 = CARTESIAN_POINT('Ctrl Pts',(131.354437375778,-73.9314805377545,-199.662961058371)) ;
#80645 = CARTESIAN_POINT('Ctrl Pts',(131.716759248505,-73.8818711627545,-200.025282931099)) ;
#80646 = CARTESIAN_POINT('Ctrl Pts',(132.079081121232,-73.8322617877545,-200.387604803826)) ;
#80647 = CARTESIAN_POINT('Ctrl Pts',(132.079081121232,-73.7826524127545,-200.900005310181)) ;
#80648 = CARTESIAN_POINT('Ctrl Pts',(132.594659680647,-81.224071832821,-200.900005310181)) ;
#80649 = CARTESIAN_POINT('Ctrl Pts',(132.594659680647,-81.174462457821,-201.625965448315)) ;
#80650 = CARTESIAN_POINT('Ctrl Pts',(132.081328344101,-81.124853082821,-202.13929678486)) ;
#80651 = CARTESIAN_POINT('Ctrl Pts',(131.567997007556,-81.075243707821,-202.652628121405)) ;
#80652 = CARTESIAN_POINT('Ctrl Pts',(130.842036869422,-81.025634332821,-202.652628121405)) ;
#80653 = CARTESIAN_POINT('Ctrl Pts',(130.116076731289,-80.976024957821,-202.652628121405)) ;
#80654 = CARTESIAN_POINT('Ctrl Pts',(129.602745394743,-80.926415582821,-202.13929678486)) ;
#80655 = CARTESIAN_POINT('Ctrl Pts',(129.089414058198,-80.876806207821,-201.625965448315)) ;
#80656 = CARTESIAN_POINT('Ctrl Pts',(129.089414058198,-80.827196832821,-200.900005310181)) ;
#80657 = CARTESIAN_POINT('Ctrl Pts',(129.089414058198,-80.777587457821,-200.174045172048)) ;
#80658 = CARTESIAN_POINT('Ctrl Pts',(129.602745394743,-80.727978082821,-199.660713835502)) ;
#80659 = CARTESIAN_POINT('Ctrl Pts',(130.116076731289,-80.678368707821,-199.147382498957)) ;
#80660 = CARTESIAN_POINT('Ctrl Pts',(130.842036869422,-80.628759332821,-199.147382498957)) ;
#80661 = CARTESIAN_POINT('Ctrl Pts',(131.567997007556,-80.579149957821,-199.147382498957)) ;
#80662 = CARTESIAN_POINT('Ctrl Pts',(132.081328344101,-80.529540582821,-199.660713835502)) ;
#80663 = CARTESIAN_POINT('Ctrl Pts',(132.594659680647,-80.479931207821,-200.174045172047)) ;
#80664 = CARTESIAN_POINT('Ctrl Pts',(132.594659680647,-80.430321832821,-200.900005310181)) ;
#80665 = CARTESIAN_POINT('Ctrl Pts',(132.594659680647,-80.380712457821,-201.625965448315)) ;
#80666 = CARTESIAN_POINT('Ctrl Pts',(132.081328344101,-80.331103082821,-202.13929678486)) ;
#80667 = CARTESIAN_POINT('Ctrl Pts',(131.567997007556,-80.281493707821,-202.652628121405)) ;
#80668 = CARTESIAN_POINT('Ctrl Pts',(130.842036869422,-80.231884332821,-202.652628121405)) ;
#80669 = CARTESIAN_POINT('Ctrl Pts',(130.116076731289,-80.182274957821,-202.652628121405)) ;
#80670 = CARTESIAN_POINT('Ctrl Pts',(129.602745394743,-80.132665582821,-202.13929678486)) ;
#80671 = CARTESIAN_POINT('Ctrl Pts',(129.089414058198,-80.083056207821,-201.625965448315)) ;
#80672 = CARTESIAN_POINT('Ctrl Pts',(129.089414058198,-80.033446832821,-200.900005310181)) ;
#80673 = CARTESIAN_POINT('Ctrl Pts',(129.089414058198,-79.983837457821,-200.174045172048)) ;
#80674 = CARTESIAN_POINT('Ctrl Pts',(129.602745394743,-79.934228082821,-199.660713835502)) ;
#80675 = CARTESIAN_POINT('Ctrl Pts',(130.116076731289,-79.884618707821,-199.147382498957)) ;
#80676 = CARTESIAN_POINT('Ctrl Pts',(130.842036869422,-79.835009332821,-199.147382498957)) ;
#80677 = CARTESIAN_POINT('Ctrl Pts',(131.567997007556,-79.785399957821,-199.147382498957)) ;
#80678 = CARTESIAN_POINT('Ctrl Pts',(132.081328344101,-79.735790582821,-199.660713835502)) ;
#80679 = CARTESIAN_POINT('Ctrl Pts',(132.594659680647,-79.686181207821,-200.174045172047)) ;
#80680 = CARTESIAN_POINT('Ctrl Pts',(132.594659680647,-79.636571832821,-200.900005310181)) ;
#80681 = CARTESIAN_POINT('Ctrl Pts',(132.594659680647,-79.586962457821,-201.625965448315)) ;
#80682 = CARTESIAN_POINT('Ctrl Pts',(132.081328344101,-79.537353082821,-202.13929678486)) ;
#80683 = CARTESIAN_POINT('Ctrl Pts',(131.567997007556,-79.487743707821,-202.652628121405)) ;
#80684 = CARTESIAN_POINT('Ctrl Pts',(130.842036869422,-79.438134332821,-202.652628121405)) ;
#80685 = CARTESIAN_POINT('Ctrl Pts',(130.116076731289,-79.388524957821,-202.652628121405)) ;
#80686 = CARTESIAN_POINT('Ctrl Pts',(129.602745394743,-79.338915582821,-202.13929678486)) ;
#80687 = CARTESIAN_POINT('Ctrl Pts',(129.089414058198,-79.289306207821,-201.625965448315)) ;
#80688 = CARTESIAN_POINT('Ctrl Pts',(129.089414058198,-79.239696832821,-200.900005310181)) ;
#80689 = CARTESIAN_POINT('Ctrl Pts',(129.089414058198,-79.190087457821,-200.174045172048)) ;
#80690 = CARTESIAN_POINT('Ctrl Pts',(129.602745394743,-79.140478082821,-199.660713835502)) ;
#80691 = CARTESIAN_POINT('Ctrl Pts',(130.116076731289,-79.090868707821,-199.147382498957)) ;
#80692 = CARTESIAN_POINT('Ctrl Pts',(130.842036869422,-79.041259332821,-199.147382498957)) ;
#80693 = CARTESIAN_POINT('Ctrl Pts',(131.567997007556,-78.991649957821,-199.147382498957)) ;
#80694 = CARTESIAN_POINT('Ctrl Pts',(132.081328344101,-78.942040582821,-199.660713835502)) ;
#80695 = CARTESIAN_POINT('Ctrl Pts',(132.594659680647,-78.892431207821,-200.174045172047)) ;
#80696 = CARTESIAN_POINT('Ctrl Pts',(132.594659680647,-78.842821832821,-200.900005310181)) ;
#80697 = CARTESIAN_POINT('Ctrl Pts',(132.594659680647,-78.793212457821,-201.625965448315)) ;
#80698 = CARTESIAN_POINT('Ctrl Pts',(132.081328344101,-78.743603082821,-202.13929678486)) ;
#80699 = CARTESIAN_POINT('Ctrl Pts',(131.567997007556,-78.693993707821,-202.652628121405)) ;
#80700 = CARTESIAN_POINT('Ctrl Pts',(130.842036869422,-78.644384332821,-202.652628121405)) ;
#80701 = CARTESIAN_POINT('Ctrl Pts',(130.116076731289,-78.594774957821,-202.652628121405)) ;
#80702 = CARTESIAN_POINT('Ctrl Pts',(129.602745394743,-78.545165582821,-202.13929678486)) ;
#80703 = CARTESIAN_POINT('Ctrl Pts',(129.089414058198,-78.495556207821,-201.625965448315)) ;
#80704 = CARTESIAN_POINT('Ctrl Pts',(129.089414058198,-78.445946832821,-200.900005310181)) ;
#80705 = CARTESIAN_POINT('Ctrl Pts',(129.089414058198,-78.396337457821,-200.174045172048)) ;
#80706 = CARTESIAN_POINT('Ctrl Pts',(129.602745394743,-78.346728082821,-199.660713835502)) ;
#80707 = CARTESIAN_POINT('Ctrl Pts',(130.116076731289,-78.297118707821,-199.147382498957)) ;
#80708 = CARTESIAN_POINT('Ctrl Pts',(130.842036869422,-78.247509332821,-199.147382498957)) ;
#80709 = CARTESIAN_POINT('Ctrl Pts',(131.567997007556,-78.197899957821,-199.147382498957)) ;
#80710 = CARTESIAN_POINT('Ctrl Pts',(132.081328344101,-78.148290582821,-199.660713835502)) ;
#80711 = CARTESIAN_POINT('Ctrl Pts',(132.594659680647,-78.098681207821,-200.174045172047)) ;
#80712 = CARTESIAN_POINT('Ctrl Pts',(132.594659680647,-78.049071832821,-200.900005310181)) ;
#80713 = CARTESIAN_POINT('Ctrl Pts',(132.594659680647,-77.999462457821,-201.625965448315)) ;
#80714 = CARTESIAN_POINT('Ctrl Pts',(132.081328344101,-77.949853082821,-202.13929678486)) ;
#80715 = CARTESIAN_POINT('Ctrl Pts',(131.567997007556,-77.900243707821,-202.652628121405)) ;
#80716 = CARTESIAN_POINT('Ctrl Pts',(130.842036869422,-77.850634332821,-202.652628121405)) ;
#80717 = CARTESIAN_POINT('Ctrl Pts',(130.116076731289,-77.801024957821,-202.652628121405)) ;
#80718 = CARTESIAN_POINT('Ctrl Pts',(129.602745394743,-77.751415582821,-202.13929678486)) ;
#80719 = CARTESIAN_POINT('Ctrl Pts',(129.089414058198,-77.701806207821,-201.625965448315)) ;
#80720 = CARTESIAN_POINT('Ctrl Pts',(129.089414058198,-77.652196832821,-200.900005310181)) ;
#80721 = CARTESIAN_POINT('Ctrl Pts',(129.089414058198,-77.602587457821,-200.174045172048)) ;
#80722 = CARTESIAN_POINT('Ctrl Pts',(129.602745394743,-77.552978082821,-199.660713835502)) ;
#80723 = CARTESIAN_POINT('Ctrl Pts',(130.116076731289,-77.503368707821,-199.147382498957)) ;
#80724 = CARTESIAN_POINT('Ctrl Pts',(130.842036869422,-77.453759332821,-199.147382498957)) ;
#80725 = CARTESIAN_POINT('Ctrl Pts',(131.567997007556,-77.404149957821,-199.147382498957)) ;
#80726 = CARTESIAN_POINT('Ctrl Pts',(132.081328344101,-77.354540582821,-199.660713835502)) ;
#80727 = CARTESIAN_POINT('Ctrl Pts',(132.594659680647,-77.304931207821,-200.174045172047)) ;
#80728 = CARTESIAN_POINT('Ctrl Pts',(132.594659680647,-77.255321832821,-200.900005310181)) ;
#80729 = CARTESIAN_POINT('Ctrl Pts',(132.594659680647,-77.205712457821,-201.625965448315)) ;
#80730 = CARTESIAN_POINT('Ctrl Pts',(132.081328344101,-77.156103082821,-202.13929678486)) ;
#80731 = CARTESIAN_POINT('Ctrl Pts',(131.567997007556,-77.106493707821,-202.652628121405)) ;
#80732 = CARTESIAN_POINT('Ctrl Pts',(130.842036869422,-77.056884332821,-202.652628121405)) ;
#80733 = CARTESIAN_POINT('Ctrl Pts',(130.116076731289,-77.007274957821,-202.652628121405)) ;
#80734 = CARTESIAN_POINT('Ctrl Pts',(129.602745394743,-76.957665582821,-202.13929678486)) ;
#80735 = CARTESIAN_POINT('Ctrl Pts',(129.089414058198,-76.908056207821,-201.625965448315)) ;
#80736 = CARTESIAN_POINT('Ctrl Pts',(129.089414058198,-76.858446832821,-200.900005310181)) ;
#80737 = CARTESIAN_POINT('Ctrl Pts',(129.089414058198,-76.808837457821,-200.174045172048)) ;
#80738 = CARTESIAN_POINT('Ctrl Pts',(129.602745394743,-76.759228082821,-199.660713835502)) ;
#80739 = CARTESIAN_POINT('Ctrl Pts',(130.116076731289,-76.709618707821,-199.147382498957)) ;
#80740 = CARTESIAN_POINT('Ctrl Pts',(130.842036869422,-76.660009332821,-199.147382498957)) ;
#80741 = CARTESIAN_POINT('Ctrl Pts',(131.567997007556,-76.610399957821,-199.147382498957)) ;
#80742 = CARTESIAN_POINT('Ctrl Pts',(132.081328344101,-76.560790582821,-199.660713835502)) ;
#80743 = CARTESIAN_POINT('Ctrl Pts',(132.594659680647,-76.511181207821,-200.174045172047)) ;
#80744 = CARTESIAN_POINT('Ctrl Pts',(132.594659680647,-76.461571832821,-200.900005310181)) ;
#80745 = CARTESIAN_POINT('Ctrl Pts',(132.594659680647,-76.411962457821,-201.625965448315)) ;
#80746 = CARTESIAN_POINT('Ctrl Pts',(132.081328344101,-76.362353082821,-202.13929678486)) ;
#80747 = CARTESIAN_POINT('Ctrl Pts',(131.567997007556,-76.312743707821,-202.652628121405)) ;
#80748 = CARTESIAN_POINT('Ctrl Pts',(130.842036869422,-76.263134332821,-202.652628121405)) ;
#80749 = CARTESIAN_POINT('Ctrl Pts',(130.116076731289,-76.213524957821,-202.652628121405)) ;
#80750 = CARTESIAN_POINT('Ctrl Pts',(129.602745394743,-76.163915582821,-202.13929678486)) ;
#80751 = CARTESIAN_POINT('Ctrl Pts',(129.089414058198,-76.114306207821,-201.625965448315)) ;
#80752 = CARTESIAN_POINT('Ctrl Pts',(129.089414058198,-76.064696832821,-200.900005310181)) ;
#80753 = CARTESIAN_POINT('Ctrl Pts',(129.089414058198,-76.015087457821,-200.174045172048)) ;
#80754 = CARTESIAN_POINT('Ctrl Pts',(129.602745394743,-75.965478082821,-199.660713835502)) ;
#80755 = CARTESIAN_POINT('Ctrl Pts',(130.116076731289,-75.915868707821,-199.147382498957)) ;
#80756 = CARTESIAN_POINT('Ctrl Pts',(130.842036869422,-75.866259332821,-199.147382498957)) ;
#80757 = CARTESIAN_POINT('Ctrl Pts',(131.567997007556,-75.816649957821,-199.147382498957)) ;
#80758 = CARTESIAN_POINT('Ctrl Pts',(132.081328344101,-75.767040582821,-199.660713835502)) ;
#80759 = CARTESIAN_POINT('Ctrl Pts',(132.594659680647,-75.717431207821,-200.174045172047)) ;
#80760 = CARTESIAN_POINT('Ctrl Pts',(132.594659680647,-75.667821832821,-200.900005310181)) ;
#80761 = CARTESIAN_POINT('Ctrl Pts',(132.594659680647,-75.618212457821,-201.625965448315)) ;
#80762 = CARTESIAN_POINT('Ctrl Pts',(132.081328344101,-75.568603082821,-202.13929678486)) ;
#80763 = CARTESIAN_POINT('Ctrl Pts',(131.567997007556,-75.518993707821,-202.652628121405)) ;
#80764 = CARTESIAN_POINT('Ctrl Pts',(130.842036869422,-75.469384332821,-202.652628121405)) ;
#80765 = CARTESIAN_POINT('Ctrl Pts',(130.116076731289,-75.419774957821,-202.652628121405)) ;
#80766 = CARTESIAN_POINT('Ctrl Pts',(129.602745394743,-75.370165582821,-202.13929678486)) ;
#80767 = CARTESIAN_POINT('Ctrl Pts',(129.089414058198,-75.320556207821,-201.625965448315)) ;
#80768 = CARTESIAN_POINT('Ctrl Pts',(129.089414058198,-75.270946832821,-200.900005310181)) ;
#80769 = CARTESIAN_POINT('Ctrl Pts',(129.089414058198,-75.221337457821,-200.174045172048)) ;
#80770 = CARTESIAN_POINT('Ctrl Pts',(129.602745394743,-75.171728082821,-199.660713835502)) ;
#80771 = CARTESIAN_POINT('Ctrl Pts',(130.116076731289,-75.122118707821,-199.147382498957)) ;
#80772 = CARTESIAN_POINT('Ctrl Pts',(130.842036869422,-75.072509332821,-199.147382498957)) ;
#80773 = CARTESIAN_POINT('Ctrl Pts',(131.567997007556,-75.022899957821,-199.147382498957)) ;
#80774 = CARTESIAN_POINT('Ctrl Pts',(132.081328344101,-74.973290582821,-199.660713835502)) ;
#80775 = CARTESIAN_POINT('Ctrl Pts',(132.594659680647,-74.923681207821,-200.174045172047)) ;
#80776 = CARTESIAN_POINT('Ctrl Pts',(132.594659680647,-74.874071832821,-200.900005310181)) ;
#80777 = CARTESIAN_POINT('Ctrl Pts',(132.594659680647,-74.824462457821,-201.625965448315)) ;
#80778 = CARTESIAN_POINT('Ctrl Pts',(132.081328344101,-74.774853082821,-202.13929678486)) ;
#80779 = CARTESIAN_POINT('Ctrl Pts',(131.567997007556,-74.725243707821,-202.652628121405)) ;
#80780 = CARTESIAN_POINT('Ctrl Pts',(130.842036869422,-74.675634332821,-202.652628121405)) ;
#80781 = CARTESIAN_POINT('Ctrl Pts',(130.116076731289,-74.626024957821,-202.652628121405)) ;
#80782 = CARTESIAN_POINT('Ctrl Pts',(129.602745394743,-74.576415582821,-202.13929678486)) ;
#80783 = CARTESIAN_POINT('Ctrl Pts',(129.089414058198,-74.526806207821,-201.625965448315)) ;
#80784 = CARTESIAN_POINT('Ctrl Pts',(129.089414058198,-74.477196832821,-200.900005310181)) ;
#80785 = CARTESIAN_POINT('Ctrl Pts',(129.089414058198,-74.427587457821,-200.174045172048)) ;
#80786 = CARTESIAN_POINT('Ctrl Pts',(129.602745394743,-74.377978082821,-199.660713835502)) ;
#80787 = CARTESIAN_POINT('Ctrl Pts',(130.116076731289,-74.328368707821,-199.147382498957)) ;
#80788 = CARTESIAN_POINT('Ctrl Pts',(130.842036869422,-74.278759332821,-199.147382498957)) ;
#80789 = CARTESIAN_POINT('Ctrl Pts',(131.567997007556,-74.229149957821,-199.147382498957)) ;
#80790 = CARTESIAN_POINT('Ctrl Pts',(132.081328344101,-74.179540582821,-199.660713835502)) ;
#80791 = CARTESIAN_POINT('Ctrl Pts',(132.594659680647,-74.129931207821,-200.174045172047)) ;
#80792 = CARTESIAN_POINT('Ctrl Pts',(132.594659680647,-74.080321832821,-200.900005310181)) ;
#80793 = CARTESIAN_POINT('',(406.738532935575,438.630519719759,41.1573672409939)) ;
#80794 = CARTESIAN_POINT('',(406.738532935568,400.630519719759,41.1573672409939)) ;
#80795 = CARTESIAN_POINT('',(406.738532935577,448.130519719759,41.1573672409939)) ;
#80796 = CARTESIAN_POINT('',(406.738532935582,476.630519719759,41.1573672409939)) ;
#80797 = CARTESIAN_POINT('',(406.738532935578,457.630519719759,41.1573672409939)) ;
#80798 = CARTESIAN_POINT('',(406.73853293558,467.130519719759,41.1573672409939)) ;
#80799 = CARTESIAN_POINT('',(406.738532935573,429.130519719759,41.1573672409939)) ;
#80800 = CARTESIAN_POINT('',(406.738532935572,419.630519719759,41.1573672409939)) ;
#80801 = CARTESIAN_POINT('',(406.73853293557,410.130519719759,41.1573672409939)) ;
#80802 = CARTESIAN_POINT('',(0.,0.,0.)) ;
#80803 = CARTESIAN_POINT('',(0.,0.,0.)) ;
#80804 = CARTESIAN_POINT('Ctrl Pts',(127.032036789131,-75.3686363338475,-197.090005390471)) ;
#80805 = CARTESIAN_POINT('Ctrl Pts',(123.222036869419,-75.3686363338475,-200.90000547076)) ;
#80806 = CARTESIAN_POINT('Ctrl Pts',(127.032036949709,-75.3686363338475,-204.710005390471)) ;
#80807 = CARTESIAN_POINT('Ctrl Pts',(130.842037029998,-75.3686363338475,-208.520005310182)) ;
#80808 = CARTESIAN_POINT('Ctrl Pts',(134.652036949709,-75.3686363338475,-204.710005229893)) ;
#80809 = CARTESIAN_POINT('Ctrl Pts',(138.46203686942,-75.3686363338475,-200.900005149604)) ;
#80810 = CARTESIAN_POINT('Ctrl Pts',(134.652036789131,-75.3686363338475,-197.090005229893)) ;
#80811 = CARTESIAN_POINT('Ctrl Pts',(130.842036708842,-75.3686363338475,-193.280005310182)) ;
#80812 = CARTESIAN_POINT('Ctrl Pts',(127.032036789131,-75.3686363338475,-197.090005390471)) ;
#80813 = CARTESIAN_POINT('Ctrl Pts',(127.032036789131,-75.1781363338475,-197.090005390471)) ;
#80814 = CARTESIAN_POINT('Ctrl Pts',(123.222036869419,-75.1781363338475,-200.90000547076)) ;
#80815 = CARTESIAN_POINT('Ctrl Pts',(127.032036949709,-75.1781363338475,-204.710005390471)) ;
#80816 = CARTESIAN_POINT('Ctrl Pts',(130.842037029998,-75.1781363338475,-208.520005310182)) ;
#80817 = CARTESIAN_POINT('Ctrl Pts',(134.652036949709,-75.1781363338475,-204.710005229893)) ;
#80818 = CARTESIAN_POINT('Ctrl Pts',(138.46203686942,-75.1781363338475,-200.900005149604)) ;
#80819 = CARTESIAN_POINT('Ctrl Pts',(134.652036789131,-75.1781363338475,-197.090005229893)) ;
#80820 = CARTESIAN_POINT('Ctrl Pts',(130.842036708842,-75.1781363338475,-193.280005310182)) ;
#80821 = CARTESIAN_POINT('Ctrl Pts',(127.032036789131,-75.1781363338475,-197.090005390471)) ;
#80822 = CARTESIAN_POINT('Ctrl Pts',(127.481049604646,-75.1781363338475,-197.539018187062)) ;
#80823 = CARTESIAN_POINT('Ctrl Pts',(124.120062481526,-75.1781363338475,-200.900005451836)) ;
#80824 = CARTESIAN_POINT('Ctrl Pts',(127.4810497463,-75.1781363338475,-204.260992574956)) ;
#80825 = CARTESIAN_POINT('Ctrl Pts',(130.842037011073,-75.1781363338475,-207.621979698075)) ;
#80826 = CARTESIAN_POINT('Ctrl Pts',(134.203024134193,-75.1781363338475,-204.260992433302)) ;
#80827 = CARTESIAN_POINT('Ctrl Pts',(137.564011257313,-75.1781363338475,-200.900005168529)) ;
#80828 = CARTESIAN_POINT('Ctrl Pts',(134.203023992539,-75.1781363338475,-197.539018045409)) ;
#80829 = CARTESIAN_POINT('Ctrl Pts',(130.842036727766,-75.1781363338475,-194.178030922289)) ;
#80830 = CARTESIAN_POINT('Ctrl Pts',(127.481049604646,-75.1781363338475,-197.539018187062)) ;
#80831 = CARTESIAN_POINT('',(128.000141404111,-75.1781363338475,-197.090005310182)) ;
#80832 = CARTESIAN_POINT('',(127.260059362794,-75.2257613351713,-197.09000531248)) ;
#80833 = CARTESIAN_POINT('Ctrl Pts',(128.000141404111,-75.1781363338475,-197.090005310182)) ;
#80834 = CARTESIAN_POINT('Ctrl Pts',(127.875189846825,-75.1781363338475,-197.090005310182)) ;
#80835 = CARTESIAN_POINT('Ctrl Pts',(127.74042967657,-75.1801139619557,-197.090005310065)) ;
#80836 = CARTESIAN_POINT('Ctrl Pts',(127.489185117998,-75.1931618999273,-197.090005310065)) ;
#80837 = CARTESIAN_POINT('Ctrl Pts',(127.362906128424,-75.2046272926173,-197.090005310182)) ;
#80838 = CARTESIAN_POINT('Ctrl Pts',(127.260059363022,-75.2257613362829,-197.090005310182)) ;
#80839 = CARTESIAN_POINT('',(127.481049604646,-75.1781363338475,-197.539018187062)) ;
#80840 = CARTESIAN_POINT('Origin',(130.842036869419,-75.1781363338481,-200.900005310182)) ;
#80841 = CARTESIAN_POINT('',(127.144290007455,-75.2257613338475,-197.202258575173)) ;
#80842 = CARTESIAN_POINT('Ctrl Pts',(127.144290007455,-75.2257613338475,-197.202258575173)) ;
#80843 = CARTESIAN_POINT('Ctrl Pts',(127.2191254716,-75.1940113338475,-197.277094046379)) ;
#80844 = CARTESIAN_POINT('Ctrl Pts',(127.331378670518,-75.1781363338475,-197.389347250489)) ;
#80845 = CARTESIAN_POINT('Ctrl Pts',(127.481049604646,-75.1781363338475,-197.539018187062)) ;
#80846 = CARTESIAN_POINT('Origin',(130.842036960968,-75.225761372682,-200.90000540173)) ;
#80847 = CARTESIAN_POINT('Ctrl Pts',(127.032036789131,-75.3686363338475,-197.090005390471)) ;
#80848 = CARTESIAN_POINT('Ctrl Pts',(123.222036869419,-75.3686363338475,-200.90000547076)) ;
#80849 = CARTESIAN_POINT('Ctrl Pts',(127.032036949709,-75.3686363338475,-204.710005390471)) ;
#80850 = CARTESIAN_POINT('Ctrl Pts',(130.842037029998,-75.3686363338475,-208.520005310182)) ;
#80851 = CARTESIAN_POINT('Ctrl Pts',(134.652036949709,-75.3686363338475,-204.710005229893)) ;
#80852 = CARTESIAN_POINT('Ctrl Pts',(138.46203686942,-75.3686363338475,-200.900005149604)) ;
#80853 = CARTESIAN_POINT('Ctrl Pts',(134.652036789131,-75.3686363338475,-197.090005229893)) ;
#80854 = CARTESIAN_POINT('Ctrl Pts',(130.842036708842,-75.3686363338475,-193.280005310182)) ;
#80855 = CARTESIAN_POINT('Ctrl Pts',(127.032036789131,-75.3686363338475,-197.090005390471)) ;
#80856 = CARTESIAN_POINT('Ctrl Pts',(127.032036789131,-75.1781363338475,-197.090005390471)) ;
#80857 = CARTESIAN_POINT('Ctrl Pts',(123.222036869419,-75.1781363338475,-200.90000547076)) ;
#80858 = CARTESIAN_POINT('Ctrl Pts',(127.032036949709,-75.1781363338475,-204.710005390471)) ;
#80859 = CARTESIAN_POINT('Ctrl Pts',(130.842037029998,-75.1781363338475,-208.520005310182)) ;
#80860 = CARTESIAN_POINT('Ctrl Pts',(134.652036949709,-75.1781363338475,-204.710005229893)) ;
#80861 = CARTESIAN_POINT('Ctrl Pts',(138.46203686942,-75.1781363338475,-200.900005149604)) ;
#80862 = CARTESIAN_POINT('Ctrl Pts',(134.652036789131,-75.1781363338475,-197.090005229893)) ;
#80863 = CARTESIAN_POINT('Ctrl Pts',(130.842036708842,-75.1781363338475,-193.280005310182)) ;
#80864 = CARTESIAN_POINT('Ctrl Pts',(127.032036789131,-75.1781363338475,-197.090005390471)) ;
#80865 = CARTESIAN_POINT('Ctrl Pts',(127.481049604646,-75.1781363338475,-197.539018187062)) ;
#80866 = CARTESIAN_POINT('Ctrl Pts',(124.120062481526,-75.1781363338475,-200.900005451836)) ;
#80867 = CARTESIAN_POINT('Ctrl Pts',(127.4810497463,-75.1781363338475,-204.260992574956)) ;
#80868 = CARTESIAN_POINT('Ctrl Pts',(130.842037011073,-75.1781363338475,-207.621979698075)) ;
#80869 = CARTESIAN_POINT('Ctrl Pts',(134.203024134193,-75.1781363338475,-204.260992433302)) ;
#80870 = CARTESIAN_POINT('Ctrl Pts',(137.564011257313,-75.1781363338475,-200.900005168529)) ;
#80871 = CARTESIAN_POINT('Ctrl Pts',(134.203023992539,-75.1781363338475,-197.539018045409)) ;
#80872 = CARTESIAN_POINT('Ctrl Pts',(130.842036727766,-75.1781363338475,-194.178030922289)) ;
#80873 = CARTESIAN_POINT('Ctrl Pts',(127.481049604646,-75.1781363338475,-197.539018187062)) ;
#80874 = CARTESIAN_POINT('',(133.683932334728,-75.1781363338475,-204.710005310183)) ;
#80875 = CARTESIAN_POINT('',(134.424014363965,-75.2257613338475,-204.710005310183)) ;
#80876 = CARTESIAN_POINT('Ctrl Pts',(133.683932334728,-75.1781363338475,-204.710005310182)) ;
#80877 = CARTESIAN_POINT('Ctrl Pts',(133.808883889989,-75.1781363338475,-204.710005310182)) ;
#80878 = CARTESIAN_POINT('Ctrl Pts',(133.943644057601,-75.1801139618916,-204.710005310299)) ;
#80879 = CARTESIAN_POINT('Ctrl Pts',(134.194892600511,-75.193162106426,-204.710005310299)) ;
#80880 = CARTESIAN_POINT('Ctrl Pts',(134.321165640767,-75.2046268889911,-204.710005310182)) ;
#80881 = CARTESIAN_POINT('Ctrl Pts',(134.424014363965,-75.2257613338474,-204.710005310183)) ;
#80882 = CARTESIAN_POINT('',(134.652036869419,-75.1781363338475,-203.741900775492)) ;
#80883 = CARTESIAN_POINT('Origin',(130.84203686942,-75.1781363338476,-200.900005310182)) ;
#80884 = CARTESIAN_POINT('',(134.652036869419,-75.2257613338475,-204.481982804729)) ;
#80885 = CARTESIAN_POINT('Ctrl Pts',(134.652036869419,-75.2257613338474,-204.481982804729)) ;
#80886 = CARTESIAN_POINT('Ctrl Pts',(134.652036869419,-75.2046268889901,-204.379134081526)) ;
#80887 = CARTESIAN_POINT('Ctrl Pts',(134.652036869535,-75.1931621064255,-204.252861041264)) ;
#80888 = CARTESIAN_POINT('Ctrl Pts',(134.652036869535,-75.1801139618916,-204.001612498367)) ;
#80889 = CARTESIAN_POINT('Ctrl Pts',(134.652036869419,-75.1781363338475,-203.866852330753)) ;
#80890 = CARTESIAN_POINT('Ctrl Pts',(134.652036869419,-75.1781363338475,-203.741900775492)) ;
#80891 = CARTESIAN_POINT('Origin',(130.842036869419,-75.225761333849,-200.900005310182)) ;
#80892 = CARTESIAN_POINT('Ctrl Pts',(127.032036789131,-75.3686363338475,-197.090005390471)) ;
#80893 = CARTESIAN_POINT('Ctrl Pts',(123.222036869419,-75.3686363338475,-200.90000547076)) ;
#80894 = CARTESIAN_POINT('Ctrl Pts',(127.032036949709,-75.3686363338475,-204.710005390471)) ;
#80895 = CARTESIAN_POINT('Ctrl Pts',(130.842037029998,-75.3686363338475,-208.520005310182)) ;
#80896 = CARTESIAN_POINT('Ctrl Pts',(134.652036949709,-75.3686363338475,-204.710005229893)) ;
#80897 = CARTESIAN_POINT('Ctrl Pts',(138.46203686942,-75.3686363338475,-200.900005149604)) ;
#80898 = CARTESIAN_POINT('Ctrl Pts',(134.652036789131,-75.3686363338475,-197.090005229893)) ;
#80899 = CARTESIAN_POINT('Ctrl Pts',(130.842036708842,-75.3686363338475,-193.280005310182)) ;
#80900 = CARTESIAN_POINT('Ctrl Pts',(127.032036789131,-75.3686363338475,-197.090005390471)) ;
#80901 = CARTESIAN_POINT('Ctrl Pts',(127.032036789131,-75.1781363338475,-197.090005390471)) ;
#80902 = CARTESIAN_POINT('Ctrl Pts',(123.222036869419,-75.1781363338475,-200.90000547076)) ;
#80903 = CARTESIAN_POINT('Ctrl Pts',(127.032036949709,-75.1781363338475,-204.710005390471)) ;
#80904 = CARTESIAN_POINT('Ctrl Pts',(130.842037029998,-75.1781363338475,-208.520005310182)) ;
#80905 = CARTESIAN_POINT('Ctrl Pts',(134.652036949709,-75.1781363338475,-204.710005229893)) ;
#80906 = CARTESIAN_POINT('Ctrl Pts',(138.46203686942,-75.1781363338475,-200.900005149604)) ;
#80907 = CARTESIAN_POINT('Ctrl Pts',(134.652036789131,-75.1781363338475,-197.090005229893)) ;
#80908 = CARTESIAN_POINT('Ctrl Pts',(130.842036708842,-75.1781363338475,-193.280005310182)) ;
#80909 = CARTESIAN_POINT('Ctrl Pts',(127.032036789131,-75.1781363338475,-197.090005390471)) ;
#80910 = CARTESIAN_POINT('Ctrl Pts',(127.481049604646,-75.1781363338475,-197.539018187062)) ;
#80911 = CARTESIAN_POINT('Ctrl Pts',(124.120062481526,-75.1781363338475,-200.900005451836)) ;
#80912 = CARTESIAN_POINT('Ctrl Pts',(127.4810497463,-75.1781363338475,-204.260992574956)) ;
#80913 = CARTESIAN_POINT('Ctrl Pts',(130.842037011073,-75.1781363338475,-207.621979698075)) ;
#80914 = CARTESIAN_POINT('Ctrl Pts',(134.203024134193,-75.1781363338475,-204.260992433302)) ;
#80915 = CARTESIAN_POINT('Ctrl Pts',(137.564011257313,-75.1781363338475,-200.900005168529)) ;
#80916 = CARTESIAN_POINT('Ctrl Pts',(134.203023992539,-75.1781363338475,-197.539018045409)) ;
#80917 = CARTESIAN_POINT('Ctrl Pts',(130.842036727766,-75.1781363338475,-194.178030922289)) ;
#80918 = CARTESIAN_POINT('Ctrl Pts',(127.481049604646,-75.1781363338475,-197.539018187062)) ;
#80919 = CARTESIAN_POINT('',(127.03203686942,-75.1781363338475,-198.058109844872)) ;
#80920 = CARTESIAN_POINT('Origin',(130.84203686942,-75.1781363338475,-200.900005310182)) ;
#80921 = CARTESIAN_POINT('',(127.032036867121,-75.2257613325238,-197.318027827716)) ;
#80922 = CARTESIAN_POINT('Ctrl Pts',(127.03203686942,-75.2257613314121,-197.318027827487)) ;
#80923 = CARTESIAN_POINT('Ctrl Pts',(127.03203686942,-75.2046272023282,-197.420875019449)) ;
#80924 = CARTESIAN_POINT('Ctrl Pts',(127.032036869317,-75.1931624628046,-197.547145758675)) ;
#80925 = CARTESIAN_POINT('Ctrl Pts',(127.032036869317,-75.1801140186575,-197.798393987226)) ;
#80926 = CARTESIAN_POINT('Ctrl Pts',(127.03203686942,-75.1781363338475,-197.933156496317)) ;
#80927 = CARTESIAN_POINT('Ctrl Pts',(127.03203686942,-75.1781363338475,-198.058109844872)) ;
#80928 = CARTESIAN_POINT('Origin',(130.842036777871,-75.225761295013,-200.900005218634)) ;
#80929 = CARTESIAN_POINT('Ctrl Pts',(127.032036789131,-75.3686363338475,-197.090005390471)) ;
#80930 = CARTESIAN_POINT('Ctrl Pts',(123.222036869419,-75.3686363338475,-200.90000547076)) ;
#80931 = CARTESIAN_POINT('Ctrl Pts',(127.032036949709,-75.3686363338475,-204.710005390471)) ;
#80932 = CARTESIAN_POINT('Ctrl Pts',(130.842037029998,-75.3686363338475,-208.520005310182)) ;
#80933 = CARTESIAN_POINT('Ctrl Pts',(134.652036949709,-75.3686363338475,-204.710005229893)) ;
#80934 = CARTESIAN_POINT('Ctrl Pts',(138.46203686942,-75.3686363338475,-200.900005149604)) ;
#80935 = CARTESIAN_POINT('Ctrl Pts',(134.652036789131,-75.3686363338475,-197.090005229893)) ;
#80936 = CARTESIAN_POINT('Ctrl Pts',(130.842036708842,-75.3686363338475,-193.280005310182)) ;
#80937 = CARTESIAN_POINT('Ctrl Pts',(127.032036789131,-75.3686363338475,-197.090005390471)) ;
#80938 = CARTESIAN_POINT('Ctrl Pts',(127.032036789131,-75.1781363338475,-197.090005390471)) ;
#80939 = CARTESIAN_POINT('Ctrl Pts',(123.222036869419,-75.1781363338475,-200.90000547076)) ;
#80940 = CARTESIAN_POINT('Ctrl Pts',(127.032036949709,-75.1781363338475,-204.710005390471)) ;
#80941 = CARTESIAN_POINT('Ctrl Pts',(130.842037029998,-75.1781363338475,-208.520005310182)) ;
#80942 = CARTESIAN_POINT('Ctrl Pts',(134.652036949709,-75.1781363338475,-204.710005229893)) ;
#80943 = CARTESIAN_POINT('Ctrl Pts',(138.46203686942,-75.1781363338475,-200.900005149604)) ;
#80944 = CARTESIAN_POINT('Ctrl Pts',(134.652036789131,-75.1781363338475,-197.090005229893)) ;
#80945 = CARTESIAN_POINT('Ctrl Pts',(130.842036708842,-75.1781363338475,-193.280005310182)) ;
#80946 = CARTESIAN_POINT('Ctrl Pts',(127.032036789131,-75.1781363338475,-197.090005390471)) ;
#80947 = CARTESIAN_POINT('Ctrl Pts',(127.481049604646,-75.1781363338475,-197.539018187062)) ;
#80948 = CARTESIAN_POINT('Ctrl Pts',(124.120062481526,-75.1781363338475,-200.900005451836)) ;
#80949 = CARTESIAN_POINT('Ctrl Pts',(127.4810497463,-75.1781363338475,-204.260992574956)) ;
#80950 = CARTESIAN_POINT('Ctrl Pts',(130.842037011073,-75.1781363338475,-207.621979698075)) ;
#80951 = CARTESIAN_POINT('Ctrl Pts',(134.203024134193,-75.1781363338475,-204.260992433302)) ;
#80952 = CARTESIAN_POINT('Ctrl Pts',(137.564011257313,-75.1781363338475,-200.900005168529)) ;
#80953 = CARTESIAN_POINT('Ctrl Pts',(134.203023992539,-75.1781363338475,-197.539018045409)) ;
#80954 = CARTESIAN_POINT('Ctrl Pts',(130.842036727766,-75.1781363338475,-194.178030922289)) ;
#80955 = CARTESIAN_POINT('Ctrl Pts',(127.481049604646,-75.1781363338475,-197.539018187062)) ;
#80956 = CARTESIAN_POINT('',(127.032036869419,-75.1781363338475,-203.741900775491)) ;
#80957 = CARTESIAN_POINT('',(127.032036869419,-75.2257613338475,-204.481982804728)) ;
#80958 = CARTESIAN_POINT('Ctrl Pts',(127.032036869419,-75.1781363338475,-203.741900775491)) ;
#80959 = CARTESIAN_POINT('Ctrl Pts',(127.032036869419,-75.1781363338475,-203.866852330753)) ;
#80960 = CARTESIAN_POINT('Ctrl Pts',(127.032036869302,-75.1801139618916,-204.001612498365)) ;
#80961 = CARTESIAN_POINT('Ctrl Pts',(127.032036869302,-75.1931618993063,-204.252857053077)) ;
#80962 = CARTESIAN_POINT('Ctrl Pts',(127.032036869419,-75.2046272914575,-204.379136040093)) ;
#80963 = CARTESIAN_POINT('Ctrl Pts',(127.032036869418,-75.2257613338477,-204.481982804728)) ;
#80964 = CARTESIAN_POINT('',(128.000141404109,-75.1781363338475,-204.710005310182)) ;
#80965 = CARTESIAN_POINT('Origin',(130.84203686942,-75.1781363338476,-200.900005310182)) ;
#80966 = CARTESIAN_POINT('',(127.260059374872,-75.2257613338475,-204.710005310181)) ;
#80967 = CARTESIAN_POINT('Ctrl Pts',(127.260059374872,-75.2257613338476,-204.710005310181)) ;
#80968 = CARTESIAN_POINT('Ctrl Pts',(127.362904608918,-75.204627605979,-204.710005310181)) ;
#80969 = CARTESIAN_POINT('Ctrl Pts',(127.489181296476,-75.1931622563878,-204.710005310284)) ;
#80970 = CARTESIAN_POINT('Ctrl Pts',(127.740425541024,-75.1801140187322,-204.710005310284)) ;
#80971 = CARTESIAN_POINT('Ctrl Pts',(127.875188053195,-75.1781363338475,-204.710005310181)) ;
#80972 = CARTESIAN_POINT('Ctrl Pts',(128.000141404109,-75.1781363338475,-204.710005310181)) ;
#80973 = CARTESIAN_POINT('Origin',(130.842036869419,-75.2257613338505,-200.900005310183)) ;
#80974 = CARTESIAN_POINT('Ctrl Pts',(127.032036789131,-75.3686363338475,-197.090005390471)) ;
#80975 = CARTESIAN_POINT('Ctrl Pts',(123.222036869419,-75.3686363338475,-200.90000547076)) ;
#80976 = CARTESIAN_POINT('Ctrl Pts',(127.032036949709,-75.3686363338475,-204.710005390471)) ;
#80977 = CARTESIAN_POINT('Ctrl Pts',(130.842037029998,-75.3686363338475,-208.520005310182)) ;
#80978 = CARTESIAN_POINT('Ctrl Pts',(134.652036949709,-75.3686363338475,-204.710005229893)) ;
#80979 = CARTESIAN_POINT('Ctrl Pts',(138.46203686942,-75.3686363338475,-200.900005149604)) ;
#80980 = CARTESIAN_POINT('Ctrl Pts',(134.652036789131,-75.3686363338475,-197.090005229893)) ;
#80981 = CARTESIAN_POINT('Ctrl Pts',(130.842036708842,-75.3686363338475,-193.280005310182)) ;
#80982 = CARTESIAN_POINT('Ctrl Pts',(127.032036789131,-75.3686363338475,-197.090005390471)) ;
#80983 = CARTESIAN_POINT('Ctrl Pts',(127.032036789131,-75.1781363338475,-197.090005390471)) ;
#80984 = CARTESIAN_POINT('Ctrl Pts',(123.222036869419,-75.1781363338475,-200.90000547076)) ;
#80985 = CARTESIAN_POINT('Ctrl Pts',(127.032036949709,-75.1781363338475,-204.710005390471)) ;
#80986 = CARTESIAN_POINT('Ctrl Pts',(130.842037029998,-75.1781363338475,-208.520005310182)) ;
#80987 = CARTESIAN_POINT('Ctrl Pts',(134.652036949709,-75.1781363338475,-204.710005229893)) ;
#80988 = CARTESIAN_POINT('Ctrl Pts',(138.46203686942,-75.1781363338475,-200.900005149604)) ;
#80989 = CARTESIAN_POINT('Ctrl Pts',(134.652036789131,-75.1781363338475,-197.090005229893)) ;
#80990 = CARTESIAN_POINT('Ctrl Pts',(130.842036708842,-75.1781363338475,-193.280005310182)) ;
#80991 = CARTESIAN_POINT('Ctrl Pts',(127.032036789131,-75.1781363338475,-197.090005390471)) ;
#80992 = CARTESIAN_POINT('Ctrl Pts',(127.481049604646,-75.1781363338475,-197.539018187062)) ;
#80993 = CARTESIAN_POINT('Ctrl Pts',(124.120062481526,-75.1781363338475,-200.900005451836)) ;
#80994 = CARTESIAN_POINT('Ctrl Pts',(127.4810497463,-75.1781363338475,-204.260992574956)) ;
#80995 = CARTESIAN_POINT('Ctrl Pts',(130.842037011073,-75.1781363338475,-207.621979698075)) ;
#80996 = CARTESIAN_POINT('Ctrl Pts',(134.203024134193,-75.1781363338475,-204.260992433302)) ;
#80997 = CARTESIAN_POINT('Ctrl Pts',(137.564011257313,-75.1781363338475,-200.900005168529)) ;
#80998 = CARTESIAN_POINT('Ctrl Pts',(134.203023992539,-75.1781363338475,-197.539018045409)) ;
#80999 = CARTESIAN_POINT('Ctrl Pts',(130.842036727766,-75.1781363338475,-194.178030922289)) ;
#81000 = CARTESIAN_POINT('Ctrl Pts',(127.481049604646,-75.1781363338475,-197.539018187062)) ;
#81001 = CARTESIAN_POINT('',(134.65203686942,-75.1781363338475,-198.058109844874)) ;
#81002 = CARTESIAN_POINT('',(134.65203686942,-75.2257613338475,-197.318027815637)) ;
#81003 = CARTESIAN_POINT('Ctrl Pts',(134.65203686942,-75.1781363338475,-198.058109844874)) ;
#81004 = CARTESIAN_POINT('Ctrl Pts',(134.65203686942,-75.1781363338475,-197.93315649396)) ;
#81005 = CARTESIAN_POINT('Ctrl Pts',(134.652036869524,-75.1801140187322,-197.798393981794)) ;
#81006 = CARTESIAN_POINT('Ctrl Pts',(134.652036869524,-75.193162256388,-197.547149737234)) ;
#81007 = CARTESIAN_POINT('Ctrl Pts',(134.65203686942,-75.2046276059798,-197.420873049679)) ;
#81008 = CARTESIAN_POINT('Ctrl Pts',(134.65203686942,-75.2257613338474,-197.318027815637)) ;
#81009 = CARTESIAN_POINT('',(133.683932334729,-75.1781363338475,-197.090005310183)) ;
#81010 = CARTESIAN_POINT('Origin',(130.84203686942,-75.1781363338475,-200.900005310182)) ;
#81011 = CARTESIAN_POINT('',(134.424014363967,-75.2257613338475,-197.090005310183)) ;
#81012 = CARTESIAN_POINT('Ctrl Pts',(134.424014363967,-75.2257613338475,-197.090005310183)) ;
#81013 = CARTESIAN_POINT('Ctrl Pts',(134.321167599324,-75.2046272914557,-197.090005310183)) ;
#81014 = CARTESIAN_POINT('Ctrl Pts',(134.194888612299,-75.1931618993052,-197.090005310067)) ;
#81015 = CARTESIAN_POINT('Ctrl Pts',(133.943644057601,-75.1801139618915,-197.090005310067)) ;
#81016 = CARTESIAN_POINT('Ctrl Pts',(133.808883889988,-75.1781363338475,-197.090005310183)) ;
#81017 = CARTESIAN_POINT('Ctrl Pts',(133.683932334729,-75.1781363338475,-197.090005310183)) ;
#81018 = CARTESIAN_POINT('Origin',(130.842036869419,-75.2257613338461,-200.900005310183)) ;
#81019 = CARTESIAN_POINT('Origin',(130.84203686942,-75.4956363338475,-200.900005310182)) ;
#81020 = CARTESIAN_POINT('',(130.84203686942,-75.1781363338475,-199.249005310182)) ;
#81021 = CARTESIAN_POINT('Origin',(130.84203686942,-75.1781363338475,-200.900005310182)) ;
#81022 = CARTESIAN_POINT('',(130.84203686942,-75.8131363338475,-199.249005310182)) ;
#81023 = CARTESIAN_POINT('',(130.84203686942,-75.4956363338475,-199.249005310182)) ;
#81024 = CARTESIAN_POINT('Origin',(130.84203686942,-75.8131363338475,-200.900005310182)) ;
#81025 = CARTESIAN_POINT('Origin',(134.65203686942,-75.1781363338475,-197.090005310183)) ;
#81026 = CARTESIAN_POINT('',(131.572286869419,-75.1781363338475,-204.710005310182)) ;
#81027 = CARTESIAN_POINT('',(131.572286869419,-75.1781363338475,-204.710005310182)) ;
#81028 = CARTESIAN_POINT('',(131.572286870962,-75.1781363338475,-203.440005310188)) ;
#81029 = CARTESIAN_POINT('',(131.572286869419,-75.1781363338475,-204.710005310182)) ;
#81030 = CARTESIAN_POINT('',(130.111786868562,-75.1781363338475,-203.440005310187)) ;
#81031 = CARTESIAN_POINT('Origin',(130.84203687019,-75.1781363338475,-203.440005310182)) ;
#81032 = CARTESIAN_POINT('',(130.111786869419,-75.1781363338475,-204.710005310182)) ;
#81033 = CARTESIAN_POINT('',(130.111786869419,-75.1781363338475,-203.440005310187)) ;
#81034 = CARTESIAN_POINT('',(128.000141404109,-75.1781363338475,-204.710005310182)) ;
#81035 = CARTESIAN_POINT('',(127.032036869419,-75.1781363338475,-201.630255310181)) ;
#81036 = CARTESIAN_POINT('',(127.032036869419,-75.1781363338475,-201.630255310181)) ;
#81037 = CARTESIAN_POINT('',(128.302036869413,-75.1781363338475,-201.630255311724)) ;
#81038 = CARTESIAN_POINT('',(127.032036869419,-75.1781363338475,-201.630255310181)) ;
#81039 = CARTESIAN_POINT('',(128.302036869415,-75.1781363338475,-200.169755309325)) ;
#81040 = CARTESIAN_POINT('Origin',(128.30203686942,-75.1781363338475,-200.900005310953)) ;
#81041 = CARTESIAN_POINT('',(127.03203686942,-75.1781363338475,-200.169755310181)) ;
#81042 = CARTESIAN_POINT('',(128.302036869415,-75.1781363338475,-200.169755310182)) ;
#81043 = CARTESIAN_POINT('',(127.03203686942,-75.1781363338475,-198.058109844872)) ;
#81044 = CARTESIAN_POINT('',(130.11178686942,-75.1781363338475,-197.090005310182)) ;
#81045 = CARTESIAN_POINT('',(130.11178686942,-75.1781363338475,-197.090005310182)) ;
#81046 = CARTESIAN_POINT('',(130.111786867877,-75.1781363338475,-198.360005310176)) ;
#81047 = CARTESIAN_POINT('',(130.11178686942,-75.1781363338475,-197.090005310182)) ;
#81048 = CARTESIAN_POINT('',(131.572286870277,-75.1781363338475,-198.360005310177)) ;
#81049 = CARTESIAN_POINT('Origin',(130.842036868649,-75.1781363338475,-198.360005310182)) ;
#81050 = CARTESIAN_POINT('',(131.57228686942,-75.1781363338475,-197.090005310182)) ;
#81051 = CARTESIAN_POINT('',(131.57228686942,-75.1781363338475,-198.360005310177)) ;
#81052 = CARTESIAN_POINT('',(133.683932334729,-75.1781363338475,-197.090005310183)) ;
#81053 = CARTESIAN_POINT('',(134.65203686942,-75.1781363338475,-200.169755310183)) ;
#81054 = CARTESIAN_POINT('',(134.65203686942,-75.1781363338475,-200.169755310183)) ;
#81055 = CARTESIAN_POINT('',(133.382036869426,-75.1781363338475,-200.16975530864)) ;
#81056 = CARTESIAN_POINT('',(134.65203686942,-75.1781363338475,-200.169755310183)) ;
#81057 = CARTESIAN_POINT('',(133.382036869424,-75.1781363338475,-201.63025531104)) ;
#81058 = CARTESIAN_POINT('Origin',(133.38203686942,-75.1781363338475,-200.900005309411)) ;
#81059 = CARTESIAN_POINT('',(134.652036869419,-75.1781363338475,-201.630255310183)) ;
#81060 = CARTESIAN_POINT('',(133.382036869424,-75.1781363338475,-201.630255310183)) ;
#81061 = CARTESIAN_POINT('',(134.652036869419,-75.1781363338475,-203.741900775492)) ;
#81062 = CARTESIAN_POINT('Origin',(134.890161869419,-75.3686363338475,-201.693755310183)) ;
#81063 = CARTESIAN_POINT('',(134.65203686942,-75.3686363338475,-200.328505310183)) ;
#81064 = CARTESIAN_POINT('',(133.382036869411,-75.3686363338475,-200.328505308646)) ;
#81065 = CARTESIAN_POINT('',(134.65203686942,-75.3686363338475,-200.328505310183)) ;
#81066 = CARTESIAN_POINT('',(134.652036869419,-75.3686363338475,-201.471505310183)) ;
#81067 = CARTESIAN_POINT('',(134.652036869419,-75.3686363338475,-201.471505310183)) ;
#81068 = CARTESIAN_POINT('',(133.382036869422,-75.3686363338475,-201.471505311719)) ;
#81069 = CARTESIAN_POINT('',(133.382036869422,-75.3686363338475,-201.471505311335)) ;
#81070 = CARTESIAN_POINT('Origin',(133.38203686942,-75.3686363338475,-200.900005310183)) ;
#81071 = CARTESIAN_POINT('Origin',(126.79391186942,-75.3686363338475,-200.106255310181)) ;
#81072 = CARTESIAN_POINT('',(127.03203686942,-75.3686363338475,-200.328505310181)) ;
#81073 = CARTESIAN_POINT('',(127.032036869419,-75.3686363338475,-201.471505310181)) ;
#81074 = CARTESIAN_POINT('',(127.03203686942,-75.3686363338475,-200.328505310181)) ;
#81075 = CARTESIAN_POINT('',(128.302036869418,-75.3686363338475,-200.328505308645)) ;
#81076 = CARTESIAN_POINT('',(128.302036869418,-75.3686363338475,-200.328505309029)) ;
#81077 = CARTESIAN_POINT('',(128.30203686943,-75.3686363338475,-201.471505311718)) ;
#81078 = CARTESIAN_POINT('Origin',(128.30203686942,-75.3686363338475,-200.900005310182)) ;
#81079 = CARTESIAN_POINT('',(127.032036869419,-75.3686363338475,-201.471505310181)) ;
#81080 = CARTESIAN_POINT('Origin',(130.048286869419,-75.3686363338475,-204.948130310182)) ;
#81081 = CARTESIAN_POINT('',(131.413536869419,-75.3686363338475,-204.710005310182)) ;
#81082 = CARTESIAN_POINT('',(131.413536870956,-75.3686363338475,-203.440005310174)) ;
#81083 = CARTESIAN_POINT('',(131.413536869419,-75.3686363338475,-204.710005310182)) ;
#81084 = CARTESIAN_POINT('',(130.270536869419,-75.3686363338475,-204.710005310182)) ;
#81085 = CARTESIAN_POINT('',(130.270536869419,-75.3686363338475,-204.710005310182)) ;
#81086 = CARTESIAN_POINT('',(130.270536867882,-75.3686363338475,-203.440005310184)) ;
#81087 = CARTESIAN_POINT('',(130.270536868267,-75.3686363338475,-203.440005310184)) ;
#81088 = CARTESIAN_POINT('Origin',(130.842036869419,-75.3686363338475,-203.440005310182)) ;
#81089 = CARTESIAN_POINT('Origin',(131.63578686942,-75.3686363338475,-196.851880310182)) ;
#81090 = CARTESIAN_POINT('',(131.41353686942,-75.3686363338475,-197.090005310182)) ;
#81091 = CARTESIAN_POINT('',(130.27053686942,-75.3686363338475,-197.090005310182)) ;
#81092 = CARTESIAN_POINT('',(131.41353686942,-75.3686363338475,-197.090005310182)) ;
#81093 = CARTESIAN_POINT('',(131.413536870957,-75.3686363338475,-198.36000531018)) ;
#81094 = CARTESIAN_POINT('',(131.413536870572,-75.3686363338475,-198.36000531018)) ;
#81095 = CARTESIAN_POINT('',(130.270536867883,-75.3686363338475,-198.36000531019)) ;
#81096 = CARTESIAN_POINT('Origin',(130.84203686942,-75.3686363338475,-198.360005310182)) ;
#81097 = CARTESIAN_POINT('',(130.27053686942,-75.3686363338475,-197.090005310182)) ;
#81098 = CARTESIAN_POINT('Origin',(130.842036869357,-75.2733863367505,-198.360005310008)) ;
#81099 = CARTESIAN_POINT('',(131.47703686942,-75.2733863338475,-198.360005310182)) ;
#81100 = CARTESIAN_POINT('Origin',(131.572286870869,-75.2733863352967,-198.360005310175)) ;
#81101 = CARTESIAN_POINT('',(130.20703686942,-75.2733863338475,-198.360005310177)) ;
#81102 = CARTESIAN_POINT('Origin',(130.111786868103,-75.2733863351644,-198.360005310176)) ;
#81103 = CARTESIAN_POINT('Origin',(130.84203686942,-75.2733863338475,-198.360005310182)) ;
#81104 = CARTESIAN_POINT('Origin',(131.57228686942,-75.2733863338475,-198.360005310182)) ;
#81105 = CARTESIAN_POINT('',(131.47703686942,-75.2733863338475,-197.090005310182)) ;
#81106 = CARTESIAN_POINT('',(131.47703686942,-75.2733863338475,-198.360005310182)) ;
#81107 = CARTESIAN_POINT('Origin',(131.57228686942,-75.2733863338475,-197.090005310182)) ;
#81108 = CARTESIAN_POINT('Origin',(130.11178686942,-75.2733863338475,-196.994755310182)) ;
#81109 = CARTESIAN_POINT('',(130.20703686942,-75.2733863338475,-197.090005310182)) ;
#81110 = CARTESIAN_POINT('Origin',(130.11178686942,-75.2733863338475,-197.090005310182)) ;
#81111 = CARTESIAN_POINT('',(130.20703686942,-75.2733863338475,-197.090005310182)) ;
#81112 = CARTESIAN_POINT('Origin',(133.382036869594,-75.2733863367505,-200.90000531012)) ;
#81113 = CARTESIAN_POINT('',(133.382036869419,-75.2733863338475,-201.535005310183)) ;
#81114 = CARTESIAN_POINT('Origin',(133.382036869422,-75.2733863351644,-201.6302553115)) ;
#81115 = CARTESIAN_POINT('',(133.382036869425,-75.2733863338475,-200.265005310183)) ;
#81116 = CARTESIAN_POINT('Origin',(133.382036869425,-75.2733863351644,-200.169755308866)) ;
#81117 = CARTESIAN_POINT('Origin',(133.38203686942,-75.2733863338475,-200.900005310183)) ;
#81118 = CARTESIAN_POINT('Origin',(133.382036869419,-75.2733863338475,-201.630255310183)) ;
#81119 = CARTESIAN_POINT('',(134.652036869419,-75.2733863338475,-201.535005310183)) ;
#81120 = CARTESIAN_POINT('',(133.382036869419,-75.2733863338475,-201.535005310183)) ;
#81121 = CARTESIAN_POINT('Origin',(134.652036869419,-75.2733863338475,-201.630255310183)) ;
#81122 = CARTESIAN_POINT('Origin',(134.74728686942,-75.2733863338475,-200.169755310183)) ;
#81123 = CARTESIAN_POINT('',(134.65203686942,-75.2733863338475,-200.265005310183)) ;
#81124 = CARTESIAN_POINT('Origin',(134.65203686942,-75.2733863338475,-200.169755310183)) ;
#81125 = CARTESIAN_POINT('',(134.65203686942,-75.2733863338475,-200.265005310183)) ;
#81126 = CARTESIAN_POINT('Origin',(130.842036869482,-75.2733863367505,-203.440005310356)) ;
#81127 = CARTESIAN_POINT('',(130.207036869419,-75.2733863338475,-203.440005310182)) ;
#81128 = CARTESIAN_POINT('Origin',(130.11178686797,-75.2733863352967,-203.440005310189)) ;
#81129 = CARTESIAN_POINT('',(131.477036869419,-75.2733863338475,-203.440005310188)) ;
#81130 = CARTESIAN_POINT('Origin',(131.572286870736,-75.2733863351644,-203.440005310188)) ;
#81131 = CARTESIAN_POINT('Origin',(130.842036869419,-75.2733863338475,-203.440005310182)) ;
#81132 = CARTESIAN_POINT('Origin',(130.111786869419,-75.2733863338475,-203.440005310182)) ;
#81133 = CARTESIAN_POINT('',(130.207036869419,-75.2733863338476,-204.710005310182)) ;
#81134 = CARTESIAN_POINT('',(130.207036869419,-75.2733863338475,-203.440005310182)) ;
#81135 = CARTESIAN_POINT('Origin',(130.111786869419,-75.2733863338475,-204.710005310182)) ;
#81136 = CARTESIAN_POINT('Origin',(131.572286869419,-75.2733863338476,-204.805255310182)) ;
#81137 = CARTESIAN_POINT('',(131.477036869419,-75.2733863338476,-204.710005310182)) ;
#81138 = CARTESIAN_POINT('Origin',(131.572286869419,-75.2733863338476,-204.710005310182)) ;
#81139 = CARTESIAN_POINT('',(131.477036869419,-75.2733863338476,-204.710005310182)) ;
#81140 = CARTESIAN_POINT('Origin',(130.207036869419,-75.2733863338475,-203.440005310182)) ;
#81141 = CARTESIAN_POINT('',(130.207036869419,-75.3051363338475,-203.440005310182)) ;
#81142 = CARTESIAN_POINT('',(130.207036869419,-75.3051363338475,-204.710005310182)) ;
#81143 = CARTESIAN_POINT('',(130.207036869419,-75.3051363338475,-203.440005310182)) ;
#81144 = CARTESIAN_POINT('',(130.207036869419,-75.2733863338476,-204.710005310182)) ;
#81145 = CARTESIAN_POINT('',(130.207036869419,-75.2733863338475,-203.440005310182)) ;
#81146 = CARTESIAN_POINT('Origin',(131.477036869419,-75.2733863338476,-204.710005310182)) ;
#81147 = CARTESIAN_POINT('',(131.477036869419,-75.3051363338475,-204.710005310182)) ;
#81148 = CARTESIAN_POINT('',(131.477036869419,-75.3051363338475,-203.440005310185)) ;
#81149 = CARTESIAN_POINT('',(131.477036869419,-75.3051363338475,-204.710005310182)) ;
#81150 = CARTESIAN_POINT('',(131.477036869419,-75.2733863338475,-203.440005310188)) ;
#81151 = CARTESIAN_POINT('',(131.477036869419,-75.2733863338476,-204.710005310182)) ;
#81152 = CARTESIAN_POINT('Origin',(130.842036869419,-75.2733863338475,-203.440005310182)) ;
#81153 = CARTESIAN_POINT('Origin',(130.842036869419,-75.3051363338475,-203.440005310182)) ;
#81154 = CARTESIAN_POINT('Origin',(130.270536869419,-75.3051363338475,-203.440005310182)) ;
#81155 = CARTESIAN_POINT('Origin',(130.270536868435,-75.3051363348312,-203.440005310183)) ;
#81156 = CARTESIAN_POINT('Origin',(130.270536869419,-75.3051363338475,-204.710005310182)) ;
#81157 = CARTESIAN_POINT('Origin',(131.413536869419,-75.3051363338475,-204.773505310182)) ;
#81158 = CARTESIAN_POINT('Origin',(131.413536869419,-75.3051363338475,-204.710005310182)) ;
#81159 = CARTESIAN_POINT('Origin',(131.413536870502,-75.3051363349301,-203.440005310169)) ;
#81160 = CARTESIAN_POINT('Origin',(130.842036869372,-75.305136336016,-203.440005310312)) ;
#81161 = CARTESIAN_POINT('Origin',(128.30203686942,-75.2733863338475,-200.265005310182)) ;
#81162 = CARTESIAN_POINT('',(128.30203686942,-75.2733863338475,-200.265005310182)) ;
#81163 = CARTESIAN_POINT('',(128.30203686942,-75.3051363338475,-200.265005310182)) ;
#81164 = CARTESIAN_POINT('',(128.30203686942,-75.2733863338475,-200.265005310182)) ;
#81165 = CARTESIAN_POINT('',(127.03203686942,-75.3051363338475,-200.265005310181)) ;
#81166 = CARTESIAN_POINT('',(128.30203686942,-75.3051363338475,-200.265005310182)) ;
#81167 = CARTESIAN_POINT('',(127.03203686942,-75.2733863338475,-200.265005310181)) ;
#81168 = CARTESIAN_POINT('',(127.03203686942,-75.2733863338475,-200.265005310181)) ;
#81169 = CARTESIAN_POINT('',(128.30203686942,-75.2733863338475,-200.265005310182)) ;
#81170 = CARTESIAN_POINT('Origin',(127.032036869419,-75.2733863338475,-201.535005310181)) ;
#81171 = CARTESIAN_POINT('',(127.032036869419,-75.2733863338475,-201.535005310181)) ;
#81172 = CARTESIAN_POINT('',(127.032036869419,-75.3051363338475,-201.535005310181)) ;
#81173 = CARTESIAN_POINT('',(127.032036869419,-75.2733863338475,-201.535005310181)) ;
#81174 = CARTESIAN_POINT('',(128.302036869419,-75.3051363338475,-201.535005310182)) ;
#81175 = CARTESIAN_POINT('',(127.032036869419,-75.3051363338475,-201.535005310181)) ;
#81176 = CARTESIAN_POINT('',(128.302036869414,-75.2733863338475,-201.535005310182)) ;
#81177 = CARTESIAN_POINT('',(128.302036869414,-75.2733863338475,-201.535005310182)) ;
#81178 = CARTESIAN_POINT('',(127.032036869419,-75.2733863338475,-201.535005310181)) ;
#81179 = CARTESIAN_POINT('Origin',(128.302036869289,-75.305136336016,-200.900005310135)) ;
#81180 = CARTESIAN_POINT('Origin',(128.302036869425,-75.3051363348312,-201.471505311165)) ;
#81181 = CARTESIAN_POINT('Origin',(128.302036869419,-75.3051363348312,-200.328505309198)) ;
#81182 = CARTESIAN_POINT('Origin',(128.30203686942,-75.3051363338475,-200.900005310182)) ;
#81183 = CARTESIAN_POINT('Origin',(128.30203686942,-75.3051363338475,-200.328505310182)) ;
#81184 = CARTESIAN_POINT('Origin',(127.03203686942,-75.3051363338475,-200.328505310181)) ;
#81185 = CARTESIAN_POINT('Origin',(126.968536869419,-75.3051363338475,-201.471505310181)) ;
#81186 = CARTESIAN_POINT('Origin',(127.032036869419,-75.3051363338475,-201.471505310181)) ;
#81187 = CARTESIAN_POINT('Origin',(131.47703686942,-75.2733863338475,-198.360005310182)) ;
#81188 = CARTESIAN_POINT('',(131.47703686942,-75.3051363338475,-198.360005310182)) ;
#81189 = CARTESIAN_POINT('',(131.47703686942,-75.3051363338475,-197.090005310182)) ;
#81190 = CARTESIAN_POINT('',(131.47703686942,-75.3051363338475,-198.360005310182)) ;
#81191 = CARTESIAN_POINT('',(131.47703686942,-75.2733863338475,-197.090005310182)) ;
#81192 = CARTESIAN_POINT('',(131.47703686942,-75.2733863338475,-198.360005310182)) ;
#81193 = CARTESIAN_POINT('Origin',(130.20703686942,-75.2733863338475,-197.090005310182)) ;
#81194 = CARTESIAN_POINT('',(130.20703686942,-75.3051363338475,-197.090005310182)) ;
#81195 = CARTESIAN_POINT('',(130.20703686942,-75.3051363338475,-198.360005310179)) ;
#81196 = CARTESIAN_POINT('',(130.20703686942,-75.3051363338475,-197.090005310182)) ;
#81197 = CARTESIAN_POINT('',(130.20703686942,-75.2733863338475,-198.360005310177)) ;
#81198 = CARTESIAN_POINT('',(130.20703686942,-75.2733863338475,-197.090005310182)) ;
#81199 = CARTESIAN_POINT('Origin',(130.84203686942,-75.2733863338475,-198.360005310182)) ;
#81200 = CARTESIAN_POINT('Origin',(130.84203686942,-75.3051363338475,-198.360005310182)) ;
#81201 = CARTESIAN_POINT('Origin',(130.842036869467,-75.305136336016,-198.360005310052)) ;
#81202 = CARTESIAN_POINT('Origin',(130.270536868436,-75.3051363348312,-198.360005310185)) ;
#81203 = CARTESIAN_POINT('Origin',(131.413536870404,-75.3051363348312,-198.360005310181)) ;
#81204 = CARTESIAN_POINT('Origin',(131.41353686942,-75.3051363338475,-198.360005310182)) ;
#81205 = CARTESIAN_POINT('Origin',(131.41353686942,-75.3051363338475,-197.090005310182)) ;
#81206 = CARTESIAN_POINT('Origin',(130.27053686942,-75.3051363338475,-197.026505310182)) ;
#81207 = CARTESIAN_POINT('Origin',(130.27053686942,-75.3051363338475,-197.090005310182)) ;
#81208 = CARTESIAN_POINT('Origin',(133.382036869419,-75.2733863338475,-201.535005310183)) ;
#81209 = CARTESIAN_POINT('',(133.382036869419,-75.3051363338475,-201.535005310183)) ;
#81210 = CARTESIAN_POINT('',(134.652036869419,-75.3051363338475,-201.535005310183)) ;
#81211 = CARTESIAN_POINT('',(133.382036869419,-75.3051363338475,-201.535005310183)) ;
#81212 = CARTESIAN_POINT('',(134.652036869419,-75.2733863338475,-201.535005310183)) ;
#81213 = CARTESIAN_POINT('',(133.382036869419,-75.2733863338475,-201.535005310183)) ;
#81214 = CARTESIAN_POINT('Origin',(134.65203686942,-75.2733863338475,-200.265005310183)) ;
#81215 = CARTESIAN_POINT('',(134.65203686942,-75.3051363338475,-200.265005310183)) ;
#81216 = CARTESIAN_POINT('',(133.382036869422,-75.3051363338475,-200.265005310183)) ;
#81217 = CARTESIAN_POINT('',(134.65203686942,-75.3051363338475,-200.265005310183)) ;
#81218 = CARTESIAN_POINT('',(133.382036869425,-75.2733863338475,-200.265005310183)) ;
#81219 = CARTESIAN_POINT('',(134.65203686942,-75.2733863338475,-200.265005310183)) ;
#81220 = CARTESIAN_POINT('Origin',(133.38203686942,-75.2733863338475,-200.900005310183)) ;
#81221 = CARTESIAN_POINT('Origin',(133.38203686942,-75.3051363338475,-200.900005310183)) ;
#81222 = CARTESIAN_POINT('Origin',(133.382036869419,-75.3051363338475,-201.471505310183)) ;
#81223 = CARTESIAN_POINT('Origin',(133.382036869421,-75.3051363348312,-201.471505311166)) ;
#81224 = CARTESIAN_POINT('Origin',(134.652036869419,-75.3051363338475,-201.471505310183)) ;
#81225 = CARTESIAN_POINT('Origin',(134.71553686942,-75.3051363338475,-200.328505310183)) ;
#81226 = CARTESIAN_POINT('Origin',(134.65203686942,-75.3051363338475,-200.328505310183)) ;
#81227 = CARTESIAN_POINT('Origin',(133.382036869407,-75.3051363349301,-200.3285053091)) ;
#81228 = CARTESIAN_POINT('Origin',(133.38203686955,-75.305136336016,-200.90000531023)) ;
#81229 = CARTESIAN_POINT('Origin',(128.30203686942,-75.2733863338475,-200.900005310182)) ;
#81230 = CARTESIAN_POINT('Origin',(128.30203686942,-75.2733863338475,-200.900005310182)) ;
#81231 = CARTESIAN_POINT('Origin',(128.302036869245,-75.2733863367505,-200.900005310245)) ;
#81232 = CARTESIAN_POINT('Origin',(128.302036869417,-75.2733863351644,-200.169755308865)) ;
#81233 = CARTESIAN_POINT('Origin',(128.302036869414,-75.2733863351644,-201.630255311499)) ;
#81234 = CARTESIAN_POINT('Origin',(128.30203686942,-75.2733863338475,-200.169755310182)) ;
#81235 = CARTESIAN_POINT('Origin',(127.03203686942,-75.2733863338475,-200.169755310181)) ;
#81236 = CARTESIAN_POINT('Origin',(126.936786869419,-75.2733863338475,-201.630255310181)) ;
#81237 = CARTESIAN_POINT('Origin',(127.032036869419,-75.2733863338475,-201.630255310181)) ;
#81238 = CARTESIAN_POINT('Origin',(134.890161869419,-76.0036363338475,-201.693755310183)) ;
#81239 = CARTESIAN_POINT('',(133.38203686942,-76.0036363338475,-200.454870310183)) ;
#81240 = CARTESIAN_POINT('',(133.382036869419,-76.0036363338475,-201.345140310183)) ;
#81241 = CARTESIAN_POINT('Origin',(133.38203686942,-76.0036363338475,-200.900005310183)) ;
#81242 = CARTESIAN_POINT('',(134.652036869419,-76.0036363338475,-201.345140310183)) ;
#81243 = CARTESIAN_POINT('',(133.382036869419,-76.0036363338475,-201.345140310183)) ;
#81244 = CARTESIAN_POINT('',(134.65203686942,-76.0036363338475,-200.454870310183)) ;
#81245 = CARTESIAN_POINT('',(134.652036869419,-76.0036363338475,-201.345140310183)) ;
#81246 = CARTESIAN_POINT('',(134.65203686942,-76.0036363338475,-200.454870310183)) ;
#81247 = CARTESIAN_POINT('Origin',(134.017036869419,-75.8131363338475,-201.535005310183)) ;
#81248 = CARTESIAN_POINT('',(133.382036869419,-75.8134538337756,-201.535005257089)) ;
#81249 = CARTESIAN_POINT('',(134.652036869419,-75.8131363338475,-201.535005310183)) ;
#81250 = CARTESIAN_POINT('',(133.382036869419,-75.8131363338475,-201.535005310183)) ;
#81251 = CARTESIAN_POINT('',(134.652036869419,-75.8137713338475,-201.535005310183)) ;
#81252 = CARTESIAN_POINT('',(134.652036869419,-75.8131363338475,-201.535005310183)) ;
#81253 = CARTESIAN_POINT('',(133.382036869419,-75.8137713338475,-201.535005310183)) ;
#81254 = CARTESIAN_POINT('Origin',(134.01703686942,-75.8131363338475,-200.265005310183)) ;
#81255 = CARTESIAN_POINT('',(134.65203686942,-75.8131363338475,-200.265005310183)) ;
#81256 = CARTESIAN_POINT('',(134.65203686942,-75.8137713338475,-200.265005310183)) ;
#81257 = CARTESIAN_POINT('',(134.65203686942,-75.8131363338475,-200.265005310183)) ;
#81258 = CARTESIAN_POINT('',(133.38203686942,-75.8131363338475,-200.265005310183)) ;
#81259 = CARTESIAN_POINT('',(134.65203686942,-75.8131363338475,-200.265005310183)) ;
#81260 = CARTESIAN_POINT('',(133.38203686942,-75.8137713338475,-200.265005310183)) ;
#81261 = CARTESIAN_POINT('',(133.38203686942,-75.8131363338475,-200.265005310183)) ;
#81262 = CARTESIAN_POINT('',(134.65203686942,-75.8137713338475,-200.265005310183)) ;
#81263 = CARTESIAN_POINT('Origin',(133.38203686942,-75.8131363338475,-200.900005310183)) ;
#81264 = CARTESIAN_POINT('Origin',(133.38203686942,-75.8131363338475,-200.900005310183)) ;
#81265 = CARTESIAN_POINT('Origin',(133.38203686942,-75.8137713338475,-200.900005310183)) ;
#81266 = CARTESIAN_POINT('Origin',(134.111969369419,-75.8137713338475,-201.345140310183)) ;
#81267 = CARTESIAN_POINT('Origin',(134.652036869419,-75.8137713338475,-201.345140310183)) ;
#81268 = CARTESIAN_POINT('Origin',(133.382036869419,-75.8137713338475,-201.345140310183)) ;
#81269 = CARTESIAN_POINT('Origin',(134.11196936942,-75.8137713338475,-200.454870310183)) ;
#81270 = CARTESIAN_POINT('Origin',(133.38203686942,-75.8137713338475,-200.454870310183)) ;
#81271 = CARTESIAN_POINT('Origin',(134.65203686942,-75.8137713338475,-200.454870310183)) ;
#81272 = CARTESIAN_POINT('Origin',(133.38203686942,-75.8137713338475,-200.900005310183)) ;
#81273 = CARTESIAN_POINT('Origin',(130.048286869419,-76.0036363338475,-204.948130310182)) ;
#81274 = CARTESIAN_POINT('',(131.287171869419,-76.0036363338475,-203.440005310182)) ;
#81275 = CARTESIAN_POINT('',(130.396901869419,-76.0036363338475,-203.440005310182)) ;
#81276 = CARTESIAN_POINT('Origin',(130.842036869419,-76.0036363338475,-203.440005310182)) ;
#81277 = CARTESIAN_POINT('',(130.396901869419,-76.0036363338475,-204.710005310182)) ;
#81278 = CARTESIAN_POINT('',(130.396901869419,-76.0036363338475,-203.440005310182)) ;
#81279 = CARTESIAN_POINT('',(131.287171869419,-76.0036363338475,-204.710005310182)) ;
#81280 = CARTESIAN_POINT('',(130.396901869419,-76.0036363338475,-204.710005310182)) ;
#81281 = CARTESIAN_POINT('',(131.287171869419,-76.0036363338475,-204.710005310182)) ;
#81282 = CARTESIAN_POINT('Origin',(130.207036869419,-75.8131363338475,-204.075005310182)) ;
#81283 = CARTESIAN_POINT('',(130.207036922513,-75.8134538337756,-203.440005310182)) ;
#81284 = CARTESIAN_POINT('',(130.207036869419,-75.8131363338475,-204.710005310182)) ;
#81285 = CARTESIAN_POINT('',(130.207036869419,-75.8131363338475,-203.440005310182)) ;
#81286 = CARTESIAN_POINT('',(130.207036869419,-75.8137713338475,-204.710005310182)) ;
#81287 = CARTESIAN_POINT('',(130.207036869419,-75.8131363338475,-204.710005310182)) ;
#81288 = CARTESIAN_POINT('',(130.207036869419,-75.8137713338475,-203.440005310182)) ;
#81289 = CARTESIAN_POINT('Origin',(131.477036869419,-75.8131363338475,-204.075005310182)) ;
#81290 = CARTESIAN_POINT('',(131.477036869419,-75.8131363338475,-204.710005310182)) ;
#81291 = CARTESIAN_POINT('',(131.477036869419,-75.8137713338475,-204.710005310182)) ;
#81292 = CARTESIAN_POINT('',(131.477036869419,-75.8131363338475,-204.710005310182)) ;
#81293 = CARTESIAN_POINT('',(131.477036869419,-75.8131363338475,-203.440005310182)) ;
#81294 = CARTESIAN_POINT('',(131.477036869419,-75.8131363338475,-204.710005310182)) ;
#81295 = CARTESIAN_POINT('',(131.477036869419,-75.8137713338475,-203.440005310182)) ;
#81296 = CARTESIAN_POINT('',(131.477036869419,-75.8131363338475,-203.440005310182)) ;
#81297 = CARTESIAN_POINT('',(131.477036869419,-75.8137713338475,-204.710005310182)) ;
#81298 = CARTESIAN_POINT('Origin',(130.842036869419,-75.8131363338475,-203.440005310182)) ;
#81299 = CARTESIAN_POINT('Origin',(130.842036869419,-75.8131363338475,-203.440005310182)) ;
#81300 = CARTESIAN_POINT('Origin',(130.842036869419,-75.8137713338475,-203.440005310182)) ;
#81301 = CARTESIAN_POINT('Origin',(130.396901869419,-75.8137713338475,-204.169937810182)) ;
#81302 = CARTESIAN_POINT('Origin',(130.396901869419,-75.8137713338475,-204.710005310182)) ;
#81303 = CARTESIAN_POINT('Origin',(130.396901869419,-75.8137713338475,-203.440005310182)) ;
#81304 = CARTESIAN_POINT('Origin',(131.287171869419,-75.8137713338475,-204.169937810182)) ;
#81305 = CARTESIAN_POINT('Origin',(131.287171869419,-75.8137713338475,-203.440005310182)) ;
#81306 = CARTESIAN_POINT('Origin',(131.287171869419,-75.8137713338475,-204.710005310182)) ;
#81307 = CARTESIAN_POINT('Origin',(130.842036869419,-75.8137713338475,-203.440005310182)) ;
#81308 = CARTESIAN_POINT('Origin',(130.04828686942,-76.0036363338475,-196.851880310182)) ;
#81309 = CARTESIAN_POINT('',(131.28717186942,-76.0036363338475,-197.090005310182)) ;
#81310 = CARTESIAN_POINT('',(131.28717186942,-76.0036363338475,-198.360005310182)) ;
#81311 = CARTESIAN_POINT('',(131.28717186942,-76.0036363338475,-197.090005310182)) ;
#81312 = CARTESIAN_POINT('',(130.39690186942,-76.0036363338475,-197.090005310182)) ;
#81313 = CARTESIAN_POINT('',(130.39690186942,-76.0036363338475,-197.090005310182)) ;
#81314 = CARTESIAN_POINT('',(130.39690186942,-76.0036363338475,-198.360005310182)) ;
#81315 = CARTESIAN_POINT('',(130.39690186942,-76.0036363338475,-198.360005310182)) ;
#81316 = CARTESIAN_POINT('Origin',(130.84203686942,-76.0036363338475,-198.360005310182)) ;
#81317 = CARTESIAN_POINT('Origin',(130.20703686942,-75.9083863338475,-198.360005310182)) ;
#81318 = CARTESIAN_POINT('',(130.207036922514,-75.8134538337756,-198.360005310182)) ;
#81319 = CARTESIAN_POINT('',(130.20703686942,-75.8137713338475,-197.090005310182)) ;
#81320 = CARTESIAN_POINT('',(130.20703686942,-75.8137713338475,-198.360005310182)) ;
#81321 = CARTESIAN_POINT('',(130.20703686942,-75.8131363338475,-197.090005310182)) ;
#81322 = CARTESIAN_POINT('',(130.20703686942,-75.8131363338475,-197.090005310182)) ;
#81323 = CARTESIAN_POINT('',(130.20703686942,-75.8131363338475,-197.090005310182)) ;
#81324 = CARTESIAN_POINT('Origin',(131.47703686942,-75.9083863338475,-197.090005310182)) ;
#81325 = CARTESIAN_POINT('',(131.47703686942,-75.8137713338475,-197.090005310182)) ;
#81326 = CARTESIAN_POINT('',(131.47703686942,-75.8137713338475,-198.360005310182)) ;
#81327 = CARTESIAN_POINT('',(131.47703686942,-75.8137713338475,-197.090005310182)) ;
#81328 = CARTESIAN_POINT('',(131.47703686942,-75.8131363338475,-198.360005310182)) ;
#81329 = CARTESIAN_POINT('',(131.47703686942,-75.8131363338475,-198.360005310182)) ;
#81330 = CARTESIAN_POINT('',(131.47703686942,-75.8131363338475,-197.090005310182)) ;
#81331 = CARTESIAN_POINT('',(131.47703686942,-75.8131363338475,-198.360005310182)) ;
#81332 = CARTESIAN_POINT('',(131.47703686942,-75.8131363338475,-197.090005310182)) ;
#81333 = CARTESIAN_POINT('Origin',(130.84203686942,-75.9083863338475,-198.360005310182)) ;
#81334 = CARTESIAN_POINT('Origin',(130.84203686942,-75.8137713338475,-198.360005310182)) ;
#81335 = CARTESIAN_POINT('Origin',(130.84203686942,-75.8131363338475,-198.360005310182)) ;
#81336 = CARTESIAN_POINT('Origin',(130.39690186942,-75.8137713338475,-198.360005310182)) ;
#81337 = CARTESIAN_POINT('Origin',(130.39690186942,-75.8137713338475,-198.360005310182)) ;
#81338 = CARTESIAN_POINT('Origin',(130.39690186942,-75.8137713338475,-197.090005310182)) ;
#81339 = CARTESIAN_POINT('Origin',(131.28717186942,-75.8137713338475,-196.900140310182)) ;
#81340 = CARTESIAN_POINT('Origin',(131.28717186942,-75.8137713338475,-197.090005310182)) ;
#81341 = CARTESIAN_POINT('Origin',(131.28717186942,-75.8137713338475,-198.360005310182)) ;
#81342 = CARTESIAN_POINT('Origin',(130.84203686942,-75.8137713338475,-198.360005310182)) ;
#81343 = CARTESIAN_POINT('Origin',(126.793911869419,-76.0036363338475,-201.693755310181)) ;
#81344 = CARTESIAN_POINT('',(127.03203686942,-76.0036363338475,-200.454870310181)) ;
#81345 = CARTESIAN_POINT('',(128.30203686942,-76.0036363338475,-200.454870310182)) ;
#81346 = CARTESIAN_POINT('',(127.03203686942,-76.0036363338475,-200.454870310181)) ;
#81347 = CARTESIAN_POINT('',(127.032036869419,-76.0036363338475,-201.345140310181)) ;
#81348 = CARTESIAN_POINT('',(127.032036869419,-76.0036363338475,-201.345140310181)) ;
#81349 = CARTESIAN_POINT('',(128.302036869419,-76.0036363338475,-201.345140310182)) ;
#81350 = CARTESIAN_POINT('',(128.302036869419,-76.0036363338475,-201.345140310182)) ;
#81351 = CARTESIAN_POINT('Origin',(128.30203686942,-76.0036363338475,-200.900005310182)) ;
#81352 = CARTESIAN_POINT('Origin',(128.302036869419,-75.9083863338475,-201.535005310182)) ;
#81353 = CARTESIAN_POINT('',(128.302036869419,-75.8134538337756,-201.535005257088)) ;
#81354 = CARTESIAN_POINT('',(127.032036869419,-75.8137713338475,-201.535005310181)) ;
#81355 = CARTESIAN_POINT('',(128.302036869419,-75.8137713338475,-201.535005310182)) ;
#81356 = CARTESIAN_POINT('',(127.032036869419,-75.8131363338475,-201.535005310181)) ;
#81357 = CARTESIAN_POINT('',(127.032036869419,-75.8131363338475,-201.535005310181)) ;
#81358 = CARTESIAN_POINT('',(127.032036869419,-75.8131363338475,-201.535005310181)) ;
#81359 = CARTESIAN_POINT('Origin',(127.03203686942,-75.9083863338475,-200.265005310181)) ;
#81360 = CARTESIAN_POINT('',(127.03203686942,-75.8137713338475,-200.265005310181)) ;
#81361 = CARTESIAN_POINT('',(128.30203686942,-75.8137713338475,-200.265005310182)) ;
#81362 = CARTESIAN_POINT('',(127.03203686942,-75.8137713338475,-200.265005310181)) ;
#81363 = CARTESIAN_POINT('',(128.30203686942,-75.8131363338475,-200.265005310182)) ;
#81364 = CARTESIAN_POINT('',(128.30203686942,-75.8131363338475,-200.265005310182)) ;
#81365 = CARTESIAN_POINT('',(127.03203686942,-75.8131363338475,-200.265005310181)) ;
#81366 = CARTESIAN_POINT('',(128.30203686942,-75.8131363338475,-200.265005310182)) ;
#81367 = CARTESIAN_POINT('',(127.03203686942,-75.8131363338475,-200.265005310181)) ;
#81368 = CARTESIAN_POINT('Origin',(128.30203686942,-75.9083863338475,-200.900005310182)) ;
#81369 = CARTESIAN_POINT('Origin',(128.30203686942,-75.8137713338475,-200.900005310182)) ;
#81370 = CARTESIAN_POINT('Origin',(128.30203686942,-75.8131363338475,-200.900005310182)) ;
#81371 = CARTESIAN_POINT('Origin',(128.302036869419,-75.8137713338475,-201.345140310182)) ;
#81372 = CARTESIAN_POINT('Origin',(128.302036869419,-75.8137713338475,-201.345140310182)) ;
#81373 = CARTESIAN_POINT('Origin',(127.032036869419,-75.8137713338475,-201.345140310181)) ;
#81374 = CARTESIAN_POINT('Origin',(126.84217186942,-75.8137713338475,-200.454870310181)) ;
#81375 = CARTESIAN_POINT('Origin',(127.03203686942,-75.8137713338475,-200.454870310181)) ;
#81376 = CARTESIAN_POINT('Origin',(128.30203686942,-75.8137713338475,-200.454870310182)) ;
#81377 = CARTESIAN_POINT('Origin',(128.30203686942,-75.8137713338475,-200.900005310182)) ;
#81378 = CARTESIAN_POINT('Origin',(134.652036869419,-75.1781363338475,-204.710005310183)) ;
#81379 = CARTESIAN_POINT('',(134.652036869419,-75.8131363338476,-204.481982804729)) ;
#81380 = CARTESIAN_POINT('',(134.652036869419,-75.8131363338476,-204.481982804729)) ;
#81381 = CARTESIAN_POINT('',(134.65203686942,-75.8131363338475,-197.318027815637)) ;
#81382 = CARTESIAN_POINT('',(134.65203686942,-75.2257613338475,-197.318027815637)) ;
#81383 = CARTESIAN_POINT('',(134.65203686942,-75.8131363338475,-198.058109844874)) ;
#81384 = CARTESIAN_POINT('',(134.65203686942,-75.8131363338475,-198.058109844874)) ;
#81385 = CARTESIAN_POINT('',(134.65203686942,-75.8131363338475,-200.265005310183)) ;
#81386 = CARTESIAN_POINT('',(134.652036869419,-75.8131363338475,-203.741900775492)) ;
#81387 = CARTESIAN_POINT('',(134.652036869419,-75.8131363338475,-203.741900775492)) ;
#81388 = CARTESIAN_POINT('',(134.652036869419,-75.8131363338476,-204.481982804729)) ;
#81389 = CARTESIAN_POINT('Origin',(127.03203686942,-75.1781363338475,-197.090005310181)) ;
#81390 = CARTESIAN_POINT('',(127.03203686942,-75.8131363338475,-197.318027815635)) ;
#81391 = CARTESIAN_POINT('',(127.03203686942,-75.8131363338475,-197.318027815635)) ;
#81392 = CARTESIAN_POINT('',(127.032036869419,-75.8131363338475,-204.481982804728)) ;
#81393 = CARTESIAN_POINT('',(127.032036869419,-75.2257613338475,-204.481982804728)) ;
#81394 = CARTESIAN_POINT('',(127.032036869419,-75.8131363338475,-203.741900775491)) ;
#81395 = CARTESIAN_POINT('',(127.032036869419,-75.8131363338475,-203.741900775491)) ;
#81396 = CARTESIAN_POINT('',(127.032036869419,-75.8131363338475,-201.535005310181)) ;
#81397 = CARTESIAN_POINT('',(127.03203686942,-75.8131363338475,-198.058109844872)) ;
#81398 = CARTESIAN_POINT('',(127.03203686942,-75.8131363338475,-198.058109844872)) ;
#81399 = CARTESIAN_POINT('',(127.03203686942,-75.8131363338475,-197.318027815635)) ;
#81400 = CARTESIAN_POINT('Origin',(127.032036869419,-75.1781363338475,-204.710005310181)) ;
#81401 = CARTESIAN_POINT('',(127.260059374872,-75.8131363338475,-204.710005310181)) ;
#81402 = CARTESIAN_POINT('',(127.260059374872,-75.8131363338475,-204.710005310181)) ;
#81403 = CARTESIAN_POINT('',(134.424014363965,-75.8131363338476,-204.710005310183)) ;
#81404 = CARTESIAN_POINT('',(134.424014363965,-75.2257613338475,-204.710005310183)) ;
#81405 = CARTESIAN_POINT('',(133.683932334728,-75.8131363338475,-204.710005310183)) ;
#81406 = CARTESIAN_POINT('',(133.683932334728,-75.8131363338475,-204.710005310183)) ;
#81407 = CARTESIAN_POINT('',(131.477036869419,-75.8131363338475,-204.710005310182)) ;
#81408 = CARTESIAN_POINT('',(128.000141404109,-75.8131363338475,-204.710005310182)) ;
#81409 = CARTESIAN_POINT('',(128.000141404109,-75.8131363338475,-204.710005310182)) ;
#81410 = CARTESIAN_POINT('',(127.260059374872,-75.8131363338475,-204.710005310181)) ;
#81411 = CARTESIAN_POINT('Origin',(134.65203686942,-75.1781363338475,-197.090005310183)) ;
#81412 = CARTESIAN_POINT('',(134.424014363967,-75.8131363338475,-197.090005310183)) ;
#81413 = CARTESIAN_POINT('',(134.424014363967,-75.8131363338475,-197.090005310183)) ;
#81414 = CARTESIAN_POINT('',(127.260059374874,-75.8131363338475,-197.090005310181)) ;
#81415 = CARTESIAN_POINT('',(127.260059356689,-75.2257613340712,-197.090005310181)) ;
#81416 = CARTESIAN_POINT('',(128.000141404111,-75.8131363338475,-197.090005310182)) ;
#81417 = CARTESIAN_POINT('',(128.000141404111,-75.8131363338475,-197.090005310182)) ;
#81418 = CARTESIAN_POINT('',(130.20703686942,-75.8131363338475,-197.090005310182)) ;
#81419 = CARTESIAN_POINT('',(133.683932334729,-75.8131363338475,-197.090005310183)) ;
#81420 = CARTESIAN_POINT('',(133.683932334729,-75.8131363338475,-197.090005310183)) ;
#81421 = CARTESIAN_POINT('',(134.424014363967,-75.8131363338475,-197.090005310183)) ;
#81422 = CARTESIAN_POINT('Origin',(134.65203686942,-75.8131363338475,-197.090005310183)) ;
#81423 = CARTESIAN_POINT('Origin',(130.84203686942,-75.8131363338476,-200.900005310182)) ;
#81424 = CARTESIAN_POINT('',(127.481049604646,-75.8131363338475,-197.539018187062)) ;
#81425 = CARTESIAN_POINT('Origin',(130.84203686942,-75.8131363338478,-200.900005310182)) ;
#81426 = CARTESIAN_POINT('Origin',(130.84203686942,-75.8131363338475,-200.900005310182)) ;
#81427 = CARTESIAN_POINT('Origin',(130.84203686942,-75.8131363338475,-200.900005310182)) ;
#81428 = CARTESIAN_POINT('Origin',(130.84203686942,-75.8131363338476,-200.900005310182)) ;
#81429 = CARTESIAN_POINT('Ctrl Pts',(127.032036789131,-76.0036363338475,-197.090005390471)) ;
#81430 = CARTESIAN_POINT('Ctrl Pts',(127.032036789131,-75.8131363338475,-197.090005390471)) ;
#81431 = CARTESIAN_POINT('Ctrl Pts',(127.481049604646,-75.8131363338475,-197.539018187062)) ;
#81432 = CARTESIAN_POINT('Ctrl Pts',(123.222036869419,-76.0036363338475,-200.90000547076)) ;
#81433 = CARTESIAN_POINT('Ctrl Pts',(123.222036869419,-75.8131363338475,-200.90000547076)) ;
#81434 = CARTESIAN_POINT('Ctrl Pts',(124.120062481526,-75.8131363338475,-200.900005451836)) ;
#81435 = CARTESIAN_POINT('Ctrl Pts',(127.032036949709,-76.0036363338475,-204.710005390471)) ;
#81436 = CARTESIAN_POINT('Ctrl Pts',(127.032036949709,-75.8131363338475,-204.710005390471)) ;
#81437 = CARTESIAN_POINT('Ctrl Pts',(127.4810497463,-75.8131363338475,-204.260992574956)) ;
#81438 = CARTESIAN_POINT('Ctrl Pts',(130.842037029998,-76.0036363338476,-208.520005310182)) ;
#81439 = CARTESIAN_POINT('Ctrl Pts',(130.842037029998,-75.8131363338476,-208.520005310182)) ;
#81440 = CARTESIAN_POINT('Ctrl Pts',(130.842037011073,-75.8131363338476,-207.621979698075)) ;
#81441 = CARTESIAN_POINT('Ctrl Pts',(134.652036949709,-76.0036363338476,-204.710005229893)) ;
#81442 = CARTESIAN_POINT('Ctrl Pts',(134.652036949709,-75.8131363338476,-204.710005229893)) ;
#81443 = CARTESIAN_POINT('Ctrl Pts',(134.203024134193,-75.8131363338476,-204.260992433302)) ;
#81444 = CARTESIAN_POINT('Ctrl Pts',(138.46203686942,-76.0036363338475,-200.900005149604)) ;
#81445 = CARTESIAN_POINT('Ctrl Pts',(138.46203686942,-75.8131363338475,-200.900005149604)) ;
#81446 = CARTESIAN_POINT('Ctrl Pts',(137.564011257313,-75.8131363338475,-200.900005168529)) ;
#81447 = CARTESIAN_POINT('Ctrl Pts',(134.652036789131,-76.0036363338475,-197.090005229893)) ;
#81448 = CARTESIAN_POINT('Ctrl Pts',(134.652036789131,-75.8131363338475,-197.090005229893)) ;
#81449 = CARTESIAN_POINT('Ctrl Pts',(134.203023992539,-75.8131363338475,-197.539018045409)) ;
#81450 = CARTESIAN_POINT('Ctrl Pts',(130.842036708842,-76.0036363338475,-193.280005310182)) ;
#81451 = CARTESIAN_POINT('Ctrl Pts',(130.842036708842,-75.8131363338475,-193.280005310182)) ;
#81452 = CARTESIAN_POINT('Ctrl Pts',(130.842036727766,-75.8131363338475,-194.178030922289)) ;
#81453 = CARTESIAN_POINT('Ctrl Pts',(127.032036789131,-76.0036363338475,-197.090005390471)) ;
#81454 = CARTESIAN_POINT('Ctrl Pts',(127.032036789131,-75.8131363338475,-197.090005390471)) ;
#81455 = CARTESIAN_POINT('Ctrl Pts',(127.481049604646,-75.8131363338475,-197.539018187062)) ;
#81456 = CARTESIAN_POINT('',(134.424014372653,-75.8607613348135,-204.710005308452)) ;
#81457 = CARTESIAN_POINT('',(134.652036871149,-75.8607613328816,-204.481982796042)) ;
#81458 = CARTESIAN_POINT('Origin',(130.842036868431,-75.8607613338483,-200.90000531117)) ;
#81459 = CARTESIAN_POINT('Ctrl Pts',(134.652036869419,-75.8607613320955,-204.481982796203)) ;
#81460 = CARTESIAN_POINT('Ctrl Pts',(134.652036869419,-75.8396272026366,-204.379135603943)) ;
#81461 = CARTESIAN_POINT('Ctrl Pts',(134.652036869522,-75.8281624630209,-204.252864864675)) ;
#81462 = CARTESIAN_POINT('Ctrl Pts',(134.652036869522,-75.8151140186796,-204.001616634739)) ;
#81463 = CARTESIAN_POINT('Ctrl Pts',(134.652036869419,-75.8131363338476,-203.866854124742)) ;
#81464 = CARTESIAN_POINT('Ctrl Pts',(134.652036869419,-75.8131363338476,-203.741900775492)) ;
#81465 = CARTESIAN_POINT('Ctrl Pts',(133.683932334728,-75.8131363338476,-204.710005310182)) ;
#81466 = CARTESIAN_POINT('Ctrl Pts',(133.808883891339,-75.8131363338476,-204.710005310182)) ;
#81467 = CARTESIAN_POINT('Ctrl Pts',(133.943644060714,-75.8151139619344,-204.710005310299)) ;
#81468 = CARTESIAN_POINT('Ctrl Pts',(134.194888618251,-75.8281618997334,-204.710005310299)) ;
#81469 = CARTESIAN_POINT('Ctrl Pts',(134.32116760723,-75.8396272922766,-204.710005310183)) ;
#81470 = CARTESIAN_POINT('Ctrl Pts',(134.424014372491,-75.8607613355995,-204.710005310183)) ;
#81471 = CARTESIAN_POINT('Origin',(134.652036869419,-75.8131363338476,-204.710005310183)) ;
#81472 = CARTESIAN_POINT('',(134.652036869419,-75.860761333691,-204.481982792)) ;
#81473 = CARTESIAN_POINT('Origin',(127.032036869419,-75.8131363338475,-204.710005310181)) ;
#81474 = CARTESIAN_POINT('',(134.424014363965,-75.8131363338476,-204.710005310183)) ;
#81475 = CARTESIAN_POINT('Ctrl Pts',(127.032036789131,-76.0036363338475,-197.090005390471)) ;
#81476 = CARTESIAN_POINT('Ctrl Pts',(127.032036789131,-75.8131363338475,-197.090005390471)) ;
#81477 = CARTESIAN_POINT('Ctrl Pts',(127.481049604646,-75.8131363338475,-197.539018187062)) ;
#81478 = CARTESIAN_POINT('Ctrl Pts',(123.222036869419,-76.0036363338475,-200.90000547076)) ;
#81479 = CARTESIAN_POINT('Ctrl Pts',(123.222036869419,-75.8131363338475,-200.90000547076)) ;
#81480 = CARTESIAN_POINT('Ctrl Pts',(124.120062481526,-75.8131363338475,-200.900005451836)) ;
#81481 = CARTESIAN_POINT('Ctrl Pts',(127.032036949709,-76.0036363338475,-204.710005390471)) ;
#81482 = CARTESIAN_POINT('Ctrl Pts',(127.032036949709,-75.8131363338475,-204.710005390471)) ;
#81483 = CARTESIAN_POINT('Ctrl Pts',(127.4810497463,-75.8131363338475,-204.260992574956)) ;
#81484 = CARTESIAN_POINT('Ctrl Pts',(130.842037029998,-76.0036363338476,-208.520005310182)) ;
#81485 = CARTESIAN_POINT('Ctrl Pts',(130.842037029998,-75.8131363338476,-208.520005310182)) ;
#81486 = CARTESIAN_POINT('Ctrl Pts',(130.842037011073,-75.8131363338476,-207.621979698075)) ;
#81487 = CARTESIAN_POINT('Ctrl Pts',(134.652036949709,-76.0036363338476,-204.710005229893)) ;
#81488 = CARTESIAN_POINT('Ctrl Pts',(134.652036949709,-75.8131363338476,-204.710005229893)) ;
#81489 = CARTESIAN_POINT('Ctrl Pts',(134.203024134193,-75.8131363338476,-204.260992433302)) ;
#81490 = CARTESIAN_POINT('Ctrl Pts',(138.46203686942,-76.0036363338475,-200.900005149604)) ;
#81491 = CARTESIAN_POINT('Ctrl Pts',(138.46203686942,-75.8131363338475,-200.900005149604)) ;
#81492 = CARTESIAN_POINT('Ctrl Pts',(137.564011257313,-75.8131363338475,-200.900005168529)) ;
#81493 = CARTESIAN_POINT('Ctrl Pts',(134.652036789131,-76.0036363338475,-197.090005229893)) ;
#81494 = CARTESIAN_POINT('Ctrl Pts',(134.652036789131,-75.8131363338475,-197.090005229893)) ;
#81495 = CARTESIAN_POINT('Ctrl Pts',(134.203023992539,-75.8131363338475,-197.539018045409)) ;
#81496 = CARTESIAN_POINT('Ctrl Pts',(130.842036708842,-76.0036363338475,-193.280005310182)) ;
#81497 = CARTESIAN_POINT('Ctrl Pts',(130.842036708842,-75.8131363338475,-193.280005310182)) ;
#81498 = CARTESIAN_POINT('Ctrl Pts',(130.842036727766,-75.8131363338475,-194.178030922289)) ;
#81499 = CARTESIAN_POINT('Ctrl Pts',(127.032036789131,-76.0036363338475,-197.090005390471)) ;
#81500 = CARTESIAN_POINT('Ctrl Pts',(127.032036789131,-75.8131363338475,-197.090005390471)) ;
#81501 = CARTESIAN_POINT('Ctrl Pts',(127.481049604646,-75.8131363338475,-197.539018187062)) ;
#81502 = CARTESIAN_POINT('',(127.032036871149,-75.8607613348136,-204.481982813415)) ;
#81503 = CARTESIAN_POINT('',(127.26005938356,-75.8607613328816,-204.710005311911)) ;
#81504 = CARTESIAN_POINT('Origin',(130.842036868431,-75.8607613338468,-200.900005309194)) ;
#81505 = CARTESIAN_POINT('Ctrl Pts',(127.260059383398,-75.8607613320955,-204.710005310181)) ;
#81506 = CARTESIAN_POINT('Ctrl Pts',(127.362906575657,-75.8396272026369,-204.710005310181)) ;
#81507 = CARTESIAN_POINT('Ctrl Pts',(127.489177314922,-75.8281624630211,-204.710005310284)) ;
#81508 = CARTESIAN_POINT('Ctrl Pts',(127.74042554486,-75.8151140186795,-204.710005310284)) ;
#81509 = CARTESIAN_POINT('Ctrl Pts',(127.875188054858,-75.8131363338475,-204.710005310181)) ;
#81510 = CARTESIAN_POINT('Ctrl Pts',(128.000141404109,-75.8131363338475,-204.710005310181)) ;
#81511 = CARTESIAN_POINT('Ctrl Pts',(127.032036869419,-75.8131363338475,-203.741900775491)) ;
#81512 = CARTESIAN_POINT('Ctrl Pts',(127.032036869419,-75.8131363338475,-203.866852332103)) ;
#81513 = CARTESIAN_POINT('Ctrl Pts',(127.032036869302,-75.8151139619343,-204.001612501477)) ;
#81514 = CARTESIAN_POINT('Ctrl Pts',(127.032036869302,-75.8281618997335,-204.252857059014)) ;
#81515 = CARTESIAN_POINT('Ctrl Pts',(127.032036869419,-75.8396272922767,-204.379136047993)) ;
#81516 = CARTESIAN_POINT('Ctrl Pts',(127.032036869419,-75.8607613355997,-204.481982813254)) ;
#81517 = CARTESIAN_POINT('Origin',(127.03203686942,-75.8131363338475,-197.090005310181)) ;
#81518 = CARTESIAN_POINT('',(127.032036869419,-75.8131363338475,-204.481982804728)) ;
#81519 = CARTESIAN_POINT('Origin',(127.032036869419,-75.8131363338475,-204.710005310181)) ;
#81520 = CARTESIAN_POINT('',(127.260059387602,-75.860761333691,-204.710005310181)) ;
#81521 = CARTESIAN_POINT('Ctrl Pts',(127.032036789131,-76.0036363338475,-197.090005390471)) ;
#81522 = CARTESIAN_POINT('Ctrl Pts',(127.032036789131,-75.8131363338475,-197.090005390471)) ;
#81523 = CARTESIAN_POINT('Ctrl Pts',(127.481049604646,-75.8131363338475,-197.539018187062)) ;
#81524 = CARTESIAN_POINT('Ctrl Pts',(123.222036869419,-76.0036363338475,-200.90000547076)) ;
#81525 = CARTESIAN_POINT('Ctrl Pts',(123.222036869419,-75.8131363338475,-200.90000547076)) ;
#81526 = CARTESIAN_POINT('Ctrl Pts',(124.120062481526,-75.8131363338475,-200.900005451836)) ;
#81527 = CARTESIAN_POINT('Ctrl Pts',(127.032036949709,-76.0036363338475,-204.710005390471)) ;
#81528 = CARTESIAN_POINT('Ctrl Pts',(127.032036949709,-75.8131363338475,-204.710005390471)) ;
#81529 = CARTESIAN_POINT('Ctrl Pts',(127.4810497463,-75.8131363338475,-204.260992574956)) ;
#81530 = CARTESIAN_POINT('Ctrl Pts',(130.842037029998,-76.0036363338476,-208.520005310182)) ;
#81531 = CARTESIAN_POINT('Ctrl Pts',(130.842037029998,-75.8131363338476,-208.520005310182)) ;
#81532 = CARTESIAN_POINT('Ctrl Pts',(130.842037011073,-75.8131363338476,-207.621979698075)) ;
#81533 = CARTESIAN_POINT('Ctrl Pts',(134.652036949709,-76.0036363338476,-204.710005229893)) ;
#81534 = CARTESIAN_POINT('Ctrl Pts',(134.652036949709,-75.8131363338476,-204.710005229893)) ;
#81535 = CARTESIAN_POINT('Ctrl Pts',(134.203024134193,-75.8131363338476,-204.260992433302)) ;
#81536 = CARTESIAN_POINT('Ctrl Pts',(138.46203686942,-76.0036363338475,-200.900005149604)) ;
#81537 = CARTESIAN_POINT('Ctrl Pts',(138.46203686942,-75.8131363338475,-200.900005149604)) ;
#81538 = CARTESIAN_POINT('Ctrl Pts',(137.564011257313,-75.8131363338475,-200.900005168529)) ;
#81539 = CARTESIAN_POINT('Ctrl Pts',(134.652036789131,-76.0036363338475,-197.090005229893)) ;
#81540 = CARTESIAN_POINT('Ctrl Pts',(134.652036789131,-75.8131363338475,-197.090005229893)) ;
#81541 = CARTESIAN_POINT('Ctrl Pts',(134.203023992539,-75.8131363338475,-197.539018045409)) ;
#81542 = CARTESIAN_POINT('Ctrl Pts',(130.842036708842,-76.0036363338475,-193.280005310182)) ;
#81543 = CARTESIAN_POINT('Ctrl Pts',(130.842036708842,-75.8131363338475,-193.280005310182)) ;
#81544 = CARTESIAN_POINT('Ctrl Pts',(130.842036727766,-75.8131363338475,-194.178030922289)) ;
#81545 = CARTESIAN_POINT('Ctrl Pts',(127.032036789131,-76.0036363338475,-197.090005390471)) ;
#81546 = CARTESIAN_POINT('Ctrl Pts',(127.032036789131,-75.8131363338475,-197.090005390471)) ;
#81547 = CARTESIAN_POINT('Ctrl Pts',(127.481049604646,-75.8131363338475,-197.539018187062)) ;
#81548 = CARTESIAN_POINT('',(127.144290007455,-75.8607613338475,-197.202258575173)) ;
#81549 = CARTESIAN_POINT('',(127.032036867121,-75.8607613325238,-197.318027827715)) ;
#81550 = CARTESIAN_POINT('Origin',(130.842036777866,-75.86076129501,-200.900005218629)) ;
#81551 = CARTESIAN_POINT('Ctrl Pts',(127.03203686942,-75.8607613314121,-197.318027827487)) ;
#81552 = CARTESIAN_POINT('Ctrl Pts',(127.03203686942,-75.8396272023282,-197.420875019448)) ;
#81553 = CARTESIAN_POINT('Ctrl Pts',(127.032036869317,-75.8281624628045,-197.547145758675)) ;
#81554 = CARTESIAN_POINT('Ctrl Pts',(127.032036869317,-75.8151140186575,-197.798393987228)) ;
#81555 = CARTESIAN_POINT('Ctrl Pts',(127.03203686942,-75.8131363338475,-197.933156496317)) ;
#81556 = CARTESIAN_POINT('Ctrl Pts',(127.03203686942,-75.8131363338475,-198.058109844872)) ;
#81557 = CARTESIAN_POINT('Ctrl Pts',(127.144290007455,-75.8607613338475,-197.202258575173)) ;
#81558 = CARTESIAN_POINT('Ctrl Pts',(127.2191254716,-75.8290113338475,-197.277094046379)) ;
#81559 = CARTESIAN_POINT('Ctrl Pts',(127.331378670518,-75.8131363338475,-197.389347250489)) ;
#81560 = CARTESIAN_POINT('Ctrl Pts',(127.481049604646,-75.8131363338475,-197.539018187062)) ;
#81561 = CARTESIAN_POINT('Ctrl Pts',(127.032036789131,-76.0036363338475,-197.090005390471)) ;
#81562 = CARTESIAN_POINT('Ctrl Pts',(127.032036789131,-75.8131363338475,-197.090005390471)) ;
#81563 = CARTESIAN_POINT('Ctrl Pts',(127.481049604646,-75.8131363338475,-197.539018187062)) ;
#81564 = CARTESIAN_POINT('Ctrl Pts',(123.222036869419,-76.0036363338475,-200.90000547076)) ;
#81565 = CARTESIAN_POINT('Ctrl Pts',(123.222036869419,-75.8131363338475,-200.90000547076)) ;
#81566 = CARTESIAN_POINT('Ctrl Pts',(124.120062481526,-75.8131363338475,-200.900005451836)) ;
#81567 = CARTESIAN_POINT('Ctrl Pts',(127.032036949709,-76.0036363338475,-204.710005390471)) ;
#81568 = CARTESIAN_POINT('Ctrl Pts',(127.032036949709,-75.8131363338475,-204.710005390471)) ;
#81569 = CARTESIAN_POINT('Ctrl Pts',(127.4810497463,-75.8131363338475,-204.260992574956)) ;
#81570 = CARTESIAN_POINT('Ctrl Pts',(130.842037029998,-76.0036363338476,-208.520005310182)) ;
#81571 = CARTESIAN_POINT('Ctrl Pts',(130.842037029998,-75.8131363338476,-208.520005310182)) ;
#81572 = CARTESIAN_POINT('Ctrl Pts',(130.842037011073,-75.8131363338476,-207.621979698075)) ;
#81573 = CARTESIAN_POINT('Ctrl Pts',(134.652036949709,-76.0036363338476,-204.710005229893)) ;
#81574 = CARTESIAN_POINT('Ctrl Pts',(134.652036949709,-75.8131363338476,-204.710005229893)) ;
#81575 = CARTESIAN_POINT('Ctrl Pts',(134.203024134193,-75.8131363338476,-204.260992433302)) ;
#81576 = CARTESIAN_POINT('Ctrl Pts',(138.46203686942,-76.0036363338475,-200.900005149604)) ;
#81577 = CARTESIAN_POINT('Ctrl Pts',(138.46203686942,-75.8131363338475,-200.900005149604)) ;
#81578 = CARTESIAN_POINT('Ctrl Pts',(137.564011257313,-75.8131363338475,-200.900005168529)) ;
#81579 = CARTESIAN_POINT('Ctrl Pts',(134.652036789131,-76.0036363338475,-197.090005229893)) ;
#81580 = CARTESIAN_POINT('Ctrl Pts',(134.652036789131,-75.8131363338475,-197.090005229893)) ;
#81581 = CARTESIAN_POINT('Ctrl Pts',(134.203023992539,-75.8131363338475,-197.539018045409)) ;
#81582 = CARTESIAN_POINT('Ctrl Pts',(130.842036708842,-76.0036363338475,-193.280005310182)) ;
#81583 = CARTESIAN_POINT('Ctrl Pts',(130.842036708842,-75.8131363338475,-193.280005310182)) ;
#81584 = CARTESIAN_POINT('Ctrl Pts',(130.842036727766,-75.8131363338475,-194.178030922289)) ;
#81585 = CARTESIAN_POINT('Ctrl Pts',(127.032036789131,-76.0036363338475,-197.090005390471)) ;
#81586 = CARTESIAN_POINT('Ctrl Pts',(127.032036789131,-75.8131363338475,-197.090005390471)) ;
#81587 = CARTESIAN_POINT('Ctrl Pts',(127.481049604646,-75.8131363338475,-197.539018187062)) ;
#81588 = CARTESIAN_POINT('',(127.260059362794,-75.8607613351713,-197.09000531248)) ;
#81589 = CARTESIAN_POINT('Origin',(130.842036960973,-75.860761372679,-200.900005401736)) ;
#81590 = CARTESIAN_POINT('Ctrl Pts',(128.000141404111,-75.8131363338475,-197.090005310182)) ;
#81591 = CARTESIAN_POINT('Ctrl Pts',(127.875189846825,-75.8131363338475,-197.090005310182)) ;
#81592 = CARTESIAN_POINT('Ctrl Pts',(127.74042967657,-75.8151139619557,-197.090005310065)) ;
#81593 = CARTESIAN_POINT('Ctrl Pts',(127.489185117999,-75.8281618999272,-197.090005310065)) ;
#81594 = CARTESIAN_POINT('Ctrl Pts',(127.362906128424,-75.8396272926172,-197.090005310182)) ;
#81595 = CARTESIAN_POINT('Ctrl Pts',(127.260059363022,-75.8607613362829,-197.090005310182)) ;
#81596 = CARTESIAN_POINT('Origin',(127.03203686942,-75.8131363338475,-197.090005310181)) ;
#81597 = CARTESIAN_POINT('',(127.03203686942,-75.8607613336239,-197.31802783382)) ;
#81598 = CARTESIAN_POINT('Origin',(134.65203686942,-75.8131363338475,-197.090005310183)) ;
#81599 = CARTESIAN_POINT('',(127.260059374874,-75.8131363338475,-197.090005310181)) ;
#81600 = CARTESIAN_POINT('Ctrl Pts',(127.032036789131,-76.0036363338475,-197.090005390471)) ;
#81601 = CARTESIAN_POINT('Ctrl Pts',(127.032036789131,-75.8131363338475,-197.090005390471)) ;
#81602 = CARTESIAN_POINT('Ctrl Pts',(127.481049604646,-75.8131363338475,-197.539018187062)) ;
#81603 = CARTESIAN_POINT('Ctrl Pts',(123.222036869419,-76.0036363338475,-200.90000547076)) ;
#81604 = CARTESIAN_POINT('Ctrl Pts',(123.222036869419,-75.8131363338475,-200.90000547076)) ;
#81605 = CARTESIAN_POINT('Ctrl Pts',(124.120062481526,-75.8131363338475,-200.900005451836)) ;
#81606 = CARTESIAN_POINT('Ctrl Pts',(127.032036949709,-76.0036363338475,-204.710005390471)) ;
#81607 = CARTESIAN_POINT('Ctrl Pts',(127.032036949709,-75.8131363338475,-204.710005390471)) ;
#81608 = CARTESIAN_POINT('Ctrl Pts',(127.4810497463,-75.8131363338475,-204.260992574956)) ;
#81609 = CARTESIAN_POINT('Ctrl Pts',(130.842037029998,-76.0036363338476,-208.520005310182)) ;
#81610 = CARTESIAN_POINT('Ctrl Pts',(130.842037029998,-75.8131363338476,-208.520005310182)) ;
#81611 = CARTESIAN_POINT('Ctrl Pts',(130.842037011073,-75.8131363338476,-207.621979698075)) ;
#81612 = CARTESIAN_POINT('Ctrl Pts',(134.652036949709,-76.0036363338476,-204.710005229893)) ;
#81613 = CARTESIAN_POINT('Ctrl Pts',(134.652036949709,-75.8131363338476,-204.710005229893)) ;
#81614 = CARTESIAN_POINT('Ctrl Pts',(134.203024134193,-75.8131363338476,-204.260992433302)) ;
#81615 = CARTESIAN_POINT('Ctrl Pts',(138.46203686942,-76.0036363338475,-200.900005149604)) ;
#81616 = CARTESIAN_POINT('Ctrl Pts',(138.46203686942,-75.8131363338475,-200.900005149604)) ;
#81617 = CARTESIAN_POINT('Ctrl Pts',(137.564011257313,-75.8131363338475,-200.900005168529)) ;
#81618 = CARTESIAN_POINT('Ctrl Pts',(134.652036789131,-76.0036363338475,-197.090005229893)) ;
#81619 = CARTESIAN_POINT('Ctrl Pts',(134.652036789131,-75.8131363338475,-197.090005229893)) ;
#81620 = CARTESIAN_POINT('Ctrl Pts',(134.203023992539,-75.8131363338475,-197.539018045409)) ;
#81621 = CARTESIAN_POINT('Ctrl Pts',(130.842036708842,-76.0036363338475,-193.280005310182)) ;
#81622 = CARTESIAN_POINT('Ctrl Pts',(130.842036708842,-75.8131363338475,-193.280005310182)) ;
#81623 = CARTESIAN_POINT('Ctrl Pts',(130.842036727766,-75.8131363338475,-194.178030922289)) ;
#81624 = CARTESIAN_POINT('Ctrl Pts',(127.032036789131,-76.0036363338475,-197.090005390471)) ;
#81625 = CARTESIAN_POINT('Ctrl Pts',(127.032036789131,-75.8131363338475,-197.090005390471)) ;
#81626 = CARTESIAN_POINT('Ctrl Pts',(127.481049604646,-75.8131363338475,-197.539018187062)) ;
#81627 = CARTESIAN_POINT('',(134.65203686769,-75.8607613348134,-197.318027806949)) ;
#81628 = CARTESIAN_POINT('',(134.424014355279,-75.8607613328816,-197.090005308453)) ;
#81629 = CARTESIAN_POINT('Origin',(130.842036870408,-75.860761333849,-200.90000531117)) ;
#81630 = CARTESIAN_POINT('Ctrl Pts',(134.424014355441,-75.8607613320954,-197.090005310183)) ;
#81631 = CARTESIAN_POINT('Ctrl Pts',(134.32116716318,-75.8396272026364,-197.090005310183)) ;
#81632 = CARTESIAN_POINT('Ctrl Pts',(134.194896423912,-75.8281624630208,-197.09000531008)) ;
#81633 = CARTESIAN_POINT('Ctrl Pts',(133.943648193978,-75.8151140186795,-197.09000531008)) ;
#81634 = CARTESIAN_POINT('Ctrl Pts',(133.80888568398,-75.8131363338475,-197.090005310183)) ;
#81635 = CARTESIAN_POINT('Ctrl Pts',(133.68393233473,-75.8131363338475,-197.090005310183)) ;
#81636 = CARTESIAN_POINT('Ctrl Pts',(134.65203686942,-75.8131363338475,-198.058109844874)) ;
#81637 = CARTESIAN_POINT('Ctrl Pts',(134.65203686942,-75.8131363338475,-197.933158288262)) ;
#81638 = CARTESIAN_POINT('Ctrl Pts',(134.652036869537,-75.8151139619343,-197.79839811889)) ;
#81639 = CARTESIAN_POINT('Ctrl Pts',(134.652036869537,-75.8281618997332,-197.547153561353)) ;
#81640 = CARTESIAN_POINT('Ctrl Pts',(134.65203686942,-75.8396272922763,-197.420874572373)) ;
#81641 = CARTESIAN_POINT('Ctrl Pts',(134.65203686942,-75.8607613355994,-197.318027807111)) ;
#81642 = CARTESIAN_POINT('Origin',(134.652036869419,-75.8131363338476,-204.710005310183)) ;
#81643 = CARTESIAN_POINT('',(134.65203686942,-75.8131363338475,-197.318027815637)) ;
#81644 = CARTESIAN_POINT('Origin',(134.65203686942,-75.8131363338475,-197.090005310183)) ;
#81645 = CARTESIAN_POINT('',(134.424014351237,-75.860761333691,-197.090005310183)) ;
#81646 = CARTESIAN_POINT('Origin',(130.84203686942,-75.8131363338475,-200.900005310182)) ;
#81647 = CARTESIAN_POINT('Origin',(130.84203686942,-75.8131363338475,-200.900005310182)) ;
#81648 = CARTESIAN_POINT('Origin',(130.84203686942,-75.8131363338475,-200.900005310182)) ;
#81649 = CARTESIAN_POINT('Origin',(130.84203686942,-75.8131363338475,-200.900005310182)) ;
#81650 = CARTESIAN_POINT('',(336.680564494876,808.37256189937,42.1559761620865)) ;
#81651 = CARTESIAN_POINT('',(336.680564494874,798.87256189937,42.1559761620865)) ;
#81652 = CARTESIAN_POINT('',(336.680564494871,779.87256189937,42.1559761620865)) ;
#81653 = CARTESIAN_POINT('',(336.680564494867,760.87256189937,42.1559761620865)) ;
#81654 = CARTESIAN_POINT('',(336.680564494869,770.37256189937,42.1559761620865)) ;
#81655 = CARTESIAN_POINT('',(336.680564494865,751.37256189937,42.1559761620865)) ;
#81656 = CARTESIAN_POINT('',(336.680564494872,789.37256189937,42.1559761620865)) ;
#81657 = CARTESIAN_POINT('',(336.680564494864,741.87256189937,42.1559761620865)) ;
#81658 = CARTESIAN_POINT('',(336.680564494862,732.37256189937,42.1559761620865)) ;
#81659 = CARTESIAN_POINT('',(-0.199999999999818,0.,0.)) ;
#81660 = CARTESIAN_POINT('',(0.,0.,0.)) ;
#81661 = CARTESIAN_POINT('',(0.,0.,0.)) ;
#81662 = CARTESIAN_POINT('',(0.,0.,0.)) ;
#81663 = CARTESIAN_POINT('',(0.,0.,0.)) ;
#81664 = CARTESIAN_POINT('Origin',(337.29203686942,-83.7093863338387,-225.630746738862)) ;
#81665 = CARTESIAN_POINT('',(337.26078686942,-83.7093863338386,-225.630746738861)) ;
#81666 = CARTESIAN_POINT('',(337.22953686942,-83.7406363338387,-225.661996738861)) ;
#81667 = CARTESIAN_POINT('',(336.938011368168,-84.0321618350953,-225.953522240115)) ;
#81668 = CARTESIAN_POINT('',(124.35453686942,-83.7406363338483,-225.661996738861)) ;
#81669 = CARTESIAN_POINT('',(337.29203686942,-83.7406363338387,-225.661996738861)) ;
#81670 = CARTESIAN_POINT('',(124.32328686942,-83.7093863338482,-225.630746738861)) ;
#81671 = CARTESIAN_POINT('',(160.479536869229,-119.865636333962,-261.786996738658)) ;
#81672 = CARTESIAN_POINT('',(124.35453686942,-83.6781363338483,-225.599496738862)) ;
#81673 = CARTESIAN_POINT('',(173.43787020291,-34.5948030003447,-176.516163405793)) ;
#81674 = CARTESIAN_POINT('',(337.22953686942,-83.6781363338387,-225.599496738862)) ;
#81675 = CARTESIAN_POINT('',(337.29203686942,-83.6781363338387,-225.599496738862)) ;
#81676 = CARTESIAN_POINT('',(323.541895704049,-69.9904951684558,-211.911855573599)) ;
#81677 = CARTESIAN_POINT('Origin',(124.32328686942,-83.7093863338481,-143.911996738861)) ;
#81678 = CARTESIAN_POINT('',(124.29203686942,-83.7406363338483,-225.599496738861)) ;
#81679 = CARTESIAN_POINT('',(110.042036869424,-97.9906363338488,-211.349496738868)) ;
#81680 = CARTESIAN_POINT('',(124.29203686942,-83.740636333848,-116.724496738861)) ;
#81681 = CARTESIAN_POINT('',(124.29203686942,-83.7406363338481,-143.911996738861)) ;
#81682 = CARTESIAN_POINT('',(124.32328686942,-83.7093863338482,-116.693246738861)) ;
#81683 = CARTESIAN_POINT('',(119.000370202754,-89.0323030005154,-122.016163405527)) ;
#81684 = CARTESIAN_POINT('',(124.35453686942,-83.678136333848,-116.724496738862)) ;
#81685 = CARTESIAN_POINT('',(164.354536869176,-43.6781363340809,-156.724496739048)) ;
#81686 = CARTESIAN_POINT('',(124.35453686942,-83.6781363338481,-143.911996738861)) ;
#81687 = CARTESIAN_POINT('Origin',(124.32328686942,-87.6781363338484,-225.630746738861)) ;
#81688 = CARTESIAN_POINT('',(124.35453686942,-85.1156363338484,-225.661996738861)) ;
#81689 = CARTESIAN_POINT('',(124.35453686942,-87.6781363338484,-225.661996738861)) ;
#81690 = CARTESIAN_POINT('',(124.32328686942,-85.1468863338484,-225.630746738861)) ;
#81691 = CARTESIAN_POINT('',(159.396203536119,-50.0739696671863,-260.703663405552)) ;
#81692 = CARTESIAN_POINT('',(124.29203686942,-85.1156363338484,-225.599496738861)) ;
#81693 = CARTESIAN_POINT('',(120.208703536087,-81.0323030005159,-221.516163405529)) ;
#81694 = CARTESIAN_POINT('',(124.29203686942,-87.6781363338484,-225.599496738861)) ;
#81695 = CARTESIAN_POINT('Origin',(337.29203686942,-83.6781363338387,-225.661996738861)) ;
#81696 = CARTESIAN_POINT('',(337.22953686942,-85.1156363338387,-225.661996738861)) ;
#81697 = CARTESIAN_POINT('',(337.22953686942,-85.677289341349,-225.661996738861)) ;
#81698 = CARTESIAN_POINT('',(337.29203686942,-85.1156363338387,-225.661996738861)) ;
#81699 = CARTESIAN_POINT('Origin',(337.29203686942,-85.1468863338387,-225.630746738861)) ;
#81700 = CARTESIAN_POINT('',(337.26078686942,-85.1468863338386,-225.630746738861)) ;
#81701 = CARTESIAN_POINT('',(337.22953686942,-85.1781363338387,-225.599496738861)) ;
#81702 = CARTESIAN_POINT('',(332.625229037348,-89.7824441659428,-220.995188906753)) ;
#81703 = CARTESIAN_POINT('',(124.35453686942,-85.1781363338484,-225.599496738861)) ;
#81704 = CARTESIAN_POINT('',(337.29203686942,-85.1781363338387,-225.599496738861)) ;
#81705 = CARTESIAN_POINT('',(164.354536869413,-125.178136333829,-185.599496738844)) ;
#81706 = CARTESIAN_POINT('',(337.354395704005,-85.240495168424,-225.537137904276)) ;
#81707 = CARTESIAN_POINT('Origin',(124.32328686942,-85.1468863338483,-198.411996738861)) ;
#81708 = CARTESIAN_POINT('',(124.35453686942,-85.178136333848,-116.724496738861)) ;
#81709 = CARTESIAN_POINT('',(124.35453686942,-85.1781363338483,-198.411996738861)) ;
#81710 = CARTESIAN_POINT('',(124.32328686942,-85.146886333848,-116.693246738861)) ;
#81711 = CARTESIAN_POINT('',(173.43787020275,-134.261469667163,-165.807830072221)) ;
#81712 = CARTESIAN_POINT('',(124.29203686942,-85.115636333848,-116.724496738861)) ;
#81713 = CARTESIAN_POINT('',(111.250370202751,-72.0739696671828,-129.76616340553)) ;
#81714 = CARTESIAN_POINT('',(124.29203686942,-85.1156363338483,-198.411996738861)) ;
#81715 = CARTESIAN_POINT('Origin',(337.29203686942,-85.1468863338384,-116.693246738861)) ;
#81716 = CARTESIAN_POINT('',(337.26078686942,-85.1468863338384,-116.693246738861)) ;
#81717 = CARTESIAN_POINT('',(337.22953686942,-85.1156363338384,-116.661996738861)) ;
#81718 = CARTESIAN_POINT('',(337.479395704005,-85.3654951684238,-116.911855573447)) ;
#81719 = CARTESIAN_POINT('',(124.35453686942,-85.115636333848,-116.661996738861)) ;
#81720 = CARTESIAN_POINT('',(337.29203686942,-85.1156363338384,-116.661996738861)) ;
#81721 = CARTESIAN_POINT('',(159.271203536106,-50.1989696671892,-81.7453300721742)) ;
#81722 = CARTESIAN_POINT('',(337.22953686942,-85.1781363338384,-116.724496738861)) ;
#81723 = CARTESIAN_POINT('',(337.29203686942,-85.1781363338384,-116.724496738861)) ;
#81724 = CARTESIAN_POINT('',(323.750511368196,-98.6571618351551,-130.203522240189)) ;
#81725 = CARTESIAN_POINT('Origin',(124.32328686942,-88.428136333848,-116.693246738861)) ;
#81726 = CARTESIAN_POINT('',(124.35453686942,-83.740636333848,-116.661996738861)) ;
#81727 = CARTESIAN_POINT('',(124.354536869421,-88.428136333848,-116.661996738861)) ;
#81728 = CARTESIAN_POINT('',(160.604536869668,-119.990636333711,-80.4119967386154)) ;
#81729 = CARTESIAN_POINT('',(124.29203686942,-88.428136333848,-116.724496738861)) ;
#81730 = CARTESIAN_POINT('Origin',(337.29203686942,-85.1781363338384,-116.661996738861)) ;
#81731 = CARTESIAN_POINT('',(337.22953686942,-83.7406363338383,-116.661996738861)) ;
#81732 = CARTESIAN_POINT('',(337.22953686942,-86.4272893413486,-116.661996738861)) ;
#81733 = CARTESIAN_POINT('',(337.29203686942,-83.7406363338383,-116.661996738861)) ;
#81734 = CARTESIAN_POINT('Origin',(337.26078686942,-86.4272893413486,-116.693246738861)) ;
#81735 = CARTESIAN_POINT('',(337.29203686942,-85.1156363338383,-116.724496738861)) ;
#81736 = CARTESIAN_POINT('',(350.562870202711,-71.8448030004564,-129.99533007221)) ;
#81737 = CARTESIAN_POINT('',(337.29203686942,-83.7406363338383,-116.724496738861)) ;
#81738 = CARTESIAN_POINT('',(337.29203686942,-86.4272893413486,-116.724496738861)) ;
#81739 = CARTESIAN_POINT('',(337.26078686942,-83.7093863338386,-116.693246738861)) ;
#81740 = CARTESIAN_POINT('',(342.145921205259,-88.5945206696818,-121.578381074721)) ;
#81741 = CARTESIAN_POINT('',(336.813011368171,-84.1571618350851,-116.24547123761)) ;
#81742 = CARTESIAN_POINT('Origin',(337.29203686942,-83.7093863338383,-116.693246738862)) ;
#81743 = CARTESIAN_POINT('',(337.22953686942,-83.6781363338383,-116.724496738862)) ;
#81744 = CARTESIAN_POINT('',(332.833844701487,-79.282444165902,-121.120188906845)) ;
#81745 = CARTESIAN_POINT('',(337.29203686942,-83.6781363338383,-116.724496738862)) ;
#81746 = CARTESIAN_POINT('Origin',(124.292036869421,-91.6781363338482,-171.161996738861)) ;
#81747 = CARTESIAN_POINT('Origin',(337.29203686942,-85.1781363338387,-225.661996738861)) ;
#81748 = CARTESIAN_POINT('',(337.22953686942,-85.1781363338386,-197.786149746371)) ;
#81749 = CARTESIAN_POINT('',(329.29203686942,-85.1781363338387,-125.411996738862)) ;
#81750 = CARTESIAN_POINT('Origin',(329.29203686942,-85.1781363338387,-124.161996738862)) ;
#81751 = CARTESIAN_POINT('',(151.79203686942,-85.1781363338468,-125.411996738862)) ;
#81752 = CARTESIAN_POINT('Origin',(151.79203686942,-85.1781363338468,-124.161996738862)) ;
#81753 = CARTESIAN_POINT('',(151.79203686942,-85.1781363338471,-220.411996738862)) ;
#81754 = CARTESIAN_POINT('Origin',(151.79203686942,-85.1781363338471,-219.161996738862)) ;
#81755 = CARTESIAN_POINT('',(329.29203686942,-85.178136333839,-220.411996738862)) ;
#81756 = CARTESIAN_POINT('Origin',(329.29203686942,-85.178136333839,-219.161996738862)) ;
#81757 = CARTESIAN_POINT('',(241.79203686942,-85.1781363338428,-165.911996738862)) ;
#81758 = CARTESIAN_POINT('Origin',(241.79203686942,-85.1781363338428,-164.661996738862)) ;
#81759 = CARTESIAN_POINT('Origin',(337.29203686942,-83.6781363338383,-116.661996738861)) ;
#81760 = CARTESIAN_POINT('',(337.22953686942,-83.6781363338384,-143.286149746371)) ;
#81761 = CARTESIAN_POINT('',(329.29203686942,-83.6781363338387,-125.411996738862)) ;
#81762 = CARTESIAN_POINT('Origin',(329.29203686942,-83.6781363338387,-124.161996738862)) ;
#81763 = CARTESIAN_POINT('',(151.79203686942,-83.6781363338468,-125.411996738862)) ;
#81764 = CARTESIAN_POINT('Origin',(151.79203686942,-83.6781363338468,-124.161996738862)) ;
#81765 = CARTESIAN_POINT('',(151.79203686942,-83.6781363338471,-220.411996738862)) ;
#81766 = CARTESIAN_POINT('Origin',(151.79203686942,-83.6781363338471,-219.161996738862)) ;
#81767 = CARTESIAN_POINT('',(329.29203686942,-83.678136333839,-220.411996738862)) ;
#81768 = CARTESIAN_POINT('Origin',(329.29203686942,-83.678136333839,-219.161996738862)) ;
#81769 = CARTESIAN_POINT('',(241.79203686942,-83.6781363338428,-165.911996738862)) ;
#81770 = CARTESIAN_POINT('Origin',(241.79203686942,-83.6781363338428,-164.661996738862)) ;
#81771 = CARTESIAN_POINT('Origin',(337.26078686942,-85.1468863338386,-197.786149746371)) ;
#81772 = CARTESIAN_POINT('',(337.29203686942,-85.1156363338387,-225.599496738861)) ;
#81773 = CARTESIAN_POINT('',(341.813152533571,-80.5945206696563,-221.078381074684)) ;
#81774 = CARTESIAN_POINT('',(337.29203686942,-85.1156363338386,-197.786149746371)) ;
#81775 = CARTESIAN_POINT('Origin',(337.29203686942,-87.6764423488591,-169.91030275388)) ;
#81776 = CARTESIAN_POINT('',(337.29203686942,-83.7406363338387,-225.599496738861)) ;
#81777 = CARTESIAN_POINT('',(337.29203686942,-85.677289341349,-225.599496738861)) ;
#81778 = CARTESIAN_POINT('',(337.29203686942,-83.7406363338384,-143.286149746371)) ;
#81779 = CARTESIAN_POINT('Origin',(337.26078686942,-83.7093863338384,-143.286149746371)) ;
#81780 = CARTESIAN_POINT('',(351.31287020277,-97.761469667201,-211.578663405432)) ;
#81781 = CARTESIAN_POINT('Origin',(337.26078686942,-85.677289341349,-225.630746738861)) ;
#81782 = CARTESIAN_POINT('Origin',(241.79203686942,-90.1781363338429,-164.661996738862)) ;
#81783 = CARTESIAN_POINT('',(241.79203686942,-90.1781363338429,-165.911996738862)) ;
#81784 = CARTESIAN_POINT('Origin',(329.29203686942,-90.1781363338391,-219.161996738862)) ;
#81785 = CARTESIAN_POINT('',(329.29203686942,-90.1781363338391,-220.411996738862)) ;
#81786 = CARTESIAN_POINT('Origin',(151.79203686942,-90.1781363338472,-219.161996738862)) ;
#81787 = CARTESIAN_POINT('',(151.79203686942,-90.1781363338472,-220.411996738862)) ;
#81788 = CARTESIAN_POINT('Origin',(151.79203686942,-90.1781363338469,-124.161996738862)) ;
#81789 = CARTESIAN_POINT('',(151.79203686942,-90.1781363338469,-125.411996738862)) ;
#81790 = CARTESIAN_POINT('Origin',(329.29203686942,-90.1781363338388,-124.161996738862)) ;
#81791 = CARTESIAN_POINT('',(329.29203686942,-90.1781363338388,-125.411996738862)) ;
#81792 = CARTESIAN_POINT('',(0.,0.,0.)) ;
#81793 = CARTESIAN_POINT('',(0.,0.,0.)) ;
#81794 = CARTESIAN_POINT('',(0.,0.,0.)) ;
#81795 = CARTESIAN_POINT('',(0.,0.,0.)) ;
#81796 = CARTESIAN_POINT('',(0.,0.,0.)) ;
#81797 = CARTESIAN_POINT('Origin',(0.,0.,0.)) ;
#81798 = CARTESIAN_POINT('',(-1.5,-8.72474074125615E-16,0.656249999999997)) ;
#81799 = CARTESIAN_POINT('',(-1.5,-3.60730648712457E-16,0.593749999999997)) ;
#81800 = CARTESIAN_POINT('',(-1.5,-1.83697019872103E-16,0.)) ;
#81801 = CARTESIAN_POINT('',(0.778543926944327,-1.28213468630176,0.324759526419166)) ;
#81802 = CARTESIAN_POINT('Ctrl Pts',(-1.5,-2.39391839684799E-15,0.656249999999998)) ;
#81803 = CARTESIAN_POINT('Ctrl Pts',(-1.5,0.1607200270702,0.647321109607209)) ;
#81804 = CARTESIAN_POINT('Ctrl Pts',(-1.4741670211068,0.320634454503277,0.638436974749825)) ;
#81805 = CARTESIAN_POINT('Ctrl Pts',(-1.36283639967842,0.655239528350988,
0.619847803980508)) ;
#81806 = CARTESIAN_POINT('Ctrl Pts',(-1.26817721619372,0.823642853630126,
0.611052903272752)) ;
#81807 = CARTESIAN_POINT('Ctrl Pts',(-1.01524271305061,1.12213782029424,0.59059205946455)) ;
#81808 = CARTESIAN_POINT('Ctrl Pts',(-0.856944680450145,1.24721443035943,
0.579501591540454)) ;
#81809 = CARTESIAN_POINT('Ctrl Pts',(-0.507462070287139,1.42457367000859,
0.557760456073417)) ;
#81810 = CARTESIAN_POINT('Ctrl Pts',(-0.320951378192811,1.47781505723871,
0.547308028793073)) ;
#81811 = CARTESIAN_POINT('Ctrl Pts',(0.0666309309435816,1.51138923147558,
0.527727850299295)) ;
#81812 = CARTESIAN_POINT('Ctrl Pts',(0.264147146078897,1.48962397255287,0.518252991524167)) ;
#81813 = CARTESIAN_POINT('Ctrl Pts',(0.639980871457319,1.37089218869411,0.496872577873832)) ;
#81814 = CARTESIAN_POINT('Ctrl Pts',(0.814538593466314,1.27492978139909,0.485808543133052)) ;
#81815 = CARTESIAN_POINT('Ctrl Pts',(1.11103575990294,1.02555152867983,0.464616142875061)) ;
#81816 = CARTESIAN_POINT('Ctrl Pts',(1.23191971314068,0.876637017425266,0.454952056523631)) ;
#81817 = CARTESIAN_POINT('Ctrl Pts',(1.41577752646327,0.533957385879126,0.435914299215511)) ;
#81818 = CARTESIAN_POINT('Ctrl Pts',(1.47399821495026,0.341819854608497,0.425239991922698)) ;
#81819 = CARTESIAN_POINT('Ctrl Pts',(1.51178732396369,-0.0501021196454836,
0.403466548908587)) ;
#81820 = CARTESIAN_POINT('Ctrl Pts',(1.49248613525052,-0.245976760588441,
0.392584624411756)) ;
#81821 = CARTESIAN_POINT('Ctrl Pts',(1.38414872473132,-0.605597575963239,
0.372605690224267)) ;
#81822 = CARTESIAN_POINT('Ctrl Pts',(1.30127330020684,-0.767657852056223,
0.364200378289862)) ;
#81823 = CARTESIAN_POINT('Ctrl Pts',(1.07817949622543,-1.05942775932347,0.345362052994947)) ;
#81824 = CARTESIAN_POINT('Ctrl Pts',(0.938095211434252,-1.18525119589866,
0.335127149240069)) ;
#81825 = CARTESIAN_POINT('Ctrl Pts',(0.778543926944331,-1.28213468630175,
0.324759526419165)) ;
#81826 = CARTESIAN_POINT('',(1.46053184144302,-0.34182852445499,0.324759526419167)) ;
#81827 = CARTESIAN_POINT('Origin',(0.,0.,0.324759526419167)) ;
#81828 = CARTESIAN_POINT('Ctrl Pts',(1.46053184144283,-0.3418285244558,0.32475952641912)) ;
#81829 = CARTESIAN_POINT('Ctrl Pts',(1.48363731923417,-0.243105674805563,
0.330244129177467)) ;
#81830 = CARTESIAN_POINT('Ctrl Pts',(1.49667194701901,-0.142307929062366,
0.335844003941008)) ;
#81831 = CARTESIAN_POINT('Ctrl Pts',(1.50221691376025,0.0606643103737226,
0.347120239465234)) ;
#81832 = CARTESIAN_POINT('Ctrl Pts',(1.49465417855031,0.162313399979073,0.352767411109976)) ;
#81833 = CARTESIAN_POINT('Ctrl Pts',(1.44242100214408,0.456280577716692,0.369098920984288)) ;
#81834 = CARTESIAN_POINT('Ctrl Pts',(1.37015036039608,0.641424489494071,0.378979290313343)) ;
#81835 = CARTESIAN_POINT('Ctrl Pts',(1.16119559714889,0.96864281127129,0.398122028874589)) ;
#81836 = CARTESIAN_POINT('Ctrl Pts',(1.02824815461798,1.10875059589915,0.408410348592026)) ;
#81837 = CARTESIAN_POINT('Ctrl Pts',(0.710844326433935,1.33575618782009,0.429987158282374)) ;
#81838 = CARTESIAN_POINT('Ctrl Pts',(0.527686779618663,1.41813255022657,0.441087562151267)) ;
#81839 = CARTESIAN_POINT('Ctrl Pts',(0.145663306121761,1.50533022648136,0.461889832763359)) ;
#81840 = CARTESIAN_POINT('Ctrl Pts',(-0.0489530922816456,1.51156802005474,
0.470783922860158)) ;
#81841 = CARTESIAN_POINT('Ctrl Pts',(-0.430582684445121,1.44985830492366,
0.490859243927657)) ;
#81842 = CARTESIAN_POINT('Ctrl Pts',(-0.613925254356179,1.38223457637478,
0.501558754339464)) ;
#81843 = CARTESIAN_POINT('Ctrl Pts',(-0.949244480379525,1.17833725920884,
0.523355622489269)) ;
#81844 = CARTESIAN_POINT('Ctrl Pts',(-1.09694604083355,1.04224392432656,0.53424228754332)) ;
#81845 = CARTESIAN_POINT('Ctrl Pts',(-1.32547379116904,0.727490619845216,
0.55398048140448)) ;
#81846 = CARTESIAN_POINT('Ctrl Pts',(-1.40689368697929,0.553880965707191,
0.562978835238514)) ;
#81847 = CARTESIAN_POINT('Ctrl Pts',(-1.48452734965408,0.248571106902,0.579940494061024)) ;
#81848 = CARTESIAN_POINT('Ctrl Pts',(-1.5,0.124386408551049,0.586839643969384)) ;
#81849 = CARTESIAN_POINT('Ctrl Pts',(-1.5,1.38777878078145E-16,0.593749999999997)) ;
#81850 = CARTESIAN_POINT('Origin',(0.,0.,0.)) ;
#81851 = CARTESIAN_POINT('',(-1.5,3.25616779869919E-15,1.15625)) ;
#81852 = CARTESIAN_POINT('',(-1.5,-1.11533536076237E-15,1.09375)) ;
#81853 = CARTESIAN_POINT('',(-1.5,-1.83697019872103E-16,0.)) ;
#81854 = CARTESIAN_POINT('Ctrl Pts',(-1.5,6.1409211049579E-15,1.15625)) ;
#81855 = CARTESIAN_POINT('Ctrl Pts',(-1.5,0.189806105391236,1.14570521636715)) ;
#81856 = CARTESIAN_POINT('Ctrl Pts',(-1.46397304873954,0.377951075523363,
1.13525271802649)) ;
#81857 = CARTESIAN_POINT('Ctrl Pts',(-1.3222161587587,0.734327472585592,1.11545402930081)) ;
#81858 = CARTESIAN_POINT('Ctrl Pts',(-1.21650652238285,0.898670433729232,
1.10648279641048)) ;
#81859 = CARTESIAN_POINT('Ctrl Pts',(-0.945002587646155,1.1816907098443,1.08555838292342)) ;
#81860 = CARTESIAN_POINT('Ctrl Pts',(-0.780467079717811,1.29625862406437,
1.07445972254562)) ;
#81861 = CARTESIAN_POINT('Ctrl Pts',(-0.423205968198729,1.45169093957452,
1.05295342498368)) ;
#81862 = CARTESIAN_POINT('Ctrl Pts',(-0.235004329546768,1.49375558567739,
1.04273010703046)) ;
#81863 = CARTESIAN_POINT('Ctrl Pts',(0.154749090124977,1.50518049501528,1.02366072829066)) ;
#81864 = CARTESIAN_POINT('Ctrl Pts',(0.352687859447389,1.47145138342095,1.01348828032349)) ;
#81865 = CARTESIAN_POINT('Ctrl Pts',(0.721375141428468,1.3296905992613,0.991812005638621)) ;
#81866 = CARTESIAN_POINT('Ctrl Pts',(0.888858008163141,1.22408904482572,0.980820605943696)) ;
#81867 = CARTESIAN_POINT('Ctrl Pts',(1.16923496541125,0.958636529157075,0.959957282307752)) ;
#81868 = CARTESIAN_POINT('Ctrl Pts',(1.28110302387416,0.80302881514754,0.950862711952652)) ;
#81869 = CARTESIAN_POINT('Ctrl Pts',(1.44459447450888,0.450228209630156,0.931262678312795)) ;
#81870 = CARTESIAN_POINT('Ctrl Pts',(1.49148846155318,0.254951726388306,0.920413984799357)) ;
#81871 = CARTESIAN_POINT('Ctrl Pts',(1.50621480594731,-0.137478762899289,
0.898612290950045)) ;
#81872 = CARTESIAN_POINT('Ctrl Pts',(1.47585978575147,-0.33080834689361,0.887871758505916)) ;
#81873 = CARTESIAN_POINT('Ctrl Pts',(1.34374220319785,-0.693812003860026,
0.867704888674449)) ;
#81874 = CARTESIAN_POINT('Ctrl Pts',(1.24378584267304,-0.860242010169573,
0.858862729529871)) ;
#81875 = CARTESIAN_POINT('Ctrl Pts',(0.981871506228363,-1.15134823900421,
0.838175086007994)) ;
#81876 = CARTESIAN_POINT('Ctrl Pts',(0.820487582424932,-1.27140244037549,
0.82707565942678)) ;
#81877 = CARTESIAN_POINT('Ctrl Pts',(0.467093846979265,-1.438245245513,0.805438473037725)) ;
#81878 = CARTESIAN_POINT('Ctrl Pts',(0.279686633416262,-1.48610985160416,
0.795092266879746)) ;
#81879 = CARTESIAN_POINT('Ctrl Pts',(-0.109993306164626,-1.50909510092276,
0.775705302897438)) ;
#81880 = CARTESIAN_POINT('Ctrl Pts',(-0.308690063405629,-1.48128448585284,
0.765878267006745)) ;
#81881 = CARTESIAN_POINT('Ctrl Pts',(-0.681837802149646,-1.35047446149059,
0.744291576267959)) ;
#81882 = CARTESIAN_POINT('Ctrl Pts',(-0.852850201293791,-1.24953248569501,
0.733259794605807)) ;
#81883 = CARTESIAN_POINT('Ctrl Pts',(-1.14114328313784,-0.991903517435437,
0.712232927009028)) ;
#81884 = CARTESIAN_POINT('Ctrl Pts',(-1.25742060362583,-0.839613205476229,
0.702895178082022)) ;
#81885 = CARTESIAN_POINT('Ctrl Pts',(-1.43098751048226,-0.491755446248058,
0.683569747013789)) ;
#81886 = CARTESIAN_POINT('Ctrl Pts',(-1.48349456128071,-0.297942723678847,
0.672802373537721)) ;
#81887 = CARTESIAN_POINT('Ctrl Pts',(-1.49889952124722,-0.0663817994101106,
0.659937877745013)) ;
#81888 = CARTESIAN_POINT('Ctrl Pts',(-1.5,-0.0331737388818849,0.658092985493435)) ;
#81889 = CARTESIAN_POINT('Ctrl Pts',(-1.5,-2.37984979295154E-15,0.656249999999997)) ;
#81890 = CARTESIAN_POINT('Ctrl Pts',(-1.5,2.97483362866747E-16,0.593749999999998)) ;
#81891 = CARTESIAN_POINT('Ctrl Pts',(-1.5,-0.0705859863589315,0.597671443686605)) ;
#81892 = CARTESIAN_POINT('Ctrl Pts',(-1.4950177408892,-0.141236928673874,
0.601596496037459)) ;
#81893 = CARTESIAN_POINT('Ctrl Pts',(-1.45699567168959,-0.408302331935193,
0.616433462885309)) ;
#81894 = CARTESIAN_POINT('Ctrl Pts',(-1.39010246512636,-0.597586788383109,
0.626801630307176)) ;
#81895 = CARTESIAN_POINT('Ctrl Pts',(-1.19056528868096,-0.932189699523634,
0.645696392494476)) ;
#81896 = CARTESIAN_POINT('Ctrl Pts',(-1.06244257795823,-1.07592532097647,
0.655853355439699)) ;
#81897 = CARTESIAN_POINT('Ctrl Pts',(-0.753373782602369,-1.31214212345324,
0.677285012636009)) ;
#81898 = CARTESIAN_POINT('Ctrl Pts',(-0.573575272037589,-1.40010946284613,
0.688379109714239)) ;
#81899 = CARTESIAN_POINT('Ctrl Pts',(-0.193917233490111,-1.50005780821647,
0.709421758537475)) ;
#81900 = CARTESIAN_POINT('Ctrl Pts',(0.0018330599722723,-1.51253682526368,
0.718489947992844)) ;
#81901 = CARTESIAN_POINT('Ctrl Pts',(0.385955527725803,-1.46229454874621,
0.738366667631604)) ;
#81902 = CARTESIAN_POINT('Ctrl Pts',(0.570728475938215,-1.40054270181248,
0.748971889328879)) ;
#81903 = CARTESIAN_POINT('Ctrl Pts',(0.913371471429655,-1.20666008869792,
0.770842936277859)) ;
#81904 = CARTESIAN_POINT('Ctrl Pts',(1.06645766524887,-1.07376035622208,0.781899958447527)) ;
#81905 = CARTESIAN_POINT('Ctrl Pts',(1.30497513749981,-0.763741406097344,
0.801987273185199)) ;
#81906 = CARTESIAN_POINT('Ctrl Pts',(1.39128549698088,-0.592107607993041,
0.810855132889296)) ;
#81907 = CARTESIAN_POINT('Ctrl Pts',(1.49643461481373,-0.220970650242353,
0.831473852764334)) ;
#81908 = CARTESIAN_POINT('Ctrl Pts',(1.51246123111777,-0.0244681350068359,
0.842390659166306)) ;
#81909 = CARTESIAN_POINT('Ctrl Pts',(1.46791659667496,0.367046590015983,0.864141477223129)) ;
#81910 = CARTESIAN_POINT('Ctrl Pts',(1.40641810169146,0.558136775334782,0.874757598629729)) ;
#81911 = CARTESIAN_POINT('Ctrl Pts',(1.21663220344887,0.897775488161019,0.893626416008965)) ;
#81912 = CARTESIAN_POINT('Ctrl Pts',(1.09304305016181,1.04474874788435,0.903515073615133)) ;
#81913 = CARTESIAN_POINT('Ctrl Pts',(0.791766360539703,1.28924912967893,0.924801932375028)) ;
#81914 = CARTESIAN_POINT('Ctrl Pts',(0.61519892799247,1.38224129434414,0.935880152619445)) ;
#81915 = CARTESIAN_POINT('Ctrl Pts',(0.237878641222853,1.49391270346963,0.957135966967693)) ;
#81916 = CARTESIAN_POINT('Ctrl Pts',(0.0410377219212674,1.51217248608932,
0.966437447069915)) ;
#81917 = CARTESIAN_POINT('Ctrl Pts',(-0.345272897341869,1.47236296906486,
0.986129645322456)) ;
#81918 = CARTESIAN_POINT('Ctrl Pts',(-0.531180586185464,1.41594320328274,
0.99664134888848)) ;
#81919 = CARTESIAN_POINT('Ctrl Pts',(-0.878202474401868,1.23239540808013,
1.01843599713659)) ;
#81920 = CARTESIAN_POINT('Ctrl Pts',(-1.03460132686121,1.10437888698023,1.02951675490895)) ;
#81921 = CARTESIAN_POINT('Ctrl Pts',(-1.28218302036428,0.801557459123725,
1.04984024102083)) ;
#81922 = CARTESIAN_POINT('Ctrl Pts',(-1.37372075766342,0.631966212932787,
1.05864076594819)) ;
#81923 = CARTESIAN_POINT('Ctrl Pts',(-1.4768043966045,0.303965309506325,1.07686303836077)) ;
#81924 = CARTESIAN_POINT('Ctrl Pts',(-1.5,0.152295076973703,1.08528916239035)) ;
#81925 = CARTESIAN_POINT('Ctrl Pts',(-1.5,-3.40005801291454E-15,1.09375)) ;
#81926 = CARTESIAN_POINT('Origin',(0.,0.,0.)) ;
#81927 = CARTESIAN_POINT('',(-1.5,2.72443420019078E-16,1.65625)) ;
#81928 = CARTESIAN_POINT('',(-1.5,2.61432011258777E-15,1.59375)) ;
#81929 = CARTESIAN_POINT('',(-1.5,-1.83697019872103E-16,0.)) ;
#81930 = CARTESIAN_POINT('Ctrl Pts',(-1.5,2.52859025224331E-15,1.65625)) ;
#81931 = CARTESIAN_POINT('Ctrl Pts',(-1.5,0.0269229379010869,1.65475428122771)) ;
#81932 = CARTESIAN_POINT('Ctrl Pts',(-1.49927516504667,0.0538717048422698,
1.65325712750878)) ;
#81933 = CARTESIAN_POINT('Ctrl Pts',(-1.48746761788753,0.272705869696385,
1.64109967390577)) ;
#81934 = CARTESIAN_POINT('Ctrl Pts',(-1.44033365134678,0.460854217967074,
1.63064698789073)) ;
#81935 = CARTESIAN_POINT('Ctrl Pts',(-1.27564436649753,0.813306103094172,
1.6110663276059)) ;
#81936 = CARTESIAN_POINT('Ctrl Pts',(-1.158051507112,0.97348254049987,1.60159226410001)) ;
#81937 = CARTESIAN_POINT('Ctrl Pts',(-0.867332870775922,1.23961897270468,
1.5802123785154)) ;
#81938 = CARTESIAN_POINT('Ctrl Pts',(-0.69695471868813,1.3428230629645,1.56914827556607)) ;
#81939 = CARTESIAN_POINT('Ctrl Pts',(-0.332746010733414,1.47493620037078,
1.5479554665621)) ;
#81940 = CARTESIAN_POINT('Ctrl Pts',(-0.143341745701085,1.50518173240013,
1.53829046996668)) ;
#81941 = CARTESIAN_POINT('Ctrl Pts',(0.245357930273443,1.49309609456688,1.51925343592483)) ;
#81942 = CARTESIAN_POINT('Ctrl Pts',(0.440867536333831,1.44746237525733,1.50857937230333)) ;
#81943 = CARTESIAN_POINT('Ctrl Pts',(0.799189721411461,1.28425366185876,1.48680601276355)) ;
#81944 = CARTESIAN_POINT('Ctrl Pts',(0.959181015582752,1.16961179356638,1.47592393169228)) ;
#81945 = CARTESIAN_POINT('Ctrl Pts',(1.22342689292453,0.888601187059828,1.45540454581025)) ;
#81946 = CARTESIAN_POINT('Ctrl Pts',(1.32637707938175,0.726020437393559,1.4465844687441)) ;
#81947 = CARTESIAN_POINT('Ctrl Pts',(1.46939559633561,0.36198147466264,1.42636008192572)) ;
#81948 = CARTESIAN_POINT('Ctrl Pts',(1.50455005374878,0.162688114647428,1.41528822859153)) ;
#81949 = CARTESIAN_POINT('Ctrl Pts',(1.49469916815378,-0.230234719873201,
1.39345918222928)) ;
#81950 = CARTESIAN_POINT('Ctrl Pts',(1.4527919325684,-0.420174405384774,1.38290697747864)) ;
#81951 = CARTESIAN_POINT('Ctrl Pts',(1.29839962557302,-0.776049202454666,
1.3631361554192)) ;
#81952 = CARTESIAN_POINT('Ctrl Pts',(1.18653192056656,-0.938213766586564,
1.35394221679549)) ;
#81953 = CARTESIAN_POINT('Ctrl Pts',(0.904968657590171,-1.21251461247927,
1.33277603004791)) ;
#81954 = CARTESIAN_POINT('Ctrl Pts',(0.73729361318162,-1.32119397820188,1.32168988944237)) ;
#81955 = CARTESIAN_POINT('Ctrl Pts',(0.376231824750659,-1.46450418670203,
1.30033745692197)) ;
#81956 = CARTESIAN_POINT('Ctrl Pts',(0.187372068618979,-1.50038585439249,
1.29027566103224)) ;
#81957 = CARTESIAN_POINT('Ctrl Pts',(-0.201866281378398,-1.49959079808594,
1.271526337289)) ;
#81958 = CARTESIAN_POINT('Ctrl Pts',(-0.39858166171527,-1.45966713696413,
1.26095287355302)) ;
#81959 = CARTESIAN_POINT('Ctrl Pts',(-0.76197337545374,-1.30676058906481,
1.23922177746569)) ;
#81960 = CARTESIAN_POINT('Ctrl Pts',(-0.925640847229525,-1.19642033877903,
1.22828231560602)) ;
#81961 = CARTESIAN_POINT('Ctrl Pts',(-1.19770027094282,-0.922883848769447,
1.20759461464605)) ;
#81962 = CARTESIAN_POINT('Ctrl Pts',(-1.30496242672345,-0.763718567813794,
1.198678809323)) ;
#81963 = CARTESIAN_POINT('Ctrl Pts',(-1.45770502735446,-0.405787189141501,
1.1787937327301)) ;
#81964 = CARTESIAN_POINT('Ctrl Pts',(-1.4986024017048,-0.209141325247903,
1.16786896251378)) ;
#81965 = CARTESIAN_POINT('Ctrl Pts',(-1.49998827054254,-0.00685020096107011,
1.15663056672007)) ;
#81966 = CARTESIAN_POINT('Ctrl Pts',(-1.5,-0.00342483006433634,1.15644026833691)) ;
#81967 = CARTESIAN_POINT('Ctrl Pts',(-1.5,6.247106623104E-15,1.15625)) ;
#81968 = CARTESIAN_POINT('Ctrl Pts',(-1.5,-3.30950241189258E-15,1.09375)) ;
#81969 = CARTESIAN_POINT('Ctrl Pts',(-1.5,-0.0418239384105527,1.09607355213392)) ;
#81970 = CARTESIAN_POINT('Ctrl Pts',(-1.49825079600136,-0.0836950016768401,
1.09839972231539)) ;
#81971 = CARTESIAN_POINT('Ctrl Pts',(-1.4781077032983,-0.323597595814322,
1.11172764421192)) ;
#81972 = CARTESIAN_POINT('Ctrl Pts',(-1.42225800040326,-0.516453274940869,
1.12244184860784)) ;
#81973 = CARTESIAN_POINT('Ctrl Pts',(-1.24267625242295,-0.86130018627444,
1.14160001034859)) ;
#81974 = CARTESIAN_POINT('Ctrl Pts',(-1.12371979539634,-1.01161623082117,
1.15111879032567)) ;
#81975 = CARTESIAN_POINT('Ctrl Pts',(-0.830646029950509,-1.26445563596451,
1.17224262524959)) ;
#81976 = CARTESIAN_POINT('Ctrl Pts',(-0.657553280567444,-1.36251432324379,
1.18329440646161)) ;
#81977 = CARTESIAN_POINT('Ctrl Pts',(-0.282819454972746,-1.48629234946708,
1.20476207455794)) ;
#81978 = CARTESIAN_POINT('Ctrl Pts',(-0.0848134752949405,-1.51057549585254,
1.21437564599363)) ;
#81979 = CARTESIAN_POINT('Ctrl Pts',(0.303657029036045,-1.4814369520598,1.23387534584185)) ;
#81980 = CARTESIAN_POINT('Ctrl Pts',(0.490562705267345,-1.43045141647857,
1.24428411425954)) ;
#81981 = CARTESIAN_POINT('Ctrl Pts',(0.841724617985318,-1.25749715628138,
1.26598368466809)) ;
#81982 = CARTESIAN_POINT('Ctrl Pts',(1.00133669730154,-1.13452023771357,1.27707904993045)) ;
#81983 = CARTESIAN_POINT('Ctrl Pts',(1.25804932273866,-0.839114472837687,
1.29763585757149)) ;
#81984 = CARTESIAN_POINT('Ctrl Pts',(1.35492854746899,-0.671542838127837,
1.30644206454847)) ;
#81985 = CARTESIAN_POINT('Ctrl Pts',(1.48109817934729,-0.306699476178405,
1.32671114021232)) ;
#81986 = CARTESIAN_POINT('Ctrl Pts',(1.50832038413776,-0.112580848819781,
1.33749550839891)) ;
#81987 = CARTESIAN_POINT('Ctrl Pts',(1.48701678921495,0.27984357135668,1.35929686507538)) ;
#81988 = CARTESIAN_POINT('Ctrl Pts',(1.43687108102397,0.474293788638321,1.37009965492436)) ;
#81989 = CARTESIAN_POINT('Ctrl Pts',(1.26754574646804,0.824247894447991,1.38954154969156)) ;
#81990 = CARTESIAN_POINT('Ctrl Pts',(1.15313619452512,0.977932993631929,1.39876784768523)) ;
#81991 = CARTESIAN_POINT('Ctrl Pts',(0.868189736426075,1.23888540915647,1.41972601875158)) ;
#81992 = CARTESIAN_POINT('Ctrl Pts',(0.698656891662839,1.34181485641221,1.43074182286096)) ;
#81993 = CARTESIAN_POINT('Ctrl Pts',(0.326654853270976,1.47753710554394,1.45240984175389)) ;
#81994 = CARTESIAN_POINT('Ctrl Pts',(0.127470830452023,1.50782568461737,1.46239967668215)) ;
#81995 = CARTESIAN_POINT('Ctrl Pts',(-0.26303471783684,1.48912044873026,1.48170747351995)) ;
#81996 = CARTESIAN_POINT('Ctrl Pts',(-0.450759234289304,1.44342001010308,
1.49200883015742)) ;
#81997 = CARTESIAN_POINT('Ctrl Pts',(-0.80563852961626,1.28082682702653,1.51359944552234)) ;
#81998 = CARTESIAN_POINT('Ctrl Pts',(-0.968219833275402,1.16281145361195,
1.52469984695881)) ;
#81999 = CARTESIAN_POINT('Ctrl Pts',(-1.23372369758581,0.874707136645695,
1.54547680527986)) ;
#82000 = CARTESIAN_POINT('Ctrl Pts',(-1.33582095620383,0.709060508116284,
1.5543577495491)) ;
#82001 = CARTESIAN_POINT('Ctrl Pts',(-1.46744352783767,0.359516168214211,
1.57377687954366)) ;
#82002 = CARTESIAN_POINT('Ctrl Pts',(-1.5,0.180429519935487,1.58372613778136)) ;
#82003 = CARTESIAN_POINT('Ctrl Pts',(-1.5,8.11850586757146E-15,1.59375)) ;
#82004 = CARTESIAN_POINT('Origin',(0.,0.,0.)) ;
#82005 = CARTESIAN_POINT('',(-1.5,-2.58117669796277E-15,2.15625)) ;
#82006 = CARTESIAN_POINT('',(-1.5,2.9582133382325E-17,2.09375)) ;
#82007 = CARTESIAN_POINT('',(-1.5,-1.83697019872103E-16,0.)) ;
#82008 = CARTESIAN_POINT('Ctrl Pts',(-1.5,-2.52859025224331E-15,2.15625)) ;
#82009 = CARTESIAN_POINT('Ctrl Pts',(-1.5,0.0546162866586652,2.15321576185229)) ;
#82010 = CARTESIAN_POINT('Ctrl Pts',(-1.49701714440264,0.10929679695477,2.15017795572474)) ;
#82011 = CARTESIAN_POINT('Ctrl Pts',(-1.4701572983793,0.353799631349553,2.13659446492503)) ;
#82012 = CARTESIAN_POINT('Ctrl Pts',(-1.41315423719555,0.538102637111959,
2.12635540904934)) ;
#82013 = CARTESIAN_POINT('Ctrl Pts',(-1.22854362231576,0.883699336998718,
2.10715559238897)) ;
#82014 = CARTESIAN_POINT('Ctrl Pts',(-1.09945939121703,1.03993932239023,2.09692722789047)) ;
#82015 = CARTESIAN_POINT('Ctrl Pts',(-0.790949993784533,1.28951844902538,
2.07515130906822)) ;
#82016 = CARTESIAN_POINT('Ctrl Pts',(-0.61576020033871,1.38177511072207,2.06415980115399)) ;
#82017 = CARTESIAN_POINT('Ctrl Pts',(-0.245689765772974,1.49188833445163,
2.04329607841019)) ;
#82018 = CARTESIAN_POINT('Ctrl Pts',(-0.0549972007493365,1.51097828870566,
2.03420100651883)) ;
#82019 = CARTESIAN_POINT('Ctrl Pts',(0.332284786771767,1.47619288546302,2.01460163200534)) ;
#82020 = CARTESIAN_POINT('Ctrl Pts',(0.524850107878419,1.41917953426664,2.00375312447399)) ;
#82021 = CARTESIAN_POINT('Ctrl Pts',(0.872082013459065,1.23574144606107,1.98195141917731)) ;
#82022 = CARTESIAN_POINT('Ctrl Pts',(1.0243423375181,1.11279807140185,1.97121069717992)) ;
#82023 = CARTESIAN_POINT('Ctrl Pts',(1.27267313163213,0.816896771103869,1.9510433957136)) ;
#82024 = CARTESIAN_POINT('Ctrl Pts',(1.36683819762821,0.647125879280804,1.94220143773783)) ;
#82025 = CARTESIAN_POINT('Ctrl Pts',(1.48801309414954,0.274758127034861,1.92151434039083)) ;
#82026 = CARTESIAN_POINT('Ctrl Pts',(1.51130549846425,0.0749686380007088,
1.91041492433338)) ;
#82027 = CARTESIAN_POINT('Ctrl Pts',(1.47912566370554,-0.314505661155098,
1.88877746326917)) ;
#82028 = CARTESIAN_POINT('Ctrl Pts',(1.42688641091888,-0.500742210877754,
1.87843098828458)) ;
#82029 = CARTESIAN_POINT('Ctrl Pts',(1.25197726548271,-0.849716174972452,
1.85904354583488)) ;
#82030 = CARTESIAN_POINT('Ctrl Pts',(1.12855862548595,-1.00789224699645,1.84921746199072)) ;
#82031 = CARTESIAN_POINT('Ctrl Pts',(0.828722297248183,-1.2656634598045,1.82763126845541)) ;
#82032 = CARTESIAN_POINT('Ctrl Pts',(0.65580381773927,-1.36330731114237,1.81659939502722)) ;
#82033 = CARTESIAN_POINT('Ctrl Pts',(0.288551400119727,-1.48418959168278,
1.79557211372)) ;
#82034 = CARTESIAN_POINT('Ctrl Pts',(0.0985270817800627,-1.50875755782986,
1.78623365192763)) ;
#82035 = CARTESIAN_POINT('Ctrl Pts',(-0.289511811254275,-1.4851705482752,
1.76690892727199)) ;
#82036 = CARTESIAN_POINT('Ctrl Pts',(-0.483615784390812,-1.43375092662312,
1.75614177268656)) ;
#82037 = CARTESIAN_POINT('Ctrl Pts',(-0.836465693283654,-1.26020606783978,
1.73434458300791)) ;
#82038 = CARTESIAN_POINT('Ctrl Pts',(-0.992594535458914,-1.14129789894949,
1.723529825895)) ;
#82039 = CARTESIAN_POINT('Ctrl Pts',(-1.24881041653316,-0.852721314778345,
1.70318661734228)) ;
#82040 = CARTESIAN_POINT('Ctrl Pts',(-1.34733341302686,-0.686551437019409,
1.69439174650109)) ;
#82041 = CARTESIAN_POINT('Ctrl Pts',(-1.47028769977342,-0.343671917814022,
1.67534288432301)) ;
#82042 = CARTESIAN_POINT('Ctrl Pts',(-1.5,-0.172365296862037,1.66582584982566)) ;
#82043 = CARTESIAN_POINT('Ctrl Pts',(-1.5,2.25514051876985E-15,1.65625)) ;
#82044 = CARTESIAN_POINT('Ctrl Pts',(-1.5,7.54864033274375E-15,1.59375)) ;
#82045 = CARTESIAN_POINT('Ctrl Pts',(-1.5,-0.0129956598470896,1.59447198110261)) ;
#82046 = CARTESIAN_POINT('Ctrl Pts',(-1.4998311134522,-0.0259982862158395,
1.59519434923422)) ;
#82047 = CARTESIAN_POINT('Ctrl Pts',(-1.49432199544045,-0.237790581132439,
1.6069605878407)) ;
#82048 = CARTESIAN_POINT('Ctrl Pts',(-1.44967258468572,-0.433602909230278,
1.6178390505128)) ;
#82049 = CARTESIAN_POINT('Ctrl Pts',(-1.29020513942681,-0.788341747578342,
1.63754676375435)) ;
#82050 = CARTESIAN_POINT('Ctrl Pts',(-1.18007256202236,-0.945278838891628,
1.64656481124586)) ;
#82051 = CARTESIAN_POINT('Ctrl Pts',(-0.902824846038532,-1.2137886544314,
1.6673625041877)) ;
#82052 = CARTESIAN_POINT('Ctrl Pts',(-0.736765013385657,-1.32119210250901,
1.67833549072461)) ;
#82053 = CARTESIAN_POINT('Ctrl Pts',(-0.369999760342863,-1.46719105679223,
1.70003701869695)) ;
#82054 = CARTESIAN_POINT('Ctrl Pts',(-0.172499063470922,-1.50324432377842,
1.71036051483423)) ;
#82055 = CARTESIAN_POINT('Ctrl Pts',(0.217098298309571,-1.49643436804736,
1.7292941920795)) ;
#82056 = CARTESIAN_POINT('Ctrl Pts',(0.405567626217661,-1.4566876028183,1.73946600365822)) ;
#82057 = CARTESIAN_POINT('Ctrl Pts',(0.764272895356052,-1.30583450988432,
1.7609145826589)) ;
#82058 = CARTESIAN_POINT('Ctrl Pts',(0.930016830917273,-1.19347891965801,
1.77200993009403)) ;
#82059 = CARTESIAN_POINT('Ctrl Pts',(1.20532717911403,-0.913728422884884,
1.79302665253012)) ;
#82060 = CARTESIAN_POINT('Ctrl Pts',(1.31335149919757,-0.750210145417528,
1.80207165858792)) ;
#82061 = CARTESIAN_POINT('Ctrl Pts',(1.46068461359121,-0.392035362147135,
1.8219702576585)) ;
#82062 = CARTESIAN_POINT('Ctrl Pts',(1.49896468002721,-0.200948327247076,
1.83258620404183)) ;
#82063 = CARTESIAN_POINT('Ctrl Pts',(1.50103431974765,0.192875182678861,1.85446528792661)) ;
#82064 = CARTESIAN_POINT('Ctrl Pts',(1.46177450149586,0.391838905988002,1.86551882811045)) ;
#82065 = CARTESIAN_POINT('Ctrl Pts',(1.31125661025412,0.752891371694118,1.88557729842745)) ;
#82066 = CARTESIAN_POINT('Ctrl Pts',(1.20524243635297,0.913036805574294,1.89445821306591)) ;
#82067 = CARTESIAN_POINT('Ctrl Pts',(0.935442584319375,1.18874637796397,1.91509756373221)) ;
#82068 = CARTESIAN_POINT('Ctrl Pts',(0.772829410305134,1.3003456666158,1.92602127395511)) ;
#82069 = CARTESIAN_POINT('Ctrl Pts',(0.410876996161621,1.45625561726341,1.94776654956251)) ;
#82070 = CARTESIAN_POINT('Ctrl Pts',(0.214493555574436,1.49783821050788,1.9583701242877)) ;
#82071 = CARTESIAN_POINT('Ctrl Pts',(-0.174599479057064,1.50190859994096,
1.97720343801786)) ;
#82072 = CARTESIAN_POINT('Ctrl Pts',(-0.363610770720251,1.46766903245709,
1.98714231379472)) ;
#82073 = CARTESIAN_POINT('Ctrl Pts',(-0.725602415935666,1.32762477447494,
2.00844876322279)) ;
#82074 = CARTESIAN_POINT('Ctrl Pts',(-0.894083220046043,1.22053486918689,
2.01952951928133)) ;
#82075 = CARTESIAN_POINT('Ctrl Pts',(-1.17832317452849,0.948597663829845,
2.04075883172748)) ;
#82076 = CARTESIAN_POINT('Ctrl Pts',(-1.29185235241837,0.78701312183995,2.05002704878667)) ;
#82077 = CARTESIAN_POINT('Ctrl Pts',(-1.44925948417428,0.432132132919838,
2.06974265928224)) ;
#82078 = CARTESIAN_POINT('Ctrl Pts',(-1.49270519361291,0.242702620053888,
2.08026652110812)) ;
#82079 = CARTESIAN_POINT('Ctrl Pts',(-1.49971956391621,0.0335040329801223,
2.09188866483444)) ;
#82080 = CARTESIAN_POINT('Ctrl Pts',(-1.5,0.016746278066708,2.09281965121851)) ;
#82081 = CARTESIAN_POINT('Ctrl Pts',(-1.5,2.71453568615908E-15,2.09375)) ;
#82082 = CARTESIAN_POINT('Origin',(0.,0.,0.)) ;
#82083 = CARTESIAN_POINT('',(-1.5,2.95259119040324E-15,2.65625)) ;
#82084 = CARTESIAN_POINT('',(-1.5,-2.17351668110822E-15,2.59374999999999)) ;
#82085 = CARTESIAN_POINT('',(-1.5,-1.83697019872103E-16,0.)) ;
#82086 = CARTESIAN_POINT('Ctrl Pts',(-1.5,4.90844004519485E-15,2.65625)) ;
#82087 = CARTESIAN_POINT('Ctrl Pts',(-1.5,0.0856151677731844,2.65149360179037)) ;
#82088 = CARTESIAN_POINT('Ctrl Pts',(-1.49267015243007,0.171275020595029,
2.64673472107806)) ;
#82089 = CARTESIAN_POINT('Ctrl Pts',(-1.44552368503536,0.443435938984391,
2.63161467005643)) ;
#82090 = CARTESIAN_POINT('Ctrl Pts',(-1.37772363683179,0.622905801337482,
2.62189948712345)) ;
#82091 = CARTESIAN_POINT('Ctrl Pts',(-1.17421465332585,0.954334641509284,
2.60290179991787)) ;
#82092 = CARTESIAN_POINT('Ctrl Pts',(-1.03753186268452,1.10137961099408,2.59224106360131)) ;
#82093 = CARTESIAN_POINT('Ctrl Pts',(-0.717891608916212,1.33141761329456,
2.57047242021322)) ;
#82094 = CARTESIAN_POINT('Ctrl Pts',(-0.538864177307172,1.41339116705685,
2.55958191573383)) ;
#82095 = CARTESIAN_POINT('Ctrl Pts',(-0.163728105175774,1.50317931500609,
2.53903905782737)) ;
#82096 = CARTESIAN_POINT('Ctrl Pts',(0.0284310311749173,1.51180110239942,
2.5302099197748)) ;
#82097 = CARTESIAN_POINT('Ctrl Pts',(0.415438810102884,1.45519666383705,2.51001765381397)) ;
#82098 = CARTESIAN_POINT('Ctrl Pts',(0.605959319102716,1.38671697207505,2.49894901789082)) ;
#82099 = CARTESIAN_POINT('Ctrl Pts',(0.942235074590785,1.18294306354376,2.47710955671331)) ;
#82100 = CARTESIAN_POINT('Ctrl Pts',(1.08632518335127,1.05217672404664,2.46654461980391)) ;
#82101 = CARTESIAN_POINT('Ctrl Pts',(1.31840597987018,0.741499024173853,2.44674869116767)) ;
#82102 = CARTESIAN_POINT('Ctrl Pts',(1.40351763898725,0.564058291685003,2.43758657176028)) ;
#82103 = CARTESIAN_POINT('Ctrl Pts',(1.50182787618189,0.183588868926401,2.41644938160702)) ;
#82104 = CARTESIAN_POINT('Ctrl Pts',(1.51292131336378,-0.0160007193501419,
2.40536107114722)) ;
#82105 = CARTESIAN_POINT('Ctrl Pts',(1.45801957138463,-0.400610722115376,
2.38399384877137)) ;
#82106 = CARTESIAN_POINT('Ctrl Pts',(1.39538669614711,-0.582434990200783,
2.37389250054441)) ;
#82107 = CARTESIAN_POINT('Ctrl Pts',(1.2013344585767,-0.919931291483191,2.35514270602872)) ;
#82108 = CARTESIAN_POINT('Ctrl Pts',(1.06900829993795,-1.07086927598327,2.34460298370062)) ;
#82109 = CARTESIAN_POINT('Ctrl Pts',(0.755658547689445,-1.31043320461103,
2.32287238314336)) ;
#82110 = CARTESIAN_POINT('Ctrl Pts',(0.578526738081543,-1.39770077925359,
2.31192602568447)) ;
#82111 = CARTESIAN_POINT('Ctrl Pts',(0.205950389837252,-1.49792085516064,
2.29121654677434)) ;
#82112 = CARTESIAN_POINT('Ctrl Pts',(0.0145779287054259,-1.51193972266469,
2.28228303988477)) ;
#82113 = CARTESIAN_POINT('Ctrl Pts',(-0.371893252832265,-1.46671798710535,
2.26243277717244)) ;
#82114 = CARTESIAN_POINT('Ctrl Pts',(-0.562875788981263,-1.40453509871487,
2.25151682316247)) ;
#82115 = CARTESIAN_POINT('Ctrl Pts',(-0.904622987191438,-1.21204236583417,
2.22972748306456)) ;
#82116 = CARTESIAN_POINT('Ctrl Pts',(-1.05318792417667,-1.08544895413135,
2.21906316554277)) ;
#82117 = CARTESIAN_POINT('Ctrl Pts',(-1.29410955375517,-0.782757285562262,
2.19906371633051)) ;
#82118 = CARTESIAN_POINT('Ctrl Pts',(-1.38416170816597,-0.609531542906844,
2.19011286349483)) ;
#82119 = CARTESIAN_POINT('Ctrl Pts',(-1.4794846403777,-0.286011580132301,
2.17213953222958)) ;
#82120 = CARTESIAN_POINT('Ctrl Pts',(-1.5,-0.143226625156057,2.16420703473089)) ;
#82121 = CARTESIAN_POINT('Ctrl Pts',(-1.5,-2.22044604925031E-15,2.15625)) ;
#82122 = CARTESIAN_POINT('Ctrl Pts',(-1.5,2.42861286636753E-15,2.09375)) ;
#82123 = CARTESIAN_POINT('Ctrl Pts',(-1.5,-0.183119263433166,2.10392329241295)) ;
#82124 = CARTESIAN_POINT('Ctrl Pts',(-1.46646507623563,-0.364866211108705,
2.1140203450616)) ;
#82125 = CARTESIAN_POINT('Ctrl Pts',(-1.33264810871975,-0.714495462261993,
2.13344419234789)) ;
#82126 = CARTESIAN_POINT('Ctrl Pts',(-1.23099892811952,-0.878122479994064,
2.14224916090078)) ;
#82127 = CARTESIAN_POINT('Ctrl Pts',(-0.969112872690051,-1.16136842759558,
2.16271710260632)) ;
#82128 = CARTESIAN_POINT('Ctrl Pts',(-0.810248162224439,-1.27728043816115,
2.17358026262359)) ;
#82129 = CARTESIAN_POINT('Ctrl Pts',(-0.453507260029782,-1.44355364633095,
2.19536266750995)) ;
#82130 = CARTESIAN_POINT('Ctrl Pts',(-0.258393502074163,-1.49089672958314,
2.20606516821237)) ;
#82131 = CARTESIAN_POINT('Ctrl Pts',(0.13012335116139,-1.50637293458213,2.22518758861236)) ;
#82132 = CARTESIAN_POINT('Ctrl Pts',(0.31970346636198,-1.47780726939408,2.23474820493614)) ;
#82133 = CARTESIAN_POINT('Ctrl Pts',(0.684825873911802,-1.34902317392027,
2.25589250094536)) ;
#82134 = CARTESIAN_POINT('Ctrl Pts',(0.855975079196342,-1.24746050606069,
2.26694810614223)) ;
#82135 = CARTESIAN_POINT('Ctrl Pts',(1.14940356144279,-0.983785017423248,
2.28839000970545)) ;
#82136 = CARTESIAN_POINT('Ctrl Pts',(1.26871450560737,-0.824200283726239,
2.29796109534854)) ;
#82137 = CARTESIAN_POINT('Ctrl Pts',(1.43644424776305,-0.472774642873999,
2.31748474206255)) ;
#82138 = CARTESIAN_POINT('Ctrl Pts',(1.48510597361535,-0.285181351989462,
2.32790659155614)) ;
#82139 = CARTESIAN_POINT('Ctrl Pts',(1.50952613238539,0.105638303090151,2.34961879461612)) ;
#82140 = CARTESIAN_POINT('Ctrl Pts',(1.48209760582561,0.305331840139509,2.36071288000775)) ;
#82141 = CARTESIAN_POINT('Ctrl Pts',(1.35327120458257,0.674844555199689,2.38124136417776)) ;
#82142 = CARTESIAN_POINT('Ctrl Pts',(1.25604736977719,0.842082751174055,2.3900429136113)) ;
#82143 = CARTESIAN_POINT('Ctrl Pts',(1.00218649199299,1.13285682360821,2.41033385835603)) ;
#82144 = CARTESIAN_POINT('Ctrl Pts',(0.847205378895785,1.25298607802845,2.42112731437042)) ;
#82145 = CARTESIAN_POINT('Ctrl Pts',(0.496008451564929,1.42951229977629,2.4429277905745)) ;
#82146 = CARTESIAN_POINT('Ctrl Pts',(0.302347799540614,1.48261176133978,2.45372027808274)) ;
#82147 = CARTESIAN_POINT('Ctrl Pts',(-0.0854763866555089,1.50955261960386,
2.47312783511495)) ;
#82148 = CARTESIAN_POINT('Ctrl Pts',(-0.275694147693553,1.48662992010136,
2.4823857319737)) ;
#82149 = CARTESIAN_POINT('Ctrl Pts',(-0.643805120793757,1.3689898690344,2.50336425862092)) ;
#82150 = CARTESIAN_POINT('Ctrl Pts',(-0.817424516468723,1.27296262986177,
2.5143849490004)) ;
#82151 = CARTESIAN_POINT('Ctrl Pts',(-1.11987963846953,1.01763999896081,2.53602912314528)) ;
#82152 = CARTESIAN_POINT('Ctrl Pts',(-1.24499584225552,0.860044432785634,
2.54596975373413)) ;
#82153 = CARTESIAN_POINT('Ctrl Pts',(-1.4228357870948,0.512082877429392,2.56530095125392)) ;
#82154 = CARTESIAN_POINT('Ctrl Pts',(-1.47652293354409,0.326418477279332,
2.57561564015114)) ;
#82155 = CARTESIAN_POINT('Ctrl Pts',(-1.49795431175567,0.0905134319012143,
2.58872147600548)) ;
#82156 = CARTESIAN_POINT('Ctrl Pts',(-1.5,0.0452298468524057,2.59123723073041)) ;
#82157 = CARTESIAN_POINT('Ctrl Pts',(-1.5,-4.53662128371792E-15,2.59374999999999)) ;
#82158 = CARTESIAN_POINT('Origin',(0.,0.,0.)) ;
#82159 = CARTESIAN_POINT('',(-1.5,4.9605336138464E-15,3.15624999999999)) ;
#82160 = CARTESIAN_POINT('',(-1.5,-1.366870264779E-15,3.09374999999999)) ;
#82161 = CARTESIAN_POINT('',(-1.5,-1.83697019872103E-16,0.)) ;
#82162 = CARTESIAN_POINT('Ctrl Pts',(-1.5,6.24500451351651E-15,3.15624999999999)) ;
#82163 = CARTESIAN_POINT('Ctrl Pts',(-1.5,0.11516372949426,3.14985201502809)) ;
#82164 = CARTESIAN_POINT('Ctrl Pts',(-1.48673694768359,0.230214992296067,
3.14346027820577)) ;
#82165 = CARTESIAN_POINT('Ctrl Pts',(-1.41687259925006,0.52778747825224,3.12692847343043)) ;
#82166 = CARTESIAN_POINT('Ctrl Pts',(-1.33873153172212,0.702759013395465,
3.11780533381227)) ;
#82167 = CARTESIAN_POINT('Ctrl Pts',(-1.11619744824656,1.02159711063618,3.09824204391682)) ;
#82168 = CARTESIAN_POINT('Ctrl Pts',(-0.971072864716749,1.16041120195476,
3.08740378715517)) ;
#82169 = CARTESIAN_POINT('Ctrl Pts',(-0.639341229669528,1.37071314560809,
3.06560162076536)) ;
#82170 = CARTESIAN_POINT('Ctrl Pts',(-0.456936833216421,1.44181586604181,
3.05485060958163)) ;
#82171 = CARTESIAN_POINT('Ctrl Pts',(-0.076827813420807,1.51031865257357,
3.03465975065849)) ;
#82172 = CARTESIAN_POINT('Ctrl Pts',(0.117152483621678,1.5077271851314,3.02582814253516)) ;
#82173 = CARTESIAN_POINT('Ctrl Pts',(0.500482061088619,1.42801404311459,3.00517093569534)) ;
#82174 = CARTESIAN_POINT('Ctrl Pts',(0.685533458305974,1.34897721804582,2.99407217883254)) ;
#82175 = CARTESIAN_POINT('Ctrl Pts',(1.0077052814503,1.12751207314981,2.97241987018396)) ;
#82176 = CARTESIAN_POINT('Ctrl Pts',(1.14343765683333,0.989608280268855,2.96205878231517)) ;
#82177 = CARTESIAN_POINT('Ctrl Pts',(1.35929288258575,0.664593590765959,2.94264525710447)) ;
#82178 = CARTESIAN_POINT('Ctrl Pts',(1.43519482065327,0.479168724862576,2.93287048471459)) ;
#82179 = CARTESIAN_POINT('Ctrl Pts',(1.51010457232472,0.0911069665243634,
2.91131149814024)) ;
#82180 = CARTESIAN_POINT('Ctrl Pts',(1.5090224152309,-0.10755521505248,2.90027471027486)) ;
#82181 = CARTESIAN_POINT('Ctrl Pts',(1.43159011268547,-0.486451731858559,
2.87922490378564)) ;
#82182 = CARTESIAN_POINT('Ctrl Pts',(1.35855993933727,-0.663607641540354,
2.86984686662555)) ;
#82183 = CARTESIAN_POINT('Ctrl Pts',(1.14541164191085,-0.988726092516216,
2.85056069630151)) ;
#82184 = CARTESIAN_POINT('Ctrl Pts',(1.00440406782438,-1.1316786535961,2.83980556175569)) ;
#82185 = CARTESIAN_POINT('Ctrl Pts',(0.678507252619518,-1.35183260774445,
2.81801045630824)) ;
#82186 = CARTESIAN_POINT('Ctrl Pts',(0.497694190148281,-1.42833269597271,
2.80718608133322)) ;
#82187 = CARTESIAN_POINT('Ctrl Pts',(0.120010058617026,-1.50738721206899,
2.78681878630208)) ;
#82188 = CARTESIAN_POINT('Ctrl Pts',(-0.0730332829740776,-1.51039185153122,
2.77802484707712)) ;
#82189 = CARTESIAN_POINT('Ctrl Pts',(-0.458262098731161,-1.44219981361828,
2.75759629376202)) ;
#82190 = CARTESIAN_POINT('Ctrl Pts',(-0.64611281319328,-1.36838199386208,
2.74650782705528)) ;
#82191 = CARTESIAN_POINT('Ctrl Pts',(-0.97543592605115,-1.15563014064546,
2.72475348769992)) ;
#82192 = CARTESIAN_POINT('Ctrl Pts',(-1.11538240998354,-1.02122344350407,
2.71428678998734)) ;
#82193 = CARTESIAN_POINT('Ctrl Pts',(-1.33937983434098,-0.703352071176045,
2.69467994854068)) ;
#82194 = CARTESIAN_POINT('Ctrl Pts',(-1.41993041352524,-0.521972346371288,
2.6852484636873)) ;
#82195 = CARTESIAN_POINT('Ctrl Pts',(-1.48771873938675,-0.221564625713655,
2.66855914587298)) ;
#82196 = CARTESIAN_POINT('Ctrl Pts',(-1.5,-0.11081974676082,2.66240665259782)) ;
#82197 = CARTESIAN_POINT('Ctrl Pts',(-1.5,4.8919202022546E-15,2.65625)) ;
#82198 = CARTESIAN_POINT('Ctrl Pts',(-1.5,-4.71844785465692E-15,2.59374999999999)) ;
#82199 = CARTESIAN_POINT('Ctrl Pts',(-1.5,-0.153082698281981,2.60225459434899)) ;
#82200 = CARTESIAN_POINT('Ctrl Pts',(-1.47656373062122,-0.305549815759312,
2.6107249897644)) ;
#82201 = CARTESIAN_POINT('Ctrl Pts',(-1.37219374715963,-0.635783357289578,
2.62907129762719)) ;
#82202 = CARTESIAN_POINT('Ctrl Pts',(-1.27927337608324,-0.806593936310442,
2.637939651449)) ;
#82203 = CARTESIAN_POINT('Ctrl Pts',(-1.0331884703089,-1.10456312202827,2.65805633882385)) ;
#82204 = CARTESIAN_POINT('Ctrl Pts',(-0.882042538773507,-1.22862754510375,
2.66877458481975)) ;
#82205 = CARTESIAN_POINT('Ctrl Pts',(-0.536452871603693,-1.41483555485109,
2.69057422014909)) ;
#82206 = CARTESIAN_POINT('Ctrl Pts',(-0.344353610376509,-1.47342515704064,
2.70144408911385)) ;
#82207 = CARTESIAN_POINT('Ctrl Pts',(0.0426928743225535,-1.5113830347619,
2.72112025728359)) ;
#82208 = CARTESIAN_POINT('Ctrl Pts',(0.233586323798436,-1.49383764067041,
2.73015960389171)) ;
#82209 = CARTESIAN_POINT('Ctrl Pts',(0.604430425126557,-1.38674616323053,
2.75097661229803)) ;
#82210 = CARTESIAN_POINT('Ctrl Pts',(0.780228173717907,-1.29600964493656,
2.7619551442622)) ;
#82211 = CARTESIAN_POINT('Ctrl Pts',(1.08925985428694,-1.05026891225514,2.7836495693893)) ;
#82212 = CARTESIAN_POINT('Ctrl Pts',(1.21870925393897,-0.896800942013726,
2.79392772544368)) ;
#82213 = CARTESIAN_POINT('Ctrl Pts',(1.4064648072281,-0.555274007709077,2.81290144401616)) ;
#82214 = CARTESIAN_POINT('Ctrl Pts',(1.46565146626508,-0.371907038656333,
2.82308849785242)) ;
#82215 = CARTESIAN_POINT('Ctrl Pts',(1.51298910573879,0.0144777298509668,
2.84455431832505)) ;
#82216 = CARTESIAN_POINT('Ctrl Pts',(1.49781990267104,0.214214659586258,2.85565081442145)) ;
#82217 = CARTESIAN_POINT('Ctrl Pts',(1.39181447279936,0.592030983292885,2.87664061018293)) ;
#82218 = CARTESIAN_POINT('Ctrl Pts',(1.30366680435728,0.766874008586105,2.88566269075828)) ;
#82219 = CARTESIAN_POINT('Ctrl Pts',(1.06616214320864,1.07266709457545,2.90558389148421)) ;
#82220 = CARTESIAN_POINT('Ctrl Pts',(0.919318889984905,1.20089696350865,2.91621083160269)) ;
#82221 = CARTESIAN_POINT('Ctrl Pts',(0.578469661586673,1.39846618248674,2.93809798161059)) ;
#82222 = CARTESIAN_POINT('Ctrl Pts',(0.386223523438131,1.46327854042905,2.94914777152099)) ;
#82223 = CARTESIAN_POINT('Ctrl Pts',(-0.00191788599131014,1.5120232743001,
2.96917625417444)) ;
#82224 = CARTESIAN_POINT('Ctrl Pts',(-0.193515144967493,1.4995921901257,2.97807182980533)) ;
#82225 = CARTESIAN_POINT('Ctrl Pts',(-0.566855974091238,1.40245224833857,
2.99873253053781)) ;
#82226 = CARTESIAN_POINT('Ctrl Pts',(-0.744563820988319,1.31674461952063,
3.00966327077524)) ;
#82227 = CARTESIAN_POINT('Ctrl Pts',(-1.05973596143589,1.08002680934193,3.0314024921798)) ;
#82228 = CARTESIAN_POINT('Ctrl Pts',(-1.19338051697833,0.930251518216961,
3.04199289360978)) ;
#82229 = CARTESIAN_POINT('Ctrl Pts',(-1.39023496041013,0.594544362523114,
3.0607892562046)) ;
#82230 = CARTESIAN_POINT('Ctrl Pts',(-1.45442868124805,0.413433012454585,
3.07078149930807)) ;
#82231 = CARTESIAN_POINT('Ctrl Pts',(-1.49434802658991,0.150424648214569,
3.08539307509918)) ;
#82232 = CARTESIAN_POINT('Ctrl Pts',(-1.5,0.0751804928068105,3.08957330595517)) ;
#82233 = CARTESIAN_POINT('Ctrl Pts',(-1.5,-4.53662128371792E-15,3.09374999999999)) ;
#82234 = CARTESIAN_POINT('Origin',(0.,0.,0.)) ;
#82235 = CARTESIAN_POINT('',(-1.5,3.76526828577686E-16,3.65624999999999)) ;
#82236 = CARTESIAN_POINT('',(-1.5,-2.3990307329852E-15,3.59374999999999)) ;
#82237 = CARTESIAN_POINT('',(-1.5,-1.83697019872103E-16,0.)) ;
#82238 = CARTESIAN_POINT('Ctrl Pts',(-1.5,5.48172618408671E-15,3.65624999999999)) ;
#82239 = CARTESIAN_POINT('Ctrl Pts',(-1.5,0.142496679359764,3.64833351781334)) ;
#82240 = CARTESIAN_POINT('Ctrl Pts',(-1.47969327645223,0.284545958301245,
3.64044189120548)) ;
#82241 = CARTESIAN_POINT('Ctrl Pts',(-1.38587417389988,0.604715323638973,
3.62265470424227)) ;
#82242 = CARTESIAN_POINT('Ctrl Pts',(-1.29792548082208,0.775701489755982,
3.61381587187405)) ;
#82243 = CARTESIAN_POINT('Ctrl Pts',(-1.05655434668454,1.08347140714469,3.5936537333964)) ;
#82244 = CARTESIAN_POINT('Ctrl Pts',(-0.902412425877809,1.21484681248879,
3.58258825995869)) ;
#82245 = CARTESIAN_POINT('Ctrl Pts',(-0.558362594348466,1.4054957323175,3.56073935139277)) ;
#82246 = CARTESIAN_POINT('Ctrl Pts',(-0.373217195344678,1.46557591106783,
3.55016264537576)) ;
#82247 = CARTESIAN_POINT('Ctrl Pts',(0.0115988163075127,1.5125503090816,3.5303433319935)) ;
#82248 = CARTESIAN_POINT('Ctrl Pts',(0.207685058067254,1.49827154866902,3.52120973544787)) ;
#82249 = CARTESIAN_POINT('Ctrl Pts',(0.586630438424552,1.39466352798266,3.50009971676013)) ;
#82250 = CARTESIAN_POINT('Ctrl Pts',(0.76543470542945,1.30511535190838,3.48900954311744)) ;
#82251 = CARTESIAN_POINT('Ctrl Pts',(1.07206353486311,1.06630935655377,3.46762335681191)) ;
#82252 = CARTESIAN_POINT('Ctrl Pts',(1.19878375694058,0.921562637602475,3.45750578509147)) ;
#82253 = CARTESIAN_POINT('Ctrl Pts',(1.39527810543078,0.585390369828785,3.43871382779262)) ;
#82254 = CARTESIAN_POINT('Ctrl Pts',(1.46050827894949,0.395546863964534,3.42822482577581)) ;
#82255 = CARTESIAN_POINT('Ctrl Pts',(1.51269993114629,0.00450706484213029,
3.40650039249123)) ;
#82256 = CARTESIAN_POINT('Ctrl Pts',(1.50039210501571,-0.192640250105679,
3.39554776388301)) ;
#82257 = CARTESIAN_POINT('Ctrl Pts',(1.40216511092891,-0.565773747141564,
3.3748181251588)) ;
#82258 = CARTESIAN_POINT('Ctrl Pts',(1.31923545756705,-0.738766459596867,
3.36586712166821)) ;
#82259 = CARTESIAN_POINT('Ctrl Pts',(1.08795698672388,-1.05162490322803,3.34604921872853)) ;
#82260 = CARTESIAN_POINT('Ctrl Pts',(0.939086996871196,-1.18644950149429,
3.33514158027261)) ;
#82261 = CARTESIAN_POINT('Ctrl Pts',(0.6021584415055,-1.3873787830828,3.31334972866142)) ;
#82262 = CARTESIAN_POINT('Ctrl Pts',(0.418406018236275,-1.45339795551531,
3.30267507017396)) ;
#82263 = CARTESIAN_POINT('Ctrl Pts',(0.0360862450027967,-1.51197500679322,
3.28265356119461)) ;
#82264 = CARTESIAN_POINT('Ctrl Pts',(-0.158832651584457,-1.50404331095635,
3.27372047468086)) ;
#82265 = CARTESIAN_POINT('Ctrl Pts',(-0.540230368816554,-1.41337675207924,
3.25285195293048)) ;
#82266 = CARTESIAN_POINT('Ctrl Pts',(-0.722490448810619,-1.32946682039408,
3.24175212930753)) ;
#82267 = CARTESIAN_POINT('Ctrl Pts',(-1.03765275048246,-1.09992646574874,
3.2202127550361)) ;
#82268 = CARTESIAN_POINT('Ctrl Pts',(-1.1692973788514,-0.958815715680369,
3.20995925684313)) ;
#82269 = CARTESIAN_POINT('Ctrl Pts',(-1.37731088447788,-0.627018029011212,
3.19073459997994)) ;
#82270 = CARTESIAN_POINT('Ctrl Pts',(-1.44867384821221,-0.437629584726534,
3.18056275470703)) ;
#82271 = CARTESIAN_POINT('Ctrl Pts',(-1.49357976662945,-0.160308684359475,
3.16515603801997)) ;
#82272 = CARTESIAN_POINT('Ctrl Pts',(-1.5,-0.080127120084231,3.16070150667134)) ;
#82273 = CARTESIAN_POINT('Ctrl Pts',(-1.5,4.90844004519486E-15,3.15624999999999)) ;
#82274 = CARTESIAN_POINT('Ctrl Pts',(-1.5,-3.81639164714898E-15,3.09374999999999)) ;
#82275 = CARTESIAN_POINT('Ctrl Pts',(-1.5,-0.121704222728767,3.10051134570714)) ;
#82276 = CARTESIAN_POINT('Ctrl Pts',(-1.48518751341521,-0.243241611160598,
3.10726342284225)) ;
#82277 = CARTESIAN_POINT('Ctrl Pts',(-1.40853373838638,-0.551575580172437,
3.12439308778735)) ;
#82278 = CARTESIAN_POINT('Ctrl Pts',(-1.32477505881493,-0.730180718244438,
3.13362786132713)) ;
#82279 = CARTESIAN_POINT('Ctrl Pts',(-1.09510085243453,-1.04301082593862,
3.1533677919475)) ;
#82280 = CARTESIAN_POINT('Ctrl Pts',(-0.952239643711773,-1.17487850304191,
3.16390419608755)) ;
#82281 = CARTESIAN_POINT('Ctrl Pts',(-0.618017382571796,-1.38135918941648,
3.18572004674559)) ;
#82282 = CARTESIAN_POINT('Ctrl Pts',(-0.428279776959831,-1.45144424895783,
3.19679560876136)) ;
#82283 = CARTESIAN_POINT('Ctrl Pts',(-0.0417903806202598,-1.51151426505888,
3.21705920007102)) ;
#82284 = CARTESIAN_POINT('Ctrl Pts',(0.150626335212339,-1.50457189944236,
3.22587001572508)) ;
#82285 = CARTESIAN_POINT('Ctrl Pts',(0.526536562508407,-1.41800688506666,
3.24636058870112)) ;
#82286 = CARTESIAN_POINT('Ctrl Pts',(0.706117818651959,-1.33767455866574,
3.25723214942692)) ;
#82287 = CARTESIAN_POINT('Ctrl Pts',(1.02767040139798,-1.11058884241468,3.27901079184003)) ;
#82288 = CARTESIAN_POINT('Ctrl Pts',(1.16566595481994,-0.964759812582032,
3.28970091238387)) ;
#82289 = CARTESIAN_POINT('Ctrl Pts',(1.37207905979523,-0.635217788060569,
3.30878591265294)) ;
#82290 = CARTESIAN_POINT('Ctrl Pts',(1.44145359726056,-0.456452881821541,
3.31839150656546)) ;
#82291 = CARTESIAN_POINT('Ctrl Pts',(1.51102102328224,-0.0754717113844235,
3.3395571271453)) ;
#82292 = CARTESIAN_POINT('Ctrl Pts',(1.50784793467382,0.123598206813867,3.35061656704521)) ;
#82293 = CARTESIAN_POINT('Ctrl Pts',(1.42468299433366,0.509064698350426,3.37203137213057)) ;
#82294 = CARTESIAN_POINT('Ctrl Pts',(1.34553229762618,0.691660079507657,3.3815591604665)) ;
#82295 = CARTESIAN_POINT('Ctrl Pts',(1.1239977878084,1.01170303964803,3.4011078267658)) ;
#82296 = CARTESIAN_POINT('Ctrl Pts',(0.985322197553707,1.14718555235198,3.41154326234343)) ;
#82297 = CARTESIAN_POINT('Ctrl Pts',(0.658147482027504,1.36260820231781,3.43326842568257)) ;
#82298 = CARTESIAN_POINT('Ctrl Pts',(0.471132314614464,1.43802161298724,3.44436101408298)) ;
#82299 = CARTESIAN_POINT('Ctrl Pts',(0.0864670322230408,1.50971448154214,
3.464859699682)) ;
#82300 = CARTESIAN_POINT('Ctrl Pts',(-0.106856079585841,1.50840865112193,
3.47365754188383)) ;
#82301 = CARTESIAN_POINT('Ctrl Pts',(-0.485287758308828,1.43257301216333,
3.49397139004218)) ;
#82302 = CARTESIAN_POINT('Ctrl Pts',(-0.666603529977372,1.35771808035757,
3.50477425283521)) ;
#82303 = CARTESIAN_POINT('Ctrl Pts',(-0.994313764835153,1.14055612369053,
3.52657349543525)) ;
#82304 = CARTESIAN_POINT('Ctrl Pts',(-1.13659166351795,0.998854267157603,
3.53735500670874)) ;
#82305 = CARTESIAN_POINT('Ctrl Pts',(-1.35261269373874,0.675643420895191,
3.55672640243397)) ;
#82306 = CARTESIAN_POINT('Ctrl Pts',(-1.42720468076801,0.499163062174969,
3.56601871876805)) ;
#82307 = CARTESIAN_POINT('Ctrl Pts',(-1.48895486038857,0.210151736290253,
3.58207490353942)) ;
#82308 = CARTESIAN_POINT('Ctrl Pts',(-1.5,0.105095275150541,3.58791137360274)) ;
#82309 = CARTESIAN_POINT('Ctrl Pts',(-1.5,-3.15719672627779E-15,3.59374999999999)) ;
#82310 = CARTESIAN_POINT('Origin',(0.,0.,0.)) ;
#82311 = CARTESIAN_POINT('',(-1.5,-4.02009930659002E-13,4.15625000000004)) ;
#82312 = CARTESIAN_POINT('',(-1.5,-2.45107243726451E-15,4.09374999999999)) ;
#82313 = CARTESIAN_POINT('',(-1.5,-1.83697019872103E-16,0.)) ;
#82314 = CARTESIAN_POINT('Ctrl Pts',(-1.5,-8.04321886871406E-13,4.15625000000004)) ;
#82315 = CARTESIAN_POINT('Ctrl Pts',(-1.50000000000009,0.171133603059582,
4.14674257760779)) ;
#82316 = CARTESIAN_POINT('Ctrl Pts',(-1.47071121488924,0.341198831191777,
4.13729450937823)) ;
#82317 = CARTESIAN_POINT('Ctrl Pts',(-1.3488319714892,0.683790252304662,4.11826165264973)) ;
#82318 = CARTESIAN_POINT('Ctrl Pts',(-1.25026747431287,0.850734260237844,
4.1094386813423)) ;
#82319 = CARTESIAN_POINT('Ctrl Pts',(-0.990699880929532,1.14378752497098,
4.08880986121809)) ;
#82320 = CARTESIAN_POINT('Ctrl Pts',(-0.830110001358271,1.26516499485942,
4.077711880649)) ;
#82321 = CARTESIAN_POINT('Ctrl Pts',(-0.477711658905107,1.43477190385086,
4.05604580446502)) ;
#82322 = CARTESIAN_POINT('Ctrl Pts',(-0.290524636825963,1.48404678783509,
4.04567101788883)) ;
#82323 = CARTESIAN_POINT('Ctrl Pts',(0.0986115526744294,1.50981516157915,
4.02623290608265)) ;
#82324 = CARTESIAN_POINT('Ctrl Pts',(0.296994345781134,1.48360506722658,4.01650543807702)) ;
#82325 = CARTESIAN_POINT('Ctrl Pts',(0.670868265347628,1.355980088746,3.99497228244384)) ;
#82326 = CARTESIAN_POINT('Ctrl Pts',(0.84282849344545,1.25633852853655,3.98393102099506)) ;
#82327 = CARTESIAN_POINT('Ctrl Pts',(1.13328837743446,1.0008741800697,3.96286003140905)) ;
#82328 = CARTESIAN_POINT('Ctrl Pts',(1.25077829060998,0.84948125492726,3.95344340305152)) ;
#82329 = CARTESIAN_POINT('Ctrl Pts',(1.42707774789501,0.502985826171431,3.93419365700952)) ;
#82330 = CARTESIAN_POINT('Ctrl Pts',(1.48110434042375,0.309600183743426,3.92345001020796)) ;
#82331 = CARTESIAN_POINT('Ctrl Pts',(1.51030351771318,-0.0826705098748036,
3.90165719389584)) ;
#82332 = CARTESIAN_POINT('Ctrl Pts',(1.48686269123112,-0.277669729350829,
3.89082390392495)) ;
#82333 = CARTESIAN_POINT('Ctrl Pts',(1.36782940170216,-0.644688161043389,
3.87043399105314)) ;
#82334 = CARTESIAN_POINT('Ctrl Pts',(1.27459213170475,-0.813629810466613,
3.86163968112704)) ;
#82335 = CARTESIAN_POINT('Ctrl Pts',(1.02409018249644,-1.1140981305869,3.84124105825081)) ;
#82336 = CARTESIAN_POINT('Ctrl Pts',(0.866649844836005,-1.2405158785012,3.83015460236462)) ;
#82337 = CARTESIAN_POINT('Ctrl Pts',(0.518273761921561,-1.42069517993084,
3.80838836966519)) ;
#82338 = CARTESIAN_POINT('Ctrl Pts',(0.332030838647065,-1.47538359057195,
3.79790863032345)) ;
#82339 = CARTESIAN_POINT('Ctrl Pts',(-0.0549754716884883,-1.51179841551055,
3.77827725762096)) ;
#82340 = CARTESIAN_POINT('Ctrl Pts',(-0.252182033789337,-1.49163500350121,
3.76888452522838)) ;
#82341 = CARTESIAN_POINT('Ctrl Pts',(-0.628701513673564,-1.37612462376939,
3.74756060164698)) ;
#82342 = CARTESIAN_POINT('Ctrl Pts',(-0.804182037469132,-1.28151209916078,
3.73648966532583)) ;
#82343 = CARTESIAN_POINT('Ctrl Pts',(-1.10286143022979,-1.03435426175478,
3.71525395085802)) ;
#82344 = CARTESIAN_POINT('Ctrl Pts',(-1.22497837383202,-0.886328218669872,
3.70549045659277)) ;
#82345 = CARTESIAN_POINT('Ctrl Pts',(-1.41154877671446,-0.54503485247189,
3.68652971402622)) ;
#82346 = CARTESIAN_POINT('Ctrl Pts',(-1.4712707707181,-0.353369120526585,
3.67588161780703)) ;
#82347 = CARTESIAN_POINT('Ctrl Pts',(-1.49730613246558,-0.103865648310611,
3.66202031379503)) ;
#82348 = CARTESIAN_POINT('Ctrl Pts',(-1.5,-0.0519031454973351,3.65913350808318)) ;
#82349 = CARTESIAN_POINT('Ctrl Pts',(-1.5,4.90844004519485E-15,3.65624999999999)) ;
#82350 = CARTESIAN_POINT('Ctrl Pts',(-1.5,-4.53662128371792E-15,3.59374999999999)) ;
#82351 = CARTESIAN_POINT('Ctrl Pts',(-1.5,-0.0905641075434439,3.59878133930796)) ;
#82352 = CARTESIAN_POINT('Ctrl Pts',(-1.49179821598492,-0.181157037767087,
3.60381427987594)) ;
#82353 = CARTESIAN_POINT('Ctrl Pts',(-1.43946376029427,-0.466437771598478,
3.61966320953324)) ;
#82354 = CARTESIAN_POINT('Ctrl Pts',(-1.3649492311358,-0.6530734364045,3.62955311162014)) ;
#82355 = CARTESIAN_POINT('Ctrl Pts',(-1.1515028967344,-0.980181871746283,
3.64890889859832)) ;
#82356 = CARTESIAN_POINT('Ctrl Pts',(-1.01702360187864,-1.11908761046717,
3.65923752943101)) ;
#82357 = CARTESIAN_POINT('Ctrl Pts',(-0.696993112621626,-1.34306654442955,
3.68085664057898)) ;
#82358 = CARTESIAN_POINT('Ctrl Pts',(-0.512789648427401,-1.42361647993805,
3.69195663209073)) ;
#82359 = CARTESIAN_POINT('Ctrl Pts',(-0.130042475882154,-1.5067093297347,
3.71267969873235)) ;
#82360 = CARTESIAN_POINT('Ctrl Pts',(0.0642221720734728,-1.51094601393429,
3.72153583475192)) ;
#82361 = CARTESIAN_POINT('Ctrl Pts',(0.445023198793493,-1.4455165182095,3.74167461868465)) ;
#82362 = CARTESIAN_POINT('Ctrl Pts',(0.627860421384518,-1.37598756773571,
3.75240273839343)) ;
#82363 = CARTESIAN_POINT('Ctrl Pts',(0.961231665515552,-1.16857762400818,
3.77420345718079)) ;
#82364 = CARTESIAN_POINT('Ctrl Pts',(1.10752938938788,-1.03098917949774,3.78506411093882)) ;
#82365 = CARTESIAN_POINT('Ctrl Pts',(1.33277994479441,-0.713995037954878,
3.80470687615938)) ;
#82366 = CARTESIAN_POINT('Ctrl Pts',(1.41240534053575,-0.53964380029473,3.81376978887251)) ;
#82367 = CARTESIAN_POINT('Ctrl Pts',(1.50377672399984,-0.164570939699714,
3.83460717001667)) ;
#82368 = CARTESIAN_POINT('Ctrl Pts',(1.51239069939861,0.0331458714058803,
3.84559143730032)) ;
#82369 = CARTESIAN_POINT('Ctrl Pts',(1.45265193985208,0.423505349670125,3.86727807498167)) ;
#82370 = CARTESIAN_POINT('Ctrl Pts',(1.38377694290032,0.612103399456392,3.87750920633362)) ;
#82371 = CARTESIAN_POINT('Ctrl Pts',(1.18061920560496,0.944794807510319,3.89652506552808)) ;
#82372 = CARTESIAN_POINT('Ctrl Pts',(1.05083061160804,1.08730435962015,3.90672812083795)) ;
#82373 = CARTESIAN_POINT('Ctrl Pts',(0.738873468516821,1.32039470365947,3.92821189766176)) ;
#82374 = CARTESIAN_POINT('Ctrl Pts',(0.557904269288321,1.40645870723091,3.9393094490851)) ;
#82375 = CARTESIAN_POINT('Ctrl Pts',(0.177414530578306,1.50203357785154,3.96027062769135)) ;
#82376 = CARTESIAN_POINT('Ctrl Pts',(-0.0179401791249838,1.5123670491789,
3.96926961812673)) ;
#82377 = CARTESIAN_POINT('Ctrl Pts',(-0.401221132172622,1.4582059859365,3.98921470555712)) ;
#82378 = CARTESIAN_POINT('Ctrl Pts',(-0.585526905180342,1.39444825345553,
3.99985316931986)) ;
#82379 = CARTESIAN_POINT('Ctrl Pts',(-0.926440532557907,1.1966931789007,4.02174858038001)) ;
#82380 = CARTESIAN_POINT('Ctrl Pts',(-1.07823908104159,1.06197238198835,4.03279423580782)) ;
#82381 = CARTESIAN_POINT('Ctrl Pts',(-1.31331721168121,0.749262857926172,
4.05279081331)) ;
#82382 = CARTESIAN_POINT('Ctrl Pts',(-1.39766131060398,0.576842450533384,
4.06170319719258)) ;
#82383 = CARTESIAN_POINT('Ctrl Pts',(-1.48243173092841,0.264783173922913,
4.07903982367094)) ;
#82384 = CARTESIAN_POINT('Ctrl Pts',(-1.5,0.132541600323799,4.08638657775978)) ;
#82385 = CARTESIAN_POINT('Ctrl Pts',(-1.5,-3.78169717762944E-15,4.09374999999999)) ;
#82386 = CARTESIAN_POINT('Origin',(0.,0.,0.)) ;
#82387 = CARTESIAN_POINT('',(-1.5,-1.25411323884051E-15,4.65624999999999)) ;
#82388 = CARTESIAN_POINT('',(-1.5,5.49396108270927E-15,4.59374999999999)) ;
#82389 = CARTESIAN_POINT('',(-1.5,-1.83697019872103E-16,0.)) ;
#82390 = CARTESIAN_POINT('Ctrl Pts',(-1.5,0.,4.65624999999999)) ;
#82391 = CARTESIAN_POINT('Ctrl Pts',(-1.5,0.00765172681326447,4.65582490406592)) ;
#82392 = CARTESIAN_POINT('Ctrl Pts',(-1.49994145115902,0.0153060271662843,
4.65539966515743)) ;
#82393 = CARTESIAN_POINT('Ctrl Pts',(-1.49678001132018,0.221801716357427,
4.64392768242458)) ;
#82394 = CARTESIAN_POINT('Ctrl Pts',(-1.45422382952216,0.418088612371266,
4.63302285486826)) ;
#82395 = CARTESIAN_POINT('Ctrl Pts',(-1.29850811284946,0.774615782250993,
4.61321578987494)) ;
#82396 = CARTESIAN_POINT('Ctrl Pts',(-1.18998137611373,0.932794904983397,
4.60425870273628)) ;
#82397 = CARTESIAN_POINT('Ctrl Pts',(-0.915634517518497,1.20412163064066,
4.58352232985737)) ;
#82398 = CARTESIAN_POINT('Ctrl Pts',(-0.750907326550277,1.31317493739108,
4.57256763066582)) ;
#82399 = CARTESIAN_POINT('Ctrl Pts',(-0.385960185672472,1.46307114925216,
4.55084531950087)) ;
#82400 = CARTESIAN_POINT('Ctrl Pts',(-0.188887711273289,1.50126810659913,
4.54037308942916)) ;
#82401 = CARTESIAN_POINT('Ctrl Pts',(0.200517010733479,1.49872002276902,4.52156706589991)) ;
#82402 = CARTESIAN_POINT('Ctrl Pts',(0.389208644959509,1.46111640651101,4.51144409051933)) ;
#82403 = CARTESIAN_POINT('Ctrl Pts',(0.749197883699321,1.31450704403914,4.49005161790413)) ;
#82404 = CARTESIAN_POINT('Ctrl Pts',(0.916033315803187,1.20420703080166,4.47896085517791)) ;
#82405 = CARTESIAN_POINT('Ctrl Pts',(1.19485086801825,0.927500969508377,4.45785995996203)) ;
#82406 = CARTESIAN_POINT('Ctrl Pts',(1.30502448153115,0.764741922445452,4.44873566235808)) ;
#82407 = CARTESIAN_POINT('Ctrl Pts',(1.45631999560281,0.407853490475697,4.42890852724865)) ;
#82408 = CARTESIAN_POINT('Ctrl Pts',(1.4966402198032,0.217402276981722,4.41832790427676)) ;
#82409 = CARTESIAN_POINT('Ctrl Pts',(1.50308295672099,-0.175933966475625,
4.39647589075135)) ;
#82410 = CARTESIAN_POINT('Ctrl Pts',(1.46612859314491,-0.375092801046321,
4.38541151105298)) ;
#82411 = CARTESIAN_POINT('Ctrl Pts',(1.31981917380275,-0.737829091200718,
4.36525949493329)) ;
#82412 = CARTESIAN_POINT('Ctrl Pts',(1.21552803507139,-0.89933901492746,4.35641714721779)) ;
#82413 = CARTESIAN_POINT('Ctrl Pts',(0.948850606174006,-1.17803578888138,
4.33584504638346)) ;
#82414 = CARTESIAN_POINT('Ctrl Pts',(0.787706228951202,-1.2913547622266,4.32494423465987)) ;
#82415 = CARTESIAN_POINT('Ctrl Pts',(0.427778741293969,-1.45138281896797,
4.30318199153753)) ;
#82416 = CARTESIAN_POINT('Ctrl Pts',(0.231876508787605,-1.49524768493686,
4.29253817248236)) ;
#82417 = CARTESIAN_POINT('Ctrl Pts',(-0.157001735674165,-1.50383036417844,
4.27358985146548)) ;
#82418 = CARTESIAN_POINT('Ctrl Pts',(-0.34623035278147,-1.47184339249322,
4.26380985639869)) ;
#82419 = CARTESIAN_POINT('Ctrl Pts',(-0.709480149048449,-1.33627470610578,
4.24256719558311)) ;
#82420 = CARTESIAN_POINT('Ctrl Pts',(-0.879042040408571,-1.23137319434659,
4.23149521439916)) ;
#82421 = CARTESIAN_POINT('Ctrl Pts',(-1.16694178851328,-0.962698703891227,
4.21018045101975)) ;
#82422 = CARTESIAN_POINT('Ctrl Pts',(-1.28275904458616,-0.801908652806195,
4.20080048071145)) ;
#82423 = CARTESIAN_POINT('Ctrl Pts',(-1.44428227005255,-0.448395681485922,
4.18116087119366)) ;
#82424 = CARTESIAN_POINT('Ctrl Pts',(-1.48981764891001,-0.25968189653311,
4.17067677204504)) ;
#82425 = CARTESIAN_POINT('Ctrl Pts',(-1.49949364665084,-0.0450232754631008,
4.15875129309639)) ;
#82426 = CARTESIAN_POINT('Ctrl Pts',(-1.49999999999999,-0.0225024017976655,
4.1575001334332)) ;
#82427 = CARTESIAN_POINT('Ctrl Pts',(-1.5,-8.04835511280435E-13,4.15625000000004)) ;
#82428 = CARTESIAN_POINT('Ctrl Pts',(-1.5,-4.53662128371792E-15,4.09374999999999)) ;
#82429 = CARTESIAN_POINT('Ctrl Pts',(-1.5,-0.0621643353056686,4.09720357418364)) ;
#82430 = CARTESIAN_POINT('Ctrl Pts',(-1.49613569807775,-0.124394669725961,
4.10066081498477)) ;
#82431 = CARTESIAN_POINT('Ctrl Pts',(-1.4636951723303,-0.383526246747067,
4.11505701370816)) ;
#82432 = CARTESIAN_POINT('Ctrl Pts',(-1.40005833887612,-0.573898595494419,
4.12563325530524)) ;
#82433 = CARTESIAN_POINT('Ctrl Pts',(-1.20639289314394,-0.911524647065871,
4.14439025817032)) ;
#82434 = CARTESIAN_POINT('Ctrl Pts',(-1.08101171753964,-1.0572279674842,4.15444057636129)) ;
#82435 = CARTESIAN_POINT('Ctrl Pts',(-0.778107783103184,-1.29727904975425,
4.17568213432053)) ;
#82436 = CARTESIAN_POINT('Ctrl Pts',(-0.602191679243006,-1.38771539990994,
4.1866580226546)) ;
#82437 = CARTESIAN_POINT('Ctrl Pts',(-0.23119587925635,-1.49421100262234,
4.20746577759026)) ;
#82438 = CARTESIAN_POINT('Ctrl Pts',(-0.0402621150360292,-1.51145138543449,
4.21649479404729)) ;
#82439 = CARTESIAN_POINT('Ctrl Pts',(0.346736688744763,-1.47286633657555,
4.23618608958829)) ;
#82440 = CARTESIAN_POINT('Ctrl Pts',(0.538742248805719,-1.41396560245127,
4.24706009290733)) ;
#82441 = CARTESIAN_POINT('Ctrl Pts',(0.884004652664943,-1.22721178111378,
4.26885914420636)) ;
#82442 = CARTESIAN_POINT('Ctrl Pts',(1.03492934112488,-1.10292691552911,4.27957286904285)) ;
#82443 = CARTESIAN_POINT('Ctrl Pts',(1.28056959752403,-0.804549316003377,
4.29967950804266)) ;
#82444 = CARTESIAN_POINT('Ctrl Pts',(1.37324335257794,-0.633532114432611,
4.3085537714204)) ;
#82445 = CARTESIAN_POINT('Ctrl Pts',(1.49067185552879,-0.259792178928917,
4.3293171011706)) ;
#82446 = CARTESIAN_POINT('Ctrl Pts',(1.5119480039113,-0.0599858873288936,
4.34041745070394)) ;
#82447 = CARTESIAN_POINT('Ctrl Pts',(1.47599570015083,0.328776967556811,4.36201538708648)) ;
#82448 = CARTESIAN_POINT('Ctrl Pts',(1.42202227581893,0.514326649085503,4.37232370272696)) ;
#82449 = CARTESIAN_POINT('Ctrl Pts',(1.24360105625019,0.862086606103215,4.39164370033906)) ;
#82450 = CARTESIAN_POINT('Ctrl Pts',(1.11814673318228,1.01956661567486,4.40160776843016)) ;
#82451 = CARTESIAN_POINT('Ctrl Pts',(0.815172055919553,1.2744009339664,4.42326337545008)) ;
#82452 = CARTESIAN_POINT('Ctrl Pts',(0.641415145557375,1.37010641258235,4.43428174421479)) ;
#82453 = CARTESIAN_POINT('Ctrl Pts',(0.273134641221515,1.48710228282742,4.45525053352567)) ;
#82454 = CARTESIAN_POINT('Ctrl Pts',(0.082877658089358,1.50969770846992,4.46449316602518)) ;
#82455 = CARTESIAN_POINT('Ctrl Pts',(-0.30490254158167,1.48208868848018,4.48391716680266)) ;
#82456 = CARTESIAN_POINT('Ctrl Pts',(-0.498473081444425,1.42865500899227,
4.49471460261874)) ;
#82457 = CARTESIAN_POINT('Ctrl Pts',(-0.849337655166835,1.25153667703389,
4.51651553595822)) ;
#82458 = CARTESIAN_POINT('Ctrl Pts',(-1.00408899033133,1.1311654253393,4.52730465892319)) ;
#82459 = CARTESIAN_POINT('Ctrl Pts',(-1.25747997168065,0.83995402889664,4.54758514365428)) ;
#82460 = CARTESIAN_POINT('Ctrl Pts',(-1.35444448938871,0.672501804939245,
4.55638878861447)) ;
#82461 = CARTESIAN_POINT('Ctrl Pts',(-1.47210926486592,0.333075112485226,
4.57524582708414)) ;
#82462 = CARTESIAN_POINT('Ctrl Pts',(-1.5,0.166997886469703,4.58447233964056)) ;
#82463 = CARTESIAN_POINT('Ctrl Pts',(-1.5,1.65839564303383E-14,4.59374999999999)) ;
#82464 = CARTESIAN_POINT('Origin',(0.,0.,0.)) ;
#82465 = CARTESIAN_POINT('',(-1.5,-2.7806698977001E-15,5.15624999999999)) ;
#82466 = CARTESIAN_POINT('',(-1.5,-6.37154749297209E-15,5.09374999999999)) ;
#82467 = CARTESIAN_POINT('',(-1.5,-1.83697019872103E-16,0.)) ;
#82468 = CARTESIAN_POINT('Ctrl Pts',(-1.5,-9.66814085323955E-15,5.15624999999999)) ;
#82469 = CARTESIAN_POINT('Ctrl Pts',(-1.5,0.0358778710446101,5.15425678494196)) ;
#82470 = CARTESIAN_POINT('Ctrl Pts',(-1.49871280185265,0.0717941731031292,
5.1522614348276)) ;
#82471 = CARTESIAN_POINT('Ctrl Pts',(-1.48185844774037,0.305972268779071,
5.13925154062338)) ;
#82472 = CARTESIAN_POINT('Ctrl Pts',(-1.42830463508477,0.499492211148273,
5.12850043271399)) ;
#82473 = CARTESIAN_POINT('Ctrl Pts',(-1.25285565470282,0.84641263616168,5.1092270757688)) ;
#82474 = CARTESIAN_POINT('Ctrl Pts',(-1.13574394743954,0.998084772639103,
5.09983559579764)) ;
#82475 = CARTESIAN_POINT('Ctrl Pts',(-0.845959362352989,1.25422483603939,
5.07877832668596)) ;
#82476 = CARTESIAN_POINT('Ctrl Pts',(-0.674293667046528,1.35427282196232,
5.06773994634956)) ;
#82477 = CARTESIAN_POINT('Ctrl Pts',(-0.300644760146208,1.48289082680636,
5.04619003257767)) ;
#82478 = CARTESIAN_POINT('Ctrl Pts',(-0.102164262404235,1.50959942036534,
5.03643203093243)) ;
#82479 = CARTESIAN_POINT('Ctrl Pts',(0.287142172077644,1.48469945082299,5.01700985054969)) ;
#82480 = CARTESIAN_POINT('Ctrl Pts',(0.474399076081781,1.43586485023365,5.00664393187212)) ;
#82481 = CARTESIAN_POINT('Ctrl Pts',(0.827110495698803,1.267120446311,4.9849867512302)) ;
#82482 = CARTESIAN_POINT('Ctrl Pts',(0.98794944184971,1.14615564342732,4.97388825041206)) ;
#82483 = CARTESIAN_POINT('Ctrl Pts',(1.24825034059657,0.85370948220949,4.95324101310364)) ;
#82484 = CARTESIAN_POINT('Ctrl Pts',(1.34724911561222,0.686926261582246,4.9444125700879)) ;
#82485 = CARTESIAN_POINT('Ctrl Pts',(1.47752437579179,0.323349875497477,4.92421388197208)) ;
#82486 = CARTESIAN_POINT('Ctrl Pts',(1.50691094426993,0.12977056403595,4.91345947577977)) ;
#82487 = CARTESIAN_POINT('Ctrl Pts',(1.49014787033123,-0.262669902249338,
4.89165722765281)) ;
#82488 = CARTESIAN_POINT('Ctrl Pts',(1.44224511840853,-0.457696413105614,
4.88082242149413)) ;
#82489 = CARTESIAN_POINT('Ctrl Pts',(1.27694453026968,-0.809618891741693,
4.86127117268102)) ;
#82490 = CARTESIAN_POINT('Ctrl Pts',(1.1642916284679,-0.964629821186249,4.85213840094854)) ;
#82491 = CARTESIAN_POINT('Ctrl Pts',(0.882501782854819,-1.22869548071468,
4.83124562347111)) ;
#82492 = CARTESIAN_POINT('Ctrl Pts',(0.714381461137337,-1.33347598066378,
4.8202463612781)) ;
#82493 = CARTESIAN_POINT('Ctrl Pts',(0.343487252002561,-1.4738235931734,4.79850316052909)) ;
#82494 = CARTESIAN_POINT('Ctrl Pts',(0.143841614987716,-1.50645645807607,
4.78834992898549)) ;
#82495 = CARTESIAN_POINT('Ctrl Pts',(-0.247427045197487,-1.49176808150959,
4.76911699633502)) ;
#82496 = CARTESIAN_POINT('Ctrl Pts',(-0.43542601141659,-1.44809320631804,
4.75885870087798)) ;
#82497 = CARTESIAN_POINT('Ctrl Pts',(-0.791649844461233,-1.28948614391686,
4.73731412198628)) ;
#82498 = CARTESIAN_POINT('Ctrl Pts',(-0.955328727134092,-1.17338797641708,
4.72621416897474)) ;
#82499 = CARTESIAN_POINT('Ctrl Pts',(-1.22417988671094,-0.888109521141881,
4.70535465999318)) ;
#82500 = CARTESIAN_POINT('Ctrl Pts',(-1.32828705678375,-0.723190900739279,
4.69642727226329)) ;
#82501 = CARTESIAN_POINT('Ctrl Pts',(-1.46552817676442,-0.369810352166903,
4.67679501956483)) ;
#82502 = CARTESIAN_POINT('Ctrl Pts',(-1.5,-0.185662761463316,4.66656459785906)) ;
#82503 = CARTESIAN_POINT('Ctrl Pts',(-1.5,-1.21430643318376E-15,4.65624999999999)) ;
#82504 = CARTESIAN_POINT('Ctrl Pts',(-1.5,1.95223456881304E-14,4.59374999999999)) ;
#82505 = CARTESIAN_POINT('Ctrl Pts',(-1.5,-0.0320111368243377,4.59552839649023)) ;
#82506 = CARTESIAN_POINT('Ctrl Pts',(-1.49897530445879,-0.0640561019145464,
4.59730867232857)) ;
#82507 = CARTESIAN_POINT('Ctrl Pts',(-1.48462161618699,-0.287671320592608,
4.60973174003291)) ;
#82508 = CARTESIAN_POINT('Ctrl Pts',(-1.43565537777401,-0.475152250276413,
4.62014734723757)) ;
#82509 = CARTESIAN_POINT('Ctrl Pts',(-1.26731784412456,-0.826371888221436,
4.63965954934563)) ;
#82510 = CARTESIAN_POINT('Ctrl Pts',(-1.14766192513784,-0.985838022986705,
4.64925081274265)) ;
#82511 = CARTESIAN_POINT('Ctrl Pts',(-0.853691440025888,-1.24901877064535,
4.67070505062593)) ;
#82512 = CARTESIAN_POINT('Ctrl Pts',(-0.682389630276099,-1.35025200138103,
4.68175884697734)) ;
#82513 = CARTESIAN_POINT('Ctrl Pts',(-0.317085410119675,-1.4783693765413,
4.70289337044097)) ;
#82514 = CARTESIAN_POINT('Ctrl Pts',(-0.127469282574041,-1.50659832384462,
4.71243384450923)) ;
#82515 = CARTESIAN_POINT('Ctrl Pts',(0.261009659059859,-1.49044119644595,
4.73157335539755)) ;
#82516 = CARTESIAN_POINT('Ctrl Pts',(0.456042047119949,-1.44275517335332,
4.74228146729572)) ;
#82517 = CARTESIAN_POINT('Ctrl Pts',(0.812462143084706,-1.27586824385568,
4.7640654851998)) ;
#82518 = CARTESIAN_POINT('Ctrl Pts',(0.971099373314515,-1.15970239190812,
4.77492475171863)) ;
#82519 = CARTESIAN_POINT('Ctrl Pts',(1.23251076416176,-0.87600802413215,4.79538231222975)) ;
#82520 = CARTESIAN_POINT('Ctrl Pts',(1.333898276055,-0.712169709791253,4.80418501612269)) ;
#82521 = CARTESIAN_POINT('Ctrl Pts',(1.47306533952245,-0.346621996132162,
4.82449322243709)) ;
#82522 = CARTESIAN_POINT('Ctrl Pts',(1.50611694989444,-0.147191233787431,
4.83557270923402)) ;
#82523 = CARTESIAN_POINT('Ctrl Pts',(1.49229096300096,0.245211971655472,4.85737288731418)) ;
#82524 = CARTESIAN_POINT('Ctrl Pts',(1.44853602465491,0.434537231392048,4.86789095729955)) ;
#82525 = CARTESIAN_POINT('Ctrl Pts',(1.29052135595237,0.789217113746672,4.88759539520814)) ;
#82526 = CARTESIAN_POINT('Ctrl Pts',(1.17665589276148,0.95068459184539,4.89687935562658)) ;
#82527 = CARTESIAN_POINT('Ctrl Pts',(0.891876127301889,1.22214282251285,4.91812133488799)) ;
#82528 = CARTESIAN_POINT('Ctrl Pts',(0.723234361962776,1.32891104260048,4.92920089949725)) ;
#82529 = CARTESIAN_POINT('Ctrl Pts',(0.361056190313792,1.46829590893425,4.95049800674786)) ;
#82530 = CARTESIAN_POINT('Ctrl Pts',(0.172013588665832,1.50220377904007,4.96041277627217)) ;
#82531 = CARTESIAN_POINT('Ctrl Pts',(-0.217048948562838,1.49747032732517,
4.97926304109208)) ;
#82532 = CARTESIAN_POINT('Ctrl Pts',(-0.413363412819334,1.45555212138303,
4.98987261976694)) ;
#82533 = CARTESIAN_POINT('Ctrl Pts',(-0.775021318655709,1.29903559041336,
5.0116205752902)) ;
#82534 = CARTESIAN_POINT('Ctrl Pts',(-0.937419838664237,1.18718251485956,
5.0225410076036)) ;
#82535 = CARTESIAN_POINT('Ctrl Pts',(-1.20676155290839,0.911033510993222,
5.04317052253512)) ;
#82536 = CARTESIAN_POINT('Ctrl Pts',(-1.31252281641666,0.750688607805427,
5.05204507734413)) ;
#82537 = CARTESIAN_POINT('Ctrl Pts',(-1.46110471375442,0.392569188654103,
5.07194060063031)) ;
#82538 = CARTESIAN_POINT('Ctrl Pts',(-1.5,0.197217047500341,5.08279349736108)) ;
#82539 = CARTESIAN_POINT('Ctrl Pts',(-1.5,-9.85322934354826E-15,5.09374999999999)) ;
#82540 = CARTESIAN_POINT('Origin',(0.,0.,0.)) ;
#82541 = CARTESIAN_POINT('',(-1.5,-5.13989382502856E-15,5.65624999999999)) ;
#82542 = CARTESIAN_POINT('',(-1.5,-8.41852119462473E-15,5.59374999999999)) ;
#82543 = CARTESIAN_POINT('',(-1.5,-1.83697019872103E-16,0.)) ;
#82544 = CARTESIAN_POINT('Ctrl Pts',(-1.5,0.,5.65624999999999)) ;
#82545 = CARTESIAN_POINT('Ctrl Pts',(-1.5,0.0650814565690276,5.65263436352393)) ;
#82546 = CARTESIAN_POINT('Ctrl Pts',(-1.49576451485979,0.130229312342809,
5.64901503820318)) ;
#82547 = CARTESIAN_POINT('Ctrl Pts',(-1.46141322360216,0.392188518898155,
5.63446174895011)) ;
#82548 = CARTESIAN_POINT('Ctrl Pts',(-1.39662093449307,0.582176712153985,
5.62394004736951)) ;
#82549 = CARTESIAN_POINT('Ctrl Pts',(-1.20092845884759,0.918757008787729,
5.60517533606088)) ;
#82550 = CARTESIAN_POINT('Ctrl Pts',(-1.07457820645903,1.06376728008664,5.59506824361685)) ;
#82551 = CARTESIAN_POINT('Ctrl Pts',(-0.768594274302649,1.3032498457893,5.57369429132526)) ;
#82552 = CARTESIAN_POINT('Ctrl Pts',(-0.590053583094108,1.39321180250573,
5.56260530507226)) ;
#82553 = CARTESIAN_POINT('Ctrl Pts',(-0.211298116530195,1.4977819459821,5.54147769798311)) ;
#82554 = CARTESIAN_POINT('Ctrl Pts',(-0.0151228445687375,1.51253455941324,
5.53232578040448)) ;
#82555 = CARTESIAN_POINT('Ctrl Pts',(0.369873909890915,1.46641759897383,5.51252158874024)) ;
#82556 = CARTESIAN_POINT('Ctrl Pts',(0.555114459108075,1.40677584347651,5.50195248323015)) ;
#82557 = CARTESIAN_POINT('Ctrl Pts',(0.899528101985093,1.21697598270753,5.48010965575648)) ;
#82558 = CARTESIAN_POINT('Ctrl Pts',(1.05394430128351,1.0860013605719,5.46904211895559)) ;
#82559 = CARTESIAN_POINT('Ctrl Pts',(1.29606201221943,0.778822370194039,5.44886047542417)) ;
#82560 = CARTESIAN_POINT('Ctrl Pts',(1.38444040948578,0.608004917147279,5.44002805095262)) ;
#82561 = CARTESIAN_POINT('Ctrl Pts',(1.49377708886147,0.238094230949914,5.41947745727499)) ;
#82562 = CARTESIAN_POINT('Ctrl Pts',(1.51204684812289,0.0420157054333175,
5.40858420585741)) ;
#82563 = CARTESIAN_POINT('Ctrl Pts',(1.47212613995471,-0.349790423796505,
5.38681719867797)) ;
#82564 = CARTESIAN_POINT('Ctrl Pts',(1.41286922649614,-0.541603734889573,
5.37616090361725)) ;
#82565 = CARTESIAN_POINT('Ctrl Pts',(1.22713958797241,-0.883327715334427,
5.35717623803698)) ;
#82566 = CARTESIAN_POINT('Ctrl Pts',(1.10540567548876,-1.03162909753595,5.34744415820516)) ;
#82567 = CARTESIAN_POINT('Ctrl Pts',(0.807403531470688,-1.27947723051666,
5.32622185300559)) ;
#82568 = CARTESIAN_POINT('Ctrl Pts',(0.63220846676621,-1.37450981795897,5.31515298242931)) ;
#82569 = CARTESIAN_POINT('Ctrl Pts',(0.255900539130508,-1.49102034763574,
5.29381145521729)) ;
#82570 = CARTESIAN_POINT('Ctrl Pts',(0.058598105097295,-1.51168064046602,
5.28439376488116)) ;
#82571 = CARTESIAN_POINT('Ctrl Pts',(-0.328587791549555,-1.47614852043145,
5.26477827140891)) ;
#82572 = CARTESIAN_POINT('Ctrl Pts',(-0.514915163604716,-1.42190993977774,
5.25430696430074)) ;
#82573 = CARTESIAN_POINT('Ctrl Pts',(-0.863637689112102,-1.24260683538295,
5.23254840218082)) ;
#82574 = CARTESIAN_POINT('Ctrl Pts',(-1.02134589636858,-1.11660552177777,
5.22146062603237)) ;
#82575 = CARTESIAN_POINT('Ctrl Pts',(-1.27260482338139,-0.816749981215801,
5.20104260469895)) ;
#82576 = CARTESIAN_POINT('Ctrl Pts',(-1.36628395637511,-0.647976112865997,
5.192248672937)) ;
#82577 = CARTESIAN_POINT('Ctrl Pts',(-1.4750072213027,-0.315423368644648,
5.17377352048026)) ;
#82578 = CARTESIAN_POINT('Ctrl Pts',(-1.5,-0.158084744109952,5.16503248578388)) ;
#82579 = CARTESIAN_POINT('Ctrl Pts',(-1.5,-8.67361737988404E-15,5.15624999999999)) ;
#82580 = CARTESIAN_POINT('Ctrl Pts',(-1.5,-9.37072593030258E-15,5.09374999999999)) ;
#82581 = CARTESIAN_POINT('Ctrl Pts',(-1.5,-0.00344187472693873,5.0939412152626)) ;
#82582 = CARTESIAN_POINT('Ctrl Pts',(-1.49998815350225,-0.00688431746682617,
5.09413246208148)) ;
#82583 = CARTESIAN_POINT('Ctrl Pts',(-1.49863541206654,-0.203360670571187,
5.10504781503172)) ;
#82584 = CARTESIAN_POINT('Ctrl Pts',(-1.46005586441752,-0.394355894599877,
5.11565866081109)) ;
#82585 = CARTESIAN_POINT('Ctrl Pts',(-1.31214236584632,-0.752343006402527,
5.13554683368902)) ;
#82586 = CARTESIAN_POINT('Ctrl Pts',(-1.20380450774007,-0.915750154214858,
5.14460276623412)) ;
#82587 = CARTESIAN_POINT('Ctrl Pts',(-0.927980887698286,-1.19505702468341,
5.16563186052046)) ;
#82588 = CARTESIAN_POINT('Ctrl Pts',(-0.762075891344222,-1.30711280946583,
5.17672662906761)) ;
#82589 = CARTESIAN_POINT('Ctrl Pts',(-0.403179906210228,-1.4573462967812,
5.19816717262872)) ;
#82590 = CARTESIAN_POINT('Ctrl Pts',(-0.214676580361502,-1.49677985789189,
5.20833191981973)) ;
#82591 = CARTESIAN_POINT('Ctrl Pts',(0.174895511444021,-1.50296666459241,
5.22724707156747)) ;
#82592 = CARTESIAN_POINT('Ctrl Pts',(0.372335002413048,-1.46659980515433,
5.23759175934614)) ;
#82593 = CARTESIAN_POINT('Ctrl Pts',(0.738836998698976,-1.32003003331521,
5.25929647741508)) ;
#82594 = CARTESIAN_POINT('Ctrl Pts',(0.904703092032137,-1.21238450586634,
5.2702668670916)) ;
#82595 = CARTESIAN_POINT('Ctrl Pts',(1.18152734442406,-0.943462455361497,
5.29105563710312)) ;
#82596 = CARTESIAN_POINT('Ctrl Pts',(1.29142533718613,-0.786344642180421,
5.30006418654552)) ;
#82597 = CARTESIAN_POINT('Ctrl Pts',(1.45034640196986,-0.431344230680077,
5.31978643162887)) ;
#82598 = CARTESIAN_POINT('Ctrl Pts',(1.49469098466996,-0.235461288359372,
5.33066881731336)) ;
#82599 = CARTESIAN_POINT('Ctrl Pts',(1.50428467728115,0.156896843711251,5.35246649131728)) ;
#82600 = CARTESIAN_POINT('Ctrl Pts',(1.47149572243588,0.349575647701331,5.36317086931673)) ;
#82601 = CARTESIAN_POINT('Ctrl Pts',(1.33473263596281,0.711123641425198,5.38325686896805)) ;
#82602 = CARTESIAN_POINT('Ctrl Pts',(1.232343504703,0.876664118202146,5.39214395987996)) ;
#82603 = CARTESIAN_POINT('Ctrl Pts',(0.966352187603716,1.16435852619215,5.4129329844238)) ;
#82604 = CARTESIAN_POINT('Ctrl Pts',(0.80360990004434,1.28209565947801,5.42403340230932)) ;
#82605 = CARTESIAN_POINT('Ctrl Pts',(0.448532344779636,1.44410974785279,5.445617470496)) ;
#82606 = CARTESIAN_POINT('Ctrl Pts',(0.260766569034991,1.48951565285212,5.45591263073244)) ;
#82607 = CARTESIAN_POINT('Ctrl Pts',(-0.129850519027224,1.50763748789584,
5.47520958845111)) ;
#82608 = CARTESIAN_POINT('Ctrl Pts',(-0.32910134254664,1.47700956127791,5.48522251902366)) ;
#82609 = CARTESIAN_POINT('Ctrl Pts',(-0.700944457067442,1.34061643389493,
5.50690152719526)) ;
#82610 = CARTESIAN_POINT('Ctrl Pts',(-0.870273581683968,1.23741727326228,
5.51791502185275)) ;
#82611 = CARTESIAN_POINT('Ctrl Pts',(-1.15476252292559,0.976012346349693,
5.53886375038982)) ;
#82612 = CARTESIAN_POINT('Ctrl Pts',(-1.26891717769988,0.822135710191326,
5.54807579387825)) ;
#82613 = CARTESIAN_POINT('Ctrl Pts',(-1.43766062436454,0.471895763218968,
5.56753356871005)) ;
#82614 = CARTESIAN_POINT('Ctrl Pts',(-1.48748217415704,0.277360504023277,
5.57834108310981)) ;
#82615 = CARTESIAN_POINT('Ctrl Pts',(-1.49931070630541,0.0525329777524311,
5.59083150123597)) ;
#82616 = CARTESIAN_POINT('Ctrl Pts',(-1.5,0.0262545598512842,5.59229141334158)) ;
#82617 = CARTESIAN_POINT('Ctrl Pts',(-1.5,-1.89645643827552E-14,5.59374999999999)) ;
#82618 = CARTESIAN_POINT('Origin',(0.,0.,0.)) ;
#82619 = CARTESIAN_POINT('',(-1.5,4.24821278652342E-15,6.15624999999999)) ;
#82620 = CARTESIAN_POINT('',(-1.5,-7.2389092309605E-15,6.09374999999999)) ;
#82621 = CARTESIAN_POINT('',(-1.5,-1.83697019872103E-16,0.)) ;
#82622 = CARTESIAN_POINT('Ctrl Pts',(-1.5,9.81688131253131E-15,6.15624999999999)) ;
#82623 = CARTESIAN_POINT('Ctrl Pts',(-1.5,0.0938400860056215,6.15103666188857)) ;
#82624 = CARTESIAN_POINT('Ctrl Pts',(-1.49119408246604,0.18769741776628,6.14582236567966)) ;
#82625 = CARTESIAN_POINT('Ctrl Pts',(-1.43645284865028,0.475454866950807,
6.12983584072496)) ;
#82626 = CARTESIAN_POINT('Ctrl Pts',(-1.36095535503423,0.661232582555009,
6.1200280899777)) ;
#82627 = CARTESIAN_POINT('Ctrl Pts',(-1.14580339935446,0.986859460641902,
6.1006313956257)) ;
#82628 = CARTESIAN_POINT('Ctrl Pts',(-1.01043659121357,1.12505731080659,6.09027972786117)) ;
#82629 = CARTESIAN_POINT('Ctrl Pts',(-0.68888878141633,1.34725938427253,6.06863697183069)) ;
#82630 = CARTESIAN_POINT('Ctrl Pts',(-0.504084036591963,1.42673943002813,
6.05753777035093)) ;
#82631 = CARTESIAN_POINT('Ctrl Pts',(-0.120923480652032,1.50744063774349,
6.03686124929372)) ;
#82632 = CARTESIAN_POINT('Ctrl Pts',(0.0731394438453323,1.51051288213524,
6.02802310137105)) ;
#82633 = CARTESIAN_POINT('Ctrl Pts',(0.453451699063325,1.44290958093571,6.00784744998277)) ;
#82634 = CARTESIAN_POINT('Ctrl Pts',(0.635984208094232,1.37226742224584,5.99710306836153)) ;
#82635 = CARTESIAN_POINT('Ctrl Pts',(0.968198538908579,1.16281092222751,5.97530116280622)) ;
#82636 = CARTESIAN_POINT('Ctrl Pts',(1.11366771024356,1.02435463556251,5.96445626607422)) ;
#82637 = CARTESIAN_POINT('Ctrl Pts',(1.33699766836063,0.706055532219886,5.94486965669495)) ;
#82638 = CARTESIAN_POINT('Ctrl Pts',(1.41557334053027,0.531266268116329,5.93576479267313)) ;
#82639 = CARTESIAN_POINT('Ctrl Pts',(1.50474854535445,0.155580242132143,5.91489334678512)) ;
#82640 = CARTESIAN_POINT('Ctrl Pts',(1.51217740036442,-0.0423044321232613,
5.90389975377093)) ;
#82641 = CARTESIAN_POINT('Ctrl Pts',(1.44975514536609,-0.434115159917777,
5.88213249111568)) ;
#82642 = CARTESIAN_POINT('Ctrl Pts',(1.37877799478145,-0.623840646366446,
5.87192424702647)) ;
#82643 = CARTESIAN_POINT('Ctrl Pts',(1.17142571722235,-0.956205955623757,
5.8527156362194)) ;
#82644 = CARTESIAN_POINT('Ctrl Pts',(1.04012680410663,-1.09757991078438,5.84247146000674)) ;
#82645 = CARTESIAN_POINT('Ctrl Pts',(0.725560469845027,-1.32778690799201,
5.82094224138175)) ;
#82646 = CARTESIAN_POINT('Ctrl Pts',(0.543539747779754,-1.41210078244945,
5.80984271323995)) ;
#82647 = CARTESIAN_POINT('Ctrl Pts',(0.162309679028314,-1.50368453042566,
5.78895678000588)) ;
#82648 = CARTESIAN_POINT('Ctrl Pts',(-0.0326899750580471,-1.51206457167333,
5.78001232983263)) ;
#82649 = CARTESIAN_POINT('Ctrl Pts',(-0.415190720627786,-1.45431417734196,
5.76000507651066)) ;
#82650 = CARTESIAN_POINT('Ctrl Pts',(-0.599048900134903,-1.38871839313835,
5.74933709060796)) ;
#82651 = CARTESIAN_POINT('Ctrl Pts',(-0.936397357604732,-1.18857375385767,
5.72754683206703)) ;
#82652 = CARTESIAN_POINT('Ctrl Pts',(-1.08557354820172,-1.05408538577059,
5.71663380124812)) ;
#82653 = CARTESIAN_POINT('Ctrl Pts',(-1.31757646822544,-0.741728147345655,
5.69679496559784)) ;
#82654 = CARTESIAN_POINT('Ctrl Pts',(-1.4009043199849,-0.568897104360946,
5.68785539468672)) ;
#82655 = CARTESIAN_POINT('Ctrl Pts',(-1.48317308356884,-0.259166673181986,
5.67064814851011)) ;
#82656 = CARTESIAN_POINT('Ctrl Pts',(-1.5,-0.12971522306197,5.66345640128121)) ;
#82657 = CARTESIAN_POINT('Ctrl Pts',(-1.5,1.11022302462516E-15,5.65624999999999)) ;
#82658 = CARTESIAN_POINT('Ctrl Pts',(-1.5,-1.87697080100691E-14,5.59374999999999)) ;
#82659 = CARTESIAN_POINT('Ctrl Pts',(-1.5,-0.167469537432786,5.6030538631907)) ;
#82660 = CARTESIAN_POINT('Ctrl Pts',(-1.47195184100008,-0.333968347888134,
5.61230379710489)) ;
#82661 = CARTESIAN_POINT('Ctrl Pts',(-1.35382876989179,-0.6737723606495,5.63118179781386)) ;
#82662 = CARTESIAN_POINT('Ctrl Pts',(-1.25664401481313,-0.841229768361045,
5.63999051354659)) ;
#82663 = CARTESIAN_POINT('Ctrl Pts',(-0.999412713006369,-1.13620944885856,
5.66056044033892)) ;
#82664 = CARTESIAN_POINT('Ctrl Pts',(-0.839622037268671,-1.25889663974064,
5.67165635033435)) ;
#82665 = CARTESIAN_POINT('Ctrl Pts',(-0.488233431159106,-1.43124403379356,
5.69334997014089)) ;
#82666 = CARTESIAN_POINT('Ctrl Pts',(-0.301275547724059,-1.48191920452157,
5.70375262913292)) ;
#82667 = CARTESIAN_POINT('Ctrl Pts',(0.0873162328487167,-1.51044673774205,
5.72324119137115)) ;
#82668 = CARTESIAN_POINT('Ctrl Pts',(0.285390240297882,-1.48581513460725,
5.73287486837702)) ;
#82669 = CARTESIAN_POINT('Ctrl Pts',(0.659969730966546,-1.36134047243951,
5.75435446202922)) ;
#82670 = CARTESIAN_POINT('Ctrl Pts',(0.832858396725634,-1.26299416389039,
5.76540441374301)) ;
#82671 = CARTESIAN_POINT('Ctrl Pts',(1.12545908186054,-1.00967855059635,5.78651871558404)) ;
#82672 = CARTESIAN_POINT('Ctrl Pts',(1.24414979380325,-0.859168050038595,
5.79601844166451)) ;
#82673 = CARTESIAN_POINT('Ctrl Pts',(1.4231386145617,-0.514022370003128,5.81519320166649)) ;
#82674 = CARTESIAN_POINT('Ctrl Pts',(1.47865917119759,-0.321069586856946,
5.82591280073016)) ;
#82675 = CARTESIAN_POINT('Ctrl Pts',(1.51091126307826,0.071098839192046,5.84769993551066)) ;
#82676 = CARTESIAN_POINT('Ctrl Pts',(1.48893860924911,0.266419057375733,5.85855105874309)) ;
#82677 = CARTESIAN_POINT('Ctrl Pts',(1.37266513433757,0.634268127106245,5.87898711817257)) ;
#82678 = CARTESIAN_POINT('Ctrl Pts',(1.28082105809126,0.803741777759219,5.88778596193725)) ;
#82679 = CARTESIAN_POINT('Ctrl Pts',(1.03271198358855,1.10613951420092,5.90812305247334)) ;
#82680 = CARTESIAN_POINT('Ctrl Pts',(0.87612409845522,1.2338682185265,5.91920491017406)) ;
#82681 = CARTESIAN_POINT('Ctrl Pts',(0.528855580859981,1.41680906373381,5.9409945646616)) ;
#82682 = CARTESIAN_POINT('Ctrl Pts',(0.342886244098983,1.47291663030694,5.95150056206419)) ;
#82683 = CARTESIAN_POINT('Ctrl Pts',(-0.0435503507273721,1.51211432137883,
5.9711818261535)) ;
#82684 = CARTESIAN_POINT('Ctrl Pts',(-0.240456802888681,1.49351229186924,
5.98049919743776)) ;
#82685 = CARTESIAN_POINT('Ctrl Pts',(-0.617634247619035,1.38114985604414,
6.00176733448129)) ;
#82686 = CARTESIAN_POINT('Ctrl Pts',(-0.794007068072516,1.28786509067901,
6.0128443192442)) ;
#82687 = CARTESIAN_POINT('Ctrl Pts',(-1.09481650099445,1.04288543426395,6.03412201028953)) ;
#82688 = CARTESIAN_POINT('Ctrl Pts',(-1.21814041222709,0.895723138282387,
6.04398760342875)) ;
#82689 = CARTESIAN_POINT('Ctrl Pts',(-1.40734887121585,0.555786377324176,
6.06287297903754)) ;
#82690 = CARTESIAN_POINT('Ctrl Pts',(-1.46852860805036,0.364591536553745,
6.0734949146359)) ;
#82691 = CARTESIAN_POINT('Ctrl Pts',(-1.49689589468376,0.111493134674231,
6.08755593696254)) ;
#82692 = CARTESIAN_POINT('Ctrl Pts',(-1.5,0.0557152328261553,6.09065470928742)) ;
#82693 = CARTESIAN_POINT('Ctrl Pts',(-1.5,-9.37072593030258E-15,6.09374999999999)) ;
#82694 = CARTESIAN_POINT('Origin',(0.,0.,0.)) ;
#82695 = CARTESIAN_POINT('',(-1.5,5.23978324035715E-16,6.65624999999999)) ;
#82696 = CARTESIAN_POINT('',(-1.5,-5.28734532048659E-15,6.59374999999999)) ;
#82697 = CARTESIAN_POINT('',(-1.5,-1.83697019872103E-16,0.)) ;
#82698 = CARTESIAN_POINT('Ctrl Pts',(-1.5,-4.5102810375397E-16,6.65624999999999)) ;
#82699 = CARTESIAN_POINT('Ctrl Pts',(-1.5,0.124981814104662,6.64930656588306)) ;
#82700 = CARTESIAN_POINT('Ctrl Pts',(-1.48437885790166,0.249763345316788,
6.64237425859351)) ;
#82701 = CARTESIAN_POINT('Ctrl Pts',(-1.40497923519992,0.560453320344288,
6.62511370442532)) ;
#82702 = CARTESIAN_POINT('Ctrl Pts',(-1.32025838181587,0.738229996303097,
6.61593123889224)) ;
#82703 = CARTESIAN_POINT('Ctrl Pts',(-1.08887343464721,1.04953098763693,6.59615147567178)) ;
#82704 = CARTESIAN_POINT('Ctrl Pts',(-0.94513821388451,1.18061729652795,6.58559472528041)) ;
#82705 = CARTESIAN_POINT('Ctrl Pts',(-0.609454725731597,1.385176787341,6.56376193784831)) ;
#82706 = CARTESIAN_POINT('Ctrl Pts',(-0.419159520584368,1.45412205074647,
6.55269120931616)) ;
#82707 = CARTESIAN_POINT('Ctrl Pts',(-0.0323006526586065,1.51172991041425,
6.53247823503077)) ;
#82708 = CARTESIAN_POINT('Ctrl Pts',(0.159932450966637,1.50359436742395,6.52365508990474)) ;
#82709 = CARTESIAN_POINT('Ctrl Pts',(0.535293751442473,1.41474059569989,6.50312735058965)) ;
#82710 = CARTESIAN_POINT('Ctrl Pts',(0.714483288689404,1.33324259147996,6.49224225650864)) ;
#82711 = CARTESIAN_POINT('Ctrl Pts',(1.03468086348225,1.10405900253399,6.47047053270454)) ;
#82712 = CARTESIAN_POINT('Ctrl Pts',(1.17174544516121,0.957365362404684,6.45980118660689)) ;
#82713 = CARTESIAN_POINT('Ctrl Pts',(1.37609716509034,0.626482797821238,6.44077812754815)) ;
#82714 = CARTESIAN_POINT('Ctrl Pts',(1.44435403624083,0.447218209615709,6.43109545608976)) ;
#82715 = CARTESIAN_POINT('Ctrl Pts',(1.51149825482502,0.0656056189570403,
6.40989475660872)) ;
#82716 = CARTESIAN_POINT('Ctrl Pts',(1.50701414843509,-0.133571729305174,
6.39882934837193)) ;
#82717 = CARTESIAN_POINT('Ctrl Pts',(1.42132330124281,-0.518225845657976,
6.37745967524123)) ;
#82718 = CARTESIAN_POINT('Ctrl Pts',(1.34117892727577,-0.699958049992881,
6.36800088872471)) ;
#82719 = CARTESIAN_POINT('Ctrl Pts',(1.11789709948255,-1.0184613443221,6.34841092304488)) ;
#82720 = CARTESIAN_POINT('Ctrl Pts',(0.978319502241427,-1.15318222579219,
6.33795324605904)) ;
#82721 = CARTESIAN_POINT('Ctrl Pts',(0.649619225769072,-1.36671320489274,
6.31620723054758)) ;
#82722 = CARTESIAN_POINT('Ctrl Pts',(0.462010248026866,-1.44099612190541,
6.30511747503596)) ;
#82723 = CARTESIAN_POINT('Ctrl Pts',(0.0769441254254464,-1.51020675207094,
6.28466845506971)) ;
#82724 = CARTESIAN_POINT('Ctrl Pts',(-0.116180026277667,-1.50769626983412,
6.27587407115268)) ;
#82725 = CARTESIAN_POINT('Ctrl Pts',(-0.494082706878714,-1.42957943689278,
6.25552230792883)) ;
#82726 = CARTESIAN_POINT('Ctrl Pts',(-0.675043776732769,-1.35355845111559,
6.2447041203467)) ;
#82727 = CARTESIAN_POINT('Ctrl Pts',(-1.0014718743312,-1.13427482675704,6.22290762939067)) ;
#82728 = CARTESIAN_POINT('Ctrl Pts',(-1.14285079494042,-0.991685518632995,
6.21214471878683)) ;
#82729 = CARTESIAN_POINT('Ctrl Pts',(-1.35683680668118,-0.667122033599381,
6.19283365963467)) ;
#82730 = CARTESIAN_POINT('Ctrl Pts',(-1.43032222715605,-0.490163771142688,
6.18348132061904)) ;
#82731 = CARTESIAN_POINT('Ctrl Pts',(-1.48960830908396,-0.203858299136244,
6.16757546106313)) ;
#82732 = CARTESIAN_POINT('Ctrl Pts',(-1.5,-0.101939325142457,6.16191329584124)) ;
#82733 = CARTESIAN_POINT('Ctrl Pts',(-1.5,1.17787724018825E-14,6.15624999999999)) ;
#82734 = CARTESIAN_POINT('Ctrl Pts',(-1.5,-9.92261828258734E-15,6.09374999999999)) ;
#82735 = CARTESIAN_POINT('Ctrl Pts',(-1.5,-0.138795933253646,6.10146088518074)) ;
#82736 = CARTESIAN_POINT('Ctrl Pts',(-1.48073442875306,-0.277202948098713,
6.10915016378326)) ;
#82737 = CARTESIAN_POINT('Ctrl Pts',(-1.39032217281161,-0.59437475913241,
6.12677081995179)) ;
#82738 = CARTESIAN_POINT('Ctrl Pts',(-1.30371818610947,-0.765891971535818,
6.13563293984562)) ;
#82739 = CARTESIAN_POINT('Ctrl Pts',(-1.06468844715775,-1.0755083150188,6.15573371750861)) ;
#82740 = CARTESIAN_POINT('Ctrl Pts',(-0.911411885737207,-1.2081353020028,
6.1667923224801)) ;
#82741 = CARTESIAN_POINT('Ctrl Pts',(-0.56851446104285,-1.40143879973568,
6.18865952412143)) ;
#82742 = CARTESIAN_POINT('Ctrl Pts',(-0.383673635175328,-1.46289104837478,
6.19925968940906)) ;
#82743 = CARTESIAN_POINT('Ctrl Pts',(0.000573644848951456,-1.51254780663004,
6.21912614968483)) ;
#82744 = CARTESIAN_POINT('Ctrl Pts',(0.196383733168085,-1.49974703911056,
6.22820554345879)) ;
#82745 = CARTESIAN_POINT('Ctrl Pts',(0.57591537113953,-1.39914381604468,6.24926030187857)) ;
#82746 = CARTESIAN_POINT('Ctrl Pts',(0.755536941194608,-1.31089279521363,
6.26035376594251)) ;
#82747 = CARTESIAN_POINT('Ctrl Pts',(1.06417064803916,-1.0742108545428,6.28177741043845)) ;
#82748 = CARTESIAN_POINT('Ctrl Pts',(1.19204295342378,-0.930293304306606,
6.29192737932854)) ;
#82749 = CARTESIAN_POINT('Ctrl Pts',(1.39103649701779,-0.595407548986935,
6.31080384275084)) ;
#82750 = CARTESIAN_POINT('Ctrl Pts',(1.45763241901129,-0.406022035808256,
6.32119322023287)) ;
#82751 = CARTESIAN_POINT('Ctrl Pts',(1.51264770441934,-0.0152206621079717,
6.34290440766066)) ;
#82752 = CARTESIAN_POINT('Ctrl Pts',(1.50171959659393,0.182147600367653,6.35386931113153)) ;
#82753 = CARTESIAN_POINT('Ctrl Pts',(1.4060553413921,0.556010522676409,6.37463947348201)) ;
#82754 = CARTESIAN_POINT('Ctrl Pts',(1.3243658414026,0.729509542578257,6.38362890604055)) ;
#82755 = CARTESIAN_POINT('Ctrl Pts',(1.09534643232919,1.0439251098773,6.40338137325538)) ;
#82756 = CARTESIAN_POINT('Ctrl Pts',(0.947435360849062,1.17979259578049,6.41427184483062)) ;
#82757 = CARTESIAN_POINT('Ctrl Pts',(0.611826754406933,1.38316072366324,6.43606793610001)) ;
#82758 = CARTESIAN_POINT('Ctrl Pts',(0.428409966272987,1.45049801396441,6.44676306071974)) ;
#82759 = CARTESIAN_POINT('Ctrl Pts',(0.046656659607905,1.51164850997432,6.4668288001395)) ;
#82760 = CARTESIAN_POINT('Ctrl Pts',(-0.148013323645245,1.50510892206033,
6.47572937985251)) ;
#82761 = CARTESIAN_POINT('Ctrl Pts',(-0.529926193154905,1.4172928056006,6.49654350792237)) ;
#82762 = CARTESIAN_POINT('Ctrl Pts',(-0.712924645156483,1.3346423648461,6.50764387062591)) ;
#82763 = CARTESIAN_POINT('Ctrl Pts',(-1.02993030182321,1.10718331722484,6.52921411927188)) ;
#82764 = CARTESIAN_POINT('Ctrl Pts',(-1.16264602587055,0.966895855390792,
6.53949628146208)) ;
#82765 = CARTESIAN_POINT('Ctrl Pts',(-1.37270991425259,0.636862577898985,
6.55877057604555)) ;
#82766 = CARTESIAN_POINT('Ctrl Pts',(-1.44526608981773,0.448516541760216,
6.56883241434665)) ;
#82767 = CARTESIAN_POINT('Ctrl Pts',(-1.4929329537697,0.168179439750475,6.58440669779164)) ;
#82768 = CARTESIAN_POINT('Ctrl Pts',(-1.5,0.0840663850849933,6.58907964527304)) ;
#82769 = CARTESIAN_POINT('Ctrl Pts',(-1.5,2.97483362866747E-16,6.59374999999999)) ;
#82770 = CARTESIAN_POINT('Origin',(0.,0.,0.)) ;
#82771 = CARTESIAN_POINT('',(-1.5,-1.70514134259448E-15,7.15624999999999)) ;
#82772 = CARTESIAN_POINT('',(-1.5,1.38700325333418E-15,7.09374999999999)) ;
#82773 = CARTESIAN_POINT('',(-1.5,-1.83697019872103E-16,0.)) ;
#82774 = CARTESIAN_POINT('Ctrl Pts',(-1.5,-7.11236625150491E-15,7.15624999999999)) ;
#82775 = CARTESIAN_POINT('Ctrl Pts',(-1.5,0.155970879159808,7.14758495115777)) ;
#82776 = CARTESIAN_POINT('Ctrl Pts',(-1.47567100304807,0.311268816362477,
7.13895728797986)) ;
#82777 = CARTESIAN_POINT('Ctrl Pts',(-1.36859153902948,0.643438650998488,
7.12050340827786)) ;
#82778 = CARTESIAN_POINT('Ctrl Pts',(-1.27483150901209,0.81354728074605,7.11165349066535)) ;
#82779 = CARTESIAN_POINT('Ctrl Pts',(-1.02723184549473,1.11012268705131,7.0915026405694)) ;
#82780 = CARTESIAN_POINT('Ctrl Pts',(-0.875333730341766,1.23343240344003,
7.08076916919696)) ;
#82781 = CARTESIAN_POINT('Ctrl Pts',(-0.52863446093955,1.41777460586891,7.05896797608639)) ;
#82782 = CARTESIAN_POINT('Ctrl Pts',(-0.336219533923613,1.47530195769444,
7.04811242659884)) ;
#82783 = CARTESIAN_POINT('Ctrl Pts',(0.0509867626765902,1.51112099286464,
7.02848798176849)) ;
#82784 = CARTESIAN_POINT('Ctrl Pts',(0.241744219449288,1.49253459485981,7.01941170345382)) ;
#82785 = CARTESIAN_POINT('Ctrl Pts',(0.612067889516041,1.38340728828563,6.99856318349895)) ;
#82786 = CARTESIAN_POINT('Ctrl Pts',(0.78745746631049,1.29164622821851,6.98757583021581)) ;
#82787 = CARTESIAN_POINT('Ctrl Pts',(1.09675715651085,1.04282559728137,6.96578295773999)) ;
#82788 = CARTESIAN_POINT('Ctrl Pts',(1.22636394567284,0.886764146108135,6.95551467478378)) ;
#82789 = CARTESIAN_POINT('Ctrl Pts',(1.41185802272716,0.541478724633405,6.93633215136852)) ;
#82790 = CARTESIAN_POINT('Ctrl Pts',(1.46929070030764,0.357357376336164,6.92610318757423)) ;
#82791 = CARTESIAN_POINT('Ctrl Pts',(1.51279019148619,-0.0298681335906356,
6.90459065924496)) ;
#82792 = CARTESIAN_POINT('Ctrl Pts',(1.49555855397567,-0.229648748802826,
6.89349173617762)) ;
#82793 = CARTESIAN_POINT('Ctrl Pts',(1.38568178600204,-0.606101868472665,
6.87257767397374)) ;
#82794 = CARTESIAN_POINT('Ctrl Pts',(1.29600326945513,-0.779644091130765,
6.86361387273169)) ;
#82795 = CARTESIAN_POINT('Ctrl Pts',(1.05575279960783,-1.08294642667726,6.84362975173546)) ;
#82796 = CARTESIAN_POINT('Ctrl Pts',(0.907525210975976,-1.20986361353978,
6.83297267113945)) ;
#82797 = CARTESIAN_POINT('Ctrl Pts',(0.566284158502573,-1.40316465850384,
6.81118522987622)) ;
#82798 = CARTESIAN_POINT('Ctrl Pts',(0.375451337987938,-1.46581143000135,
6.8002635934212)) ;
#82799 = CARTESIAN_POINT('Ctrl Pts',(-0.0109415681523102,-1.51197434190153,
6.78039095294844)) ;
#82800 = CARTESIAN_POINT('Ctrl Pts',(-0.202378019607965,-1.49841150830115,
6.77146895822236)) ;
#82801 = CARTESIAN_POINT('Ctrl Pts',(-0.575174916429631,-1.39907699561318,
6.75077346714216)) ;
#82802 = CARTESIAN_POINT('Ctrl Pts',(-0.752473738342542,-1.31225762170762,
6.73983152432047)) ;
#82803 = CARTESIAN_POINT('Ctrl Pts',(-1.06628383312216,-1.07356112140703,
6.71810287075417)) ;
#82804 = CARTESIAN_POINT('Ctrl Pts',(-1.19900989580016,-0.922982733540992,
6.70753435208992)) ;
#82805 = CARTESIAN_POINT('Ctrl Pts',(-1.3938697751391,-0.586005200031803,
6.68879866473212)) ;
#82806 = CARTESIAN_POINT('Ctrl Pts',(-1.45698248258737,-0.404394641375286,
6.67871636896529)) ;
#82807 = CARTESIAN_POINT('Ctrl Pts',(-1.49480995094287,-0.14415235976927,
6.66425846443162)) ;
#82808 = CARTESIAN_POINT('Ctrl Pts',(-1.5,-0.0720429060650724,6.66025238367027)) ;
#82809 = CARTESIAN_POINT('Ctrl Pts',(-1.5,0.,6.65624999999999)) ;
#82810 = CARTESIAN_POINT('Ctrl Pts',(-1.5,-1.21430643318376E-15,6.59374999999999)) ;
#82811 = CARTESIAN_POINT('Ctrl Pts',(-1.5,-0.111361082712955,6.59993672681737)) ;
#82812 = CARTESIAN_POINT('Ctrl Pts',(-1.48759844499926,-0.222640270679804,
6.60611890392665)) ;
#82813 = CARTESIAN_POINT('Ctrl Pts',(-1.42084385215368,-0.516992673569965,
6.62247181519833)) ;
#82814 = CARTESIAN_POINT('Ctrl Pts',(-1.34404671761395,-0.692531276762383,
6.6316548353919)) ;
#82815 = CARTESIAN_POINT('Ctrl Pts',(-1.12397619152421,-1.01303129154334,
6.65114576170348)) ;
#82816 = CARTESIAN_POINT('Ctrl Pts',(-0.97992280872646,-1.15294615050247,
6.66196305717479)) ;
#82817 = CARTESIAN_POINT('Ctrl Pts',(-0.649697411365527,-1.36585525071345,
6.68376517568562)) ;
#82818 = CARTESIAN_POINT('Ctrl Pts',(-0.467696385807258,-1.4383808020701,
6.69453630275932)) ;
#82819 = CARTESIAN_POINT('Ctrl Pts',(-0.0882190491870855,-1.509663036695,
6.71477397670299)) ;
#82820 = CARTESIAN_POINT('Ctrl Pts',(0.105509085441113,-1.5085533975611,6.72358871386342)) ;
#82821 = CARTESIAN_POINT('Ctrl Pts',(0.489353528451194,-1.43188764015323,
6.74418604261076)) ;
#82822 = CARTESIAN_POINT('Ctrl Pts',(0.67515914264358,-1.35422220285163,6.75528299265005)) ;
#82823 = CARTESIAN_POINT('Ctrl Pts',(0.999244984673385,-1.13504027758486,
6.77696396680771)) ;
#82824 = CARTESIAN_POINT('Ctrl Pts',(1.13610075771986,-0.998049285255926,
6.78735374860089)) ;
#82825 = CARTESIAN_POINT('Ctrl Pts',(1.35411996744601,-0.674923104365787,
6.8068189299665)) ;
#82826 = CARTESIAN_POINT('Ctrl Pts',(1.43126335112967,-0.490580595220442,
6.81649552248775)) ;
#82827 = CARTESIAN_POINT('Ctrl Pts',(1.5093267236132,-0.103499418996943,6.83800003227795)) ;
#82828 = CARTESIAN_POINT('Ctrl Pts',(1.50986472630013,0.0953286944885322,
6.84904603858269)) ;
#82829 = CARTESIAN_POINT('Ctrl Pts',(1.43542715550702,0.47502528955843,6.87014029386435)) ;
#82830 = CARTESIAN_POINT('Ctrl Pts',(1.36379416565911,0.65279156298978,6.87960085491672)) ;
#82831 = CARTESIAN_POINT('Ctrl Pts',(1.15321846841009,0.97960764740451,6.89881040744143)) ;
#82832 = CARTESIAN_POINT('Ctrl Pts',(1.01335589122013,1.1236681895384,6.90954123054988)) ;
#82833 = CARTESIAN_POINT('Ctrl Pts',(0.68910323787394,1.34648368114626,6.93133116281912)) ;
#82834 = CARTESIAN_POINT('Ctrl Pts',(0.508751931396615,1.42445173175803,6.9421740982814)) ;
#82835 = CARTESIAN_POINT('Ctrl Pts',(0.131741837294639,1.50638091622421,6.96258881557077)) ;
#82836 = CARTESIAN_POINT('Ctrl Pts',(-0.0610573145705921,1.51089691893831,
6.97138492922422)) ;
#82837 = CARTESIAN_POINT('Ctrl Pts',(-0.446777479089504,1.44582129502042,
6.99175055551223)) ;
#82838 = CARTESIAN_POINT('Ctrl Pts',(-0.63536076460844,1.37343070700381,7.00283462273427)) ;
#82839 = CARTESIAN_POINT('Ctrl Pts',(-0.966577871508148,1.16307287847368,
7.02461358623473)) ;
#82840 = CARTESIAN_POINT('Ctrl Pts',(-1.10764838590662,1.02963334093072,7.03510749834392)) ;
#82841 = CARTESIAN_POINT('Ctrl Pts',(-1.33383010390516,0.713695777908442,
7.05476571474223)) ;
#82842 = CARTESIAN_POINT('Ctrl Pts',(-1.41561801260082,0.533388227676851,
7.06411732068462)) ;
#82843 = CARTESIAN_POINT('Ctrl Pts',(-1.48677251611317,0.22991157572445,7.08097713468198)) ;
#82844 = CARTESIAN_POINT('Ctrl Pts',(-1.5,0.115009252399373,7.08736059708891)) ;
#82845 = CARTESIAN_POINT('Ctrl Pts',(-1.5,1.13450915328883E-14,7.09374999999999)) ;
#82846 = CARTESIAN_POINT('Origin',(0.,0.,0.)) ;
#82847 = CARTESIAN_POINT('',(-1.5,-2.17351668110822E-15,7.65624999999999)) ;
#82848 = CARTESIAN_POINT('',(-1.5,2.87452863398429E-15,7.59374999999998)) ;
#82849 = CARTESIAN_POINT('',(-1.5,-1.83697019872103E-16,0.)) ;
#82850 = CARTESIAN_POINT('Ctrl Pts',(-1.5,-7.63278329429795E-15,7.65624999999999)) ;
#82851 = CARTESIAN_POINT('Ctrl Pts',(-1.5,0.1861458861506,7.64590856188051)) ;
#82852 = CARTESIAN_POINT('Ctrl Pts',(-1.4653476410335,0.370821775569803,7.63564879024612)) ;
#82853 = CARTESIAN_POINT('Ctrl Pts',(-1.32841052256855,0.722308822181751,
7.61612173210102)) ;
#82854 = CARTESIAN_POINT('Ctrl Pts',(-1.22588013089401,0.885226385993034,
7.60730723013069)) ;
#82855 = CARTESIAN_POINT('Ctrl Pts',(-0.962395644933833,1.16695931533222,
7.58680441218545)) ;
#82856 = CARTESIAN_POINT('Ctrl Pts',(-0.802767042430613,1.28201247368992,
7.57592835640116)) ;
#82857 = CARTESIAN_POINT('Ctrl Pts',(-0.444952562952282,1.44621235819178,
7.55415189132776)) ;
#82858 = CARTESIAN_POINT('Ctrl Pts',(-0.249569090721813,1.4923983972716,7.54346855410715)) ;
#82859 = CARTESIAN_POINT('Ctrl Pts',(0.139072625428861,1.50557896499573,7.52440389393943)) ;
#82860 = CARTESIAN_POINT('Ctrl Pts',(0.328533048250181,1.47587651637286,7.51477334957883)) ;
#82861 = CARTESIAN_POINT('Ctrl Pts',(0.693038358340403,1.3448401171827,7.49359617969286)) ;
#82862 = CARTESIAN_POINT('Ctrl Pts',(0.863667549151541,1.24216627735557,7.48253472781602)) ;
#82863 = CARTESIAN_POINT('Ctrl Pts',(1.15526329027305,0.976824102726417,7.46113470521818)) ;
#82864 = CARTESIAN_POINT('Ctrl Pts',(1.27341103702043,0.81683896816719,7.45162994267596)) ;
#82865 = CARTESIAN_POINT('Ctrl Pts',(1.43908475574544,0.464718579020663,7.43206769883448)) ;
#82866 = CARTESIAN_POINT('Ctrl Pts',(1.48671418225868,0.276748660010704,7.42162492555615)) ;
#82867 = CARTESIAN_POINT('Ctrl Pts',(1.50890089335789,-0.114429023727044,
7.39989283201516)) ;
#82868 = CARTESIAN_POINT('Ctrl Pts',(1.48028463544928,-0.314079750787138,
7.38880112495627)) ;
#82869 = CARTESIAN_POINT('Ctrl Pts',(1.34926843422165,-0.682763372048332,
7.36831870155287)) ;
#82870 = CARTESIAN_POINT('Ctrl Pts',(1.25116644086583,-0.849278719452466,
7.35952236457923)) ;
#82871 = CARTESIAN_POINT('Ctrl Pts',(0.995713855764172,-1.13856859594314,
7.33919606644558)) ;
#82872 = CARTESIAN_POINT('Ctrl Pts',(0.839956299406488,-1.25787404469203,
7.32838813727827)) ;
#82873 = CARTESIAN_POINT('Ctrl Pts',(0.487639817921922,-1.43238773447714,
7.30658970016548)) ;
#82874 = CARTESIAN_POINT('Ctrl Pts',(0.293678011497376,-1.48435269459901,
7.29581423728834)) ;
#82875 = CARTESIAN_POINT('Ctrl Pts',(-0.0942923383214878,-1.50902769141779,
7.27646258855124)) ;
#82876 = CARTESIAN_POINT('Ctrl Pts',(-0.284378782084336,-1.48499391784799,
7.26715098385231)) ;
#82877 = CARTESIAN_POINT('Ctrl Pts',(-0.651911110962182,-1.36516501901101,
7.24613949591127)) ;
#82878 = CARTESIAN_POINT('Ctrl Pts',(-0.825058919774653,-1.26804586784891,
7.23511116387671)) ;
#82879 = CARTESIAN_POINT('Ctrl Pts',(-1.12574676982119,-1.01106851517849,
7.21350605314977)) ;
#82880 = CARTESIAN_POINT('Ctrl Pts',(-1.24971616502101,-0.853080854350677,
7.20364338079726)) ;
#82881 = CARTESIAN_POINT('Ctrl Pts',(-1.42557846088632,-0.504435403451394,
7.18427418908063)) ;
#82882 = CARTESIAN_POINT('Ctrl Pts',(-1.47828940988115,-0.318383776178807,
7.17393798756549)) ;
#82883 = CARTESIAN_POINT('Ctrl Pts',(-1.49819523775879,-0.0850159091993737,
7.16097310606663)) ;
#82884 = CARTESIAN_POINT('Ctrl Pts',(-1.5,-0.0424829919454561,7.15861016621918)) ;
#82885 = CARTESIAN_POINT('Ctrl Pts',(-1.5,-9.66814085323954E-15,7.15624999999999)) ;
#82886 = CARTESIAN_POINT('Ctrl Pts',(-1.5,1.00028780763944E-14,7.09374999999999)) ;
#82887 = CARTESIAN_POINT('Ctrl Pts',(-1.5,-0.0815960447684402,7.09828311359823)) ;
#82888 = CARTESIAN_POINT('Ctrl Pts',(-1.49334221031576,-0.163245912606358,
7.10281921736702)) ;
#82889 = CARTESIAN_POINT('Ctrl Pts',(-1.44902861703293,-0.431890594248862,
7.11774392190272)) ;
#82890 = CARTESIAN_POINT('Ctrl Pts',(-1.382619826531,-0.611989318737896,7.12756170921206)) ;
#82891 = CARTESIAN_POINT('Ctrl Pts',(-1.18167785850058,-0.945075901262501,
7.14648193922668)) ;
#82892 = CARTESIAN_POINT('Ctrl Pts',(-1.0461622008619,-1.09318335400795,7.15711603525437)) ;
#82893 = CARTESIAN_POINT('Ctrl Pts',(-0.728231481697741,-1.32581226318711,
7.17887439825599)) ;
#82894 = CARTESIAN_POINT('Ctrl Pts',(-0.5497048048325,-1.4092307172552,7.18978094628113)) ;
#82895 = CARTESIAN_POINT('Ctrl Pts',(-0.175257719464432,-1.50186036307312,
7.21036958579283)) ;
#82896 = CARTESIAN_POINT('Ctrl Pts',(0.0166800168265415,-1.51195786524259,
7.21922035476033)) ;
#82897 = CARTESIAN_POINT('Ctrl Pts',(0.404133880099292,-1.45839867267581,
7.23934949279767)) ;
#82898 = CARTESIAN_POINT('Ctrl Pts',(0.595331248838867,-1.39133561973484,
7.25041134307188)) ;
#82899 = CARTESIAN_POINT('Ctrl Pts',(0.93339288951111,-1.18995502000163,7.27227024689042)) ;
#82900 = CARTESIAN_POINT('Ctrl Pts',(1.07855535558916,-1.0601651251158,7.2828596541539)) ;
#82901 = CARTESIAN_POINT('Ctrl Pts',(1.31274322598517,-0.751379456456309,
7.30270440300672)) ;
#82902 = CARTESIAN_POINT('Ctrl Pts',(1.39903638673437,-0.574952294707854,
7.31180820584957)) ;
#82903 = CARTESIAN_POINT('Ctrl Pts',(1.50034365131131,-0.195507154400685,
7.33288849142218)) ;
#82904 = CARTESIAN_POINT('Ctrl Pts',(1.51302058012752,0.00414932182816016,
7.34398051787934)) ;
#82905 = CARTESIAN_POINT('Ctrl Pts',(1.46105430473585,0.389466756601615,7.36538704203342)) ;
#82906 = CARTESIAN_POINT('Ctrl Pts',(1.39975717137317,0.571898589845439,7.3755221438803)) ;
#82907 = CARTESIAN_POINT('Ctrl Pts',(1.20814359709347,0.910975961757015,7.39435977565317)) ;
#82908 = CARTESIAN_POINT('Ctrl Pts',(1.07693060012791,1.06290383237179,7.40479459213124)) ;
#82909 = CARTESIAN_POINT('Ctrl Pts',(0.76524656804414,1.30487847604685,7.42651201499658)) ;
#82910 = CARTESIAN_POINT('Ctrl Pts',(0.588625691888289,1.39349738551153,7.43747132723668)) ;
#82911 = CARTESIAN_POINT('Ctrl Pts',(0.21671876678619,1.49639045746761,7.45822284840112)) ;
#82912 = CARTESIAN_POINT('Ctrl Pts',(0.0255363238703203,1.51178362234739,
7.46719406020196)) ;
#82913 = CARTESIAN_POINT('Ctrl Pts',(-0.361165341329922,1.46939576911905,
7.48697669311104)) ;
#82914 = CARTESIAN_POINT('Ctrl Pts',(-0.552591732084792,1.40861203393721,
7.49787513671878)) ;
#82915 = CARTESIAN_POINT('Ctrl Pts',(-0.895851526154825,1.21856151679165,
7.51966941229296)) ;
#82916 = CARTESIAN_POINT('Ctrl Pts',(-1.04542819758655,1.0929484300856,7.5303551756611)) ;
#82917 = CARTESIAN_POINT('Ctrl Pts',(-1.28836769275067,0.792097162750906,
7.5504005872201)) ;
#82918 = CARTESIAN_POINT('Ctrl Pts',(-1.37954201897998,0.619819417571374,
7.5593155879127)) ;
#82919 = CARTESIAN_POINT('Ctrl Pts',(-1.47836564920042,0.293655230972509,
7.57743582050153)) ;
#82920 = CARTESIAN_POINT('Ctrl Pts',(-1.5,0.147080497195422,7.5855788612669)) ;
#82921 = CARTESIAN_POINT('Ctrl Pts',(-1.5,1.02348685082632E-14,7.59374999999998)) ;
#82922 = CARTESIAN_POINT('Origin',(0.,0.,0.)) ;
#82923 = CARTESIAN_POINT('',(-1.17524047358084,1.05150989506409E-10,0.406249999985091)) ;
#82924 = CARTESIAN_POINT('',(-1.17524047358084,2.87273037626067E-15,0.343750000000002)) ;
#82925 = CARTESIAN_POINT('',(-1.17524047358084,-1.4392544841992E-16,0.)) ;
#82926 = CARTESIAN_POINT('',(-0.45578786625158,-1.08325786021627,0.)) ;
#82927 = CARTESIAN_POINT('Ctrl Pts',(-1.17524047358084,2.10302814174179E-10,
0.406249999985091)) ;
#82928 = CARTESIAN_POINT('Ctrl Pts',(-1.17524047358083,3.33428712385673E-5,
0.406247635741228)) ;
#82929 = CARTESIAN_POINT('Ctrl Pts',(-1.17524047216194,6.66856023358135E-5,
0.406245271492423)) ;
#82930 = CARTESIAN_POINT('Ctrl Pts',(-1.17522757665485,0.151576869489721,
0.395502067066514)) ;
#82931 = CARTESIAN_POINT('Ctrl Pts',(-1.145929008722,0.301658245186112,0.38486017582027)) ;
#82932 = CARTESIAN_POINT('Ctrl Pts',(-1.03172938875857,0.582968732539079,
0.364913159750174)) ;
#82933 = CARTESIAN_POINT('Ctrl Pts',(-0.947742468184635,0.711412293797784,
0.355893102642213)) ;
#82934 = CARTESIAN_POINT('Ctrl Pts',(-0.732986343659152,0.931732084592661,
0.334894268679289)) ;
#82935 = CARTESIAN_POINT('Ctrl Pts',(-0.603354347417427,1.0204657587481,0.323787928991981)) ;
#82936 = CARTESIAN_POINT('Ctrl Pts',(-0.322468561346593,1.14000796889925,
0.302301168183816)) ;
#82937 = CARTESIAN_POINT('Ctrl Pts',(-0.174733803845013,1.17179163907959,
0.292102270501326)) ;
#82938 = CARTESIAN_POINT('Ctrl Pts',(0.130808108867636,1.17828656423486,0.273109383022199)) ;
#82939 = CARTESIAN_POINT('Ctrl Pts',(0.285781753044923,1.15058516116786,0.262826684366474)) ;
#82940 = CARTESIAN_POINT('Ctrl Pts',(0.573856810241372,1.03705912960264,0.241111743155458)) ;
#82941 = CARTESIAN_POINT('Ctrl Pts',(0.704399560267853,0.953220128037648,
0.230123010631557)) ;
#82942 = CARTESIAN_POINT('Ctrl Pts',(0.922471833417844,0.743267926701739,
0.209288109485642)) ;
#82943 = CARTESIAN_POINT('Ctrl Pts',(1.00916274464,0.620467650978295,0.200245793834457)) ;
#82944 = CARTESIAN_POINT('Ctrl Pts',(1.13495314535437,0.342640116918902,0.180545745184494)) ;
#82945 = CARTESIAN_POINT('Ctrl Pts',(1.17034734576148,0.18917786967726,0.16966412487703)) ;
#82946 = CARTESIAN_POINT('Ctrl Pts',(1.17907453998758,-0.118511772839143,
0.147846629547835)) ;
#82947 = CARTESIAN_POINT('Ctrl Pts',(1.15390583968203,-0.269771473464922,
0.137121186257288)) ;
#82948 = CARTESIAN_POINT('Ctrl Pts',(1.04763953904311,-0.553611342601334,
0.116994818114125)) ;
#82949 = CARTESIAN_POINT('Ctrl Pts',(0.967863217709318,-0.683576658879517,
0.108115548345547)) ;
#82950 = CARTESIAN_POINT('Ctrl Pts',(0.760092353676459,-0.909832915906859,
0.0873351930678865)) ;
#82951 = CARTESIAN_POINT('Ctrl Pts',(0.632728327525695,-1.00258751053419,
0.0762255674912086)) ;
#82952 = CARTESIAN_POINT('Ctrl Pts',(0.354593874883976,-1.13048305812118,
0.0546116026402439)) ;
#82953 = CARTESIAN_POINT('Ctrl Pts',(0.20739856690986,-1.16650602409258,0.0442955324203148)) ;
#82954 = CARTESIAN_POINT('Ctrl Pts',(-0.0285609865855068,-1.1780396392425,
0.0293968953689426)) ;
#82955 = CARTESIAN_POINT('Ctrl Pts',(-0.114694549034007,-1.17279463536867,
0.0241201604405704)) ;
#82956 = CARTESIAN_POINT('Ctrl Pts',(-0.287536914348188,-1.14301640971954,
0.0124505634703877)) ;
#82957 = CARTESIAN_POINT('Ctrl Pts',(-0.373501658918062,-1.11788032291883,
0.00628050026599479)) ;
#82958 = CARTESIAN_POINT('Ctrl Pts',(-0.455787866252675,-1.08325786021582,
-8.27188350007229E-14)) ;
#82959 = CARTESIAN_POINT('',(0.455787866251495,-1.08325786021631,0.)) ;
#82960 = CARTESIAN_POINT('Origin',(0.,0.,1.91347191551875E-17)) ;
#82961 = CARTESIAN_POINT('',(0.,1.17524047358084,0.218750000000004)) ;
#82962 = CARTESIAN_POINT('Ctrl Pts',(0.455787866251497,-1.08325786021631,
8.88950230295211E-16)) ;
#82963 = CARTESIAN_POINT('Ctrl Pts',(0.555456626337732,-1.04132157416659,
0.00760722476484358)) ;
#82964 = CARTESIAN_POINT('Ctrl Pts',(0.648808587897722,-0.985853182093984,
0.0153063133539367)) ;
#82965 = CARTESIAN_POINT('Ctrl Pts',(0.73322905633996,-0.918458121899505,
0.0228797846822488)) ;
#82966 = CARTESIAN_POINT('Ctrl Pts',(0.742719106373334,-0.910881967620221,
0.0237311495604381)) ;
#82967 = CARTESIAN_POINT('Ctrl Pts',(0.752096210069285,-0.903155153397013,
0.0245809201248136)) ;
#82968 = CARTESIAN_POINT('Ctrl Pts',(0.761356502140137,-0.895280094380157,
0.0254287733909492)) ;
#82969 = CARTESIAN_POINT('Ctrl Pts',(0.807820971065409,-0.855766174929913,
0.0296829644505966)) ;
#82970 = CARTESIAN_POINT('Ctrl Pts',(0.851070642967234,-0.812754819245497,
0.0338637394877002)) ;
#82971 = CARTESIAN_POINT('Ctrl Pts',(0.89075805595094,-0.766642195879478,
0.0379357160198994)) ;
#82972 = CARTESIAN_POINT('Ctrl Pts',(0.916698449836841,-0.736502171037903,
0.0405972317801421)) ;
#82973 = CARTESIAN_POINT('Ctrl Pts',(0.941116361855842,-0.705036795841439,
0.0432122440934423)) ;
#82974 = CARTESIAN_POINT('Ctrl Pts',(0.963905565511381,-0.672366143942861,
0.045769972778043)) ;
#82975 = CARTESIAN_POINT('Ctrl Pts',(0.970921870664855,-0.662307553623158,
0.0465574423720755)) ;
#82976 = CARTESIAN_POINT('Ctrl Pts',(0.977783737726072,-0.652134817790821,
0.0473394751670997)) ;
#82977 = CARTESIAN_POINT('Ctrl Pts',(0.984487934328163,-0.641851756955354,
0.0481157372196471)) ;
#82978 = CARTESIAN_POINT('Ctrl Pts',(0.987004204195475,-0.637992240646428,
0.048407089775053)) ;
#82979 = CARTESIAN_POINT('Ctrl Pts',(0.989499607468229,-0.634115061770119,
0.0486977871654455)) ;
#82980 = CARTESIAN_POINT('Ctrl Pts',(0.991969521565222,-0.630227450235288,
0.0489872892015786)) ;
#82981 = CARTESIAN_POINT('Ctrl Pts',(1.00094420270959,-0.616101422945214,
0.050039223950282)) ;
#82982 = CARTESIAN_POINT('Ctrl Pts',(1.00954934528882,-0.601890188375154,
0.0510714871118151)) ;
#82983 = CARTESIAN_POINT('Ctrl Pts',(1.01778810567736,-0.587620236790823,
0.052083333332872)) ;
#82984 = CARTESIAN_POINT('Ctrl Pts',(1.03588297104925,-0.556279010610585,
0.0543056605136163)) ;
#82985 = CARTESIAN_POINT('Ctrl Pts',(1.05265649617207,-0.523875077122629,
0.0566033415851627)) ;
#82986 = CARTESIAN_POINT('Ctrl Pts',(1.06794121459765,-0.490603437521713,
0.0589625495053588)) ;
#82987 = CARTESIAN_POINT('Ctrl Pts',(1.0831560161713,-0.457483992304385,0.0613109657062566)) ;
#82988 = CARTESIAN_POINT('Ctrl Pts',(1.09689501026764,-0.423505381285014,
0.0637203031839332)) ;
#82989 = CARTESIAN_POINT('Ctrl Pts',(1.10903206965691,-0.38889335198346,0.0661745547519881)) ;
#82990 = CARTESIAN_POINT('Ctrl Pts',(1.12110084630513,-0.354476048946159,
0.0686149987725218)) ;
#82991 = CARTESIAN_POINT('Ctrl Pts',(1.13158529026317,-0.319433203135218,
0.0710997984510217)) ;
#82992 = CARTESIAN_POINT('Ctrl Pts',(1.14040729558434,-0.284009455691929,
0.0736116069021118)) ;
#82993 = CARTESIAN_POINT('Ctrl Pts',(1.14639361115526,-0.259972094209997,
0.0753160354866054)) ;
#82994 = CARTESIAN_POINT('Ctrl Pts',(1.15161504008478,-0.235761997361788,
0.0770327122995954)) ;
#82995 = CARTESIAN_POINT('Ctrl Pts',(1.15606152093929,-0.211451958013961,
0.0787564757827807)) ;
#82996 = CARTESIAN_POINT('Ctrl Pts',(1.16293619560641,-0.173866366817296,
0.0814215751136272)) ;
#82997 = CARTESIAN_POINT('Ctrl Pts',(1.16796201959779,-0.136032559741066,
0.0841042748055188)) ;
#82998 = CARTESIAN_POINT('Ctrl Pts',(1.17114009049391,-0.0980869980277225,
0.0867948987364481)) ;
#82999 = CARTESIAN_POINT('Ctrl Pts',(1.17750913668542,-0.0220417985293885,
0.0921870717433521)) ;
#83000 = CARTESIAN_POINT('Ctrl Pts',(1.1764575549977,0.0544503015484298,0.0976109333415215)) ;
#83001 = CARTESIAN_POINT('Ctrl Pts',(1.16799326335438,0.130314648071384,0.102990282520794)) ;
#83002 = CARTESIAN_POINT('Ctrl Pts',(1.1645137386421,0.161501176091812,0.105201640445828)) ;
#83003 = CARTESIAN_POINT('Ctrl Pts',(1.15978139602167,0.192581525329594,0.107405469501587)) ;
#83004 = CARTESIAN_POINT('Ctrl Pts',(1.15379723626192,0.223477310564639,0.10959621159011)) ;
#83005 = CARTESIAN_POINT('Ctrl Pts',(1.15113866660766,0.237203313941591,0.1105694878178)) ;
#83006 = CARTESIAN_POINT('Ctrl Pts',(1.14823292643457,0.250893708838873,0.111540239138144)) ;
#83007 = CARTESIAN_POINT('Ctrl Pts',(1.14507883494787,0.264546087661879,0.112508294834686)) ;
#83008 = CARTESIAN_POINT('Ctrl Pts',(1.13736632444846,0.297929429729847,0.114875423294677)) ;
#83009 = CARTESIAN_POINT('Ctrl Pts',(1.12816921570323,0.331063129141963,0.117224850224537)) ;
#83010 = CARTESIAN_POINT('Ctrl Pts',(1.11754564321342,0.363705796045817,0.119539459279577)) ;
#83011 = CARTESIAN_POINT('Ctrl Pts',(1.10685168558726,0.396564732812124,0.121869403484268)) ;
#83012 = CARTESIAN_POINT('Ctrl Pts',(1.09471263728511,0.428925268436663,0.124164007322948)) ;
#83013 = CARTESIAN_POINT('Ctrl Pts',(1.08123676383361,0.460561864766466,0.126407278454903)) ;
#83014 = CARTESIAN_POINT('Ctrl Pts',(1.06776089038211,0.492198461096268,0.128650549586858)) ;
#83015 = CARTESIAN_POINT('Ctrl Pts',(1.05294880728718,0.523110465237353,0.13084244171702)) ;
#83016 = CARTESIAN_POINT('Ctrl Pts',(1.03695027890869,0.553104230515107,0.132969223848851)) ;
#83017 = CARTESIAN_POINT('Ctrl Pts',(1.03073801379148,0.564750878091717,0.133795058209168)) ;
#83018 = CARTESIAN_POINT('Ctrl Pts',(1.0243472497762,0.576259465955854,0.13461110310401)) ;
#83019 = CARTESIAN_POINT('Ctrl Pts',(1.01778810567666,0.58762023679042,0.135416666666671)) ;
#83020 = CARTESIAN_POINT('Ctrl Pts',(1.01147691905926,0.598551532667805,0.136191777244968)) ;
#83021 = CARTESIAN_POINT('Ctrl Pts',(1.00495532187839,0.609440442024016,0.136978305885939)) ;
#83022 = CARTESIAN_POINT('Ctrl Pts',(0.998223622886107,0.620273947102929,
0.137775772101735)) ;
#83023 = CARTESIAN_POINT('Ctrl Pts',(0.994230328960125,0.626700462916888,
0.138248834994084)) ;
#83024 = CARTESIAN_POINT('Ctrl Pts',(0.990163120027323,0.633107478035257,
0.138725745462529)) ;
#83025 = CARTESIAN_POINT('Ctrl Pts',(0.986022228864173,0.639492247746788,
0.139206391902537)) ;
#83026 = CARTESIAN_POINT('Ctrl Pts',(0.982391378490878,0.645090594232399,
0.139627836281867)) ;
#83027 = CARTESIAN_POINT('Ctrl Pts',(0.978701509136287,0.650675207237517,
0.140052417976343)) ;
#83028 = CARTESIAN_POINT('Ctrl Pts',(0.974968401333292,0.65622159911429,0.140478299761523)) ;
#83029 = CARTESIAN_POINT('Ctrl Pts',(0.94517954247386,0.700479813319558,0.143876683376199)) ;
#83030 = CARTESIAN_POINT('Ctrl Pts',(0.912465254098321,0.742576356849108,
0.147378071508724)) ;
#83031 = CARTESIAN_POINT('Ctrl Pts',(0.877105627658379,0.782224960399829,
0.150955115078013)) ;
#83032 = CARTESIAN_POINT('Ctrl Pts',(0.831750620023092,0.833081343733677,
0.155543309432169)) ;
#83033 = CARTESIAN_POINT('Ctrl Pts',(0.782044785587662,0.879913760162883,
0.160256013274919)) ;
#83034 = CARTESIAN_POINT('Ctrl Pts',(0.728524264359262,0.92219443014058,0.165041591738334)) ;
#83035 = CARTESIAN_POINT('Ctrl Pts',(0.706132108701109,0.939884006432844,
0.167043803514445)) ;
#83036 = CARTESIAN_POINT('Ctrl Pts',(0.683071546470738,0.95677716846021,0.169058824721421)) ;
#83037 = CARTESIAN_POINT('Ctrl Pts',(0.659380441035754,0.972834829106157,
0.171082944473584)) ;
#83038 = CARTESIAN_POINT('Ctrl Pts',(0.649585211206294,0.979473965341576,
0.171919828941859)) ;
#83039 = CARTESIAN_POINT('Ctrl Pts',(0.639687548158731,0.985966464245742,
0.1727578047544)) ;
#83040 = CARTESIAN_POINT('Ctrl Pts',(0.629702276471932,0.992302984853204,
0.173595630396174)) ;
#83041 = CARTESIAN_POINT('Ctrl Pts',(0.557229399416611,1.03829330873695,0.17967655003808)) ;
#83042 = CARTESIAN_POINT('Ctrl Pts',(0.479966401464458,1.07618734135146,0.185764576080157)) ;
#83043 = CARTESIAN_POINT('Ctrl Pts',(0.399297087258105,1.10532891342338,0.191751468645449)) ;
#83044 = CARTESIAN_POINT('Ctrl Pts',(0.390512697340452,1.10850225057657,0.192403404256976)) ;
#83045 = CARTESIAN_POINT('Ctrl Pts',(0.381687975012754,1.11157177312558,0.19305413597231)) ;
#83046 = CARTESIAN_POINT('Ctrl Pts',(0.372824787348853,1.11453660715151,0.193703518155098)) ;
#83047 = CARTESIAN_POINT('Ctrl Pts',(0.360834972624344,1.11854733241287,0.194581979985341)) ;
#83048 = CARTESIAN_POINT('Ctrl Pts',(0.34877476153917,1.12236648064852,0.19545797257085)) ;
#83049 = CARTESIAN_POINT('Ctrl Pts',(0.336648882234719,1.12599187423029,0.196331128362409)) ;
#83050 = CARTESIAN_POINT('Ctrl Pts',(0.326768217427892,1.12894599391718,0.19704261158634)) ;
#83051 = CARTESIAN_POINT('Ctrl Pts',(0.316853206965907,1.13176869706379,0.197751544689599)) ;
#83052 = CARTESIAN_POINT('Ctrl Pts',(0.306906979259801,1.1344594646016,0.198457717160829)) ;
#83053 = CARTESIAN_POINT('Ctrl Pts',(0.253270239805225,1.14896989022454,0.202265873375283)) ;
#83054 = CARTESIAN_POINT('Ctrl Pts',(0.198716886494649,1.15964686582265,0.205994406585413)) ;
#83055 = CARTESIAN_POINT('Ctrl Pts',(0.143643430230035,1.16642905300505,0.209616793303918)) ;
#83056 = CARTESIAN_POINT('Ctrl Pts',(0.0960555021956946,1.17228941219517,
0.212746828899368)) ;
#83057 = CARTESIAN_POINT('Ctrl Pts',(0.0480783523083568,1.17524047358084,
0.215797620224182)) ;
#83058 = CARTESIAN_POINT('Ctrl Pts',(-5.2787093272888E-18,1.17524047358084,
0.218750000000004)) ;
#83059 = CARTESIAN_POINT('Ctrl Pts',(1.69773917146898E-12,1.17524047358084,
0.218749999999899)) ;
#83060 = CARTESIAN_POINT('Ctrl Pts',(-0.126600692090499,1.17524047358102,
0.226524254003875)) ;
#83061 = CARTESIAN_POINT('Ctrl Pts',(-0.252329587007292,1.15478626807222,
0.234970150993983)) ;
#83062 = CARTESIAN_POINT('Ctrl Pts',(-0.4964174014379,1.07325253106312,0.252849691552136)) ;
#83063 = CARTESIAN_POINT('Ctrl Pts',(-0.612698810244334,1.01138495191746,
0.262183699254262)) ;
#83064 = CARTESIAN_POINT('Ctrl Pts',(-0.84002034410012,0.836587015392715,
0.282340225925395)) ;
#83065 = CARTESIAN_POINT('Ctrl Pts',(-0.943423576788923,0.717916941119984,
0.292844323157757)) ;
#83066 = CARTESIAN_POINT('Ctrl Pts',(-1.09478665341015,0.45276593025062,0.311645511569115)) ;
#83067 = CARTESIAN_POINT('Ctrl Pts',(-1.14343934987247,0.309962728219041,
0.321771325905397)) ;
#83068 = CARTESIAN_POINT('Ctrl Pts',(-1.17151191967199,0.10815275245462,0.336081161516424)) ;
#83069 = CARTESIAN_POINT('Ctrl Pts',(-1.17524047358084,0.0540497505340984,
0.339917468718878)) ;
#83070 = CARTESIAN_POINT('Ctrl Pts',(-1.17524047358084,5.94966725733499E-15,
0.343750000000002)) ;
#83071 = CARTESIAN_POINT('Origin',(0.,0.,0.)) ;
#83072 = CARTESIAN_POINT('',(-1.17524047358084,1.36204092907257E-16,0.906250000000002)) ;
#83073 = CARTESIAN_POINT('',(-1.17524047358084,-1.69338707316203E-15,0.843750000000002)) ;
#83074 = CARTESIAN_POINT('',(-1.17524047358084,-1.4392544841992E-16,0.)) ;
#83075 = CARTESIAN_POINT('Ctrl Pts',(-1.17524047358084,1.04119177003363E-15,
0.906250000000002)) ;
#83076 = CARTESIAN_POINT('Ctrl Pts',(-1.17524047358084,0.0202793012904351,
0.904812045970855)) ;
#83077 = CARTESIAN_POINT('Ctrl Pts',(-1.17471558743293,0.0405774738555247,
0.903372753827319)) ;
#83078 = CARTESIAN_POINT('Ctrl Pts',(-1.16585586118875,0.211393740268767,
0.891260603856515)) ;
#83079 = CARTESIAN_POINT('Ctrl Pts',(-1.12916400813093,0.359047310690368,
0.880790862149689)) ;
#83080 = CARTESIAN_POINT('Ctrl Pts',(-1.00050354246883,0.635582556545377,
0.861182446391989)) ;
#83081 = CARTESIAN_POINT('Ctrl Pts',(-0.908572250758423,0.761238895462286,
0.85172121147626)) ;
#83082 = CARTESIAN_POINT('Ctrl Pts',(-0.680988460715921,0.970251111909413,
0.830335556180614)) ;
#83083 = CARTESIAN_POINT('Ctrl Pts',(-0.547470900446216,1.05138296722918,
0.819260125930664)) ;
#83084 = CARTESIAN_POINT('Ctrl Pts',(-0.261932318018029,1.15534724208175,
0.798039943742627)) ;
#83085 = CARTESIAN_POINT('Ctrl Pts',(-0.11341618306421,1.17920917547203,0.788355329287387)) ;
#83086 = CARTESIAN_POINT('Ctrl Pts',(0.19139296078578,1.16998813394558,0.769310788426688)) ;
#83087 = CARTESIAN_POINT('Ctrl Pts',(0.344719843502962,1.13430450684253,0.758630223295995)) ;
#83088 = CARTESIAN_POINT('Ctrl Pts',(0.6257620144399,1.00647439980544,0.736840022340475)) ;
#83089 = CARTESIAN_POINT('Ctrl Pts',(0.751272026900972,0.916606473578397,
0.725946590613973)) ;
#83090 = CARTESIAN_POINT('Ctrl Pts',(0.958534826557889,0.696258186516551,
0.705406894001169)) ;
#83091 = CARTESIAN_POINT('Ctrl Pts',(1.03925302012441,0.568782956917435,0.696580962733728)) ;
#83092 = CARTESIAN_POINT('Ctrl Pts',(1.15135135229401,0.283314574452573,0.676339120824057)) ;
#83093 = CARTESIAN_POINT('Ctrl Pts',(1.17886389517849,0.127048431846906,0.665258683378948)) ;
#83094 = CARTESIAN_POINT('Ctrl Pts',(1.17100472484766,-0.181027472991394,
0.643413799164202)) ;
#83095 = CARTESIAN_POINT('Ctrl Pts',(1.13805352029235,-0.329961447770428,
0.632853267218683)) ;
#83096 = CARTESIAN_POINT('Ctrl Pts',(1.01675529018029,-0.608954557836807,
0.6130705705183)) ;
#83097 = CARTESIAN_POINT('Ctrl Pts',(0.928913126162766,-0.736034408769977,
0.603863890560589)) ;
#83098 = CARTESIAN_POINT('Ctrl Pts',(0.707873747457054,-0.950883999345414,
0.582673155614445)) ;
#83099 = CARTESIAN_POINT('Ctrl Pts',(0.576292200247247,-1.03592879950197,
0.571577882905812)) ;
#83100 = CARTESIAN_POINT('Ctrl Pts',(0.292999335820162,-1.14790387139071,
0.550211592344942)) ;
#83101 = CARTESIAN_POINT('Ctrl Pts',(0.144866780735161,-1.17579331214599,
0.540165532210261)) ;
#83102 = CARTESIAN_POINT('Ctrl Pts',(-0.160315813799847,-1.17464616911588,
0.521384308485598)) ;
#83103 = CARTESIAN_POINT('Ctrl Pts',(-0.3145033932383,-1.14304656608018,0.510795683886598)) ;
#83104 = CARTESIAN_POINT('Ctrl Pts',(-0.599172761887689,-1.0225856529898,
0.48904401062123)) ;
#83105 = CARTESIAN_POINT('Ctrl Pts',(-0.72731437612933,-0.935793429643947,
0.478098023512044)) ;
#83106 = CARTESIAN_POINT('Ctrl Pts',(-0.940171384116082,-0.72078997858306,
0.457404293988808)) ;
#83107 = CARTESIAN_POINT('Ctrl Pts',(-1.02397644071054,-0.595756300398089,
0.448493574385486)) ;
#83108 = CARTESIAN_POINT('Ctrl Pts',(-1.14360031635853,-0.31333144758319,
0.428467541475363)) ;
#83109 = CARTESIAN_POINT('Ctrl Pts',(-1.17524047360901,-0.157447947684027,
0.417414236257988)) ;
#83110 = CARTESIAN_POINT('Ctrl Pts',(-1.17524047358084,2.10302920911065E-10,
0.406249999985091)) ;
#83111 = CARTESIAN_POINT('Ctrl Pts',(-1.17524047358084,5.96744875736022E-15,
0.343750000000002)) ;
#83112 = CARTESIAN_POINT('Ctrl Pts',(-1.17524047358084,-0.10056073900197,
0.350880507986989)) ;
#83113 = CARTESIAN_POINT('Ctrl Pts',(-1.16233296013586,-0.200937146127487,
0.357997945466203)) ;
#83114 = CARTESIAN_POINT('Ctrl Pts',(-1.09785564047115,-0.446351823951105,
0.375399680355109)) ;
#83115 = CARTESIAN_POINT('Ctrl Pts',(-1.03064731215459,-0.585043083983595,
0.384535643011968)) ;
#83116 = CARTESIAN_POINT('Ctrl Pts',(-0.84776435181588,-0.827873160197687,
0.404375293844389)) ;
#83117 = CARTESIAN_POINT('Ctrl Pts',(-0.734282924849944,-0.929994728118301,
0.414964515506367)) ;
#83118 = CARTESIAN_POINT('Ctrl Pts',(-0.469784373122341,-1.08867274565634,
0.436832484995882)) ;
#83119 = CARTESIAN_POINT('Ctrl Pts',(-0.320081111277505,-1.14169623565684,
0.447905294936889)) ;
#83120 = CARTESIAN_POINT('Ctrl Pts',(-0.0164013647280398,-1.18458870108195,
0.468074259944006)) ;
#83121 = CARTESIAN_POINT('Ctrl Pts',(0.134153473501831,-1.17708405685267,
0.476922690824644)) ;
#83122 = CARTESIAN_POINT('Ctrl Pts',(0.427990911138155,-1.10518837239671,
0.497515535036282)) ;
#83123 = CARTESIAN_POINT('Ctrl Pts',(0.568123902524849,-1.04011790080108,
0.508427767447896)) ;
#83124 = CARTESIAN_POINT('Ctrl Pts',(0.817806327670518,-0.858293519786357,
0.530206538152454)) ;
#83125 = CARTESIAN_POINT('Ctrl Pts',(0.924317628413691,-0.742386396552834,
0.540856490029454)) ;
#83126 = CARTESIAN_POINT('Ctrl Pts',(1.0823830905674,-0.481525143101595,0.559811428644212)) ;
#83127 = CARTESIAN_POINT('Ctrl Pts',(1.13471881974578,-0.340406375375874,
0.569612643785922)) ;
#83128 = CARTESIAN_POINT('Ctrl Pts',(1.18471102264315,-0.0404316039914042,
0.590883097090857)) ;
#83129 = CARTESIAN_POINT('Ctrl Pts',(1.17972508402808,0.115872602932994,0.601966233580656)) ;
#83130 = CARTESIAN_POINT('Ctrl Pts',(1.10966180879066,0.416545840309742,0.623286213344783)) ;
#83131 = CARTESIAN_POINT('Ctrl Pts',(1.04568659395149,0.558019808731794,0.632654039607303)) ;
#83132 = CARTESIAN_POINT('Ctrl Pts',(0.868552388088852,0.805966324916247,
0.652322069717154)) ;
#83133 = CARTESIAN_POINT('Ctrl Pts',(0.758009163999587,0.910696733028636,
0.662823356309342)) ;
#83134 = CARTESIAN_POINT('Ctrl Pts',(0.498423053649437,1.0758012021434,0.684617505925215)) ;
#83135 = CARTESIAN_POINT('Ctrl Pts',(0.350593694266161,1.13263935614624,0.69571048796941)) ;
#83136 = CARTESIAN_POINT('Ctrl Pts',(0.0481602798510692,1.18378120089601,
0.716095389944385)) ;
#83137 = CARTESIAN_POINT('Ctrl Pts',(-0.103009693180801,1.18027462929666,
0.724897106005194)) ;
#83138 = CARTESIAN_POINT('Ctrl Pts',(-0.39867718968897,1.11604386548558,0.745330579794386)) ;
#83139 = CARTESIAN_POINT('Ctrl Pts',(-0.540113184163221,1.05487699393238,
0.7561844293853)) ;
#83140 = CARTESIAN_POINT('Ctrl Pts',(-0.794319299722647,0.880080649233699,
0.777991819243996)) ;
#83141 = CARTESIAN_POINT('Ctrl Pts',(-0.903942617574611,0.767070080997107,
0.788730179153422)) ;
#83142 = CARTESIAN_POINT('Ctrl Pts',(-1.06890822958908,0.510689481693172,
0.807949983986318)) ;
#83143 = CARTESIAN_POINT('Ctrl Pts',(-1.12497808721731,0.37124377155117,0.817426041918157)) ;
#83144 = CARTESIAN_POINT('Ctrl Pts',(-1.16799649676227,0.150680192339373,
0.833065648178182)) ;
#83145 = CARTESIAN_POINT('Ctrl Pts',(-1.17524047358084,0.0753367271238741,
0.838408062979634)) ;
#83146 = CARTESIAN_POINT('Ctrl Pts',(-1.17524047358084,-3.71854203583437E-15,
0.843750000000002)) ;
#83147 = CARTESIAN_POINT('Origin',(0.,0.,0.)) ;
#83148 = CARTESIAN_POINT('',(-1.17524047358084,1.0382603004152E-15,1.40625)) ;
#83149 = CARTESIAN_POINT('',(-1.17524047358084,7.52030926879024E-16,1.34375)) ;
#83150 = CARTESIAN_POINT('',(-1.17524047358084,-1.4392544841992E-16,0.)) ;
#83151 = CARTESIAN_POINT('Ctrl Pts',(-1.17524047358084,1.93364185863387E-15,
1.40625)) ;
#83152 = CARTESIAN_POINT('Ctrl Pts',(-1.17524047358084,0.04022257400546,1.40339791887918)) ;
#83153 = CARTESIAN_POINT('Ctrl Pts',(-1.17317560429429,0.0804927572900409,
1.40054246190466)) ;
#83154 = CARTESIAN_POINT('Ctrl Pts',(-1.15363384185356,0.269838964882093,
1.38711640061135)) ;
#83155 = CARTESIAN_POINT('Ctrl Pts',(-1.10981617409642,0.414746302173939,
1.3768413873588)) ;
#83156 = CARTESIAN_POINT('Ctrl Pts',(-0.966822628308877,0.686334315935149,
1.35758376733219)) ;
#83157 = CARTESIAN_POINT('Ctrl Pts',(-0.866656139323778,0.809163180776926,
1.34744814557029)) ;
#83158 = CARTESIAN_POINT('Ctrl Pts',(-0.626271893489302,1.00630816652666,
1.32569718173687)) ;
#83159 = CARTESIAN_POINT('Ctrl Pts',(-0.489259202086931,1.0795836502592,1.31468566134647)) ;
#83160 = CARTESIAN_POINT('Ctrl Pts',(-0.199493226876555,1.16772697093534,
1.29376679674992)) ;
#83161 = CARTESIAN_POINT('Ctrl Pts',(-0.0500767687957025,1.18357945674508,
1.28462074599962)) ;
#83162 = CARTESIAN_POINT('Ctrl Pts',(0.253749602960034,1.15807119453095,1.26505911204832)) ;
#83163 = CARTESIAN_POINT('Ctrl Pts',(0.404998008215433,1.11421428515519,1.25421640798347)) ;
#83164 = CARTESIAN_POINT('Ctrl Pts',(0.678131728877579,0.971835826442956,
1.23239605312863)) ;
#83165 = CARTESIAN_POINT('Ctrl Pts',(0.798109033041594,0.875991959562471,
1.22163050272023)) ;
#83166 = CARTESIAN_POINT('Ctrl Pts',(0.993951951775847,0.644955162106818,
1.2014131267936)) ;
#83167 = CARTESIAN_POINT('Ctrl Pts',(1.06836977023306,0.512342277031657,1.19257889669174)) ;
#83168 = CARTESIAN_POINT('Ctrl Pts',(1.16482435595196,0.22089396801138,1.17191303329527)) ;
#83169 = CARTESIAN_POINT('Ctrl Pts',(1.18383776080121,0.0642437159595267,
1.16080535961959)) ;
#83170 = CARTESIAN_POINT('Ctrl Pts',(1.15996489664612,-0.241400433726271,
1.13913290502011)) ;
#83171 = CARTESIAN_POINT('Ctrl Pts',(1.11960234743318,-0.387690749984452,
1.12875982822244)) ;
#83172 = CARTESIAN_POINT('Ctrl Pts',(0.983613341401883,-0.661723584428254,
1.10932885213684)) ;
#83173 = CARTESIAN_POINT('Ctrl Pts',(0.887517303054449,-0.785946092176641,
1.09955231366117)) ;
#83174 = CARTESIAN_POINT('Ctrl Pts',(0.65339647872034,-0.988975611380567,
1.0779773432707)) ;
#83175 = CARTESIAN_POINT('Ctrl Pts',(0.518044727734835,-1.06612844449193,
1.06693035084248)) ;
#83176 = CARTESIAN_POINT('Ctrl Pts',(0.230321117048486,-1.16204066071992,
1.04586146672072)) ;
#83177 = CARTESIAN_POINT('Ctrl Pts',(0.0813714242245326,-1.18183751648957,
1.03648071970046)) ;
#83178 = CARTESIAN_POINT('Ctrl Pts',(-0.222980227030622,-1.16438441904261,
1.01717241525019)) ;
#83179 = CARTESIAN_POINT('Ctrl Pts',(-0.375313403061051,-1.12455686395351,
1.0064059536026)) ;
#83180 = CARTESIAN_POINT('Ctrl Pts',(-0.652455471206262,-0.989317123906594,
0.98459254970711)) ;
#83181 = CARTESIAN_POINT('Ctrl Pts',(-0.775205273694797,-0.896389255418135,
0.973760129666063)) ;
#83182 = CARTESIAN_POINT('Ctrl Pts',(-0.976718230171345,-0.670624059163199,
0.953381467873824)) ;
#83183 = CARTESIAN_POINT('Ctrl Pts',(-1.05426732657947,-0.54058712396737,
0.944581667441689)) ;
#83184 = CARTESIAN_POINT('Ctrl Pts',(-1.15162322837993,-0.271198393744022,
0.925479993055387)) ;
#83185 = CARTESIAN_POINT('Ctrl Pts',(-1.17524047358084,-0.136023713315906,
0.915895097916393)) ;
#83186 = CARTESIAN_POINT('Ctrl Pts',(-1.17524047358084,8.67361737988404E-16,
0.906250000000002)) ;
#83187 = CARTESIAN_POINT('Ctrl Pts',(-1.17524047358084,-3.71854203583437E-15,
0.843750000000002)) ;
#83188 = CARTESIAN_POINT('Ctrl Pts',(-1.17524047358084,-0.078372892307368,
0.849307223824201)) ;
#83189 = CARTESIAN_POINT('Ctrl Pts',(-1.16740080636849,-0.156738492471966,
0.854863930580949)) ;
#83190 = CARTESIAN_POINT('Ctrl Pts',(-1.12085118653128,-0.385937684285252,
0.871115866317054)) ;
#83191 = CARTESIAN_POINT('Ctrl Pts',(-1.06019873478228,-0.530294701065063,
0.880779924121279)) ;
#83192 = CARTESIAN_POINT('Ctrl Pts',(-0.888915438186115,-0.783377667817373,
0.900270769870976)) ;
#83193 = CARTESIAN_POINT('Ctrl Pts',(-0.781390210104203,-0.890651624122545,
0.910676906637472)) ;
#83194 = CARTESIAN_POINT('Ctrl Pts',(-0.5269036707543,-1.06208047624785,0.932382126472764)) ;
#83195 = CARTESIAN_POINT('Ctrl Pts',(-0.381055225059466,-1.12269807590544,
0.943487460687598)) ;
#83196 = CARTESIAN_POINT('Ctrl Pts',(-0.0799626681969364,-1.18213557941063,
0.964084135823149)) ;
#83197 = CARTESIAN_POINT('Ctrl Pts',(0.071867518770716,-1.18265521488411,
0.972900336861989)) ;
#83198 = CARTESIAN_POINT('Ctrl Pts',(0.369300845634156,-1.12605315656733,
0.993171780067366)) ;
#83199 = CARTESIAN_POINT('Ctrl Pts',(0.511924838644523,-1.0687843688582,1.00396038024544)) ;
#83200 = CARTESIAN_POINT('Ctrl Pts',(0.770425194894299,-0.901076654851032,
1.02578015098746)) ;
#83201 = CARTESIAN_POINT('Ctrl Pts',(0.883058018607359,-0.791027335171729,
1.03659833032357)) ;
#83202 = CARTESIAN_POINT('Ctrl Pts',(1.05483070655924,-0.539159838753598,
1.05607613549244)) ;
#83203 = CARTESIAN_POINT('Ctrl Pts',(1.11459544966178,-0.401318682169378,
1.06529350597521)) ;
#83204 = CARTESIAN_POINT('Ctrl Pts',(1.18057883902678,-0.105594918914387,
1.0862625310317)) ;
#83205 = CARTESIAN_POINT('Ctrl Pts',(1.18424105822213,0.0498773760115757,
1.09728667874309)) ;
#83206 = CARTESIAN_POINT('Ctrl Pts',(1.13096504430472,0.355816569528943,1.11898005415539)) ;
#83207 = CARTESIAN_POINT('Ctrl Pts',(1.07359647263153,0.503036071445992,1.12899077992006)) ;
#83208 = CARTESIAN_POINT('Ctrl Pts',(0.908029028731414,0.761068349354,1.14830610002792)) ;
#83209 = CARTESIAN_POINT('Ctrl Pts',(0.803473383957124,0.870718346127371,
1.15861412110518)) ;
#83210 = CARTESIAN_POINT('Ctrl Pts',(0.55405468980877,1.04811272561393,1.18021963659358)) ;
#83211 = CARTESIAN_POINT('Ctrl Pts',(0.410207640003824,1.11232003373639,1.19132933832228)) ;
#83212 = CARTESIAN_POINT('Ctrl Pts',(0.11049155378206,1.17976547217851,1.21212539881691)) ;
#83213 = CARTESIAN_POINT('Ctrl Pts',(-0.0420042747174427,1.18418253655367,
1.2210123552515)) ;
#83214 = CARTESIAN_POINT('Ctrl Pts',(-0.341078428303618,1.13487089602653,
1.24112608525408)) ;
#83215 = CARTESIAN_POINT('Ctrl Pts',(-0.484735956272483,1.08133427966265,
1.25184583298843)) ;
#83216 = CARTESIAN_POINT('Ctrl Pts',(-0.747142454712865,0.920478081773251,
1.27366255898542)) ;
#83217 = CARTESIAN_POINT('Ctrl Pts',(-0.862566052875092,0.813327180918138,
1.28454935350987)) ;
#83218 = CARTESIAN_POINT('Ctrl Pts',(-1.04078647908616,0.565824186520556,
1.30426836137977)) ;
#83219 = CARTESIAN_POINT('Ctrl Pts',(-1.1040680687744,0.429463242089193,1.31329784632424)) ;
#83220 = CARTESIAN_POINT('Ctrl Pts',(-1.16352312203673,0.191486738352365,
1.33017215907742)) ;
#83221 = CARTESIAN_POINT('Ctrl Pts',(-1.17524047358084,0.0958129055313116,
1.33695614889143)) ;
#83222 = CARTESIAN_POINT('Ctrl Pts',(-1.17524047358084,3.04920446938418E-15,
1.34375)) ;
#83223 = CARTESIAN_POINT('Origin',(0.,0.,0.)) ;
#83224 = CARTESIAN_POINT('',(-1.17524047358084,-1.51178320927071E-15,1.90625)) ;
#83225 = CARTESIAN_POINT('',(-1.17524047358084,-3.66865715126017E-16,1.84375)) ;
#83226 = CARTESIAN_POINT('',(-1.17524047358084,-1.4392544841992E-16,0.)) ;
#83227 = CARTESIAN_POINT('Ctrl Pts',(-1.17524047358084,-1.93364185863387E-15,
1.90625)) ;
#83228 = CARTESIAN_POINT('Ctrl Pts',(-1.17524047358084,0.0620702449181597,
1.90184875572181)) ;
#83229 = CARTESIAN_POINT('Ctrl Pts',(-1.17032322149779,0.124185902335723,
1.89744429135801)) ;
#83230 = CARTESIAN_POINT('Ctrl Pts',(-1.13686603480775,0.333198273001777,
1.8826237521177)) ;
#83231 = CARTESIAN_POINT('Ctrl Pts',(-1.08539661824635,0.474712480263841,
1.87273801672552)) ;
#83232 = CARTESIAN_POINT('Ctrl Pts',(-0.928933450973058,0.736601141370628,
1.85384504587131)) ;
#83233 = CARTESIAN_POINT('Ctrl Pts',(-0.823153083206283,0.853165552137381,
1.84321667558877)) ;
#83234 = CARTESIAN_POINT('Ctrl Pts',(-0.574544799352632,1.03659861296798,
1.82144683169118)) ;
#83235 = CARTESIAN_POINT('Ctrl Pts',(-0.434728280900438,1.10256826143134,
1.81052215396611)) ;
#83236 = CARTESIAN_POINT('Ctrl Pts',(-0.141321704421145,1.17623437512204,
1.78989299960338)) ;
#83237 = CARTESIAN_POINT('Ctrl Pts',(0.00909819868139983,1.1846564506662,
1.78102513235836)) ;
#83238 = CARTESIAN_POINT('Ctrl Pts',(0.313051975628829,1.14365715711825,1.76090645979978)) ;
#83239 = CARTESIAN_POINT('Ctrl Pts',(0.463171539465951,1.0915165113851,1.7498393858503)) ;
#83240 = CARTESIAN_POINT('Ctrl Pts',(0.728774489075423,0.934331756521546,
1.72795653959804)) ;
#83241 = CARTESIAN_POINT('Ctrl Pts',(0.842920959693578,0.832819718037304,
1.71734808924873)) ;
#83242 = CARTESIAN_POINT('Ctrl Pts',(1.0271136198994,0.591165030054373,1.69746968469931)) ;
#83243 = CARTESIAN_POINT('Ctrl Pts',(1.09505484350283,0.453100495453474,1.6883782116043)) ;
#83244 = CARTESIAN_POINT('Ctrl Pts',(1.17518605745325,0.155812781552446,1.66729829075803)) ;
#83245 = CARTESIAN_POINT('Ctrl Pts',(1.18546762072542,-0.000766465150745417,
1.65619565189226)) ;
#83246 = CARTESIAN_POINT('Ctrl Pts',(1.14530292216298,-0.303048152507463,
1.63476162100299)) ;
#83247 = CARTESIAN_POINT('Ctrl Pts',(1.09748010274341,-0.446226863218259,
1.62460918029479)) ;
#83248 = CARTESIAN_POINT('Ctrl Pts',(0.947630262761121,-0.712359381071128,
1.60573839570251)) ;
#83249 = CARTESIAN_POINT('Ctrl Pts',(0.844917717132733,-0.831641643055628,
1.59531629414138)) ;
#83250 = CARTESIAN_POINT('Ctrl Pts',(0.600700962335393,-1.02172106265588,
1.57358048557175)) ;
#83251 = CARTESIAN_POINT('Ctrl Pts',(0.462244563371156,-1.09137091714145,
1.5626088525641)) ;
#83252 = CARTESIAN_POINT('Ctrl Pts',(0.170639783454818,-1.17230698850336,
1.54183259516968)) ;
#83253 = CARTESIAN_POINT('Ctrl Pts',(0.0207459066617789,-1.18447520582619,
1.5328513636375)) ;
#83254 = CARTESIAN_POINT('Ctrl Pts',(-0.282514133918315,-1.15139421754003,
1.51305602532775)) ;
#83255 = CARTESIAN_POINT('Ctrl Pts',(-0.432642605518342,-1.10377731834681,
1.50214878809337)) ;
#83256 = CARTESIAN_POINT('Ctrl Pts',(-0.701839874216317,-0.954796873471342,
1.48033609651557)) ;
#83257 = CARTESIAN_POINT('Ctrl Pts',(-0.819149554004533,-0.856285326726335,
1.46963977949436)) ;
#83258 = CARTESIAN_POINT('Ctrl Pts',(-1.00962200101427,-0.620317325344421,
1.44957736213647)) ;
#83259 = CARTESIAN_POINT('Ctrl Pts',(-1.08106222403007,-0.485219252727698,
1.44065567155089)) ;
#83260 = CARTESIAN_POINT('Ctrl Pts',(-1.15834765003112,-0.229692427266968,
1.42253690981624)) ;
#83261 = CARTESIAN_POINT('Ctrl Pts',(-1.17524047358084,-0.115040940888189,
1.41440726252586)) ;
#83262 = CARTESIAN_POINT('Ctrl Pts',(-1.17524047358084,1.76941794549634E-15,
1.40625)) ;
#83263 = CARTESIAN_POINT('Ctrl Pts',(-1.17524047358084,3.04920446938418E-15,
1.34375)) ;
#83264 = CARTESIAN_POINT('Ctrl Pts',(-1.17524047358084,-0.0571461524468516,
1.34780208931927)) ;
#83265 = CARTESIAN_POINT('Ctrl Pts',(-1.17107246744237,-0.11434177785293,
1.35185768664109)) ;
#83266 = CARTESIAN_POINT('Ctrl Pts',(-1.14000361664372,-0.325435712949174,
1.36682582435713)) ;
#83267 = CARTESIAN_POINT('Ctrl Pts',(-1.08681495493178,-0.473604338824473,
1.37713559876278)) ;
#83268 = CARTESIAN_POINT('Ctrl Pts',(-0.928983299727095,-0.735260713248269,
1.39610436984653)) ;
#83269 = CARTESIAN_POINT('Ctrl Pts',(-0.827849738352091,-0.8475019580805,
1.40629411816986)) ;
#83270 = CARTESIAN_POINT('Ctrl Pts',(-0.584329250040727,-1.03147256612151,
1.4277705904358)) ;
#83271 = CARTESIAN_POINT('Ctrl Pts',(-0.44284916566883,-1.09966702637141,
1.43887630176619)) ;
#83272 = CARTESIAN_POINT('Ctrl Pts',(-0.144797673821169,-1.17617198619236,
1.45989133728082)) ;
#83273 = CARTESIAN_POINT('Ctrl Pts',(0.0084922086471124,-1.18501871018999,
1.4689248117494)) ;
#83274 = CARTESIAN_POINT('Ctrl Pts',(0.309344866126974,-1.14387388278698,
1.48885821149429)) ;
#83275 = CARTESIAN_POINT('Ctrl Pts',(0.454041837088111,-1.09451906300235,
1.49949352868873)) ;
#83276 = CARTESIAN_POINT('Ctrl Pts',(0.721892420234701,-0.940665283792315,
1.52139630135329)) ;
#83277 = CARTESIAN_POINT('Ctrl Pts',(0.841303444694949,-0.835587345031483,
1.53245446019827)) ;
#83278 = CARTESIAN_POINT('Ctrl Pts',(1.02663502806333,-0.591169448394882,
1.55250076944265)) ;
#83279 = CARTESIAN_POINT('Ctrl Pts',(1.09332082134992,-0.456198563499785,
1.56140211221623)) ;
#83280 = CARTESIAN_POINT('Ctrl Pts',(1.17371744524374,-0.164538408549839,
1.58208299707245)) ;
#83281 = CARTESIAN_POINT('Ctrl Pts',(1.18514751286619,-0.0102269767388764,
1.59302483091269)) ;
#83282 = CARTESIAN_POINT('Ctrl Pts',(1.14782573398913,0.296588702875181,1.61478035574011)) ;
#83283 = CARTESIAN_POINT('Ctrl Pts',(1.09843102085877,0.446032345250234,1.62537702692745)) ;
#83284 = CARTESIAN_POINT('Ctrl Pts',(0.94743739780899,0.711217516993629,1.64418063760009)) ;
#83285 = CARTESIAN_POINT('Ctrl Pts',(0.849498492656227,0.825756775880921,
1.65419377055637)) ;
#83286 = CARTESIAN_POINT('Ctrl Pts',(0.611371103160633,1.01561578403287,1.67554783095833)) ;
#83287 = CARTESIAN_POINT('Ctrl Pts',(0.472131147139452,1.08735755872389,1.68664174677093)) ;
#83288 = CARTESIAN_POINT('Ctrl Pts',(0.175693143720339,1.17208665320142,1.70784927802165)) ;
#83289 = CARTESIAN_POINT('Ctrl Pts',(0.0216498618195364,1.18497964669672,
1.71707524226508)) ;
#83290 = CARTESIAN_POINT('Ctrl Pts',(-0.280748676962267,1.15117800427482,
1.73684322763561)) ;
#83291 = CARTESIAN_POINT('Ctrl Pts',(-0.426273891349944,1.10557843348025,
1.74739626772215)) ;
#83292 = CARTESIAN_POINT('Ctrl Pts',(-0.69727449409683,0.958988168389735,
1.7692349570435)) ;
#83293 = CARTESIAN_POINT('Ctrl Pts',(-0.819053205034701,0.857331536334873,
1.78031721189922)) ;
#83294 = CARTESIAN_POINT('Ctrl Pts',(-1.01078815793964,0.617964087801939,
1.80057767991255)) ;
#83295 = CARTESIAN_POINT('Ctrl Pts',(-1.08114979329975,0.484448938981724,
1.80939894945103)) ;
#83296 = CARTESIAN_POINT('Ctrl Pts',(-1.15823561048095,0.230432003852988,
1.82741064867621)) ;
#83297 = CARTESIAN_POINT('Ctrl Pts',(-1.17524047358084,0.11542194896722,1.83556572115368)) ;
#83298 = CARTESIAN_POINT('Ctrl Pts',(-1.17524047358084,-2.0122792321331E-15,
1.84375)) ;
#83299 = CARTESIAN_POINT('Origin',(0.,0.,0.)) ;
#83300 = CARTESIAN_POINT('',(-1.17524047358084,1.46543595637449E-15,2.40625)) ;
#83301 = CARTESIAN_POINT('',(-1.17524047358084,-2.10740602288104E-16,2.34375)) ;
#83302 = CARTESIAN_POINT('',(-1.17524047358084,-1.4392544841992E-16,0.)) ;
#83303 = CARTESIAN_POINT('Ctrl Pts',(-1.17524047358084,3.86728371726775E-15,
2.40625)) ;
#83304 = CARTESIAN_POINT('Ctrl Pts',(-1.17524047358084,0.0834495761747775,
2.40033280134642)) ;
#83305 = CARTESIAN_POINT('Ctrl Pts',(-1.16635217935271,0.166862378997987,
2.39441821019833)) ;
#83306 = CARTESIAN_POINT('Ctrl Pts',(-1.11706459718736,0.394393758538108,
2.37828453481763)) ;
#83307 = CARTESIAN_POINT('Ctrl Pts',(-1.05815594704201,0.532602159607403,
2.36901282500718)) ;
#83308 = CARTESIAN_POINT('Ctrl Pts',(-0.887957895915845,0.785522102144264,
2.34959440147497)) ;
#83309 = CARTESIAN_POINT('Ctrl Pts',(-0.776015636887052,0.89626550280217,
2.33879402034525)) ;
#83310 = CARTESIAN_POINT('Ctrl Pts',(-0.518493345242722,1.0656264026718,2.31697569865871)) ;
#83311 = CARTESIAN_POINT('Ctrl Pts',(-0.376135411641797,1.12380087866683,
2.30617132653577)) ;
#83312 = CARTESIAN_POINT('Ctrl Pts',(-0.0791076040610528,1.1821736635866,
2.28586200645094)) ;
#83313 = CARTESIAN_POINT('Ctrl Pts',(0.0725661795061427,1.18259313534048,
2.27705455905564)) ;
#83314 = CARTESIAN_POINT('Ctrl Pts',(0.37397870511359,1.12508890452228,2.25650677712517)) ;
#83315 = CARTESIAN_POINT('Ctrl Pts',(0.520297290338154,1.06534672146473,2.24540360952536)) ;
#83316 = CARTESIAN_POINT('Ctrl Pts',(0.775986170953501,0.895378863462734,
2.22367635441125)) ;
#83317 = CARTESIAN_POINT('Ctrl Pts',(0.884220168238866,0.788690305821157,
2.21324744834696)) ;
#83318 = CARTESIAN_POINT('Ctrl Pts',(1.05687330065032,0.536803523834036,2.19371489338642)) ;
#83319 = CARTESIAN_POINT('Ctrl Pts',(1.11830696198107,0.393125915306599,2.1841255656214)) ;
#83320 = CARTESIAN_POINT('Ctrl Pts',(1.18190897774897,0.0903690543124847,
2.16265784136978)) ;
#83321 = CARTESIAN_POINT('Ctrl Pts',(1.18353793976289,-0.0656690731964901,
2.15159357189922)) ;
#83322 = CARTESIAN_POINT('Ctrl Pts',(1.12733899954514,-0.364026815236812,
2.13043777806047)) ;
#83323 = CARTESIAN_POINT('Ctrl Pts',(1.07214749838274,-0.503861438847376,
2.12089097958312)) ;
#83324 = CARTESIAN_POINT('Ctrl Pts',(0.908803610461331,-0.761303455262943,
2.10173312985122)) ;
#83325 = CARTESIAN_POINT('Ctrl Pts',(0.799906337408573,-0.875004375116867,
2.09101487911931)) ;
#83326 = CARTESIAN_POINT('Ctrl Pts',(0.546748269139941,-1.05146697417733,
2.06921277246286)) ;
#83327 = CARTESIAN_POINT('Ctrl Pts',(0.405609687779362,-1.11355576229213,
2.0583445009321)) ;
#83328 = CARTESIAN_POINT('Ctrl Pts',(0.110368603997391,-1.17959403248063,
2.03787312930077)) ;
#83329 = CARTESIAN_POINT('Ctrl Pts',(-0.0406517881214192,-1.18404743083405,
2.02906590780156)) ;
#83330 = CARTESIAN_POINT('Ctrl Pts',(-0.343388059821988,-1.13485866192171,
2.00873165190228)) ;
#83331 = CARTESIAN_POINT('Ctrl Pts',(-0.491669810186357,-1.07891875610629,
1.99764273583528)) ;
#83332 = CARTESIAN_POINT('Ctrl Pts',(-0.752433496068832,-0.915323715049072,
1.97582978891062)) ;
#83333 = CARTESIAN_POINT('Ctrl Pts',(-0.863678168296611,-0.811203927399449,
1.96530707679724)) ;
#83334 = CARTESIAN_POINT('Ctrl Pts',(-1.04217961452683,-0.564467980662324,
1.9455980068477)) ;
#83335 = CARTESIAN_POINT('Ctrl Pts',(-1.10692635915049,-0.423660441951649,
1.93629069177583)) ;
#83336 = CARTESIAN_POINT('Ctrl Pts',(-1.16439348800968,-0.184272101586651,
1.91931626925363)) ;
#83337 = CARTESIAN_POINT('Ctrl Pts',(-1.17524047358084,-0.0921861360282586,
1.9127866860443)) ;
#83338 = CARTESIAN_POINT('Ctrl Pts',(-1.17524047358084,-1.93364185863387E-15,
1.90625)) ;
#83339 = CARTESIAN_POINT('Ctrl Pts',(-1.17524047358084,-1.97082727899222E-15,
1.84375)) ;
#83340 = CARTESIAN_POINT('Ctrl Pts',(-1.17524047358084,-0.0369227145432839,
1.84636809642177)) ;
#83341 = CARTESIAN_POINT('Ctrl Pts',(-1.17350050494735,-0.0738875789323789,
1.84898918158263)) ;
#83342 = CARTESIAN_POINT('Ctrl Pts',(-1.15531888768442,-0.265927879751574,
1.86260627422142)) ;
#83343 = CARTESIAN_POINT('Ctrl Pts',(-1.10990808627486,-0.416663234139651,
1.87329453744474)) ;
#83344 = CARTESIAN_POINT('Ctrl Pts',(-0.966120197721852,-0.685568682193822,
1.8923619435132)) ;
#83345 = CARTESIAN_POINT('Ctrl Pts',(-0.871483293981198,-0.802462772346145,
1.90201787557277)) ;
#83346 = CARTESIAN_POINT('Ctrl Pts',(-0.639185790066518,-0.998278888114406,
1.92322513798936)) ;
#83347 = CARTESIAN_POINT('Ctrl Pts',(-0.502379855421458,-1.07365518346609,
1.93429844355089)) ;
#83348 = CARTESIAN_POINT('Ctrl Pts',(-0.207738743852656,-1.16699033977343,
1.95570074890575)) ;
#83349 = CARTESIAN_POINT('Ctrl Pts',(-0.0528796569725674,-1.18414916102219,
1.96518693701189)) ;
#83350 = CARTESIAN_POINT('Ctrl Pts',(0.251069176422445,-1.15796405987137,
1.98478008751724)) ;
#83351 = CARTESIAN_POINT('Ctrl Pts',(0.397347839176802,-1.11624903803342,
1.99524167333822)) ;
#83352 = CARTESIAN_POINT('Ctrl Pts',(0.671396769691305,-0.977212386910812,
2.01699974953374)) ;
#83353 = CARTESIAN_POINT('Ctrl Pts',(0.795518854725933,-0.879136203929369,
2.0280989652418)) ;
#83354 = CARTESIAN_POINT('Ctrl Pts',(0.993804818622206,-0.645043587864466,
2.04857470307815)) ;
#83355 = CARTESIAN_POINT('Ctrl Pts',(1.06797519504685,-0.512990391897107,
2.05737514712029)) ;
#83356 = CARTESIAN_POINT('Ctrl Pts',(1.16338541714191,-0.225789755613562,
2.07773981877259)) ;
#83357 = CARTESIAN_POINT('Ctrl Pts',(1.18283238528975,-0.0731000063795935,
2.08856666319766)) ;
#83358 = CARTESIAN_POINT('Ctrl Pts',(1.16209969672046,0.234549305736465,2.11038129880004)) ;
#83359 = CARTESIAN_POINT('Ctrl Pts',(1.12077669646272,0.386486048632133,2.12115474944774)) ;
#83360 = CARTESIAN_POINT('Ctrl Pts',(0.984348216925391,0.659104502713493,
2.14048543539456)) ;
#83361 = CARTESIAN_POINT('Ctrl Pts',(0.893009466813732,0.778407601930865,
2.14984315768763)) ;
#83362 = CARTESIAN_POINT('Ctrl Pts',(0.666587026440478,0.980128001727854,
2.17089897505181)) ;
#83363 = CARTESIAN_POINT('Ctrl Pts',(0.53231423687697,1.05907036021218,2.18194315633091)) ;
#83364 = CARTESIAN_POINT('Ctrl Pts',(0.239593499292404,1.16104702568118,2.20353390977969)) ;
#83365 = CARTESIAN_POINT('Ctrl Pts',(0.0838932043262317,1.1825275122596,2.21333996072108)) ;
#83366 = CARTESIAN_POINT('Ctrl Pts',(-0.221545121912344,1.16392516257651,
2.23275574064081)) ;
#83367 = CARTESIAN_POINT('Ctrl Pts',(-0.368468205679511,1.12606139499527,
2.24312035750159)) ;
#83368 = CARTESIAN_POINT('Ctrl Pts',(-0.645330677917689,0.994553419131068,
2.26478428707692)) ;
#83369 = CARTESIAN_POINT('Ctrl Pts',(-0.771671046636979,0.900068111178731,
2.27589241248701)) ;
#83370 = CARTESIAN_POINT('Ctrl Pts',(-0.976388228670599,0.671262250230045,
2.29657564124344)) ;
#83371 = CARTESIAN_POINT('Ctrl Pts',(-1.05434711077808,0.540627456958495,
2.3054154726478)) ;
#83372 = CARTESIAN_POINT('Ctrl Pts',(-1.15169317363573,0.270768039187681,
2.32455052229915)) ;
#83373 = CARTESIAN_POINT('Ctrl Pts',(-1.17524047358084,0.135823181646263,
2.33411912127776)) ;
#83374 = CARTESIAN_POINT('Ctrl Pts',(-1.17524047358084,-2.04697370165263E-15,
2.34375)) ;
#83375 = CARTESIAN_POINT('Origin',(0.,0.,0.)) ;
#83376 = CARTESIAN_POINT('',(-1.17524047358084,-1.87607513922584E-15,2.90625)) ;
#83377 = CARTESIAN_POINT('',(-1.17524047358084,1.76684416032546E-15,2.84375)) ;
#83378 = CARTESIAN_POINT('',(-1.17524047358084,-1.4392544841992E-16,0.)) ;
#83379 = CARTESIAN_POINT('Ctrl Pts',(-1.17524047358084,-3.33066907387547E-15,
2.90625)) ;
#83380 = CARTESIAN_POINT('Ctrl Pts',(-1.17524047358084,0.102796714931198,
2.89896094460793)) ;
#83381 = CARTESIAN_POINT('Ctrl Pts',(-1.16175251768774,0.205374231616836,
2.89168743200976)) ;
#83382 = CARTESIAN_POINT('Ctrl Pts',(-1.09622846694473,0.449144165446436,
2.87440232176286)) ;
#83383 = CARTESIAN_POINT('Ctrl Pts',(-1.03044749565387,0.584480502606388,
2.8654720323337)) ;
#83384 = CARTESIAN_POINT('Ctrl Pts',(-0.847669471907953,0.828843250210975,
2.84558448648495)) ;
#83385 = CARTESIAN_POINT('Ctrl Pts',(-0.73031054313643,0.933891377908787,
2.83465339897623)) ;
#83386 = CARTESIAN_POINT('Ctrl Pts',(-0.465241211512785,1.0898268629092,2.81284761224835)) ;
#83387 = CARTESIAN_POINT('Ctrl Pts',(-0.320908177432949,1.14070369228232,
2.80218068264354)) ;
#83388 = CARTESIAN_POINT('Ctrl Pts',(-0.0206957133140149,1.1848215140349,
2.78218119192395)) ;
#83389 = CARTESIAN_POINT('Ctrl Pts',(0.132299481600214,1.17759557215243,2.77320929363418)) ;
#83390 = CARTESIAN_POINT('Ctrl Pts',(0.430972390015288,1.10439932805368,2.75227340471072)) ;
#83391 = CARTESIAN_POINT('Ctrl Pts',(0.573329363895275,1.03765163917832,2.74116513908726)) ;
#83392 = CARTESIAN_POINT('Ctrl Pts',(0.819023758124217,0.856061032113319,
2.71963955224451)) ;
#83393 = CARTESIAN_POINT('Ctrl Pts',(0.921414527925757,0.744754050742277,
2.70940572480726)) ;
#83394 = CARTESIAN_POINT('Ctrl Pts',(1.08283436189426,0.48317272917608,2.69021927291669)) ;
#83395 = CARTESIAN_POINT('Ctrl Pts',(1.1377932318867,0.33385005147702,2.67992246384761)) ;
#83396 = CARTESIAN_POINT('Ctrl Pts',(1.18496375441424,0.0261162310963888,
2.65810183597765)) ;
#83397 = CARTESIAN_POINT('Ctrl Pts',(1.17821842944344,-0.128942780920343,
2.6471069931134)) ;
#83398 = CARTESIAN_POINT('Ctrl Pts',(1.10652469798646,-0.423082410616588,
2.62625029496606)) ;
#83399 = CARTESIAN_POINT('Ctrl Pts',(1.04404604218016,-0.5597773011796,2.6171829082496)) ;
#83400 = CARTESIAN_POINT('Ctrl Pts',(0.867294413301401,-0.808282445052659,
2.59751856586323)) ;
#83401 = CARTESIAN_POINT('Ctrl Pts',(0.752501217679453,-0.916101525685282,
2.58664679342224)) ;
#83402 = CARTESIAN_POINT('Ctrl Pts',(0.490970385683506,-1.07852996685889,
2.56482809816473)) ;
#83403 = CARTESIAN_POINT('Ctrl Pts',(0.347540328044389,-1.13292001959081,
2.55409206134565)) ;
#83404 = CARTESIAN_POINT('Ctrl Pts',(0.0488368145967983,-1.1838982236926,
2.53394200558513)) ;
#83405 = CARTESIAN_POINT('Ctrl Pts',(-0.103503123360973,-1.18037661342213,
2.5250762093136)) ;
#83406 = CARTESIAN_POINT('Ctrl Pts',(-0.403542762412943,-1.11476842320377,
2.50432541750764)) ;
#83407 = CARTESIAN_POINT('Ctrl Pts',(-0.547856624339745,-1.05137942574436,
2.49321606210347)) ;
#83408 = CARTESIAN_POINT('Ctrl Pts',(-0.798450359446747,-0.875341296917099,
2.47158647423735)) ;
#83409 = CARTESIAN_POINT('Ctrl Pts',(-0.903692038123453,-0.76622942971059,
2.46125540411813)) ;
#83410 = CARTESIAN_POINT('Ctrl Pts',(-1.07057692923121,-0.509331921162476,
2.44189941445632)) ;
#83411 = CARTESIAN_POINT('Ctrl Pts',(-1.12870603757051,-0.362776011402504,
2.43197353059918)) ;
#83412 = CARTESIAN_POINT('Ctrl Pts',(-1.16899556970882,-0.139924281782822,
2.41617167737358)) ;
#83413 = CARTESIAN_POINT('Ctrl Pts',(-1.17524047358084,-0.0699492221345031,
2.41120992265036)) ;
#83414 = CARTESIAN_POINT('Ctrl Pts',(-1.17524047358084,3.86728371726775E-15,
2.40625)) ;
#83415 = CARTESIAN_POINT('Ctrl Pts',(-1.17524047358084,-1.97082727899222E-15,
2.34375)) ;
#83416 = CARTESIAN_POINT('Ctrl Pts',(-1.17524047358084,-0.0159893943237037,
2.34488376756241)) ;
#83417 = CARTESIAN_POINT('Ctrl Pts',(-1.17491416755614,-0.031990960902034,
2.34601839822863)) ;
#83418 = CARTESIAN_POINT('Ctrl Pts',(-1.16789302334604,-0.203772957593621,
2.35819902569405)) ;
#83419 = CARTESIAN_POINT('Ctrl Pts',(-1.13058937576196,-0.35677151180435,
2.36904776669998)) ;
#83420 = CARTESIAN_POINT('Ctrl Pts',(-1.00137560583638,-0.632943406666202,
2.38863041815657)) ;
#83421 = CARTESIAN_POINT('Ctrl Pts',(-0.91320344982542,-0.754615858669875,
2.39775958595751)) ;
#83422 = CARTESIAN_POINT('Ctrl Pts',(-0.692462386878117,-0.961956822065874,
2.41866579313358)) ;
#83423 = CARTESIAN_POINT('Ctrl Pts',(-0.560711658947958,-1.04425308901793,
2.42967400906333)) ;
#83424 = CARTESIAN_POINT('Ctrl Pts',(-0.269955844015801,-1.15455632123922,
2.45143930909058)) ;
#83425 = CARTESIAN_POINT('Ctrl Pts',(-0.113430199319369,-1.1802422369551,
2.46160718411688)) ;
#83426 = CARTESIAN_POINT('Ctrl Pts',(0.193381317443829,-1.16888890246322,
2.48085028379429)) ;
#83427 = CARTESIAN_POINT('Ctrl Pts',(0.340823271976921,-1.13468702620785,
2.4911169355698)) ;
#83428 = CARTESIAN_POINT('Ctrl Pts',(0.620169972116385,-1.0103740433884,2.51267832641062)) ;
#83429 = CARTESIAN_POINT('Ctrl Pts',(0.748523511011231,-0.919340734146067,
2.52378768966377)) ;
#83430 = CARTESIAN_POINT('Ctrl Pts',(0.95930284898831,-0.695623131354465,
2.54466278354844)) ;
#83431 = CARTESIAN_POINT('Ctrl Pts',(1.0408833027931,-0.566314536431026,2.55359406672777)) ;
#83432 = CARTESIAN_POINT('Ctrl Pts',(1.15057221143423,-0.283558081993978,
2.5736436126713)) ;
#83433 = CARTESIAN_POINT('Ctrl Pts',(1.17752841498523,-0.132793104251016,
2.5843339764119)) ;
#83434 = CARTESIAN_POINT('Ctrl Pts',(1.17258071781568,0.174811322933465,2.60614542933716)) ;
#83435 = CARTESIAN_POINT('Ctrl Pts',(1.13906811408573,0.328705172668025,2.61705765348718)) ;
#83436 = CARTESIAN_POINT('Ctrl Pts',(1.01665018435854,0.608144314357815,2.6368719771633)) ;
#83437 = CARTESIAN_POINT('Ctrl Pts',(0.931405988739206,0.732058253005227,
2.64584205896672)) ;
#83438 = CARTESIAN_POINT('Ctrl Pts',(0.715945908723865,0.944548908495419,
2.66660654909468)) ;
#83439 = CARTESIAN_POINT('Ctrl Pts',(0.586599278267999,1.02987735240299,2.67757463699525)) ;
#83440 = CARTESIAN_POINT('Ctrl Pts',(0.300150572994426,1.14691880914246,2.69931434267748)) ;
#83441 = CARTESIAN_POINT('Ctrl Pts',(0.14555775932464,1.17654992989502,2.70976521147525)) ;
#83442 = CARTESIAN_POINT('Ctrl Pts',(-0.159812805757192,1.17389589616134,
2.72861140294063)) ;
#83443 = CARTESIAN_POINT('Ctrl Pts',(-0.307753050386385,1.14404354082301,
2.73875444678115)) ;
#83444 = CARTESIAN_POINT('Ctrl Pts',(-0.589810317143855,1.02832259298039,
2.76017766746428)) ;
#83445 = CARTESIAN_POINT('Ctrl Pts',(-0.720434359265456,0.941436947348458,
2.77127940686414)) ;
#83446 = CARTESIAN_POINT('Ctrl Pts',(-0.938352564545528,0.72385413908037,
2.79237538059191)) ;
#83447 = CARTESIAN_POINT('Ctrl Pts',(-1.02427130333543,0.596096991198836,
2.80148226809044)) ;
#83448 = CARTESIAN_POINT('Ctrl Pts',(-1.14204739775072,0.315947654532678,
2.82134694989839)) ;
#83449 = CARTESIAN_POINT('Ctrl Pts',(-1.17319161754045,0.166433527854817,
2.8319486189496)) ;
#83450 = CARTESIAN_POINT('Ctrl Pts',(-1.17520791360152,0.0101030964659361,
2.84303361494994)) ;
#83451 = CARTESIAN_POINT('Ctrl Pts',(-1.17524047358084,0.00505079841659654,
2.84339186064256)) ;
#83452 = CARTESIAN_POINT('Ctrl Pts',(-1.17524047358084,3.8300982969094E-15,
2.84375)) ;
#83453 = CARTESIAN_POINT('Origin',(0.,0.,0.)) ;
#83454 = CARTESIAN_POINT('',(-1.17524047358084,1.11632285683415E-15,3.40625)) ;
#83455 = CARTESIAN_POINT('',(-1.17524047358084,3.12860208896725E-15,3.34375)) ;
#83456 = CARTESIAN_POINT('',(-1.17524047358084,-1.4392544841992E-16,0.)) ;
#83457 = CARTESIAN_POINT('Ctrl Pts',(-1.17524047358084,4.40619762898109E-15,
3.40625)) ;
#83458 = CARTESIAN_POINT('Ctrl Pts',(-1.17524047358084,0.123092062062834,
3.39752185280871)) ;
#83459 = CARTESIAN_POINT('Ctrl Pts',(-1.15590038001192,0.245621219624255,
3.38883361975373)) ;
#83460 = CARTESIAN_POINT('Ctrl Pts',(-1.07142376848625,0.505704859705224,
3.37039174580484)) ;
#83461 = CARTESIAN_POINT('Ctrl Pts',(-0.998235456447153,0.638130708170466,
3.3615918656591)) ;
#83462 = CARTESIAN_POINT('Ctrl Pts',(-0.801629981464181,0.873587217586578,
3.3411709676216)) ;
#83463 = CARTESIAN_POINT('Ctrl Pts',(-0.678101194694549,0.972589508504834,
3.33007535099264)) ;
#83464 = CARTESIAN_POINT('Ctrl Pts',(-0.40481703820335,1.11357539151809,3.30829513023606)) ;
#83465 = CARTESIAN_POINT('Ctrl Pts',(-0.258722442497593,1.15629084316166,
3.29780937856914)) ;
#83466 = CARTESIAN_POINT('Ctrl Pts',(0.0448317785119429,1.18444011834994,
3.27817082298269)) ;
#83467 = CARTESIAN_POINT('Ctrl Pts',(0.199477442066073,1.16838838479748,3.26875762215172)) ;
#83468 = CARTESIAN_POINT('Ctrl Pts',(0.494594327588301,1.07727980730025,3.24740504116467)) ;
#83469 = CARTESIAN_POINT('Ctrl Pts',(0.632038624059815,1.00283603509006,3.23632559671853)) ;
#83470 = CARTESIAN_POINT('Ctrl Pts',(0.865846472707079,0.808553580002312,
3.21507996154768)) ;
#83471 = CARTESIAN_POINT('Ctrl Pts',(0.961335813428651,0.692272716898223,
3.20533730967976)) ;
#83472 = CARTESIAN_POINT('Ctrl Pts',(1.10699956285693,0.424327747474994,3.18633800872487)) ;
#83473 = CARTESIAN_POINT('Ctrl Pts',(1.1534495275018,0.273917693398749,3.17567281172495)) ;
#83474 = CARTESIAN_POINT('Ctrl Pts',(1.18468568302401,-0.0333087329033022,
3.15388816188743)) ;
#83475 = CARTESIAN_POINT('Ctrl Pts',(1.17029961616188,-0.187073114751344,
3.14298511797822)) ;
#83476 = CARTESIAN_POINT('Ctrl Pts',(1.08438834604793,-0.477121901343889,
3.12241849118191)) ;
#83477 = CARTESIAN_POINT('Ctrl Pts',(1.01498853020898,-0.611013566767672,
3.11358203694755)) ;
#83478 = CARTESIAN_POINT('Ctrl Pts',(0.824921751742507,-0.851706530322419,
3.09337701318501)) ;
#83479 = CARTESIAN_POINT('Ctrl Pts',(0.703752672949174,-0.95426200692336,
3.08230032702302)) ;
#83480 = CARTESIAN_POINT('Ctrl Pts',(0.433556743847305,-1.10275613565874,
3.06044355175743)) ;
#83481 = CARTESIAN_POINT('Ctrl Pts',(0.288238670419427,-1.14933810079984,
3.04986840216459)) ;
#83482 = CARTESIAN_POINT('Ctrl Pts',(-0.0137600089507247,-1.18506222361528,
3.03005681211611)) ;
#83483 = CARTESIAN_POINT('Ctrl Pts',(-0.167602700280939,-1.17323466445312,
3.02088679462236)) ;
#83484 = CARTESIAN_POINT('Ctrl Pts',(-0.464474152133334,-1.09066572219718,
2.99972923178039)) ;
#83485 = CARTESIAN_POINT('Ctrl Pts',(-0.604310753179328,-1.01984881684707,
2.9886314674591)) ;
#83486 = CARTESIAN_POINT('Ctrl Pts',(-0.843789761265557,-0.831582903172137,
2.96725088845622)) ;
#83487 = CARTESIAN_POINT('Ctrl Pts',(-0.942598090975861,-0.717666170959262,
2.95714452491155)) ;
#83488 = CARTESIAN_POINT('Ctrl Pts',(-1.09538049653803,-0.453420168177252,
2.93839400450008)) ;
#83489 = CARTESIAN_POINT('Ctrl Pts',(-1.14581664734383,-0.30432730260374,
2.92782908029924)) ;
#83490 = CARTESIAN_POINT('Ctrl Pts',(-1.17205840686471,-0.0999155125112192,
2.91333475660637)) ;
#83491 = CARTESIAN_POINT('Ctrl Pts',(-1.17524047358084,-0.0499318976710169,
2.90979054473627)) ;
#83492 = CARTESIAN_POINT('Ctrl Pts',(-1.17524047358084,-3.79291287655106E-15,
2.90625)) ;
#83493 = CARTESIAN_POINT('Ctrl Pts',(-1.17524047358084,3.92047505570758E-15,
2.84375)) ;
#83494 = CARTESIAN_POINT('Ctrl Pts',(-1.17524047358084,-0.152126593682685,
2.85453691248745)) ;
#83495 = CARTESIAN_POINT('Ctrl Pts',(-1.14570195523154,-0.30289276073012,
2.86522736055861)) ;
#83496 = CARTESIAN_POINT('Ctrl Pts',(-1.03177105272725,-0.582195023770608,
2.88503197851547)) ;
#83497 = CARTESIAN_POINT('Ctrl Pts',(-0.949525466818209,-0.70845542441791,
2.89389257548998)) ;
#83498 = CARTESIAN_POINT('Ctrl Pts',(-0.739493191168034,-0.926167026186486,
2.91450885883425)) ;
#83499 = CARTESIAN_POINT('Ctrl Pts',(-0.612673416800777,-1.01452432539374,
2.92542916261959)) ;
#83500 = CARTESIAN_POINT('Ctrl Pts',(-0.329814365549704,-1.13872553130698,
2.94720227586273)) ;
#83501 = CARTESIAN_POINT('Ctrl Pts',(-0.176048087867001,-1.1723934496705,
2.95783835880861)) ;
#83502 = CARTESIAN_POINT('Ctrl Pts',(0.128954723639944,-1.17762545861859,
2.97675336623768)) ;
#83503 = CARTESIAN_POINT('Ctrl Pts',(0.27727628357567,-1.15177912605721,2.98660868402162)) ;
#83504 = CARTESIAN_POINT('Ctrl Pts',(0.561718479925036,-1.04387119659527,
3.00790135698431)) ;
#83505 = CARTESIAN_POINT('Ctrl Pts',(0.69429664646387,-0.960806993799944,
3.01898761018966)) ;
#83506 = CARTESIAN_POINT('Ctrl Pts',(0.918663492912159,-0.748906987703286,
3.04027810339717)) ;
#83507 = CARTESIAN_POINT('Ctrl Pts',(1.00857503310541,-0.62254998347992,3.04960655322784)) ;
#83508 = CARTESIAN_POINT('Ctrl Pts',(1.13362015305737,-0.34480079881445,3.06930104632019)) ;
#83509 = CARTESIAN_POINT('Ctrl Pts',(1.16848146009738,-0.196507126553218,
3.07981617603158)) ;
#83510 = CARTESIAN_POINT('Ctrl Pts',(1.18045210584942,0.111025344536259,3.1016225267319)) ;
#83511 = CARTESIAN_POINT('Ctrl Pts',(1.15511396970844,0.267432180839338,3.1127129404117)) ;
#83512 = CARTESIAN_POINT('Ctrl Pts',(1.04700014446727,0.554458555440088,3.13306525560825)) ;
#83513 = CARTESIAN_POINT('Ctrl Pts',(0.967898515283207,0.683233687816861,
3.14187012450672)) ;
#83514 = CARTESIAN_POINT('Ctrl Pts',(0.763568577207577,0.906354575428315,
3.16232801996293)) ;
#83515 = CARTESIAN_POINT('Ctrl Pts',(0.639459802292681,0.99779626387338,3.17319120070305)) ;
#83516 = CARTESIAN_POINT('Ctrl Pts',(0.360385805909782,1.12942715567709,3.19499529266108)) ;
#83517 = CARTESIAN_POINT('Ctrl Pts',(0.207552209614602,1.16723163352072,3.20572075830446)) ;
#83518 = CARTESIAN_POINT('Ctrl Pts',(-0.0970329583631905,1.18066001159202,
3.22490071113121)) ;
#83519 = CARTESIAN_POINT('Ctrl Pts',(-0.24576523956688,1.15888046266532,3.23442189518927)) ;
#83520 = CARTESIAN_POINT('Ctrl Pts',(-0.532433326707437,1.0590459441693,3.25556502233849)) ;
#83521 = CARTESIAN_POINT('Ctrl Pts',(-0.666905793461843,0.979949453657754,
3.26662692988576)) ;
#83522 = CARTESIAN_POINT('Ctrl Pts',(-0.897847745957213,0.773991028819708,
3.28811053380133)) ;
#83523 = CARTESIAN_POINT('Ctrl Pts',(-0.991908182729067,0.649069202730488,
3.29772614237813)) ;
#83524 = CARTESIAN_POINT('Ctrl Pts',(-1.12433615609302,0.373813399472767,
3.31724383609312)) ;
#83525 = CARTESIAN_POINT('Ctrl Pts',(-1.16292193409571,0.226849787736784,
3.32766465457238)) ;
#83526 = CARTESIAN_POINT('Ctrl Pts',(-1.17440830644317,0.0510959910084378,
3.34012691234566)) ;
#83527 = CARTESIAN_POINT('Ctrl Pts',(-1.17524047358084,0.025534463780991,
3.34193941567314)) ;
#83528 = CARTESIAN_POINT('Ctrl Pts',(-1.17524047358084,3.8300982969094E-15,
3.34375)) ;
#83529 = CARTESIAN_POINT('Origin',(0.,0.,0.)) ;
#83530 = CARTESIAN_POINT('',(-1.17524047358084,-8.87282757919059E-16,3.90625)) ;
#83531 = CARTESIAN_POINT('',(-1.17524047358084,-7.65852114600683E-16,3.84375)) ;
#83532 = CARTESIAN_POINT('',(-1.17524047358084,-1.4392544841992E-16,0.)) ;
#83533 = CARTESIAN_POINT('Ctrl Pts',(-1.17524047358084,-4.61436444609831E-15,
3.90625)) ;
#83534 = CARTESIAN_POINT('Ctrl Pts',(-1.17524047358084,0.142946901613543,
3.89611399628934)) ;
#83535 = CARTESIAN_POINT('Ctrl Pts',(-1.1491589245173,0.284799858846186,3.88605556141144)) ;
#83536 = CARTESIAN_POINT('Ctrl Pts',(-1.04428959141748,0.559955417645546,
3.86654497577778)) ;
#83537 = CARTESIAN_POINT('Ctrl Pts',(-0.963615569038733,0.68959302865811,
3.85764140732964)) ;
#83538 = CARTESIAN_POINT('Ctrl Pts',(-0.754344875320265,0.914587047104567,
3.83681370207455)) ;
#83539 = CARTESIAN_POINT('Ctrl Pts',(-0.626485163312983,1.0064855174128,3.82570399038894)) ;
#83540 = CARTESIAN_POINT('Ctrl Pts',(-0.3477412494646,1.13259792905656,3.80411581877577)) ;
#83541 = CARTESIAN_POINT('Ctrl Pts',(-0.200420290895077,1.16771393451668,
3.7938241877845)) ;
#83542 = CARTESIAN_POINT('Ctrl Pts',(0.106052340955811,1.18088096493308,3.77453759594294)) ;
#83543 = CARTESIAN_POINT('Ctrl Pts',(0.262369877053113,1.15625423255477,3.7644653429766)) ;
#83544 = CARTESIAN_POINT('Ctrl Pts',(0.55362950714163,1.04804009767492,3.74274317114028)) ;
#83545 = CARTESIAN_POINT('Ctrl Pts',(0.686020312601358,0.966577589927002,
3.73172520941794)) ;
#83546 = CARTESIAN_POINT('Ctrl Pts',(0.908188754124144,0.760640735684068,
3.71078113116053)) ;
#83547 = CARTESIAN_POINT('Ctrl Pts',(0.997154657087659,0.639567498828977,
3.70160011579944)) ;
#83548 = CARTESIAN_POINT('Ctrl Pts',(1.12819030460119,0.364284748481715,3.6820805113344)) ;
#83549 = CARTESIAN_POINT('Ctrl Pts',(1.16650968655984,0.21154349106954,3.67125001459453)) ;
#83550 = CARTESIAN_POINT('Ctrl Pts',(1.18114170999137,-0.0961853876034204,
3.64942973712858)) ;
#83551 = CARTESIAN_POINT('Ctrl Pts',(1.15877886932711,-0.248175324724643,
3.63865251461271)) ;
#83552 = CARTESIAN_POINT('Ctrl Pts',(1.05785413346947,-0.533682336843727,
3.61840793357184)) ;
#83553 = CARTESIAN_POINT('Ctrl Pts',(0.980856866002174,-0.664674810720661,
3.60958359921497)) ;
#83554 = CARTESIAN_POINT('Ctrl Pts',(0.777764588059354,-0.894826428636171,
3.58895243992535)) ;
#83555 = CARTESIAN_POINT('Ctrl Pts',(0.651976704282397,-0.990225850296007,
3.57784583258341)) ;
#83556 = CARTESIAN_POINT('Ctrl Pts',(0.375807896236073,-1.12364601950554,
3.55615670491253)) ;
#83557 = CARTESIAN_POINT('Ctrl Pts',(0.229038560342614,-1.16248604997788,
3.54576691718324)) ;
#83558 = CARTESIAN_POINT('Ctrl Pts',(-0.0760266080667465,-1.18301413991114,
3.52630577732941)) ;
#83559 = CARTESIAN_POINT('Ctrl Pts',(-0.231510867798561,-1.16263852629176,
3.51658667002208)) ;
#83560 = CARTESIAN_POINT('Ctrl Pts',(-0.524732102727574,-1.06286326271082,
3.49504323011921)) ;
#83561 = CARTESIAN_POINT('Ctrl Pts',(-0.65965851366554,-0.984821206774737,
3.48399083056172)) ;
#83562 = CARTESIAN_POINT('Ctrl Pts',(-0.887579615110947,-0.78459783705296,
3.46289605921784)) ;
#83563 = CARTESIAN_POINT('Ctrl Pts',(-0.979757190311564,-0.665913011896129,
3.45346820958247)) ;
#83564 = CARTESIAN_POINT('Ctrl Pts',(-1.11807259121496,-0.394238123750088,
3.43420442951269)) ;
#83565 = CARTESIAN_POINT('Ctrl Pts',(-1.16044512750511,-0.242598028979702,
3.42345201343422)) ;
#83566 = CARTESIAN_POINT('Ctrl Pts',(-1.17416414971479,-0.0581108873613505,
3.41037049623514)) ;
#83567 = CARTESIAN_POINT('Ctrl Pts',(-1.17524047358084,-0.0290397786505206,
3.40830913734985)) ;
#83568 = CARTESIAN_POINT('Ctrl Pts',(-1.17524047358084,3.86728371726775E-15,
3.40625)) ;
#83569 = CARTESIAN_POINT('Ctrl Pts',(-1.17524047358084,3.22658566531686E-15,
3.34375)) ;
#83570 = CARTESIAN_POINT('Ctrl Pts',(-1.17524047358084,-0.130483209475118,
3.35300223478431)) ;
#83571 = CARTESIAN_POINT('Ctrl Pts',(-1.15350790037109,-0.260259712787548,
3.36220435881975)) ;
#83572 = CARTESIAN_POINT('Ctrl Pts',(-1.06162271654697,-0.526085279377952,
3.38105337827336)) ;
#83573 = CARTESIAN_POINT('Ctrl Pts',(-0.985684775170123,-0.657445115209627,
3.38986361039039)) ;
#83574 = CARTESIAN_POINT('Ctrl Pts',(-0.787094018328788,-0.88593423012538,
3.41015939979644)) ;
#83575 = CARTESIAN_POINT('Ctrl Pts',(-0.665766803792927,-0.980377255471268,
3.42095817999328)) ;
#83576 = CARTESIAN_POINT('Ctrl Pts',(-0.390670514530027,-1.11931648336967,
3.44277711803581)) ;
#83577 = CARTESIAN_POINT('Ctrl Pts',(-0.238883506616201,-1.16122754663595,
3.45358390892082)) ;
#83578 = CARTESIAN_POINT('Ctrl Pts',(0.0652067499452988,-1.1828388016687,
3.47302358395648)) ;
#83579 = CARTESIAN_POINT('Ctrl Pts',(0.21439210539306,-1.1650817465961,3.48227548530999)) ;
#83580 = CARTESIAN_POINT('Ctrl Pts',(0.503181454485975,-1.073193310475,3.50326715590652)) ;
#83581 = CARTESIAN_POINT('Ctrl Pts',(0.639406917105912,-0.998044366447435,
3.51429675557723)) ;
#83582 = CARTESIAN_POINT('Ctrl Pts',(0.876777484238287,-0.798048737993809,
3.53596372234866)) ;
#83583 = CARTESIAN_POINT('Ctrl Pts',(0.974975375041977,-0.674546337411974,
3.54591962311291)) ;
#83584 = CARTESIAN_POINT('Ctrl Pts',(1.11460032262829,-0.401776023878272,
3.56526107702989)) ;
#83585 = CARTESIAN_POINT('Ctrl Pts',(1.15676310438279,-0.256194006053251,
3.57558393017482)) ;
#83586 = CARTESIAN_POINT('Ctrl Pts',(1.18455103405537,0.0487251835052672,
3.59720497968292)) ;
#83587 = CARTESIAN_POINT('Ctrl Pts',(1.16762799416042,0.205401534263999,3.60831450395198)) ;
#83588 = CARTESIAN_POINT('Ctrl Pts',(1.07505395344607,0.498276653639495,3.62908153886662)) ;
#83589 = CARTESIAN_POINT('Ctrl Pts',(1.00218359127923,0.632176154534591,3.63795457738639)) ;
#83590 = CARTESIAN_POINT('Ctrl Pts',(0.809134037081688,0.865785758313647,
3.65809163489348)) ;
#83591 = CARTESIAN_POINT('Ctrl Pts',(0.690539621904492,0.963028817488338,
3.66882187190168)) ;
#83592 = CARTESIAN_POINT('Ctrl Pts',(0.419437138478927,1.10886120636148,3.69063994793443)) ;
#83593 = CARTESIAN_POINT('Ctrl Pts',(0.268760300407346,1.15468110020436,3.70151714852314)) ;
#83594 = CARTESIAN_POINT('Ctrl Pts',(-0.0347798880424834,1.18413544278438,
3.72120111191882)) ;
#83595 = CARTESIAN_POINT('Ctrl Pts',(-0.18444046516192,1.17020530514855,3.7302545754592)) ;
#83596 = CARTESIAN_POINT('Ctrl Pts',(-0.475174156686655,1.08582907581352,
3.75109930779784)) ;
#83597 = CARTESIAN_POINT('Ctrl Pts',(-0.612953208086329,1.01444551153309,
3.76209081295829)) ;
#83598 = CARTESIAN_POINT('Ctrl Pts',(-0.854990498523108,0.821285178496173,
3.7838020155861)) ;
#83599 = CARTESIAN_POINT('Ctrl Pts',(-0.956258019499858,0.700744194359125,
3.79406199925237)) ;
#83600 = CARTESIAN_POINT('Ctrl Pts',(-1.10294642971048,0.432602098744818,
3.81307527792753)) ;
#83601 = CARTESIAN_POINT('Ctrl Pts',(-1.14903783149158,0.288659253487398,
3.82328190148623)) ;
#83602 = CARTESIAN_POINT('Ctrl Pts',(-1.17245792453858,0.093437291591936,
3.83712459767508)) ;
#83603 = CARTESIAN_POINT('Ctrl Pts',(-1.17524047358084,0.0466922986522145,
3.84043916704695)) ;
#83604 = CARTESIAN_POINT('Ctrl Pts',(-1.17524047358084,-3.71854203583437E-15,
3.84375)) ;
#83605 = CARTESIAN_POINT('Origin',(0.,0.,0.)) ;
#83606 = CARTESIAN_POINT('',(-1.17524047358084,9.68871361376125E-16,4.40624999999999)) ;
#83607 = CARTESIAN_POINT('',(-1.17524047358084,-2.37914494725911E-15,4.34374999999999)) ;
#83608 = CARTESIAN_POINT('',(-1.17524047358084,-1.4392544841992E-16,0.)) ;
#83609 = CARTESIAN_POINT('Ctrl Pts',(-1.17524047358084,1.90683135537553E-30,
4.40624999999999)) ;
#83610 = CARTESIAN_POINT('Ctrl Pts',(-1.17524047358084,0.0128716194911538,
4.40533730597549)) ;
#83611 = CARTESIAN_POINT('Ctrl Pts',(-1.17502901344671,0.0257515459259134,
4.40442402292659)) ;
#83612 = CARTESIAN_POINT('Ctrl Pts',(-1.16947972214485,0.194466094770272,
4.39246090043968)) ;
#83613 = CARTESIAN_POINT('Ctrl Pts',(-1.1333934290327,0.347763277250189,4.38159098445752)) ;
#83614 = CARTESIAN_POINT('Ctrl Pts',(-1.00636237929119,0.624993082444022,
4.36193331925155)) ;
#83615 = CARTESIAN_POINT('Ctrl Pts',(-0.919136169074253,0.747384332887866,
4.35286111314413)) ;
#83616 = CARTESIAN_POINT('Ctrl Pts',(-0.700098714093276,0.956394260739641,
4.33200034954346)) ;
#83617 = CARTESIAN_POINT('Ctrl Pts',(-0.569117427224042,1.03967776490008,
4.32100438195105)) ;
#83618 = CARTESIAN_POINT('Ctrl Pts',(-0.278971950167976,1.1524718093816,4.2991882527502)) ;
#83619 = CARTESIAN_POINT('Ctrl Pts',(-0.122197490070545,1.1794242883068,4.28890219547748)) ;
#83620 = CARTESIAN_POINT('Ctrl Pts',(0.185013179439947,1.1702291438196,4.2697111006592)) ;
#83621 = CARTESIAN_POINT('Ctrl Pts',(0.332591497936668,1.13711307177577,4.25947457090684)) ;
#83622 = CARTESIAN_POINT('Ctrl Pts',(0.612639221476556,1.01494031829922,4.23794601097797)) ;
#83623 = CARTESIAN_POINT('Ctrl Pts',(0.741571806097502,0.924937605955755,
4.22683762838516)) ;
#83624 = CARTESIAN_POINT('Ctrl Pts',(0.954139258068047,0.70274177553902,4.2059066830972)) ;
#83625 = CARTESIAN_POINT('Ctrl Pts',(1.03679863747558,0.573822476343852,4.19693830232643)) ;
#83626 = CARTESIAN_POINT('Ctrl Pts',(1.14851756853483,0.291714221415981,4.17693471857275)) ;
#83627 = CARTESIAN_POINT('Ctrl Pts',(1.17652988979183,0.141252473189452,4.16626585607121)) ;
#83628 = CARTESIAN_POINT('Ctrl Pts',(1.17382180480569,-0.166279287440103,
4.1444595557478)) ;
#83629 = CARTESIAN_POINT('Ctrl Pts',(1.14142759470212,-0.320417855077137,
4.13352997926948)) ;
#83630 = CARTESIAN_POINT('Ctrl Pts',(1.02101421940899,-0.600805711523604,
4.11364838462641)) ;
#83631 = CARTESIAN_POINT('Ctrl Pts',(0.936624318794625,-0.725382913496972,
4.10471505227448)) ;
#83632 = CARTESIAN_POINT('Ctrl Pts',(0.722708975269278,-0.93936673538121,
4.08399248249237)) ;
#83633 = CARTESIAN_POINT('Ctrl Pts',(0.594075891314688,-1.02556630487159,
4.07303732716529)) ;
#83634 = CARTESIAN_POINT('Ctrl Pts',(0.308605328998943,-1.14467192257802,
4.0512845047467)) ;
#83635 = CARTESIAN_POINT('Ctrl Pts',(0.154247834183575,-1.17543888794573,
4.04072903521798)) ;
#83636 = CARTESIAN_POINT('Ctrl Pts',(-0.150998891746284,-1.17504814395324,
4.02197069050609)) ;
#83637 = CARTESIAN_POINT('Ctrl Pts',(-0.299048572172097,-1.14633511102661,
4.01186131970491)) ;
#83638 = CARTESIAN_POINT('Ctrl Pts',(-0.580235062583513,-1.03349017525507,
3.99059353674741)) ;
#83639 = CARTESIAN_POINT('Ctrl Pts',(-0.710182219725325,-0.948904884149489,
3.97961491944388)) ;
#83640 = CARTESIAN_POINT('Ctrl Pts',(-0.926950131953632,-0.737683011794045,
3.95881510148556)) ;
#83641 = CARTESIAN_POINT('Ctrl Pts',(-1.01291829531872,-0.614327874904145,
3.94981043782202)) ;
#83642 = CARTESIAN_POINT('Ctrl Pts',(-1.13702740411321,-0.335694479443153,
3.93005324757567)) ;
#83643 = CARTESIAN_POINT('Ctrl Pts',(-1.17148359162314,-0.182013941692096,
3.91915614883959)) ;
#83644 = CARTESIAN_POINT('Ctrl Pts',(-1.17514374548819,-0.0174150947011532,
3.90748486037486)) ;
#83645 = CARTESIAN_POINT('Ctrl Pts',(-1.17524047358084,-0.00870551871022769,
3.90686728634167)) ;
#83646 = CARTESIAN_POINT('Ctrl Pts',(-1.17524047358084,-3.79291287655106E-15,
3.90625)) ;
#83647 = CARTESIAN_POINT('Ctrl Pts',(-1.17524047358084,-3.12250225675825E-15,
3.84375)) ;
#83648 = CARTESIAN_POINT('Ctrl Pts',(-1.17524047358084,-0.108258895333412,
3.85142636480696)) ;
#83649 = CARTESIAN_POINT('Ctrl Pts',(-1.16028088637367,-0.216234520909998,
3.85908264367101)) ;
#83650 = CARTESIAN_POINT('Ctrl Pts',(-1.08910194938674,-0.467076363318089,
3.87686920509162)) ;
#83651 = CARTESIAN_POINT('Ctrl Pts',(-1.01964084687618,-0.603846833868942,
3.88587818764472)) ;
#83652 = CARTESIAN_POINT('Ctrl Pts',(-0.832725477793128,-0.843046352796263,
3.90583674249475)) ;
#83653 = CARTESIAN_POINT('Ctrl Pts',(-0.71720215641018,-0.943273281852801,
3.91648418011504)) ;
#83654 = CARTESIAN_POINT('Ctrl Pts',(-0.449321885193019,-1.09731938696322,
3.93839559452685)) ;
#83655 = CARTESIAN_POINT('Ctrl Pts',(-0.298349998552315,-1.14760859635405,
3.94944936729988)) ;
#83656 = CARTESIAN_POINT('Ctrl Pts',(0.00616172932227222,-1.18465574205611,
3.96946218391667)) ;
#83657 = CARTESIAN_POINT('Ctrl Pts',(0.156307571630098,-1.17431790910372,
3.97838119273087)) ;
#83658 = CARTESIAN_POINT('Ctrl Pts',(0.448801251791293,-1.0969418842604,3.99908581846858)) ;
#83659 = CARTESIAN_POINT('Ctrl Pts',(0.58793583219071,-1.0290916116714,4.0100352951173)) ;
#83660 = CARTESIAN_POINT('Ctrl Pts',(0.834258197193588,-0.842306532240701,
4.03178360764163)) ;
#83661 = CARTESIAN_POINT('Ctrl Pts',(0.93849259450696,-0.724379572815127,
4.04236535091666)) ;
#83662 = CARTESIAN_POINT('Ctrl Pts',(1.09158794225778,-0.460347016038917,
4.06112752092142)) ;
#83663 = CARTESIAN_POINT('Ctrl Pts',(1.14123666714252,-0.317992959561192,
4.07120192248525)) ;
#83664 = CARTESIAN_POINT('Ctrl Pts',(1.18532600445379,-0.0165202074694624,
4.09257859381825)) ;
#83665 = CARTESIAN_POINT('Ctrl Pts',(1.17715057099471,0.139970764168848,4.10367497298973)) ;
#83666 = CARTESIAN_POINT('Ctrl Pts',(1.10197749426139,0.434810365215498,4.12458130498915)) ;
#83667 = CARTESIAN_POINT('Ctrl Pts',(1.03802033559752,0.57089215321861,4.13358117941572)) ;
#83668 = CARTESIAN_POINT('Ctrl Pts',(0.858565778431052,0.817549425241584,
4.15334598837812)) ;
#83669 = CARTESIAN_POINT('Ctrl Pts',(0.74261499275234,0.924135312990195,4.16424512443554)) ;
#83670 = CARTESIAN_POINT('Ctrl Pts',(0.479479286439668,1.08366531170208,4.18605961067483)) ;
#83671 = CARTESIAN_POINT('Ctrl Pts',(0.33563429935706,1.1364834116783,4.19676539574625)) ;
#83672 = CARTESIAN_POINT('Ctrl Pts',(0.0362501517362821,1.18439204189214,
4.21684841980273)) ;
#83673 = CARTESIAN_POINT('Ctrl Pts',(-0.116378575296644,1.17921896890736,
4.22575548506318)) ;
#83674 = CARTESIAN_POINT('Ctrl Pts',(-0.415818103686213,1.11022378891706,
4.24658950691394)) ;
#83675 = CARTESIAN_POINT('Ctrl Pts',(-0.559267897367201,1.04532872852346,
4.25769919745631)) ;
#83676 = CARTESIAN_POINT('Ctrl Pts',(-0.807689818907504,0.86679618491432,
4.279283855629)) ;
#83677 = CARTESIAN_POINT('Ctrl Pts',(-0.911664654473727,0.75669555126946,
4.28957218732499)) ;
#83678 = CARTESIAN_POINT('Ctrl Pts',(-1.0761179660709,0.49770643017,4.30885301482668)) ;
#83679 = CARTESIAN_POINT('Ctrl Pts',(-1.13284157540801,0.349924032353012,
4.31893777077122)) ;
#83680 = CARTESIAN_POINT('Ctrl Pts',(-1.16979960242193,0.130620444338645,
4.33448803423816)) ;
#83681 = CARTESIAN_POINT('Ctrl Pts',(-1.17524047358084,0.065291328614083,
4.33912035681335)) ;
#83682 = CARTESIAN_POINT('Ctrl Pts',(-1.17524047358084,-3.71854203583437E-15,
4.34374999999999)) ;
#83683 = CARTESIAN_POINT('Origin',(0.,0.,0.)) ;
#83684 = CARTESIAN_POINT('',(-1.17524047358084,-2.89956199005216E-15,4.90624999999999)) ;
#83685 = CARTESIAN_POINT('',(-1.17524047358084,-1.37300533119257E-15,4.84374999999999)) ;
#83686 = CARTESIAN_POINT('',(-1.17524047358084,-1.4392544841992E-16,0.)) ;
#83687 = CARTESIAN_POINT('Ctrl Pts',(-1.17524047358084,-7.58582575310211E-15,
4.90624999999999)) ;
#83688 = CARTESIAN_POINT('Ctrl Pts',(-1.17524047358084,0.0336064111452372,
4.90386705427522)) ;
#83689 = CARTESIAN_POINT('Ctrl Pts',(-1.17379902465408,0.0672506944046495,
4.90148142313449)) ;
#83690 = CARTESIAN_POINT('Ctrl Pts',(-1.15753280327446,0.256125621332427,
4.88808877916264)) ;
#83691 = CARTESIAN_POINT('Ctrl Pts',(-1.11339784493106,0.407249272087715,
4.87737298282475)) ;
#83692 = CARTESIAN_POINT('Ctrl Pts',(-0.97191001713831,0.677324635980341,
4.85822262097939)) ;
#83693 = CARTESIAN_POINT('Ctrl Pts',(-0.878311667224519,0.794970991004644,
4.84866705058936)) ;
#83694 = CARTESIAN_POINT('Ctrl Pts',(-0.647858954275702,0.992651478855324,
4.82750697353716)) ;
#83695 = CARTESIAN_POINT('Ctrl Pts',(-0.511839952604746,1.06915809467643,
4.81644191761435)) ;
#83696 = CARTESIAN_POINT('Ctrl Pts',(-0.217789837788617,1.16521007102824,
4.79497958257196)) ;
#83697 = CARTESIAN_POINT('Ctrl Pts',(-0.0626683588253212,1.18372319582663,
4.78539906234046)) ;
#83698 = CARTESIAN_POINT('Ctrl Pts',(0.241755923350193,1.15992886988465,4.76586147754698)) ;
#83699 = CARTESIAN_POINT('Ctrl Pts',(0.388249083467121,1.11943010005734,4.75542984062084)) ;
#83700 = CARTESIAN_POINT('Ctrl Pts',(0.66320889718637,0.982766788481499,4.73369997296271)) ;
#83701 = CARTESIAN_POINT('Ctrl Pts',(0.78804277392843,0.885820221574825,4.7225970968929)) ;
#83702 = CARTESIAN_POINT('Ctrl Pts',(0.988365812490969,0.653391146675087,
4.70205524579088)) ;
#83703 = CARTESIAN_POINT('Ctrl Pts',(1.06373156815355,0.521787684346926,4.69324864666541)) ;
#83704 = CARTESIAN_POINT('Ctrl Pts',(1.16148270650949,0.235303024827453,4.6729347431169)) ;
#83705 = CARTESIAN_POINT('Ctrl Pts',(1.18216976652638,0.0829036082278015,
4.66212848544556)) ;
#83706 = CARTESIAN_POINT('Ctrl Pts',(1.16402721483696,-0.224794388844498,
4.64031039771591)) ;
#83707 = CARTESIAN_POINT('Ctrl Pts',(1.1239771417896,-0.377080091451739,4.62951220321653)) ;
#83708 = CARTESIAN_POINT('Ctrl Pts',(0.98983529323125,-0.650834129120896,
4.61010099590598)) ;
#83709 = CARTESIAN_POINT('Ctrl Pts',(0.899507015930689,-0.770887185367275,
4.6008224685601)) ;
#83710 = CARTESIAN_POINT('Ctrl Pts',(0.67489360591369,-0.974406537661227,
4.57981395995323)) ;
#83711 = CARTESIAN_POINT('Ctrl Pts',(0.541416377616256,-1.05442702615244,
4.56878040850312)) ;
#83712 = CARTESIAN_POINT('Ctrl Pts',(0.249309634015072,-1.15905825563868,
4.54713324478207)) ;
#83713 = CARTESIAN_POINT('Ctrl Pts',(0.0933474980749243,-1.18187483724993,
4.53721746569737)) ;
#83714 = CARTESIAN_POINT('Ctrl Pts',(-0.212535149674799,-1.16558942260184,
4.51785654503261)) ;
#83715 = CARTESIAN_POINT('Ctrl Pts',(-0.359634330439741,-1.12889840454129,
4.50752269281791)) ;
#83716 = CARTESIAN_POINT('Ctrl Pts',(-0.637312589759921,-0.999690819910851,
4.48589022512135)) ;
#83717 = CARTESIAN_POINT('Ctrl Pts',(-0.764307844796796,-0.906307054685691,
4.47478093847204)) ;
#83718 = CARTESIAN_POINT('Ctrl Pts',(-0.970971990849064,-0.679123640590144,
4.45403567298827)) ;
#83719 = CARTESIAN_POINT('Ctrl Pts',(-1.05008805783472,-0.548916067448755,
4.44517225178508)) ;
#83720 = CARTESIAN_POINT('Ctrl Pts',(-1.15062478854163,-0.276774697313999,
4.4258753946558)) ;
#83721 = CARTESIAN_POINT('Ctrl Pts',(-1.17524047358084,-0.138870815676883,
4.41609697875304)) ;
#83722 = CARTESIAN_POINT('Ctrl Pts',(-1.17524047358084,4.85722573273506E-16,
4.40624999999999)) ;
#83723 = CARTESIAN_POINT('Ctrl Pts',(-1.17524047358084,-3.71854203583437E-15,
4.34374999999999)) ;
#83724 = CARTESIAN_POINT('Ctrl Pts',(-1.17524047358084,-0.0879429296864962,
4.3499858110009)) ;
#83725 = CARTESIAN_POINT('Ctrl Pts',(-1.16536913559801,-0.175817305099971,
4.35621676099149)) ;
#83726 = CARTESIAN_POINT('Ctrl Pts',(-1.11247180243315,-0.407170807428106,
4.37262145344443)) ;
#83727 = CARTESIAN_POINT('Ctrl Pts',(-1.05198089044729,-0.544702587945109,
4.38179537625786)) ;
#83728 = CARTESIAN_POINT('Ctrl Pts',(-0.878873963396262,-0.795674243273616,
4.40132335303172)) ;
#83729 = CARTESIAN_POINT('Ctrl Pts',(-0.765658722969771,-0.905131200820453,
4.41215629577215)) ;
#83730 = CARTESIAN_POINT('Ctrl Pts',(-0.506336955375604,-1.07143189443511,
4.4339766233431)) ;
#83731 = CARTESIAN_POINT('Ctrl Pts',(-0.363491689914812,-1.12793145483258,
4.44475153936484)) ;
#83732 = CARTESIAN_POINT('Ctrl Pts',(-0.0657158903894447,-1.18303025212162,
4.4649907167986)) ;
#83733 = CARTESIAN_POINT('Ctrl Pts',(0.0862480431561069,-1.18171108530207,
4.47381688433456)) ;
#83734 = CARTESIAN_POINT('Ctrl Pts',(0.387064954368621,-1.12062857541088,
4.49445495433573)) ;
#83735 = CARTESIAN_POINT('Ctrl Pts',(0.532509355951195,-1.05926876454441,
4.50556179130252)) ;
#83736 = CARTESIAN_POINT('Ctrl Pts',(0.785966327506931,-0.886603103199955,
4.52724763728332)) ;
#83737 = CARTESIAN_POINT('Ctrl Pts',(0.892885955994929,-0.778834630601013,
4.53763411803812)) ;
#83738 = CARTESIAN_POINT('Ctrl Pts',(1.06300065633516,-0.524734283547396,
4.55708927294375)) ;
#83739 = CARTESIAN_POINT('Ctrl Pts',(1.12298496714204,-0.379795602326755,
4.56681965319974)) ;
#83740 = CARTESIAN_POINT('Ctrl Pts',(1.18290300104997,-0.0758824019829007,
4.58836937055374)) ;
#83741 = CARTESIAN_POINT('Ctrl Pts',(1.18263352169829,0.0799734538844092,
4.59942071560261)) ;
#83742 = CARTESIAN_POINT('Ctrl Pts',(1.12292510957113,0.377398239203149,4.62051035583687)) ;
#83743 = CARTESIAN_POINT('Ctrl Pts',(1.06610382786025,0.516513514215964,4.6299287115176)) ;
#83744 = CARTESIAN_POINT('Ctrl Pts',(0.899751763152944,0.771982532616731,
4.64920133623562)) ;
#83745 = CARTESIAN_POINT('Ctrl Pts',(0.789510436318703,0.884398262703763,
4.65995655740372)) ;
#83746 = CARTESIAN_POINT('Ctrl Pts',(0.534415846616042,1.05776313639872,4.6817677553963)) ;
#83747 = CARTESIAN_POINT('Ctrl Pts',(0.392729941126095,1.11813973013556,4.69260893313949)) ;
#83748 = CARTESIAN_POINT('Ctrl Pts',(0.0966996952851368,1.1808222055235,4.71300978991082)) ;
#83749 = CARTESIAN_POINT('Ctrl Pts',(-0.0546006167114424,1.18351564863586,
4.72180951098071)) ;
#83750 = CARTESIAN_POINT('Ctrl Pts',(-0.356770105579204,1.13069703761872,
4.74223765353203)) ;
#83751 = CARTESIAN_POINT('Ctrl Pts',(-0.504206792548302,1.07309022025021,
4.75333377446551)) ;
#83752 = CARTESIAN_POINT('Ctrl Pts',(-0.762774838742479,0.906695985440486,
4.77511113414352)) ;
#83753 = CARTESIAN_POINT('Ctrl Pts',(-0.872713039004967,0.801444885450279,
4.78559372810281)) ;
#83754 = CARTESIAN_POINT('Ctrl Pts',(-1.04867033163315,0.552459444916847,
4.80522632045929)) ;
#83755 = CARTESIAN_POINT('Ctrl Pts',(-1.11198000105894,0.410409566754714,
4.81464889431279)) ;
#83756 = CARTESIAN_POINT('Ctrl Pts',(-1.16550862440625,0.17457751663472,4.83137114927687)) ;
#83757 = CARTESIAN_POINT('Ctrl Pts',(-1.17524047358084,0.0873194511436137,
4.83755839828765)) ;
#83758 = CARTESIAN_POINT('Ctrl Pts',(-1.17524047358084,0.,4.84374999999999)) ;
#83759 = CARTESIAN_POINT('Origin',(0.,0.,0.)) ;
#83760 = CARTESIAN_POINT('',(-1.17524047358084,-3.06002391158001E-15,5.40624999999999)) ;
#83761 = CARTESIAN_POINT('',(-1.17524047358084,4.2243346644343E-16,5.34374999999999)) ;
#83762 = CARTESIAN_POINT('',(-1.17524047358084,-1.4392544841992E-16,0.)) ;
#83763 = CARTESIAN_POINT('Ctrl Pts',(-1.17524047358084,-1.50972806654875E-14,
5.40625)) ;
#83764 = CARTESIAN_POINT('Ctrl Pts',(-1.17524047358084,0.054156322179546,
5.40240991199269)) ;
#83765 = CARTESIAN_POINT('Ctrl Pts',(-1.17149719619506,0.108363865139321,
5.39856619204925)) ;
#83766 = CARTESIAN_POINT('Ctrl Pts',(-1.14245991904882,0.316700694650271,
5.38379355372584)) ;
#83767 = CARTESIAN_POINT('Ctrl Pts',(-1.09041023303251,0.465258281745517,
5.37338107781476)) ;
#83768 = CARTESIAN_POINT('Ctrl Pts',(-0.934665993484623,0.727999724774848,
5.3545020203338)) ;
#83769 = CARTESIAN_POINT('Ctrl Pts',(-0.834492771222264,0.840941110532362,
5.34434642158922)) ;
#83770 = CARTESIAN_POINT('Ctrl Pts',(-0.592638212946615,1.02670227320812,
5.32290876835838)) ;
#83771 = CARTESIAN_POINT('Ctrl Pts',(-0.451833533797191,1.09598812006894,
5.3118058383577)) ;
#83772 = CARTESIAN_POINT('Ctrl Pts',(-0.154264542505518,1.1750060408126,5.29073133822417)) ;
#83773 = CARTESIAN_POINT('Ctrl Pts',(-0.000747491529236952,1.18508632964804,
5.28164497410758)) ;
#83774 = CARTESIAN_POINT('Ctrl Pts',(0.300584332058249,1.14619222074689,5.26176194626849)) ;
#83775 = CARTESIAN_POINT('Ctrl Pts',(0.445545839603115,1.09798914509645,5.25115121813143)) ;
#83776 = CARTESIAN_POINT('Ctrl Pts',(0.714383924244483,0.94635903855499,5.22926664280317)) ;
#83777 = CARTESIAN_POINT('Ctrl Pts',(0.834531897528456,0.842326220849121,
5.21820028309222)) ;
#83778 = CARTESIAN_POINT('Ctrl Pts',(1.02183521132734,0.599452713433834,5.19808764883802)) ;
#83779 = CARTESIAN_POINT('Ctrl Pts',(1.08964832106457,0.464933155992749,5.18921723567391)) ;
#83780 = CARTESIAN_POINT('Ctrl Pts',(1.17234517244266,0.173941348274813,5.16858374163167)) ;
#83781 = CARTESIAN_POINT('Ctrl Pts',(1.18500959824535,0.0198512012903376,
5.15765759853952)) ;
#83782 = CARTESIAN_POINT('Ctrl Pts',(1.15022464875196,-0.287150503762624,
5.13588888311813)) ;
#83783 = CARTESIAN_POINT('Ctrl Pts',(1.10205516619926,-0.437004301439408,
5.12526312885439)) ;
#83784 = CARTESIAN_POINT('Ctrl Pts',(0.953281888395458,-0.70334467726024,
5.10637760557866)) ;
#83785 = CARTESIAN_POINT('Ctrl Pts',(0.856368474205286,-0.818609396179132,
5.09648150034986)) ;
#83786 = CARTESIAN_POINT('Ctrl Pts',(0.620045591679404,-1.01032312726072,
5.07517249366432)) ;
#83787 = CARTESIAN_POINT('Ctrl Pts',(0.481550303729629,-1.08319994735702,
5.06408406458446)) ;
#83788 = CARTESIAN_POINT('Ctrl Pts',(0.185657123836112,-1.17059619417369,
5.0428154291615)) ;
#83789 = CARTESIAN_POINT('Ctrl Pts',(0.0313637348566941,-1.18480750453488,
5.03351516099886)) ;
#83790 = CARTESIAN_POINT('Ctrl Pts',(-0.27152252717408,-1.15337354604257,
5.01380116892149)) ;
#83791 = CARTESIAN_POINT('Ctrl Pts',(-0.417293433366323,-1.10898293008958,
5.00327590343977)) ;
#83792 = CARTESIAN_POINT('Ctrl Pts',(-0.689265529178068,-0.964739169361853,
4.98146074933774)) ;
#83793 = CARTESIAN_POINT('Ctrl Pts',(-0.811785020904053,-0.864192363580381,
4.97037235234583)) ;
#83794 = CARTESIAN_POINT('Ctrl Pts',(-1.00556637310702,-0.626460634302472,
4.9500442120722)) ;
#83795 = CARTESIAN_POINT('Ctrl Pts',(-1.07711222144063,-0.493404919958927,
4.9412360965373)) ;
#83796 = CARTESIAN_POINT('Ctrl Pts',(-1.15727203498349,-0.236821733408562,
4.92304243090614)) ;
#83797 = CARTESIAN_POINT('Ctrl Pts',(-1.17524047358084,-0.118646891707225,
4.91466295138983)) ;
#83798 = CARTESIAN_POINT('Ctrl Pts',(-1.17524047358084,-5.27355936696949E-15,
4.90624999999999)) ;
#83799 = CARTESIAN_POINT('Ctrl Pts',(-1.17524047358084,0.,4.84374999999999)) ;
#83800 = CARTESIAN_POINT('Ctrl Pts',(-1.17524047358084,-0.0667390125405247,
4.84848229479701)) ;
#83801 = CARTESIAN_POINT('Ctrl Pts',(-1.16955564460581,-0.133513884598031,
4.8532171323018)) ;
#83802 = CARTESIAN_POINT('Ctrl Pts',(-1.13283143136164,-0.346611060159256,
4.86832731473904)) ;
#83803 = CARTESIAN_POINT('Ctrl Pts',(-1.07974815915801,-0.487390792329828,
4.87805833554934)) ;
#83804 = CARTESIAN_POINT('Ctrl Pts',(-0.920300351277828,-0.747361772037844,
4.89706659726841)) ;
#83805 = CARTESIAN_POINT('Ctrl Pts',(-0.813160901989492,-0.86269717468872,
4.9077348526552)) ;
#83806 = CARTESIAN_POINT('Ctrl Pts',(-0.562558857002137,-1.04312657461033,
4.92952063778222)) ;
#83807 = CARTESIAN_POINT('Ctrl Pts',(-0.422157008304024,-1.10741905073089,
4.94042179724895)) ;
#83808 = CARTESIAN_POINT('Ctrl Pts',(-0.127949644136201,-1.17778450934342,
4.96098310556376)) ;
#83809 = CARTESIAN_POINT('Ctrl Pts',(0.022723984492035,-1.18449444420266,
4.96981733918665)) ;
#83810 = CARTESIAN_POINT('Ctrl Pts',(0.326162761302332,-1.13996195065271,
4.99002965192844)) ;
#83811 = CARTESIAN_POINT('Ctrl Pts',(0.475501214059982,-1.08617584423663,
5.00110709739386)) ;
#83812 = CARTESIAN_POINT('Ctrl Pts',(0.739036042438915,-0.92620970159878,
5.02296155572285)) ;
#83813 = CARTESIAN_POINT('Ctrl Pts',(0.85193851793381,-0.823563331821022,
5.03353383150877)) ;
#83814 = CARTESIAN_POINT('Ctrl Pts',(1.03368402663923,-0.579715396745444,
5.0533397209827)) ;
#83815 = CARTESIAN_POINT('Ctrl Pts',(1.10025481630781,-0.44047762754836,5.06251684407359)) ;
#83816 = CARTESIAN_POINT('Ctrl Pts',(1.17691073218495,-0.142002365400373,
5.08368097096632)) ;
#83817 = CARTESIAN_POINT('Ctrl Pts',(1.18535584236089,0.0145014606441104,
5.09477826194369)) ;
#83818 = CARTESIAN_POINT('Ctrl Pts',(1.14176601862325,0.316099164561747,5.11616379329503)) ;
#83819 = CARTESIAN_POINT('Ctrl Pts',(1.09234347057307,0.458558371862131,5.12626266972199)) ;
#83820 = CARTESIAN_POINT('Ctrl Pts',(0.939666462827153,0.722855780487681,
5.145008540428)) ;
#83821 = CARTESIAN_POINT('Ctrl Pts',(0.835624990096788,0.840950188579383,
5.15558437333414)) ;
#83822 = CARTESIAN_POINT('Ctrl Pts',(0.589589205037277,1.02814885579379,5.1773297508833)) ;
#83823 = CARTESIAN_POINT('Ctrl Pts',(0.450540903554148,1.09623183439873,5.18828217964236)) ;
#83824 = CARTESIAN_POINT('Ctrl Pts',(0.158161311409111,1.17406763505529,5.20899610027115)) ;
#83825 = CARTESIAN_POINT('Ctrl Pts',(0.00804861590346991,1.18464228572274,
5.21792242384493)) ;
#83826 = CARTESIAN_POINT('Ctrl Pts',(-0.296530748862871,1.14808352384729,
5.23792207885416)) ;
#83827 = CARTESIAN_POINT('Ctrl Pts',(-0.447606380953899,1.09802387470485,
5.24897408362528)) ;
#83828 = CARTESIAN_POINT('Ctrl Pts',(-0.715765400545716,0.94436759315512,
5.27088879462436)) ;
#83829 = CARTESIAN_POINT('Ctrl Pts',(-0.831457772948567,0.844300644444529,
5.28154094137343)) ;
#83830 = CARTESIAN_POINT('Ctrl Pts',(-1.01870853473459,0.605404657890455,
5.30150933055223)) ;
#83831 = CARTESIAN_POINT('Ctrl Pts',(-1.08835654108605,0.468792762534213,
5.31050908937556)) ;
#83832 = CARTESIAN_POINT('Ctrl Pts',(-1.1601035158885,0.217504967293211,5.32832727218508)) ;
#83833 = CARTESIAN_POINT('Ctrl Pts',(-1.17524047358084,0.108898732755448,
5.33602826593765)) ;
#83834 = CARTESIAN_POINT('Ctrl Pts',(-1.17524047358084,6.17561557447743E-15,
5.34374999999999)) ;
#83835 = CARTESIAN_POINT('Origin',(0.,0.,0.)) ;
#83836 = CARTESIAN_POINT('',(-1.17524047358084,-2.2495827876471E-15,5.90624999999999)) ;
#83837 = CARTESIAN_POINT('',(-1.17524047358084,1.83623309936453E-15,5.84374999999999)) ;
#83838 = CARTESIAN_POINT('',(-1.17524047358084,-1.4392544841992E-16,0.)) ;
#83839 = CARTESIAN_POINT('Ctrl Pts',(-1.17524047358084,-7.58582575310211E-15,
5.90624999999999)) ;
#83840 = CARTESIAN_POINT('Ctrl Pts',(-1.17524047358084,0.0749412078928489,
5.90093610824922)) ;
#83841 = CARTESIAN_POINT('Ctrl Pts',(-1.16807236315843,0.149890538220418,
5.89562164055712)) ;
#83842 = CARTESIAN_POINT('Ctrl Pts',(-1.12410951984973,0.37651515556659,5.87955226139312)) ;
#83843 = CARTESIAN_POINT('Ctrl Pts',(-1.06448232899237,0.521764927946688,
5.86978553376752)) ;
#83844 = CARTESIAN_POINT('Ctrl Pts',(-0.894991089303138,0.776406902522572,
5.85034946141045)) ;
#83845 = CARTESIAN_POINT('Ctrl Pts',(-0.788394897908854,0.88443736721281,
5.8399735535765)) ;
#83846 = CARTESIAN_POINT('Ctrl Pts',(-0.535488632620262,1.05775927797598,
5.81829825869221)) ;
#83847 = CARTESIAN_POINT('Ctrl Pts',(-0.390260895491309,1.11951332927642,
5.80719074928886)) ;
#83848 = CARTESIAN_POINT('Ctrl Pts',(-0.0895922589655112,1.18147183035352,
5.78653072733016)) ;
#83849 = CARTESIAN_POINT('Ctrl Pts',(0.0624435431070185,1.18321696626138,
5.77769828374712)) ;
#83850 = CARTESIAN_POINT('Ctrl Pts',(0.360400561462412,1.1289174745997,5.75747631645805)) ;
#83851 = CARTESIAN_POINT('Ctrl Pts',(0.503361754371328,1.07282701451939,5.74670878573645)) ;
#83852 = CARTESIAN_POINT('Ctrl Pts',(0.763116910540795,0.907275709569743,
5.72488841340987)) ;
#83853 = CARTESIAN_POINT('Ctrl Pts',(0.876640368697243,0.798134855960196,
5.71404775080149)) ;
#83854 = CARTESIAN_POINT('Ctrl Pts',(1.05045573515797,0.547640396735084,5.69449318879659)) ;
#83855 = CARTESIAN_POINT('Ctrl Pts',(1.11133252962224,0.410272222105063,5.68534136692503)) ;
#83856 = CARTESIAN_POINT('Ctrl Pts',(1.17966470128619,0.115195906161128,5.66441825072192)) ;
#83857 = CARTESIAN_POINT('Ctrl Pts',(1.18459572722913,-0.0401138114626467,
5.65340563095636)) ;
#83858 = CARTESIAN_POINT('Ctrl Pts',(1.13382399717879,-0.346797007312973,
5.63165950021797)) ;
#83859 = CARTESIAN_POINT('Ctrl Pts',(1.07744306071906,-0.494878503776931,
5.6215346463652)) ;
#83860 = CARTESIAN_POINT('Ctrl Pts',(0.913580515513978,-0.754373946827181,
5.60227214544814)) ;
#83861 = CARTESIAN_POINT('Ctrl Pts',(0.809913879086464,-0.864711878274894,
5.59199432645043)) ;
#83862 = CARTESIAN_POINT('Ctrl Pts',(0.56202160582472,-1.04384466298271,5.57042091195641)) ;
#83863 = CARTESIAN_POINT('Ctrl Pts',(0.418783365136616,-1.1091028100288,5.55931133961254)) ;
#83864 = CARTESIAN_POINT('Ctrl Pts',(0.119491572437825,-1.17891825992327,
5.53845730823343)) ;
#83865 = CARTESIAN_POINT('Ctrl Pts',(-0.033208005507292,-1.18449175161955,
5.52953876600849)) ;
#83866 = CARTESIAN_POINT('Ctrl Pts',(-0.332755258580171,-1.13732471487981,
5.50947201828561)) ;
#83867 = CARTESIAN_POINT('Ctrl Pts',(-0.476697840529487,-1.08488640619213,
5.49877370516092)) ;
#83868 = CARTESIAN_POINT('Ctrl Pts',(-0.740216032869487,-0.926058330823341,
5.47696061715002)) ;
#83869 = CARTESIAN_POINT('Ctrl Pts',(-0.85644416733711,-0.819772004395771,
5.46605507031694)) ;
#83870 = CARTESIAN_POINT('Ctrl Pts',(-1.03655016378708,-0.573562522277988,
5.44626613380904)) ;
#83871 = CARTESIAN_POINT('Ctrl Pts',(-1.1008642792567,-0.437627573512256,
5.43728106579391)) ;
#83872 = CARTESIAN_POINT('Ctrl Pts',(-1.16280481815703,-0.197241280534875,
5.42023588097279)) ;
#83873 = CARTESIAN_POINT('Ctrl Pts',(-1.17524047358084,-0.0987057153674117,
5.41324897294683)) ;
#83874 = CARTESIAN_POINT('Ctrl Pts',(-1.17524047358084,-1.50972806654875E-14,
5.40625)) ;
#83875 = CARTESIAN_POINT('Ctrl Pts',(-1.17524047358084,7.69738201417715E-15,
5.34374999999999)) ;
#83876 = CARTESIAN_POINT('Ctrl Pts',(-1.17524047358084,-0.0460814382391025,
5.34701751838417)) ;
#83877 = CARTESIAN_POINT('Ctrl Pts',(-1.17253025465147,-0.0922152521519931,
5.35028875059508)) ;
#83878 = CARTESIAN_POINT('Ctrl Pts',(-1.14948489675735,-0.286885631866481,
5.36409233548477)) ;
#83879 = CARTESIAN_POINT('Ctrl Pts',(-1.10360733284383,-0.430921057723322,
5.37430552369991)) ;
#83880 = CARTESIAN_POINT('Ctrl Pts',(-0.957309780951295,-0.699307780007639,
5.39333614823432)) ;
#83881 = CARTESIAN_POINT('Ctrl Pts',(-0.85622111678967,-0.820002489146776,
5.40357693887794)) ;
#83882 = CARTESIAN_POINT('Ctrl Pts',(-0.614454492851251,-1.01354027017214,
5.42528490244742)) ;
#83883 = CARTESIAN_POINT('Ctrl Pts',(-0.476760246395516,-1.08513670825354,
5.43627874710529)) ;
#83884 = CARTESIAN_POINT('Ctrl Pts',(-0.186134534229494,-1.16993609825664,
5.45713185130973)) ;
#83885 = CARTESIAN_POINT('Ctrl Pts',(-0.0365019681565856,-1.18408252796803,
5.46619501517522)) ;
#83886 = CARTESIAN_POINT('Ctrl Pts',(0.267071427811465,-1.15507276534244,
5.48586525574657)) ;
#83887 = CARTESIAN_POINT('Ctrl Pts',(0.417813971737475,-1.10947363824431,
5.49673866417285)) ;
#83888 = CARTESIAN_POINT('Ctrl Pts',(0.689147490984914,-0.964028909960287,
5.51855718356141)) ;
#83889 = CARTESIAN_POINT('Ctrl Pts',(0.807898497105404,-0.866942506731837,
5.52929148241646)) ;
#83890 = CARTESIAN_POINT('Ctrl Pts',(1.00126331908508,-0.633622414306119,
5.5494376355253)) ;
#83891 = CARTESIAN_POINT('Ctrl Pts',(1.07430845771922,-0.499868779088293,
5.55830556753948)) ;
#83892 = CARTESIAN_POINT('Ctrl Pts',(1.16732151556813,-0.207153881912603,
5.57906124150266)) ;
#83893 = CARTESIAN_POINT('Ctrl Pts',(1.18448062330524,-0.0504791232455658,
5.59017065288052)) ;
#83894 = CARTESIAN_POINT('Ctrl Pts',(1.15713436045325,0.254524452443586,5.61179768599597)) ;
#83895 = CARTESIAN_POINT('Ctrl Pts',(1.11517443295985,0.400187610684816,5.62212629260286)) ;
#83896 = CARTESIAN_POINT('Ctrl Pts',(0.975960647319752,0.673101398981301,
5.64147791995286)) ;
#83897 = CARTESIAN_POINT('Ctrl Pts',(0.878001633002891,0.796685571300439,
5.65141277616985)) ;
#83898 = CARTESIAN_POINT('Ctrl Pts',(0.640998731844676,0.997026504127541,
5.67306940775951)) ;
#83899 = CARTESIAN_POINT('Ctrl Pts',(0.504870832789386,1.07240301387313,5.68410108433379)) ;
#83900 = CARTESIAN_POINT('Ctrl Pts',(0.216201394429409,1.16474743402637,5.70510155782909)) ;
#83901 = CARTESIAN_POINT('Ctrl Pts',(0.0670433973381126,1.18273596616217,
5.71436727770251)) ;
#83902 = CARTESIAN_POINT('Ctrl Pts',(-0.237077617719062,1.16159741992614,
5.73379208225248)) ;
#83903 = CARTESIAN_POINT('Ctrl Pts',(-0.388928202532001,1.11992285024332,
5.74459439266565)) ;
#83904 = CARTESIAN_POINT('Ctrl Pts',(-0.664259586879038,0.981402662111225,
5.76641291082476)) ;
#83905 = CARTESIAN_POINT('Ctrl Pts',(-0.785749458649678,0.887130828527359,
5.7772156100363)) ;
#83906 = CARTESIAN_POINT('Ctrl Pts',(-0.984673026824418,0.658950965260441,
5.79752087248553)) ;
#83907 = CARTESIAN_POINT('Ctrl Pts',(-1.06079452208989,0.527742519535345,
5.80632911101323)) ;
#83908 = CARTESIAN_POINT('Ctrl Pts',(-1.15329706571952,0.261507134193389,
5.82520718967931)) ;
#83909 = CARTESIAN_POINT('Ctrl Pts',(-1.17524047358084,0.131114627104794,
5.83445299298652)) ;
#83910 = CARTESIAN_POINT('Ctrl Pts',(-1.17524047358084,-1.04083408558608E-16,
5.84374999999999)) ;
#83911 = CARTESIAN_POINT('Origin',(0.,0.,0.)) ;
#83912 = CARTESIAN_POINT('',(-1.17524047358084,-2.72175283376453E-15,6.40624999999999)) ;
#83913 = CARTESIAN_POINT('',(-1.17524047358084,4.94679191084167E-17,6.34374999999999)) ;
#83914 = CARTESIAN_POINT('',(-1.17524047358084,-1.4392544841992E-16,0.)) ;
#83915 = CARTESIAN_POINT('Ctrl Pts',(-1.17524047358084,1.90683135537553E-30,
6.40624999999999)) ;
#83916 = CARTESIAN_POINT('Ctrl Pts',(-1.17524047358084,0.0972130928115972,
6.39935686514824)) ;
#83917 = CARTESIAN_POINT('Ctrl Pts',(-1.16317811940475,0.194278275973553,
6.39247421819613)) ;
#83918 = CARTESIAN_POINT('Ctrl Pts',(-1.10153824254022,0.437298694669516,
6.37524225417408)) ;
#83919 = CARTESIAN_POINT('Ctrl Pts',(-1.03531235227418,0.576832605858214,
6.36604191838211)) ;
#83920 = CARTESIAN_POINT('Ctrl Pts',(-0.854181441061047,0.82122938275905,
6.34625431141678)) ;
#83921 = CARTESIAN_POINT('Ctrl Pts',(-0.74159230416404,0.924157550836251,
6.33569128622248)) ;
#83922 = CARTESIAN_POINT('Ctrl Pts',(-0.478579939800903,1.08481631082732,
6.31384435531985)) ;
#83923 = CARTESIAN_POINT('Ctrl Pts',(-0.329439848447114,1.13901287968353,
6.30276453833942)) ;
#83924 = CARTESIAN_POINT('Ctrl Pts',(-0.0261324283789686,1.18442992169236,
6.28252893136117)) ;
#83925 = CARTESIAN_POINT('Ctrl Pts',(0.124605997283236,1.17814861438563,6.27370134002346)) ;
#83926 = CARTESIAN_POINT('Ctrl Pts',(0.419011611408069,1.10860715347419,6.25315707143774)) ;
#83927 = CARTESIAN_POINT('Ctrl Pts',(0.559556434964203,1.04473390860149,6.24226199553197)) ;
#83928 = CARTESIAN_POINT('Ctrl Pts',(0.810650286515072,0.865057396938094,
6.22047270241022)) ;
#83929 = CARTESIAN_POINT('Ctrl Pts',(0.918126580154595,0.750031227263427,
6.20979472566)) ;
#83930 = CARTESIAN_POINT('Ctrl Pts',(1.07831776895032,0.490540515161358,6.19075784192955)) ;
#83931 = CARTESIAN_POINT('Ctrl Pts',(1.1318031266677,0.349942297815048,6.18106352438655)) ;
#83932 = CARTESIAN_POINT('Ctrl Pts',(1.18430248810267,0.0506155938961819,
6.15983902390858)) ;
#83933 = CARTESIAN_POINT('Ctrl Pts',(1.18067233732404,-0.105589764350431,
6.14876289652883)) ;
#83934 = CARTESIAN_POINT('Ctrl Pts',(1.11321071305007,-0.407110440650127,
6.1273828270113)) ;
#83935 = CARTESIAN_POINT('Ctrl Pts',(1.05025894768157,-0.549470383003391,
6.11792984709037)) ;
#83936 = CARTESIAN_POINT('Ctrl Pts',(0.874933559125881,-0.799012447392118,
6.09831632409727)) ;
#83937 = CARTESIAN_POINT('Ctrl Pts',(0.765320654280662,-0.904541234041102,
6.0878438607431)) ;
#83938 = CARTESIAN_POINT('Ctrl Pts',(0.507300872470456,-1.07162431480738,
6.06607574654216)) ;
#83939 = CARTESIAN_POINT('Ctrl Pts',(0.360076243292598,-1.12964209827539,
6.05497807730034)) ;
#83940 = CARTESIAN_POINT('Ctrl Pts',(0.0580496940573428,-1.18335930321019,
6.03452685382692)) ;
#83941 = CARTESIAN_POINT('Ctrl Pts',(-0.0933211913583464,-1.18110174006449,
6.02572716652203)) ;
#83942 = CARTESIAN_POINT('Ctrl Pts',(-0.389544578689132,-1.11924768487494,
6.00534381997293)) ;
#83943 = CARTESIAN_POINT('Ctrl Pts',(-0.531362360870357,-1.05929413324628,
5.99450954241255)) ;
#83944 = CARTESIAN_POINT('Ctrl Pts',(-0.78692880581635,-0.886696722849366,
5.97269657832903)) ;
#83945 = CARTESIAN_POINT('Ctrl Pts',(-0.897499306377748,-0.774600571175226,
5.96193247361706)) ;
#83946 = CARTESIAN_POINT('Ctrl Pts',(-1.06459217294446,-0.519620206308922,
5.94263168257401)) ;
#83947 = CARTESIAN_POINT('Ctrl Pts',(-1.1218151619999,-0.380680717852885,
5.93324310810642)) ;
#83948 = CARTESIAN_POINT('Ctrl Pts',(-1.16734732758849,-0.157270511476844,
5.91740165470473)) ;
#83949 = CARTESIAN_POINT('Ctrl Pts',(-1.17524047358084,-0.0786397277081866,
5.91182614444844)) ;
#83950 = CARTESIAN_POINT('Ctrl Pts',(-1.17524047358084,-7.58582575310211E-15,
5.90624999999999)) ;
#83951 = CARTESIAN_POINT('Ctrl Pts',(-1.17524047358084,0.,5.84374999999999)) ;
#83952 = CARTESIAN_POINT('Ctrl Pts',(-1.17524047358084,-0.0249351682621398,
5.84551808979542)) ;
#83953 = CARTESIAN_POINT('Ctrl Pts',(-1.17444690966321,-0.049896454030164,
5.84728803151721)) ;
#83954 = CARTESIAN_POINT('Ctrl Pts',(-1.16326691459726,-0.225088989663869,
5.85971049168401)) ;
#83955 = CARTESIAN_POINT('Ctrl Pts',(-1.12489655565861,-0.372132512664032,
5.87013697646916)) ;
#83956 = CARTESIAN_POINT('Ctrl Pts',(-0.992898546841716,-0.647535079178023,
5.88966507679593)) ;
#83957 = CARTESIAN_POINT('Ctrl Pts',(-0.899082365125593,-0.772540989574306,
5.89926224179742)) ;
#83958 = CARTESIAN_POINT('Ctrl Pts',(-0.668523936196988,-0.978850247286171,
5.92073473275935)) ;
#83959 = CARTESIAN_POINT('Ctrl Pts',(-0.534159183145627,-1.05818012315957,
5.93179830024191)) ;
#83960 = CARTESIAN_POINT('Ctrl Pts',(-0.247619332292761,-1.15848698536751,
5.95295029904875)) ;
#83961 = CARTESIAN_POINT('Ctrl Pts',(-0.0989124286993728,-1.18050496089781,
5.96248937209396)) ;
#83962 = CARTESIAN_POINT('Ctrl Pts',(0.205699478839078,-1.16755936647318,
5.98165385045049)) ;
#83963 = CARTESIAN_POINT('Ctrl Pts',(0.358591230794876,-1.12999795665931,
5.9923742696277)) ;
#83964 = CARTESIAN_POINT('Ctrl Pts',(0.637893753861499,-0.998801759709271,
6.01417698332077)) ;
#83965 = CARTESIAN_POINT('Ctrl Pts',(0.762164334503225,-0.907539621260408,
6.02504373445584)) ;
#83966 = CARTESIAN_POINT('Ctrl Pts',(0.966831430978108,-0.684736450733742,
6.04551106976708)) ;
#83967 = CARTESIAN_POINT('Ctrl Pts',(1.04611887486588,-0.556111465096944,
6.05431754074319)) ;
#83968 = CARTESIAN_POINT('Ctrl Pts',(1.15469189529256,-0.269263414025172,
6.07465721146874)) ;
#83969 = CARTESIAN_POINT('Ctrl Pts',(1.18028032062798,-0.112871287684847,
6.08574658210224)) ;
#83970 = CARTESIAN_POINT('Ctrl Pts',(1.16878242538718,0.194726490535913,6.10755756356628)) ;
#83971 = CARTESIAN_POINT('Ctrl Pts',(1.13414049508146,0.343095127788057,6.11807800885581)) ;
#83972 = CARTESIAN_POINT('Ctrl Pts',(1.00952700365956,0.620988342124133,6.13778271472828)) ;
#83973 = CARTESIAN_POINT('Ctrl Pts',(0.919855079768746,0.74742876887245,6.14709631564413)) ;
#83974 = CARTESIAN_POINT('Ctrl Pts',(0.695871898043459,0.959670786413457,
6.16837537447728)) ;
#83975 = CARTESIAN_POINT('Ctrl Pts',(0.563407357950225,1.04296430140369,6.17946278012117)) ;
#83976 = CARTESIAN_POINT('Ctrl Pts',(0.279096880839658,1.15134179026669,6.20076401214732)) ;
#83977 = CARTESIAN_POINT('Ctrl Pts',(0.130797737839273,1.1774241662368,6.21064059511467)) ;
#83978 = CARTESIAN_POINT('Ctrl Pts',(-0.174226850731518,1.17266526439425,
6.22954016640769)) ;
#83979 = CARTESIAN_POINT('Ctrl Pts',(-0.328043409459078,1.13923669513064,
6.24017085117553)) ;
#83980 = CARTESIAN_POINT('Ctrl Pts',(-0.611114743371182,1.0154674591827,6.26194168525353)) ;
#83981 = CARTESIAN_POINT('Ctrl Pts',(-0.738088625482068,0.927290495646206,
6.27286505886348)) ;
#83982 = CARTESIAN_POINT('Ctrl Pts',(-0.948448644284149,0.709892127722752,
6.29349036284195)) ;
#83983 = CARTESIAN_POINT('Ctrl Pts',(-1.0308750732841,0.583774691885055,6.30235601120873)) ;
#83984 = CARTESIAN_POINT('Ctrl Pts',(-1.14546161092712,0.304105800060345,
6.32218662588658)) ;
#83985 = CARTESIAN_POINT('Ctrl Pts',(-1.17524047358084,0.152744487257788,
6.33291927423992)) ;
#83986 = CARTESIAN_POINT('Ctrl Pts',(-1.17524047358084,-7.28583859910259E-15,
6.34374999999999)) ;
#83987 = CARTESIAN_POINT('Origin',(0.,0.,0.)) ;
#83988 = CARTESIAN_POINT('',(-1.17524047358084,-4.25264630131406E-15,6.90624999999999)) ;
#83989 = CARTESIAN_POINT('',(-1.17524047358084,3.5883038101011E-15,6.84374999999999)) ;
#83990 = CARTESIAN_POINT('',(-1.17524047358084,-1.4392544841992E-16,0.)) ;
#83991 = CARTESIAN_POINT('Ctrl Pts',(-1.17524047358084,-5.759281940243E-15,
6.90624999999999)) ;
#83992 = CARTESIAN_POINT('Ctrl Pts',(-1.17524047358084,0.119521171290162,
6.89777505565335)) ;
#83993 = CARTESIAN_POINT('Ctrl Pts',(-1.15700615440808,0.238572139687923,
6.8893334522061)) ;
#83994 = CARTESIAN_POINT('Ctrl Pts',(-1.07558381670212,0.497141372528847,
6.87099896104922)) ;
#83995 = CARTESIAN_POINT('Ctrl Pts',(-1.0028380249261,0.631144921015609,6.8621221709435)) ;
#83996 = CARTESIAN_POINT('Ctrl Pts',(-0.810013135609759,0.864960701822275,
6.84199159983804)) ;
#83997 = CARTESIAN_POINT('Ctrl Pts',(-0.691530387648851,0.962315200348783,
6.83126426911237)) ;
#83998 = CARTESIAN_POINT('Ctrl Pts',(-0.420592817665239,1.10842350505255,
6.80944653778318)) ;
#83999 = CARTESIAN_POINT('Ctrl Pts',(-0.269962987074766,1.15440059797669,
6.79856665051965)) ;
#84000 = CARTESIAN_POINT('Ctrl Pts',(0.0335533958635028,1.18417163324696,
6.7788729210257)) ;
#84001 = CARTESIAN_POINT('Ctrl Pts',(0.183234004924584,1.17039552724657,6.76982625454176)) ;
#84002 = CARTESIAN_POINT('Ctrl Pts',(0.474044454137496,1.08632053978066,6.74898748884204)) ;
#84003 = CARTESIAN_POINT('Ctrl Pts',(0.611883678841635,1.01508856981479,6.7379976631639)) ;
#84004 = CARTESIAN_POINT('Ctrl Pts',(0.854113308250065,0.822197143610017,
6.71628418319936)) ;
#84005 = CARTESIAN_POINT('Ctrl Pts',(0.955508006956892,0.701765744281576,
6.70601043627221)) ;
#84006 = CARTESIAN_POINT('Ctrl Pts',(1.10247440168677,0.433798141151207,6.68700953041831)) ;
#84007 = CARTESIAN_POINT('Ctrl Pts',(1.14871791834261,0.289921392349667,6.67680759359234)) ;
#84008 = CARTESIAN_POINT('Ctrl Pts',(1.18541864386451,-0.0131519852271414,
6.65531742594936)) ;
#84009 = CARTESIAN_POINT('Ctrl Pts',(1.17327314348846,-0.169786209996843,
6.64421088872777)) ;
#84010 = CARTESIAN_POINT('Ctrl Pts',(1.0896308401728,-0.465854103473383,6.62321746226654)) ;
#84011 = CARTESIAN_POINT('Ctrl Pts',(1.02030279684906,-0.60273754292522,6.61420178967267)) ;
#84012 = CARTESIAN_POINT('Ctrl Pts',(0.833626125081446,-0.842152937460216,
6.5942502390725)) ;
#84013 = CARTESIAN_POINT('Ctrl Pts',(0.718223192197296,-0.942493500016631,
6.58360616549766)) ;
#84014 = CARTESIAN_POINT('Ctrl Pts',(0.45054154591066,-1.09681661498434,6.56169712714617)) ;
#84015 = CARTESIAN_POINT('Ctrl Pts',(0.299643662535163,-1.1472690025159,6.55064211346663)) ;
#84016 = CARTESIAN_POINT('Ctrl Pts',(-0.0048197825588484,-1.18466352171105,
6.53061994609462)) ;
#84017 = CARTESIAN_POINT('Ctrl Pts',(-0.154989297907911,-1.17449411767808,
6.52170600664431)) ;
#84018 = CARTESIAN_POINT('Ctrl Pts',(-0.447563953364002,-1.09744493981908,
6.50100799634912)) ;
#84019 = CARTESIAN_POINT('Ctrl Pts',(-0.586759631694064,-1.02976014462743,
6.49006063461073)) ;
#84020 = CARTESIAN_POINT('Ctrl Pts',(-0.83328528339986,-0.843269327369928,
6.46831027141656)) ;
#84021 = CARTESIAN_POINT('Ctrl Pts',(-0.937656650770386,-0.725461595602201,
6.45772434419496)) ;
#84022 = CARTESIAN_POINT('Ctrl Pts',(-1.09104926102747,-0.46161743045704,
6.43895059917853)) ;
#84023 = CARTESIAN_POINT('Ctrl Pts',(-1.14085869704814,-0.319337980171836,
6.42889344952874)) ;
#84024 = CARTESIAN_POINT('Ctrl Pts',(-1.17105675703185,-0.114558877463233,
6.41437308062609)) ;
#84025 = CARTESIAN_POINT('Ctrl Pts',(-1.17524047358084,-0.0572537864841875,
6.41030972137697)) ;
#84026 = CARTESIAN_POINT('Ctrl Pts',(-1.17524047358084,1.90683135537553E-30,
6.40624999999999)) ;
#84027 = CARTESIAN_POINT('Ctrl Pts',(-1.17524047358084,-7.58582575310211E-15,
6.34374999999999)) ;
#84028 = CARTESIAN_POINT('Ctrl Pts',(-1.17524047358084,-0.0044678076702123,
6.34406680095624)) ;
#84029 = CARTESIAN_POINT('Ctrl Pts',(-1.17521499629935,-0.008936798749249,
6.344383685825)) ;
#84030 = CARTESIAN_POINT('Ctrl Pts',(-1.17343789132738,-0.164708197103276,
6.35542904220494)) ;
#84031 = CARTESIAN_POINT('Ctrl Pts',(-1.14250769285491,-0.314289406667729,
6.36603546793419)) ;
#84032 = CARTESIAN_POINT('Ctrl Pts',(-1.02514738656922,-0.594574402112479,
6.38590976896346)) ;
#84033 = CARTESIAN_POINT('Ctrl Pts',(-0.939454328608444,-0.722411403523905,
6.39500581227288)) ;
#84034 = CARTESIAN_POINT('Ctrl Pts',(-0.721904121579447,-0.940314378340289,
6.41609053918469)) ;
#84035 = CARTESIAN_POINT('Ctrl Pts',(-0.591394401613091,-1.02741597556096,
6.42719291461776)) ;
#84036 = CARTESIAN_POINT('Ctrl Pts',(-0.309471063041387,-1.14358288483808,
6.44862372208196)) ;
#84037 = CARTESIAN_POINT('Ctrl Pts',(-0.161553478030403,-1.17366037958495,
6.45877335648141)) ;
#84038 = CARTESIAN_POINT('Ctrl Pts',(0.143839569063921,-1.17676187995031,
6.47763679287917)) ;
#84039 = CARTESIAN_POINT('Ctrl Pts',(0.298477955528415,-1.14735543048462,
6.4880674659165)) ;
#84040 = CARTESIAN_POINT('Ctrl Pts',(0.58511831199092,-1.03072270487193,6.50980444940654)) ;
#84041 = CARTESIAN_POINT('Ctrl Pts',(0.714605246437693,-0.945567060310018,
6.52077502666626)) ;
#84042 = CARTESIAN_POINT('Ctrl Pts',(0.930370235619318,-0.733371830307261,
6.54154776661931)) ;
#84043 = CARTESIAN_POINT('Ctrl Pts',(1.0157831583268,-0.609588394125534,6.55052562678806)) ;
#84044 = CARTESIAN_POINT('Ctrl Pts',(1.13859585747244,-0.330336899820532,
6.57032664486213)) ;
#84045 = CARTESIAN_POINT('Ctrl Pts',(1.1723287213559,-0.176492281748416,6.58123537811932)) ;
#84046 = CARTESIAN_POINT('Ctrl Pts',(1.17771809657695,0.131124527411696,6.6030477090192)) ;
#84047 = CARTESIAN_POINT('Ctrl Pts',(1.15097044421376,0.281948420449146,6.61374225029451)) ;
#84048 = CARTESIAN_POINT('Ctrl Pts',(1.04168170028128,0.564832157819538,6.63380082154932)) ;
#84049 = CARTESIAN_POINT('Ctrl Pts',(0.960313145035741,0.694217503492424,
6.64272534176084)) ;
#84050 = CARTESIAN_POINT('Ctrl Pts',(0.749885964309827,0.918233666595859,
6.66358939556668)) ;
#84051 = CARTESIAN_POINT('Ctrl Pts',(0.621647266996083,1.00946928529428,6.67469887929173)) ;
#84052 = CARTESIAN_POINT('Ctrl Pts',(0.34244034865538,1.13420282045342,6.69626659660949)) ;
#84053 = CARTESIAN_POINT('Ctrl Pts',(0.195026152245701,1.1686182415064,6.70653911478431)) ;
#84054 = CARTESIAN_POINT('Ctrl Pts',(-0.111706431977466,1.18039552467786,
6.72579239796304)) ;
#84055 = CARTESIAN_POINT('Ctrl Pts',(-0.268183346404951,1.154957615284,6.73593761858074)) ;
#84056 = CARTESIAN_POINT('Ctrl Pts',(-0.5590576673299,1.04514304650888,6.75769287084004)) ;
#84057 = CARTESIAN_POINT('Ctrl Pts',(-0.690958549416792,0.963041337460044,
6.76870340958252)) ;
#84058 = CARTESIAN_POINT('Ctrl Pts',(-0.912033611663407,0.756028455339652,
6.78961849517136)) ;
#84059 = CARTESIAN_POINT('Ctrl Pts',(-1.00039140029523,0.634496461721281,
6.79875945863243)) ;
#84060 = CARTESIAN_POINT('Ctrl Pts',(-1.13003204407789,0.358532398497774,
6.81832737327253)) ;
#84061 = CARTESIAN_POINT('Ctrl Pts',(-1.16757371714912,0.205593473793426,
6.82917188610079)) ;
#84062 = CARTESIAN_POINT('Ctrl Pts',(-1.17488878285825,0.0332123672961974,
6.84139499492917)) ;
#84063 = CARTESIAN_POINT('Ctrl Pts',(-1.17524047358084,0.0165996920375581,
6.8425729577683)) ;
#84064 = CARTESIAN_POINT('Ctrl Pts',(-1.17524047358084,1.51344660858459E-14,
6.84374999999999)) ;
#84065 = CARTESIAN_POINT('Origin',(0.,0.,0.)) ;
#84066 = CARTESIAN_POINT('',(-1.17524047358084,1.18856858147489E-16,7.40624999999999)) ;
#84067 = CARTESIAN_POINT('',(-1.17524047358084,2.22940266706097E-16,7.34374999999999)) ;
#84068 = CARTESIAN_POINT('',(-1.17524047358084,-1.4392544841992E-16,0.)) ;
#84069 = CARTESIAN_POINT('Ctrl Pts',(-1.17524047358084,-7.52869988573934E-15,
7.40624999999999)) ;
#84070 = CARTESIAN_POINT('Ctrl Pts',(-1.17524047358084,0.140900390422391,
7.39625910922843)) ;
#84071 = CARTESIAN_POINT('Ctrl Pts',(-1.14989965594148,0.280812784794329,
7.38633827476116)) ;
#84072 = CARTESIAN_POINT('Ctrl Pts',(-1.04762920185557,0.553274912443593,
7.36701867352676)) ;
#84073 = CARTESIAN_POINT('Ctrl Pts',(-0.968660523144742,0.682157590236431,
7.35821482030409)) ;
#84074 = CARTESIAN_POINT('Ctrl Pts',(-0.764571824481488,0.905505645411124,
7.33776368485999)) ;
#84075 = CARTESIAN_POINT('Ctrl Pts',(-0.64057893563885,0.997075584412772,
7.32690307345249)) ;
#84076 = CARTESIAN_POINT('Ctrl Pts',(-0.361668809505296,1.12901714389102,
7.30509803005525)) ;
#84077 = CARTESIAN_POINT('Ctrl Pts',(-0.208877053390522,1.16699541834544,
7.29436897198069)) ;
#84078 = CARTESIAN_POINT('Ctrl Pts',(0.0956888238037573,1.18076909072001,
7.27517796178267)) ;
#84079 = CARTESIAN_POINT('Ctrl Pts',(0.244439347390227,1.15915998788396,7.26566943497862)) ;
#84080 = CARTESIAN_POINT('Ctrl Pts',(0.531198935603337,1.05966305353421,7.24453265758091)) ;
#84081 = CARTESIAN_POINT('Ctrl Pts',(0.665748146250717,0.980733454568991,
7.2334719542987)) ;
#84082 = CARTESIAN_POINT('Ctrl Pts',(0.896964111186548,0.775026017070139,
7.21198042235567)) ;
#84083 = CARTESIAN_POINT('Ctrl Pts',(0.991199233222183,0.65016430083957,7.20235150826259)) ;
#84084 = CARTESIAN_POINT('Ctrl Pts',(1.12393435326191,0.375013456795158,7.18284125694029)) ;
#84085 = CARTESIAN_POINT('Ctrl Pts',(1.16267390068334,0.228107113413445,7.17242449921537)) ;
#84086 = CARTESIAN_POINT('Ctrl Pts',(1.18302576086515,-0.0781448611877374,
7.1507089452865)) ;
#84087 = CARTESIAN_POINT('Ctrl Pts',(1.1621366215204,-0.234748686209369,7.13960456363426)) ;
#84088 = CARTESIAN_POINT('Ctrl Pts',(1.06221252552216,-0.52490121083084,7.11903058103637)) ;
#84089 = CARTESIAN_POINT('Ctrl Pts',(0.986405785060841,-0.656369039599867,
7.11021881605146)) ;
#84090 = CARTESIAN_POINT('Ctrl Pts',(0.788052581691994,-0.88507891389793,
7.08992978750648)) ;
#84091 = CARTESIAN_POINT('Ctrl Pts',(0.66684160771477,-0.979643959324821,
7.0791338193041)) ;
#84092 = CARTESIAN_POINT('Ctrl Pts',(0.391913510093961,-1.11888203078298,
7.05731461439808)) ;
#84093 = CARTESIAN_POINT('Ctrl Pts',(0.240172112542563,-1.16096183035088,
7.04650464200688)) ;
#84094 = CARTESIAN_POINT('Ctrl Pts',(-0.063896025711483,-1.18291047801106,
7.02705436337555)) ;
#84095 = CARTESIAN_POINT('Ctrl Pts',(-0.213100997195953,-1.16531857614416,
7.01781219513354)) ;
#84096 = CARTESIAN_POINT('Ctrl Pts',(-0.501975738719509,-1.07375536950523,
6.99682681138702)) ;
#84097 = CARTESIAN_POINT('Ctrl Pts',(-0.638270561450102,-0.998768809012039,
6.98579870957638)) ;
#84098 = CARTESIAN_POINT('Ctrl Pts',(-0.875903269288135,-0.799019702673039,
6.96412438548422)) ;
#84099 = CARTESIAN_POINT('Ctrl Pts',(-0.974271645666074,-0.675575654491047,
6.95415336316112)) ;
#84100 = CARTESIAN_POINT('Ctrl Pts',(-1.11418971784618,-0.402907736973438,
6.93481916988699)) ;
#84101 = CARTESIAN_POINT('Ctrl Pts',(-1.15649700435257,-0.257383727073601,
6.92450042993751)) ;
#84102 = CARTESIAN_POINT('Ctrl Pts',(-1.17359052160968,-0.0719524690405092,
6.9113519678283)) ;
#84103 = CARTESIAN_POINT('Ctrl Pts',(-1.17524047358084,-0.0359549588519092,
6.90879947531023)) ;
#84104 = CARTESIAN_POINT('Ctrl Pts',(-1.17524047358084,-7.58582575310211E-15,
6.90624999999999)) ;
#84105 = CARTESIAN_POINT('Ctrl Pts',(-1.17524047358084,1.57512891618694E-14,
6.84374999999999)) ;
#84106 = CARTESIAN_POINT('Ctrl Pts',(-1.17524047358084,-0.135226891452661,
6.85333859729082)) ;
#84107 = CARTESIAN_POINT('Ctrl Pts',(-1.15189944472838,-0.26959217728986,
6.86286610030385)) ;
#84108 = CARTESIAN_POINT('Ctrl Pts',(-1.05517274840351,-0.539002344572276,
6.88196929473786)) ;
#84109 = CARTESIAN_POINT('Ctrl Pts',(-0.977439522827835,-0.669720851075183,
6.89080515286758)) ;
#84110 = CARTESIAN_POINT('Ctrl Pts',(-0.773103081343997,-0.898842717747965,
6.91147620481635)) ;
#84111 = CARTESIAN_POINT('Ctrl Pts',(-0.646891687261351,-0.993542643945497,
6.92258401921284)) ;
#84112 = CARTESIAN_POINT('Ctrl Pts',(-0.370190709228593,-1.12549930666603,
6.94425393943049)) ;
#84113 = CARTESIAN_POINT('Ctrl Pts',(-0.223303099307756,-1.16359203364959,
6.95462449539132)) ;
#84114 = CARTESIAN_POINT('Ctrl Pts',(0.0820479794397184,-1.18264625779152,
6.97405093828379)) ;
#84115 = CARTESIAN_POINT('Ctrl Pts',(0.237697446954262,-1.16142548556799,
6.98383624023947)) ;
#84116 = CARTESIAN_POINT('Ctrl Pts',(0.530536422283173,-1.05996578566071,
7.00541592603201)) ;
#84117 = CARTESIAN_POINT('Ctrl Pts',(0.664963206627907,-0.981234344893288,
7.01646208595114)) ;
#84118 = CARTESIAN_POINT('Ctrl Pts',(0.891737710114681,-0.779865074238771,
7.03752707385189)) ;
#84119 = CARTESIAN_POINT('Ctrl Pts',(0.983273371875511,-0.660707460643659,
7.04690090290762)) ;
#84120 = CARTESIAN_POINT('Ctrl Pts',(1.12014572345183,-0.388310441098143,
7.06621588749084)) ;
#84121 = CARTESIAN_POINT('Ctrl Pts',(1.16171568906366,-0.236442774008544,
7.07698444014762)) ;
#84122 = CARTESIAN_POINT('Ctrl Pts',(1.18295170444811,0.0711945256250565,
7.09879822397522)) ;
#84123 = CARTESIAN_POINT('Ctrl Pts',(1.16374607860161,0.223939531610267,7.10962898651693)) ;
#84124 = CARTESIAN_POINT('Ctrl Pts',(1.06879077063093,0.511278658467174,7.13000347818596)) ;
#84125 = CARTESIAN_POINT('Ctrl Pts',(0.994851762372556,0.643419387816601,
7.13880342258014)) ;
#84126 = CARTESIAN_POINT('Ctrl Pts',(0.796961154022966,0.87783355824789,7.15926628285598)) ;
#84127 = CARTESIAN_POINT('Ctrl Pts',(0.672978156071706,0.976128090143578,
7.17036469883477)) ;
#84128 = CARTESIAN_POINT('Ctrl Pts',(0.399108068044064,1.11562402974253,7.19212807622204)) ;
#84129 = CARTESIAN_POINT('Ctrl Pts',(0.252872132475181,1.15757465457084,7.20259539127241)) ;
#84130 = CARTESIAN_POINT('Ctrl Pts',(-0.0509840568487462,1.18422250573345,
7.22219925893808)) ;
#84131 = CARTESIAN_POINT('Ctrl Pts',(-0.2057926830757,1.167324956904,7.23166788460105)) ;
#84132 = CARTESIAN_POINT('Ctrl Pts',(-0.500546672836903,1.07451481806782,
7.25305850771178)) ;
#84133 = CARTESIAN_POINT('Ctrl Pts',(-0.637503666397729,0.999357909769225,
7.26413331135905)) ;
#84134 = CARTESIAN_POINT('Ctrl Pts',(-0.870157429570499,0.803902957339546,
7.28534964623793)) ;
#84135 = CARTESIAN_POINT('Ctrl Pts',(-0.9649952259348,0.687153725923925,7.29502566503965)) ;
#84136 = CARTESIAN_POINT('Ctrl Pts',(-1.10922617325092,0.418474621077651,
7.31407702168297)) ;
#84137 = CARTESIAN_POINT('Ctrl Pts',(-1.15488253080609,0.267815401325705,
7.32475988639157)) ;
#84138 = CARTESIAN_POINT('Ctrl Pts',(-1.17343972786484,0.0751669931566532,
7.33842009838646)) ;
#84139 = CARTESIAN_POINT('Ctrl Pts',(-1.17524047358084,0.037562040414441,
7.34108657059562)) ;
#84140 = CARTESIAN_POINT('Ctrl Pts',(-1.17524047358084,7.69738201417715E-15,
7.34374999999999)) ;
#84141 = CARTESIAN_POINT('Origin',(0.,0.,0.)) ;
#84142 = CARTESIAN_POINT('',(-1.17524047358084,-7.09759280191603E-15,7.90624999999999)) ;
#84143 = CARTESIAN_POINT('',(-1.17524047358084,1.08596519600456E-15,7.84374999999999)) ;
#84144 = CARTESIAN_POINT('',(-1.17524047358084,-1.4392544841992E-16,0.)) ;
#84145 = CARTESIAN_POINT('Ctrl Pts',(-1.17524047358084,-7.58582575310211E-15,
7.90624999999999)) ;
#84146 = CARTESIAN_POINT('Ctrl Pts',(-1.17524047358084,0.0058948731809242,
7.90583200943313)) ;
#84147 = CARTESIAN_POINT('Ctrl Pts',(-1.17519612161567,0.0117916867983566,
7.90541388127487)) ;
#84148 = CARTESIAN_POINT('Ctrl Pts',(-1.17276021783936,0.173603808745751,
7.89394019244374)) ;
#84149 = CARTESIAN_POINT('Ctrl Pts',(-1.13940585452016,0.32753281696594,7.88302547529432)) ;
#84150 = CARTESIAN_POINT('Ctrl Pts',(-1.01727153832607,0.607106605361429,
7.86320160416041)) ;
#84151 = CARTESIAN_POINT('Ctrl Pts',(-0.932148461486229,0.731114324393812,
7.85423700035429)) ;
#84152 = CARTESIAN_POINT('Ctrl Pts',(-0.716907295609362,0.9438169432025,7.83347843834259)) ;
#84153 = CARTESIAN_POINT('Ctrl Pts',(-0.587661508996336,1.0292692781813,7.82251215062637)) ;
#84154 = CARTESIAN_POINT('Ctrl Pts',(-0.301350693636575,1.14660392666468,
7.80077051770002)) ;
#84155 = CARTESIAN_POINT('Ctrl Pts',(-0.146790779180812,1.17639625830996,
7.79030505717394)) ;
#84156 = CARTESIAN_POINT('Ctrl Pts',(0.158563243857567,1.17406334471649,7.77147126642596)) ;
#84157 = CARTESIAN_POINT('Ctrl Pts',(0.306519541774214,1.14437258126579,7.76133296582669)) ;
#84158 = CARTESIAN_POINT('Ctrl Pts',(0.588672505983702,1.02897180053752,7.7399152197063)) ;
#84159 = CARTESIAN_POINT('Ctrl Pts',(0.719378386679859,0.942241237046807,
7.72881395303141)) ;
#84160 = CARTESIAN_POINT('Ctrl Pts',(0.937560621433912,0.724888409377175,
7.70770991953948)) ;
#84161 = CARTESIAN_POINT('Ctrl Pts',(1.0236414217451,0.597188552307871,7.69859513175054)) ;
#84162 = CARTESIAN_POINT('Ctrl Pts',(1.14171576494173,0.317136633283916,7.67873735758152)) ;
#84163 = CARTESIAN_POINT('Ctrl Pts',(1.1730134137733,0.167670809135427,7.66813911354066)) ;
#84164 = CARTESIAN_POINT('Ctrl Pts',(1.17732189197484,-0.140829977811578,
7.64626410200883)) ;
#84165 = CARTESIAN_POINT('Ctrl Pts',(1.14793575214488,-0.296951504562182,
7.63519391890871)) ;
#84166 = CARTESIAN_POINT('Ctrl Pts',(1.0324120929391,-0.581061428499252,7.61504840186178)) ;
#84167 = CARTESIAN_POINT('Ctrl Pts',(0.950296156040182,-0.707424436632612,
7.60619130311218)) ;
#84168 = CARTESIAN_POINT('Ctrl Pts',(0.740498868551504,-0.925360465755667,
7.58558149305588)) ;
#84169 = CARTESIAN_POINT('Ctrl Pts',(0.613789705347934,-1.01384686019507,
7.57466340473639)) ;
#84170 = CARTESIAN_POINT('Ctrl Pts',(0.331083216715362,-1.13835745748783,
7.55288869092816)) ;
#84171 = CARTESIAN_POINT('Ctrl Pts',(0.177353214776067,-1.17219688281456,
7.54224875502853)) ;
#84172 = CARTESIAN_POINT('Ctrl Pts',(-0.127633834305618,-1.17776796833596,
7.52332269400168)) ;
#84173 = CARTESIAN_POINT('Ctrl Pts',(-0.275971546063842,-1.1520907162658,
7.51348248391123)) ;
#84174 = CARTESIAN_POINT('Ctrl Pts',(-0.560507923634067,-1.0445190806793,
7.49219595037346)) ;
#84175 = CARTESIAN_POINT('Ctrl Pts',(-0.693167236998827,-0.961619211029062,
7.48111054035441)) ;
#84176 = CARTESIAN_POINT('Ctrl Pts',(-0.917808778987186,-0.749964388364812,
7.45981187140171)) ;
#84177 = CARTESIAN_POINT('Ctrl Pts',(-1.0078920433783,-0.623667128528289,
7.45047266070564)) ;
#84178 = CARTESIAN_POINT('Ctrl Pts',(-1.13324613899673,-0.346021163261254,
7.43078548664011)) ;
#84179 = CARTESIAN_POINT('Ctrl Pts',(-1.16826437655785,-0.197781345255079,
7.42027417559792)) ;
#84180 = CARTESIAN_POINT('Ctrl Pts',(-1.1749274611804,-0.0313328213326564,
7.40847173121425)) ;
#84181 = CARTESIAN_POINT('Ctrl Pts',(-1.17524047358084,-0.0156603082556396,
7.40736043290058)) ;
#84182 = CARTESIAN_POINT('Ctrl Pts',(-1.17524047358084,-7.58582575310211E-15,
7.40624999999999)) ;
#84183 = CARTESIAN_POINT('Ctrl Pts',(-1.17524047358084,7.25114412958305E-15,
7.34374999999999)) ;
#84184 = CARTESIAN_POINT('Ctrl Pts',(-1.17524047358084,-0.114800540624639,
7.35189021635041)) ;
#84185 = CARTESIAN_POINT('Ctrl Pts',(-1.15841823069317,-0.229200240755181,
7.36000201011389)) ;
#84186 = CARTESIAN_POINT('Ctrl Pts',(-1.08191912485661,-0.48272018550954,
7.37797846900701)) ;
#84187 = CARTESIAN_POINT('Ctrl Pts',(-1.01178498089613,-0.616324113861105,
7.38680296430364)) ;
#84188 = CARTESIAN_POINT('Ctrl Pts',(-0.82044410185443,-0.856005323624095,
7.40705035716586)) ;
#84189 = CARTESIAN_POINT('Ctrl Pts',(-0.698808940480666,-0.957874766339547,
7.41813134190996)) ;
#84190 = CARTESIAN_POINT('Ctrl Pts',(-0.427997399400052,-1.10491551108798,
7.4399743925815)) ;
#84191 = CARTESIAN_POINT('Ctrl Pts',(-0.282520564355878,-1.15074740822359,
7.45053269864208)) ;
#84192 = CARTESIAN_POINT('Ctrl Pts',(0.019783699303596,-1.18500381086977,
7.47031101774605)) ;
#84193 = CARTESIAN_POINT('Ctrl Pts',(0.173779326513984,-1.17236324487432,
7.47952339270713)) ;
#84194 = CARTESIAN_POINT('Ctrl Pts',(0.470320579500165,-1.08814557758605,
7.50071913226851)) ;
#84195 = CARTESIAN_POINT('Ctrl Pts',(0.609702319781948,-1.0166223215586,7.51181400741951)) ;
#84196 = CARTESIAN_POINT('Ctrl Pts',(0.848175488757153,-0.827119850559174,
7.53317666076052)) ;
#84197 = CARTESIAN_POINT('Ctrl Pts',(0.946311269830303,-0.712719278720804,
7.54321287626921)) ;
#84198 = CARTESIAN_POINT('Ctrl Pts',(1.09772935000642,-0.447755836558663,
7.56200076465733)) ;
#84199 = CARTESIAN_POINT('Ctrl Pts',(1.14735802281595,-0.298391829379991,
7.57259178911405)) ;
#84200 = CARTESIAN_POINT('Ctrl Pts',(1.18516499220896,0.00838585772460532,
7.59434461998859)) ;
#84201 = CARTESIAN_POINT('Ctrl Pts',(1.17397135458397,0.162738510214385,7.60528937668304)) ;
#84202 = CARTESIAN_POINT('Ctrl Pts',(1.09401493221283,0.454525951531374,7.62597928709402)) ;
#84203 = CARTESIAN_POINT('Ctrl Pts',(1.02754412146254,0.589583406649628,7.63488717413944)) ;
#84204 = CARTESIAN_POINT('Ctrl Pts',(0.842589314505928,0.834295352560546,
7.65492077156646)) ;
#84205 = CARTESIAN_POINT('Ctrl Pts',(0.723319896849969,0.939572148399538,
7.66597728489355)) ;
#84206 = CARTESIAN_POINT('Ctrl Pts',(0.455659765401045,1.09384952159629,7.68788338035219)) ;
#84207 = CARTESIAN_POINT('Ctrl Pts',(0.31101429630278,1.14342395280021,7.69852332098254)) ;
#84208 = CARTESIAN_POINT('Ctrl Pts',(0.0102535189430444,1.18499783305075,
7.7184662901098)) ;
#84209 = CARTESIAN_POINT('Ctrl Pts',(-0.142993451744908,1.17638561620861,
7.72749029565596)) ;
#84210 = CARTESIAN_POINT('Ctrl Pts',(-0.441135736426058,1.1003589123575,7.74849395058592)) ;
#84211 = CARTESIAN_POINT('Ctrl Pts',(-0.582743444374524,1.03237289144522,
7.75960010902981)) ;
#84212 = CARTESIAN_POINT('Ctrl Pts',(-0.826579541055378,0.848744728621272,
7.7810838211089)) ;
#84213 = CARTESIAN_POINT('Ctrl Pts',(-0.927895337597086,0.73663765641396,
7.79128000314893)) ;
#84214 = CARTESIAN_POINT('Ctrl Pts',(-1.08612342439241,0.475189699535579,
7.81026572899363)) ;
#84215 = CARTESIAN_POINT('Ctrl Pts',(-1.13952856720092,0.327096064670921,
7.82055644429624)) ;
#84216 = CARTESIAN_POINT('Ctrl Pts',(-1.17098904386158,0.115479407808046,
7.83556164689236)) ;
#84217 = CARTESIAN_POINT('Ctrl Pts',(-1.17524047358084,0.0577152052619275,
7.83965756058302)) ;
#84218 = CARTESIAN_POINT('Ctrl Pts',(-1.17524047358084,7.69738201417715E-15,
7.84374999999999)) ;
#84219 = CARTESIAN_POINT('Origin',(0.,0.,3.17500000000003)) ;
#84220 = CARTESIAN_POINT('',(-1.39316924099002,5.26377606127364E-10,0.217928767409175)) ;
#84221 = CARTESIAN_POINT('',(-1.17524047358084,-1.4392544841992E-16,-2.77555756156289E-15)) ;
#84222 = CARTESIAN_POINT('',(-4.35024047358084,-5.32750807149204E-16,3.17500000000003)) ;
#84223 = CARTESIAN_POINT('',(0.,1.31392241650299,0.138681942922155)) ;
#84224 = CARTESIAN_POINT('Ctrl Pts',(1.74721348500384E-12,1.31392241650293,
0.138681942922092)) ;
#84225 = CARTESIAN_POINT('Ctrl Pts',(-0.167266855118978,1.31974695353597,
0.144506479954901)) ;
#84226 = CARTESIAN_POINT('Ctrl Pts',(-0.334124488002528,1.29418388150016,
0.150878326562875)) ;
#84227 = CARTESIAN_POINT('Ctrl Pts',(-0.652060491102024,1.18211772827159,
0.164090894186344)) ;
#84228 = CARTESIAN_POINT('Ctrl Pts',(-0.799989205130994,1.09575091156118,
0.170816999489089)) ;
#84229 = CARTESIAN_POINT('Ctrl Pts',(-1.06340473087861,0.865641363708454,
0.184102644672758)) ;
#84230 = CARTESIAN_POINT('Ctrl Pts',(-1.1726050878534,0.721855450662107,0.190024438180476)) ;
#84231 = CARTESIAN_POINT('Ctrl Pts',(-1.3335089728491,0.394133514358114,0.202849944858133)) ;
#84232 = CARTESIAN_POINT('Ctrl Pts',(-1.38118306540828,0.212723127559774,
0.209850714302632)) ;
#84233 = CARTESIAN_POINT('Ctrl Pts',(-1.39238912395266,0.0182111698154136,
0.217237913870716)) ;
#84234 = CARTESIAN_POINT('Ctrl Pts',(-1.39282395373248,0.00910529163896913,
0.217583480158522)) ;
#84235 = CARTESIAN_POINT('Ctrl Pts',(-1.39316924099002,1.05275545825681E-9,
0.217928767409175)) ;
#84236 = CARTESIAN_POINT('Ctrl Pts',(3.46944695195361E-17,1.313922416503,
0.138681942922154)) ;
#84237 = CARTESIAN_POINT('Ctrl Pts',(0.121098558534658,1.30970554378009,0.134465070199245)) ;
#84238 = CARTESIAN_POINT('Ctrl Pts',(0.240975723217191,1.2884142130355,0.129912989605975)) ;
#84239 = CARTESIAN_POINT('Ctrl Pts',(0.468004205836076,1.21399303966281,0.120506510970423)) ;
#84240 = CARTESIAN_POINT('Ctrl Pts',(0.574338680072799,1.16212197232517,0.115708518042526)) ;
#84241 = CARTESIAN_POINT('Ctrl Pts',(0.810645309221597,1.0035800682715,0.104033084804398)) ;
#84242 = CARTESIAN_POINT('Ctrl Pts',(0.929777469010434,0.884582495704132,
0.0972302038558343)) ;
#84243 = CARTESIAN_POINT('Ctrl Pts',(1.10705252184507,0.621012134582888,0.0851203819684317)) ;
#84244 = CARTESIAN_POINT('Ctrl Pts',(1.17642194056122,0.470512057886478,0.0792919584706692)) ;
#84245 = CARTESIAN_POINT('Ctrl Pts',(1.24281530973834,0.140961942944052,0.0654717101243752)) ;
#84246 = CARTESIAN_POINT('Ctrl Pts',(1.24387622027251,-0.0190346630085623,
0.0586570394766492)) ;
#84247 = CARTESIAN_POINT('Ctrl Pts',(1.1998121485432,-0.253773770858911,0.0484886700811816)) ;
#84248 = CARTESIAN_POINT('Ctrl Pts',(1.17732416720795,-0.331067562529302,
0.045111449811975)) ;
#84249 = CARTESIAN_POINT('Ctrl Pts',(1.10851242855053,-0.503006066466911,
0.0375382749190259)) ;
#84250 = CARTESIAN_POINT('Ctrl Pts',(1.03395653270362,-0.656327700634369,
0.031502652974492)) ;
#84251 = CARTESIAN_POINT('Ctrl Pts',(0.826032359412923,-0.866968095167022,
0.0190841208660029)) ;
#84252 = CARTESIAN_POINT('Ctrl Pts',(0.758282491098308,-0.921926165773169,
0.0153019770602942)) ;
#84253 = CARTESIAN_POINT('Ctrl Pts',(0.613046880469622,-1.01525486110679,
0.00765611751817106)) ;
#84254 = CARTESIAN_POINT('Ctrl Pts',(0.536151617816848,-1.05358542078566,
0.00381702273341533)) ;
#84255 = CARTESIAN_POINT('Ctrl Pts',(0.455787866251496,-1.08325786021632,
-1.07414819494005E-15)) ;
#84256 = CARTESIAN_POINT('Origin',(0.,0.,1.91347191551875E-17)) ;
#84257 = CARTESIAN_POINT('Origin',(0.,0.,3.17500000000003)) ;
#84258 = CARTESIAN_POINT('Origin',(0.,0.,1.91347191551875E-17)) ;
#84259 = CARTESIAN_POINT('Ctrl Pts',(-0.455787866251585,-1.08325786021629,
7.45931094670027E-15)) ;
#84260 = CARTESIAN_POINT('Ctrl Pts',(-0.339450345579036,-1.15671718194011,
0.0225912551073548)) ;
#84261 = CARTESIAN_POINT('Ctrl Pts',(-0.210569648303892,-1.20857442445214,
0.0439022454998153)) ;
#84262 = CARTESIAN_POINT('Ctrl Pts',(0.0513954888457053,-1.26231602057434,
0.0816139151640012)) ;
#84263 = CARTESIAN_POINT('Ctrl Pts',(0.206168368761232,-1.27168280828374,
0.102415923974052)) ;
#84264 = CARTESIAN_POINT('Ctrl Pts',(0.54006497178572,-1.22359742953493,0.151575420771421)) ;
#84265 = CARTESIAN_POINT('Ctrl Pts',(0.702493852367329,-1.16720785633507,
0.176560474021524)) ;
#84266 = CARTESIAN_POINT('Ctrl Pts',(0.986274961170952,-1.00279284711702,
0.222626794633426)) ;
#84267 = CARTESIAN_POINT('Ctrl Pts',(1.10763761296648,-0.900326883506944,
0.243527666641757)) ;
#84268 = CARTESIAN_POINT('Ctrl Pts',(1.29324613200729,-0.677217027216316,
0.278664266693318)) ;
#84269 = CARTESIAN_POINT('Ctrl Pts',(1.39030020188671,-0.53001090787689,0.299259900155697)) ;
#84270 = CARTESIAN_POINT('Ctrl Pts',(1.46053184144303,-0.341828524454995,
0.324759526419172)) ;
#84271 = CARTESIAN_POINT('Ctrl Pts',(-1.39316924099002,1.05275552164663E-9,
0.217928767409175)) ;
#84272 = CARTESIAN_POINT('Ctrl Pts',(-1.39980350682736,-0.174946849597754,
0.224563033114318)) ;
#84273 = CARTESIAN_POINT('Ctrl Pts',(-1.37337989354183,-0.349676949483546,
0.231091430108109)) ;
#84274 = CARTESIAN_POINT('Ctrl Pts',(-1.24575263556661,-0.71231580729705,
0.244473225311046)) ;
#84275 = CARTESIAN_POINT('Ctrl Pts',(-1.13982635511045,-0.871321905508161,
0.250346387180502)) ;
#84276 = CARTESIAN_POINT('Ctrl Pts',(-0.909270559414451,-1.1289009029262,
0.262595703399922)) ;
#84277 = CARTESIAN_POINT('Ctrl Pts',(-0.761488569708769,-1.24131052195541,
0.269371248043327)) ;
#84278 = CARTESIAN_POINT('Ctrl Pts',(-0.425577664861815,-1.40767484606303,
0.28294008110021)) ;
#84279 = CARTESIAN_POINT('Ctrl Pts',(-0.239452270725757,-1.45766729711709,
0.289592176453111)) ;
#84280 = CARTESIAN_POINT('Ctrl Pts',(0.0747747453737359,-1.47811532752047,
0.299565085727837)) ;
#84281 = CARTESIAN_POINT('Ctrl Pts',(0.226155217538108,-1.47209514011507,
0.304325733785537)) ;
#84282 = CARTESIAN_POINT('Ctrl Pts',(0.527358450674983,-1.40067277358841,
0.314969262175127)) ;
#84283 = CARTESIAN_POINT('Ctrl Pts',(0.657371735221159,-1.34999571672739,
0.319872264403233)) ;
#84284 = CARTESIAN_POINT('Ctrl Pts',(0.778543926945339,-1.28213468630119,
0.324759526419204)) ;
#84285 = CARTESIAN_POINT('Origin',(0.,0.,0.)) ;
#84286 = CARTESIAN_POINT('',(0.455787866252619,-1.08325786021584,8.00000000000007)) ;
#84287 = CARTESIAN_POINT('Ctrl Pts',(-1.17524047358084,7.69738201417715E-15,
7.84374999999999)) ;
#84288 = CARTESIAN_POINT('Ctrl Pts',(-1.17524047358084,-0.0952625616493213,
7.85050482761405)) ;
#84289 = CARTESIAN_POINT('Ctrl Pts',(-1.16365735659741,-0.190391637202836,
7.8572501900662)) ;
#84290 = CARTESIAN_POINT('Ctrl Pts',(-1.10467059844949,-0.427908134816351,
7.87409188494714)) ;
#84291 = CARTESIAN_POINT('Ctrl Pts',(-1.04158501620156,-0.56435038347386,
7.88313035048783)) ;
#84292 = CARTESIAN_POINT('Ctrl Pts',(-0.863722948037223,-0.812098320702218,
7.9028360365624)) ;
#84293 = CARTESIAN_POINT('Ctrl Pts',(-0.748452859552877,-0.919412673019757,
7.91371919937978)) ;
#84294 = CARTESIAN_POINT('Ctrl Pts',(-0.486259227192268,-1.08065308415695,
7.93553647556142)) ;
#84295 = CARTESIAN_POINT('Ctrl Pts',(-0.342656760736266,-1.13439809447822,
7.94626023044091)) ;
#84296 = CARTESIAN_POINT('Ctrl Pts',(-0.085547857400007,-1.17715319798042,
7.96356451830549)) ;
#84297 = CARTESIAN_POINT('Ctrl Pts',(0.0235942810878135,-1.18002040743108,
7.97002940339912)) ;
#84298 = CARTESIAN_POINT('Ctrl Pts',(0.243174285763268,-1.15527572473979,
7.98439059217357)) ;
#84299 = CARTESIAN_POINT('Ctrl Pts',(0.352337269914904,-1.12678537873124,
7.99210412633095)) ;
#84300 = CARTESIAN_POINT('Ctrl Pts',(0.455787866253993,-1.08325786021526,
8.00000000000017)) ;
#84301 = CARTESIAN_POINT('',(-0.455787866251364,-1.08325786021637,8.)) ;
#84302 = CARTESIAN_POINT('Origin',(0.,0.,8.)) ;
#84303 = CARTESIAN_POINT('Ctrl Pts',(-0.455787866250356,-1.08325786021679,
8.00000000000008)) ;
#84304 = CARTESIAN_POINT('Ctrl Pts',(-0.531256398246912,-1.0515039792333,
7.99423985925915)) ;
#84305 = CARTESIAN_POINT('Ctrl Pts',(-0.603190980473794,-1.01195569703915,
7.98842038950236)) ;
#84306 = CARTESIAN_POINT('Ctrl Pts',(-0.737096443487214,-0.918948446823796,
7.9769001119198)) ;
#84307 = CARTESIAN_POINT('Ctrl Pts',(-0.798787320119198,-0.865862967133268,
7.97122974005493)) ;
#84308 = CARTESIAN_POINT('Ctrl Pts',(-0.958575679625279,-0.696632226777244,
7.95541764643436)) ;
#84309 = CARTESIAN_POINT('Ctrl Pts',(-1.04030848497531,-0.567378753684563,
7.94648139422948)) ;
#84310 = CARTESIAN_POINT('Ctrl Pts',(-1.14814522391219,-0.290213046141342,
7.92682827402602)) ;
#84311 = CARTESIAN_POINT('Ctrl Pts',(-1.17524047358084,-0.145699223142899,
7.91658116387795)) ;
#84312 = CARTESIAN_POINT('Ctrl Pts',(-1.17524047358084,-8.50014503228635E-15,
7.90624999999999)) ;
#84313 = CARTESIAN_POINT('Origin',(0.,0.,0.)) ;
#84314 = CARTESIAN_POINT('',(-0.581737793027629,1.38259941420621,8.)) ;
#84315 = CARTESIAN_POINT('Ctrl Pts',(-1.5,1.00028780763944E-14,7.59374999999998)) ;
#84316 = CARTESIAN_POINT('Ctrl Pts',(-1.5,-0.0509437253219826,7.59658020696231)) ;
#84317 = CARTESIAN_POINT('Ctrl Pts',(-1.49740480695262,-0.101948126880478,
7.59941378482669)) ;
#84318 = CARTESIAN_POINT('Ctrl Pts',(-1.4727084914817,-0.343100689898983,
7.61281114943883)) ;
#84319 = CARTESIAN_POINT('Ctrl Pts',(-1.41699909629399,-0.527943361805503,
7.62308018676697)) ;
#84320 = CARTESIAN_POINT('Ctrl Pts',(-1.23503998147008,-0.874470527776589,
7.64233169598759)) ;
#84321 = CARTESIAN_POINT('Ctrl Pts',(-1.10751742534909,-1.03124396290167,
7.65244354199804)) ;
#84322 = CARTESIAN_POINT('Ctrl Pts',(-0.80137955361333,-1.2830869061876,7.67416824453285)) ;
#84323 = CARTESIAN_POINT('Ctrl Pts',(-0.626796522977761,-1.37682605537175,
7.68517173976574)) ;
#84324 = CARTESIAN_POINT('Ctrl Pts',(-0.257489486781775,-1.4898930142487,
7.70608078168688)) ;
#84325 = CARTESIAN_POINT('Ctrl Pts',(-0.0669875740693966,-1.51048940633529,
7.71523568644169)) ;
#84326 = CARTESIAN_POINT('Ctrl Pts',(0.32051462680166,-1.47879221828775,7.73475987221949)) ;
#84327 = CARTESIAN_POINT('Ctrl Pts',(0.513520886644871,-1.42331700179412,
7.74558686846174)) ;
#84328 = CARTESIAN_POINT('Ctrl Pts',(0.862330105706918,-1.24258946154641,
7.76738916928984)) ;
#84329 = CARTESIAN_POINT('Ctrl Pts',(1.01566751877847,-1.12074684324605,7.77815113619099)) ;
#84330 = CARTESIAN_POINT('Ctrl Pts',(1.2661792463292,-0.826861703363028,7.79836736341024)) ;
#84331 = CARTESIAN_POINT('Ctrl Pts',(1.3615516870939,-0.658094117149608,7.80718921571392)) ;
#84332 = CARTESIAN_POINT('Ctrl Pts',(1.48575203610995,-0.286847017644384,
7.82781405457532)) ;
#84333 = CARTESIAN_POINT('Ctrl Pts',(1.51067710287673,-0.0870855361917978,
7.83891191465601)) ;
#84334 = CARTESIAN_POINT('Ctrl Pts',(1.48155691646122,0.302938128189284,7.86057989601052)) ;
#84335 = CARTESIAN_POINT('Ctrl Pts',(1.43072661101655,0.489718620170333,7.87095659000947)) ;
#84336 = CARTESIAN_POINT('Ctrl Pts',(1.25865525265882,0.8396664471157,7.89039813595088)) ;
#84337 = CARTESIAN_POINT('Ctrl Pts',(1.13686882978925,0.998401435207855,7.90011907945755)) ;
#84338 = CARTESIAN_POINT('Ctrl Pts',(0.839566688676397,1.25852222601811,7.92164861291357)) ;
#84339 = CARTESIAN_POINT('Ctrl Pts',(0.667338761300122,1.35772216803583,7.93269048687789)) ;
#84340 = CARTESIAN_POINT('Ctrl Pts',(0.309739960677104,1.47875080212639,7.95325737369721)) ;
#84341 = CARTESIAN_POINT('Ctrl Pts',(0.129593969136037,1.50526254987928,7.96236872531174)) ;
#84342 = CARTESIAN_POINT('Ctrl Pts',(-0.2334837963999,1.49293881233257,7.98017963849379)) ;
#84343 = CARTESIAN_POINT('Ctrl Pts',(-0.413384241403028,1.45343527784404,
7.98993242309205)) ;
#84344 = CARTESIAN_POINT('Ctrl Pts',(-0.581737793027622,1.38259941420621,
8.)) ;
#84345 = CARTESIAN_POINT('',(0.581737793027052,1.38259941420645,8.)) ;
#84346 = CARTESIAN_POINT('Origin',(0.,0.,8.)) ;
#84347 = CARTESIAN_POINT('Ctrl Pts',(0.581737793026286,1.38259941420677,8.00000000000004)) ;
#84348 = CARTESIAN_POINT('Ctrl Pts',(0.67475850150618,1.34346033957619,7.99443734255911)) ;
#84349 = CARTESIAN_POINT('Ctrl Pts',(0.763582990950793,1.29503877601366,7.98881872888587)) ;
#84350 = CARTESIAN_POINT('Ctrl Pts',(0.929533949930955,1.18152247381298,7.97768117903257)) ;
#84351 = CARTESIAN_POINT('Ctrl Pts',(1.00632475086677,1.11684435455,7.97218996547596)) ;
#84352 = CARTESIAN_POINT('Ctrl Pts',(1.21089201470299,0.906188142783699,7.95649615696774)) ;
#84353 = CARTESIAN_POINT('Ctrl Pts',(1.31753983147867,0.742644036694035,7.94750800203856)) ;
#84354 = CARTESIAN_POINT('Ctrl Pts',(1.46276050636553,0.384267716790858,7.92759820648838)) ;
#84355 = CARTESIAN_POINT('Ctrl Pts',(1.50003763254766,0.19287700920056,7.91696538940003)) ;
#84356 = CARTESIAN_POINT('Ctrl Pts',(1.49996080802917,-0.201167980378509,
7.89507400109008)) ;
#84357 = CARTESIAN_POINT('Ctrl Pts',(1.45957105504829,-0.400026721363593,
7.88402629325758)) ;
#84358 = CARTESIAN_POINT('Ctrl Pts',(1.306992989412,-0.760247630347313,7.86401402053627)) ;
#84359 = CARTESIAN_POINT('Ctrl Pts',(1.20013180168387,-0.919727078186579,
7.85511006050304)) ;
#84360 = CARTESIAN_POINT('Ctrl Pts',(0.928798149448953,-1.19396261027086,
7.83443786040419)) ;
#84361 = CARTESIAN_POINT('Ctrl Pts',(0.765468514485824,-1.30470859053651,
7.82350338244853)) ;
#84362 = CARTESIAN_POINT('Ctrl Pts',(0.402536691306379,-1.4585819400554,7.8017675572555)) ;
#84363 = CARTESIAN_POINT('Ctrl Pts',(0.20592642872561,-1.49903910617981,7.7911843314165)) ;
#84364 = CARTESIAN_POINT('Ctrl Pts',(-0.183266169425525,-1.50088711532144,
7.77240796022013)) ;
#84365 = CARTESIAN_POINT('Ctrl Pts',(-0.37217407632198,-1.46553401384534,
7.76238637789988)) ;
#84366 = CARTESIAN_POINT('Ctrl Pts',(-0.733536341658091,-1.32327533097475,
7.74104869772291)) ;
#84367 = CARTESIAN_POINT('Ctrl Pts',(-0.901472357833655,-1.21510701387381,
7.72996419690242)) ;
#84368 = CARTESIAN_POINT('Ctrl Pts',(-1.18389796843274,-0.941565603956125,
7.70877761587926)) ;
#84369 = CARTESIAN_POINT('Ctrl Pts',(-1.2962998624187,-0.779587835417801,
7.69956043530099)) ;
#84370 = CARTESIAN_POINT('Ctrl Pts',(-1.45166388269414,-0.424032599075321,
7.6798073666153)) ;
#84371 = CARTESIAN_POINT('Ctrl Pts',(-1.49406770049158,-0.234256040953705,
7.66926422449743)) ;
#84372 = CARTESIAN_POINT('Ctrl Pts',(-1.49980716686,-0.0277811177528503,7.65779339543071)) ;
#84373 = CARTESIAN_POINT('Ctrl Pts',(-1.5,-0.0138864685015336,7.65702147047229)) ;
#84374 = CARTESIAN_POINT('Ctrl Pts',(-1.5,-9.66814085323955E-15,7.65624999999999)) ;
#84375 = CARTESIAN_POINT('Origin',(2.07158391530995E-14,-2.18372685607914E-14,
10.5)) ;
#84376 = CARTESIAN_POINT('',(-0.214086590007418,-0.905647899858313,8.375)) ;
#84377 = CARTESIAN_POINT('',(0.214086590007422,-0.905647899858319,8.375)) ;
#84378 = CARTESIAN_POINT('Origin',(1.33147826576248E-14,-2.18372685607914E-14,
8.375)) ;
#84379 = CARTESIAN_POINT('',(-0.378092453297405,-1.38212190130695,10.249595595364)) ;
#84380 = CARTESIAN_POINT('Ctrl Pts',(-0.214086590007057,-0.905647899857255,
8.37499999999588)) ;
#84381 = CARTESIAN_POINT('Ctrl Pts',(-0.279010764447842,-1.09462213691599,
9.11708670956764)) ;
#84382 = CARTESIAN_POINT('Ctrl Pts',(-0.378092453294835,-1.38212190129948,
10.2495955953347)) ;
#84383 = CARTESIAN_POINT('',(0.378092453297409,-1.38212190130694,10.249595595364)) ;
#84384 = CARTESIAN_POINT('Origin',(-5.47577883755165E-29,-2.39231904255907E-14,
10.2495955953641)) ;
#84385 = CARTESIAN_POINT('Ctrl Pts',(0.214086590007062,-0.90564789985724,
8.37499999999589)) ;
#84386 = CARTESIAN_POINT('Ctrl Pts',(0.279010764452302,-1.09462213692897,
9.11708670961856)) ;
#84387 = CARTESIAN_POINT('Ctrl Pts',(0.378092453297408,-1.38212190130698,
10.249595595364)) ;
#84388 = CARTESIAN_POINT('Origin',(0.,0.,10.5)) ;
#84389 = CARTESIAN_POINT('',(0.905647899858292,-0.214086590007431,8.375)) ;
#84390 = CARTESIAN_POINT('',(0.905647899858297,0.214086590007409,8.375)) ;
#84391 = CARTESIAN_POINT('Origin',(0.,0.,8.375)) ;
#84392 = CARTESIAN_POINT('',(1.38212190130692,-0.378092453297421,10.2495955953641)) ;
#84393 = CARTESIAN_POINT('Ctrl Pts',(0.905647899857241,-0.21408659000707,
8.37499999999588)) ;
#84394 = CARTESIAN_POINT('Ctrl Pts',(1.09462213691615,-0.279010764447917,
9.11708670956834)) ;
#84395 = CARTESIAN_POINT('Ctrl Pts',(1.38212190129946,-0.37809245329485,10.2495955953347)) ;
#84396 = CARTESIAN_POINT('',(1.38212190130692,0.378092453297394,10.2495955953641)) ;
#84397 = CARTESIAN_POINT('Origin',(0.,-8.23993651088983E-15,10.2495955953641)) ;
#84398 = CARTESIAN_POINT('Ctrl Pts',(0.905647899857261,0.214086590007048,
8.37499999999588)) ;
#84399 = CARTESIAN_POINT('Ctrl Pts',(1.09462213691212,0.279010764446507,9.11708670955249)) ;
#84400 = CARTESIAN_POINT('Ctrl Pts',(1.38212190130691,0.378092453297394,10.2495955953641)) ;
#84401 = CARTESIAN_POINT('Origin',(0.,-5.20417042793042E-15,9.0585454011027)) ;
#84402 = CARTESIAN_POINT('',(-3.49510952379173E-16,2.85397350993377,9.39035876017455)) ;
#84403 = CARTESIAN_POINT('Origin',(0.,-5.89341654657538E-15,9.39035876017455)) ;
#84404 = CARTESIAN_POINT('',(-3.67394039744206E-16,3.,9.05854540110271)) ;
#84405 = CARTESIAN_POINT('Origin',(-3.12284933782575E-16,2.54999999999999,
9.05854540110271)) ;
#84406 = CARTESIAN_POINT('',(2.99999999999999,-3.67394039744205E-16,9.05854540110271)) ;
#84407 = CARTESIAN_POINT('Origin',(0.,-5.23876967272948E-15,9.0585454011027)) ;
#84408 = CARTESIAN_POINT('Origin',(0.,-5.23876967272948E-15,9.0585454011027)) ;
#84409 = CARTESIAN_POINT('Origin',(0.,-8.23993651088983E-15,6.275)) ;
#84410 = CARTESIAN_POINT('',(0.378092453297396,1.38212190130692,10.2495955953641)) ;
#84411 = CARTESIAN_POINT('',(-0.378092453297399,1.38212190130692,10.2495955953641)) ;
#84412 = CARTESIAN_POINT('Origin',(0.,-8.23993651088983E-15,10.2495955953641)) ;
#84413 = CARTESIAN_POINT('',(0.39252831458563,0.748513789365911,10.414598244924)) ;
#84414 = CARTESIAN_POINT('Origin',(0.0301297752810506,-8.23524087264071E-15,
6.27236398622833)) ;
#84415 = CARTESIAN_POINT('',(0.498545645256686,0.498545645256685,10.4407567714872)) ;
#84416 = CARTESIAN_POINT('Origin',(0.263070324890146,0.108967296427384,6.25008801707577)) ;
#84417 = CARTESIAN_POINT('',(0.748513789365912,0.392528314585628,10.414598244924)) ;
#84418 = CARTESIAN_POINT('Origin',(0.108967296427394,0.263070324890141,6.25008801707577)) ;
#84419 = CARTESIAN_POINT('Origin',(0.,0.0301297752810484,6.27236398622833)) ;
#84420 = CARTESIAN_POINT('',(0.748513789365931,-0.392528314585653,10.414598244924)) ;
#84421 = CARTESIAN_POINT('Origin',(-1.05702599154822E-16,-0.0301297752810628,
6.27236398622833)) ;
#84422 = CARTESIAN_POINT('',(0.498545645256703,-0.498545645256708,10.4407567714872)) ;
#84423 = CARTESIAN_POINT('Origin',(0.108967296427393,-0.263070324890159,6.25008801707577)) ;
#84424 = CARTESIAN_POINT('',(0.392528314585646,-0.748513789365934,10.414598244924)) ;
#84425 = CARTESIAN_POINT('Origin',(0.263070324890154,-0.108967296427406,6.25008801707577)) ;
#84426 = CARTESIAN_POINT('Origin',(0.0301297752810606,-8.33993336976058E-15,
6.27236398622833)) ;
#84427 = CARTESIAN_POINT('',(-0.392528314585635,-0.74851378936595,10.414598244924)) ;
#84428 = CARTESIAN_POINT('Origin',(-0.0301297752810506,-8.02383567433109E-15,
6.27236398622833)) ;
#84429 = CARTESIAN_POINT('',(-0.49854564525669,-0.498545645256722,10.4407567714872)) ;
#84430 = CARTESIAN_POINT('Origin',(-0.26307032489015,-0.1089672964274,6.25008801707577)) ;
#84431 = CARTESIAN_POINT('',(-0.748513789365915,-0.392528314585664,10.414598244924)) ;
#84432 = CARTESIAN_POINT('Origin',(-0.108967296427399,-0.263070324890164,
6.25008801707577)) ;
#84433 = CARTESIAN_POINT('',(-1.38212190130693,-0.378092453297424,10.249595595364)) ;
#84434 = CARTESIAN_POINT('Origin',(-2.1039509627475E-16,-0.0301297752810731,
6.27236398622833)) ;
#84435 = CARTESIAN_POINT('',(-1.38212190130693,0.37809245329739,10.249595595364)) ;
#84436 = CARTESIAN_POINT('Origin',(-7.84162695735042E-15,-1.60815634682402E-14,
10.2495955953641)) ;
#84437 = CARTESIAN_POINT('',(-0.748513789365927,0.392528314585617,10.414598244924)) ;
#84438 = CARTESIAN_POINT('Origin',(3.16097695429417E-16,0.0301297752810384,
6.27236398622833)) ;
#84439 = CARTESIAN_POINT('',(-0.4985456452567,0.498545645256671,10.4407567714872)) ;
#84440 = CARTESIAN_POINT('Origin',(-0.108967296427388,0.263070324890137,6.25008801707577)) ;
#84441 = CARTESIAN_POINT('',(-0.392528314585641,0.748513789365896,10.414598244924)) ;
#84442 = CARTESIAN_POINT('Origin',(-0.26307032489015,0.10896729642739,6.25008801707577)) ;
#84443 = CARTESIAN_POINT('Origin',(-0.0301297752810606,-7.91914317721115E-15,
6.27236398622833)) ;
#84444 = CARTESIAN_POINT('Origin',(0.,0.,0.)) ;
#84445 = CARTESIAN_POINT('',(-3.67394039744206E-16,2.99999999999999,8.45)) ;
#84446 = CARTESIAN_POINT('',(2.99999999999999,-3.67394039744205E-16,8.44999999999999)) ;
#84447 = CARTESIAN_POINT('Origin',(0.,-4.0381478968626E-15,8.44999999999999)) ;
#84448 = CARTESIAN_POINT('',(2.99999999999999,-3.67394039744205E-16,0.)) ;
#84449 = CARTESIAN_POINT('Origin',(0.,-4.0381478968626E-15,8.44999999999999)) ;
#84450 = CARTESIAN_POINT('Origin',(0.,-4.33680868994202E-15,8.44999999999999)) ;
#84451 = CARTESIAN_POINT('',(-3.12284933782575E-16,2.54999999999999,8.)) ;
#84452 = CARTESIAN_POINT('Origin',(-3.12284933782575E-16,2.55,8.45)) ;
#84453 = CARTESIAN_POINT('Origin',(0.,-3.15032621887263E-15,7.99999999999999)) ;
#84454 = CARTESIAN_POINT('Origin',(0.,-8.094915342364E-15,8.)) ;
#84455 = CARTESIAN_POINT('Ctrl Pts',(-0.581737793027625,1.38259941420621,
8.)) ;
#84456 = CARTESIAN_POINT('Ctrl Pts',(-0.729864874634484,1.3029320087127,8.)) ;
#84457 = CARTESIAN_POINT('Ctrl Pts',(-0.863262176577335,1.19854179063676,
7.99999999999998)) ;
#84458 = CARTESIAN_POINT('Ctrl Pts',(-1.11135289090838,0.924723635099756,
7.99999999999998)) ;
#84459 = CARTESIAN_POINT('Ctrl Pts',(-1.19622518509719,0.769719328397424,
7.9999999998933)) ;
#84460 = CARTESIAN_POINT('Ctrl Pts',(-1.3131079977207,0.4825998456181,7.9999999998933)) ;
#84461 = CARTESIAN_POINT('Ctrl Pts',(-1.34659883481402,0.308343046285069,
8.)) ;
#84462 = CARTESIAN_POINT('Ctrl Pts',(-1.3439581077645,-0.0381523603338236,
8.)) ;
#84463 = CARTESIAN_POINT('Ctrl Pts',(-1.30980794379433,-0.207008363331256,
8.)) ;
#84464 = CARTESIAN_POINT('Ctrl Pts',(-1.1949082548263,-0.485324594498909,
8.)) ;
#84465 = CARTESIAN_POINT('Ctrl Pts',(-1.11064003044993,-0.640909763593095,
7.99999999998602)) ;
#84466 = CARTESIAN_POINT('Ctrl Pts',(-0.89560004435886,-0.855220230784529,
7.99999999998602)) ;
#84467 = CARTESIAN_POINT('Ctrl Pts',(-0.813300635214957,-0.91826563598073,
8.)) ;
#84468 = CARTESIAN_POINT('Ctrl Pts',(-0.639506338952977,-1.01853200109966,
8.)) ;
#84469 = CARTESIAN_POINT('Ctrl Pts',(-0.549475089174124,-1.0566200499526,
8.)) ;
#84470 = CARTESIAN_POINT('Ctrl Pts',(-0.455787866251369,-1.08325786021637,
8.)) ;
#84471 = CARTESIAN_POINT('Ctrl Pts',(0.455787866252654,-1.08325786021595,
8.)) ;
#84472 = CARTESIAN_POINT('Ctrl Pts',(0.572824329435331,-1.0499812297112,8.)) ;
#84473 = CARTESIAN_POINT('Ctrl Pts',(0.684011935637464,-0.998876628478368,
8.)) ;
#84474 = CARTESIAN_POINT('Ctrl Pts',(0.903757997974771,-0.853530202235782,
8.)) ;
#84475 = CARTESIAN_POINT('Ctrl Pts',(1.00703055401931,-0.754755114613078,
7.99999999999225)) ;
#84476 = CARTESIAN_POINT('Ctrl Pts',(1.15763806880758,-0.548083195129258,
7.99999999999225)) ;
#84477 = CARTESIAN_POINT('Ctrl Pts',(1.25545705153481,-0.389463905034916,
8.00000000003248)) ;
#84478 = CARTESIAN_POINT('Ctrl Pts',(1.34993353979521,0.00500026766052222,
8.00000000003248)) ;
#84479 = CARTESIAN_POINT('Ctrl Pts',(1.35637890633501,0.183538835590366,8.)) ;
#84480 = CARTESIAN_POINT('Ctrl Pts',(1.29407820061595,0.563580295571493,8.)) ;
#84481 = CARTESIAN_POINT('Ctrl Pts',(1.21679738901834,0.732819558362854,7.99999999999994)) ;
#84482 = CARTESIAN_POINT('Ctrl Pts',(1.06567098606457,0.974403116538763,7.99999999999994)) ;
#84483 = CARTESIAN_POINT('Ctrl Pts',(0.983776834865333,1.07380659930599,8.)) ;
#84484 = CARTESIAN_POINT('Ctrl Pts',(0.797226824491547,1.24808435953097,8.)) ;
#84485 = CARTESIAN_POINT('Ctrl Pts',(0.693609148877066,1.32243147885714,8.)) ;
#84486 = CARTESIAN_POINT('Ctrl Pts',(0.581737793027051,1.38259941420645,8.)) ;
#84487 = CARTESIAN_POINT('Ctrl Pts',(0.00408156060463945,1.5000051209297,
0.0310476188649207)) ;
#84488 = CARTESIAN_POINT('Ctrl Pts',(-0.864669974149657,1.50236902088577,
0.0727794857188941)) ;
#84489 = CARTESIAN_POINT('Ctrl Pts',(-1.29904734958516,0.750005336973063,
0.114577170727664)) ;
#84490 = CARTESIAN_POINT('Ctrl Pts',(-1.73206313278021,1.06058278574021E-16,
0.15624383739433)) ;
#84491 = CARTESIAN_POINT('Ctrl Pts',(-1.29904734958516,-0.750005336973063,
0.197910504060997)) ;
#84492 = CARTESIAN_POINT('Ctrl Pts',(-0.866031566390109,-1.50001067394612,
0.239577170727664)) ;
#84493 = CARTESIAN_POINT('Ctrl Pts',(-1.83698327053499E-16,-1.50001067394612,
0.28124383739433)) ;
#84494 = CARTESIAN_POINT('Ctrl Pts',(0.866031566390108,-1.50001067394612,
0.322910504060997)) ;
#84495 = CARTESIAN_POINT('Ctrl Pts',(1.29904734958516,-0.750005336973063,
0.364577170727663)) ;
#84496 = CARTESIAN_POINT('Ctrl Pts',(1.73206313278021,-3.18174835722064E-16,
0.40624383739433)) ;
#84497 = CARTESIAN_POINT('Ctrl Pts',(1.29904734958516,0.750005336973062,0.447910504060997)) ;
#84498 = CARTESIAN_POINT('Ctrl Pts',(0.866031566390109,1.50001067394612,0.489577170727663)) ;
#84499 = CARTESIAN_POINT('Ctrl Pts',(0.,1.50001067394612,0.53124383739433)) ;
#84500 = CARTESIAN_POINT('Ctrl Pts',(-0.866031566390108,1.50001067394612,
0.572910504060996)) ;
#84501 = CARTESIAN_POINT('Ctrl Pts',(-1.29904734958516,0.750005336973063,
0.614577170727663)) ;
#84502 = CARTESIAN_POINT('Ctrl Pts',(-1.73206313278021,1.06058278574021E-16,
0.656243837394329)) ;
#84503 = CARTESIAN_POINT('Ctrl Pts',(-1.29904734958516,-0.750005336973063,
0.697910504060997)) ;
#84504 = CARTESIAN_POINT('Ctrl Pts',(-0.866031566390109,-1.50001067394612,
0.739577170727663)) ;
#84505 = CARTESIAN_POINT('Ctrl Pts',(-1.83698327053499E-16,-1.50001067394612,
0.78124383739433)) ;
#84506 = CARTESIAN_POINT('Ctrl Pts',(0.866031566390108,-1.50001067394612,
0.822910504060996)) ;
#84507 = CARTESIAN_POINT('Ctrl Pts',(1.29904734958516,-0.750005336973063,
0.864577170727663)) ;
#84508 = CARTESIAN_POINT('Ctrl Pts',(1.73206313278021,-3.18174835722064E-16,
0.906243837394329)) ;
#84509 = CARTESIAN_POINT('Ctrl Pts',(1.29904734958516,0.750005336973062,0.947910504060997)) ;
#84510 = CARTESIAN_POINT('Ctrl Pts',(0.866031566390109,1.50001067394612,0.989577170727662)) ;
#84511 = CARTESIAN_POINT('Ctrl Pts',(0.,1.50001067394612,1.03124383739434)) ;
#84512 = CARTESIAN_POINT('Ctrl Pts',(-0.866031566390108,1.50001067394612,
1.072910504061)) ;
#84513 = CARTESIAN_POINT('Ctrl Pts',(-1.29904734958516,0.750005336973063,
1.11457717072767)) ;
#84514 = CARTESIAN_POINT('Ctrl Pts',(-1.73206313278021,1.06058278574021E-16,
1.15624383739434)) ;
#84515 = CARTESIAN_POINT('Ctrl Pts',(-1.29904734958516,-0.750005336973063,
1.197910504061)) ;
#84516 = CARTESIAN_POINT('Ctrl Pts',(-0.866031566390109,-1.50001067394612,
1.23957717072767)) ;
#84517 = CARTESIAN_POINT('Ctrl Pts',(-1.83698327053499E-16,-1.50001067394612,
1.28124383739434)) ;
#84518 = CARTESIAN_POINT('Ctrl Pts',(0.866031566390108,-1.50001067394612,
1.322910504061)) ;
#84519 = CARTESIAN_POINT('Ctrl Pts',(1.29904734958516,-0.750005336973063,
1.36457717072767)) ;
#84520 = CARTESIAN_POINT('Ctrl Pts',(1.73206313278021,-3.18174835722064E-16,
1.40624383739433)) ;
#84521 = CARTESIAN_POINT('Ctrl Pts',(1.29904734958516,0.750005336973062,1.447910504061)) ;
#84522 = CARTESIAN_POINT('Ctrl Pts',(0.866031566390109,1.50001067394612,1.48957717072767)) ;
#84523 = CARTESIAN_POINT('Ctrl Pts',(0.,1.50001067394612,1.53124383739433)) ;
#84524 = CARTESIAN_POINT('Ctrl Pts',(-0.866031566390108,1.50001067394612,
1.572910504061)) ;
#84525 = CARTESIAN_POINT('Ctrl Pts',(-1.29904734958516,0.750005336973063,
1.61457717072767)) ;
#84526 = CARTESIAN_POINT('Ctrl Pts',(-1.73206313278021,1.06058278574021E-16,
1.65624383739433)) ;
#84527 = CARTESIAN_POINT('Ctrl Pts',(-1.29904734958516,-0.750005336973063,
1.697910504061)) ;
#84528 = CARTESIAN_POINT('Ctrl Pts',(-0.866031566390109,-1.50001067394612,
1.73957717072767)) ;
#84529 = CARTESIAN_POINT('Ctrl Pts',(-1.83698327053499E-16,-1.50001067394612,
1.78124383739433)) ;
#84530 = CARTESIAN_POINT('Ctrl Pts',(0.866031566390108,-1.50001067394612,
1.822910504061)) ;
#84531 = CARTESIAN_POINT('Ctrl Pts',(1.29904734958516,-0.750005336973063,
1.86457717072767)) ;
#84532 = CARTESIAN_POINT('Ctrl Pts',(1.73206313278021,-3.18174835722064E-16,
1.90624383739433)) ;
#84533 = CARTESIAN_POINT('Ctrl Pts',(1.29904734958516,0.750005336973062,1.947910504061)) ;
#84534 = CARTESIAN_POINT('Ctrl Pts',(0.866031566390109,1.50001067394612,1.98957717072767)) ;
#84535 = CARTESIAN_POINT('Ctrl Pts',(0.,1.50001067394612,2.03124383739433)) ;
#84536 = CARTESIAN_POINT('Ctrl Pts',(-0.866031566390108,1.50001067394612,
2.072910504061)) ;
#84537 = CARTESIAN_POINT('Ctrl Pts',(-1.29904734958516,0.750005336973063,
2.11457717072767)) ;
#84538 = CARTESIAN_POINT('Ctrl Pts',(-1.73206313278021,1.06058278574021E-16,
2.15624383739433)) ;
#84539 = CARTESIAN_POINT('Ctrl Pts',(-1.29904734958516,-0.750005336973063,
2.197910504061)) ;
#84540 = CARTESIAN_POINT('Ctrl Pts',(-0.866031566390109,-1.50001067394612,
2.23957717072767)) ;
#84541 = CARTESIAN_POINT('Ctrl Pts',(-1.83698327053499E-16,-1.50001067394612,
2.28124383739433)) ;
#84542 = CARTESIAN_POINT('Ctrl Pts',(0.866031566390108,-1.50001067394612,
2.322910504061)) ;
#84543 = CARTESIAN_POINT('Ctrl Pts',(1.29904734958516,-0.750005336973063,
2.36457717072767)) ;
#84544 = CARTESIAN_POINT('Ctrl Pts',(1.73206313278021,-3.18174835722064E-16,
2.40624383739433)) ;
#84545 = CARTESIAN_POINT('Ctrl Pts',(1.29904734958516,0.750005336973062,2.447910504061)) ;
#84546 = CARTESIAN_POINT('Ctrl Pts',(0.866031566390109,1.50001067394612,2.48957717072767)) ;
#84547 = CARTESIAN_POINT('Ctrl Pts',(0.,1.50001067394612,2.53124383739433)) ;
#84548 = CARTESIAN_POINT('Ctrl Pts',(-0.866031566390108,1.50001067394612,
2.572910504061)) ;
#84549 = CARTESIAN_POINT('Ctrl Pts',(-1.29904734958516,0.750005336973063,
2.61457717072767)) ;
#84550 = CARTESIAN_POINT('Ctrl Pts',(-1.73206313278021,1.06058278574021E-16,
2.65624383739433)) ;
#84551 = CARTESIAN_POINT('Ctrl Pts',(-1.29904734958516,-0.750005336973063,
2.697910504061)) ;
#84552 = CARTESIAN_POINT('Ctrl Pts',(-0.866031566390109,-1.50001067394612,
2.73957717072767)) ;
#84553 = CARTESIAN_POINT('Ctrl Pts',(-1.83698327053499E-16,-1.50001067394612,
2.78124383739433)) ;
#84554 = CARTESIAN_POINT('Ctrl Pts',(0.866031566390108,-1.50001067394612,
2.822910504061)) ;
#84555 = CARTESIAN_POINT('Ctrl Pts',(1.29904734958516,-0.750005336973063,
2.86457717072767)) ;
#84556 = CARTESIAN_POINT('Ctrl Pts',(1.73206313278021,-3.18174835722064E-16,
2.90624383739433)) ;
#84557 = CARTESIAN_POINT('Ctrl Pts',(1.29904734958516,0.750005336973062,2.947910504061)) ;
#84558 = CARTESIAN_POINT('Ctrl Pts',(0.866031566390109,1.50001067394612,2.98957717072767)) ;
#84559 = CARTESIAN_POINT('Ctrl Pts',(0.,1.50001067394612,3.03124383739433)) ;
#84560 = CARTESIAN_POINT('Ctrl Pts',(-0.866031566390108,1.50001067394612,
3.072910504061)) ;
#84561 = CARTESIAN_POINT('Ctrl Pts',(-1.29904734958516,0.750005336973063,
3.11457717072766)) ;
#84562 = CARTESIAN_POINT('Ctrl Pts',(-1.73206313278021,1.06058278574021E-16,
3.15624383739433)) ;
#84563 = CARTESIAN_POINT('Ctrl Pts',(-1.29904734958516,-0.750005336973063,
3.197910504061)) ;
#84564 = CARTESIAN_POINT('Ctrl Pts',(-0.866031566390109,-1.50001067394612,
3.23957717072767)) ;
#84565 = CARTESIAN_POINT('Ctrl Pts',(-1.83698327053499E-16,-1.50001067394612,
3.28124383739433)) ;
#84566 = CARTESIAN_POINT('Ctrl Pts',(0.866031566390108,-1.50001067394612,
3.32291050406099)) ;
#84567 = CARTESIAN_POINT('Ctrl Pts',(1.29904734958516,-0.750005336973063,
3.36457717072766)) ;
#84568 = CARTESIAN_POINT('Ctrl Pts',(1.73206313278021,-3.18174835722064E-16,
3.40624383739432)) ;
#84569 = CARTESIAN_POINT('Ctrl Pts',(1.29904734958516,0.750005336973062,3.447910504061)) ;
#84570 = CARTESIAN_POINT('Ctrl Pts',(0.866031566390109,1.50001067394612,3.48957717072766)) ;
#84571 = CARTESIAN_POINT('Ctrl Pts',(0.,1.50001067394612,3.53124383739433)) ;
#84572 = CARTESIAN_POINT('Ctrl Pts',(-0.866031566390108,1.50001067394612,
3.572910504061)) ;
#84573 = CARTESIAN_POINT('Ctrl Pts',(-1.29904734958516,0.750005336973063,
3.61457717072766)) ;
#84574 = CARTESIAN_POINT('Ctrl Pts',(-1.73206313278021,1.06058278574021E-16,
3.65624383739433)) ;
#84575 = CARTESIAN_POINT('Ctrl Pts',(-1.29904734958516,-0.750005336973063,
3.697910504061)) ;
#84576 = CARTESIAN_POINT('Ctrl Pts',(-0.866031566390109,-1.50001067394612,
3.73957717072766)) ;
#84577 = CARTESIAN_POINT('Ctrl Pts',(-1.83698327053499E-16,-1.50001067394612,
3.78124383739433)) ;
#84578 = CARTESIAN_POINT('Ctrl Pts',(0.866031566390108,-1.50001067394612,
3.822910504061)) ;
#84579 = CARTESIAN_POINT('Ctrl Pts',(1.29904734958516,-0.750005336973063,
3.86457717072766)) ;
#84580 = CARTESIAN_POINT('Ctrl Pts',(1.73206313278021,-3.18174835722064E-16,
3.90624383739433)) ;
#84581 = CARTESIAN_POINT('Ctrl Pts',(1.29904734958516,0.750005336973062,3.947910504061)) ;
#84582 = CARTESIAN_POINT('Ctrl Pts',(0.866031566390109,1.50001067394612,3.98957717072766)) ;
#84583 = CARTESIAN_POINT('Ctrl Pts',(0.,1.50001067394612,4.03124383739433)) ;
#84584 = CARTESIAN_POINT('Ctrl Pts',(-0.866031566390108,1.50001067394612,
4.07291050406099)) ;
#84585 = CARTESIAN_POINT('Ctrl Pts',(-1.29904734958516,0.750005336973063,
4.11457717072766)) ;
#84586 = CARTESIAN_POINT('Ctrl Pts',(-1.73206313278021,1.06058278574021E-16,
4.15624383739433)) ;
#84587 = CARTESIAN_POINT('Ctrl Pts',(-1.29904734958516,-0.750005336973063,
4.197910504061)) ;
#84588 = CARTESIAN_POINT('Ctrl Pts',(-0.866031566390109,-1.50001067394612,
4.23957717072765)) ;
#84589 = CARTESIAN_POINT('Ctrl Pts',(-1.83698327053499E-16,-1.50001067394612,
4.28124383739433)) ;
#84590 = CARTESIAN_POINT('Ctrl Pts',(0.866031566390108,-1.50001067394612,
4.322910504061)) ;
#84591 = CARTESIAN_POINT('Ctrl Pts',(1.29904734958516,-0.750005336973063,
4.36457717072766)) ;
#84592 = CARTESIAN_POINT('Ctrl Pts',(1.73206313278021,-3.18174835722064E-16,
4.40624383739433)) ;
#84593 = CARTESIAN_POINT('Ctrl Pts',(1.29904734958516,0.750005336973062,4.447910504061)) ;
#84594 = CARTESIAN_POINT('Ctrl Pts',(0.866031566390109,1.50001067394612,4.48957717072766)) ;
#84595 = CARTESIAN_POINT('Ctrl Pts',(0.,1.50001067394612,4.53124383739433)) ;
#84596 = CARTESIAN_POINT('Ctrl Pts',(-0.866031566390108,1.50001067394612,
4.572910504061)) ;
#84597 = CARTESIAN_POINT('Ctrl Pts',(-1.29904734958516,0.750005336973063,
4.61457717072766)) ;
#84598 = CARTESIAN_POINT('Ctrl Pts',(-1.73206313278021,1.06058278574021E-16,
4.65624383739433)) ;
#84599 = CARTESIAN_POINT('Ctrl Pts',(-1.29904734958516,-0.750005336973063,
4.69791050406099)) ;
#84600 = CARTESIAN_POINT('Ctrl Pts',(-0.866031566390109,-1.50001067394612,
4.73957717072766)) ;
#84601 = CARTESIAN_POINT('Ctrl Pts',(-1.83698327053499E-16,-1.50001067394612,
4.78124383739433)) ;
#84602 = CARTESIAN_POINT('Ctrl Pts',(0.866031566390108,-1.50001067394612,
4.822910504061)) ;
#84603 = CARTESIAN_POINT('Ctrl Pts',(1.29904734958516,-0.750005336973063,
4.86457717072765)) ;
#84604 = CARTESIAN_POINT('Ctrl Pts',(1.73206313278021,-3.18174835722064E-16,
4.90624383739433)) ;
#84605 = CARTESIAN_POINT('Ctrl Pts',(1.29904734958516,0.750005336973062,4.94791050406099)) ;
#84606 = CARTESIAN_POINT('Ctrl Pts',(0.866031566390109,1.50001067394612,4.98957717072766)) ;
#84607 = CARTESIAN_POINT('Ctrl Pts',(0.,1.50001067394612,5.03124383739433)) ;
#84608 = CARTESIAN_POINT('Ctrl Pts',(-0.866031566390108,1.50001067394612,
5.07291050406099)) ;
#84609 = CARTESIAN_POINT('Ctrl Pts',(-1.29904734958516,0.750005336973063,
5.11457717072766)) ;
#84610 = CARTESIAN_POINT('Ctrl Pts',(-1.73206313278021,1.06058278574021E-16,
5.15624383739433)) ;
#84611 = CARTESIAN_POINT('Ctrl Pts',(-1.29904734958516,-0.750005336973063,
5.19791050406099)) ;
#84612 = CARTESIAN_POINT('Ctrl Pts',(-0.866031566390109,-1.50001067394612,
5.23957717072765)) ;
#84613 = CARTESIAN_POINT('Ctrl Pts',(-1.83698327053499E-16,-1.50001067394612,
5.28124383739433)) ;
#84614 = CARTESIAN_POINT('Ctrl Pts',(0.866031566390108,-1.50001067394612,
5.32291050406099)) ;
#84615 = CARTESIAN_POINT('Ctrl Pts',(1.29904734958516,-0.750005336973063,
5.36457717072766)) ;
#84616 = CARTESIAN_POINT('Ctrl Pts',(1.73206313278021,-3.18174835722064E-16,
5.40624383739433)) ;
#84617 = CARTESIAN_POINT('Ctrl Pts',(1.29904734958516,0.750005336973062,5.44791050406099)) ;
#84618 = CARTESIAN_POINT('Ctrl Pts',(0.866031566390109,1.50001067394612,5.48957717072765)) ;
#84619 = CARTESIAN_POINT('Ctrl Pts',(0.,1.50001067394612,5.53124383739433)) ;
#84620 = CARTESIAN_POINT('Ctrl Pts',(-0.866031566390108,1.50001067394612,
5.57291050406099)) ;
#84621 = CARTESIAN_POINT('Ctrl Pts',(-1.29904734958516,0.750005336973063,
5.61457717072766)) ;
#84622 = CARTESIAN_POINT('Ctrl Pts',(-1.73206313278021,1.06058278574021E-16,
5.65624383739433)) ;
#84623 = CARTESIAN_POINT('Ctrl Pts',(-1.29904734958516,-0.750005336973063,
5.69791050406099)) ;
#84624 = CARTESIAN_POINT('Ctrl Pts',(-0.866031566390109,-1.50001067394612,
5.73957717072766)) ;
#84625 = CARTESIAN_POINT('Ctrl Pts',(-1.83698327053499E-16,-1.50001067394612,
5.78124383739433)) ;
#84626 = CARTESIAN_POINT('Ctrl Pts',(0.866031566390108,-1.50001067394612,
5.82291050406099)) ;
#84627 = CARTESIAN_POINT('Ctrl Pts',(1.29904734958516,-0.750005336973063,
5.86457717072765)) ;
#84628 = CARTESIAN_POINT('Ctrl Pts',(1.73206313278021,-3.18174835722064E-16,
5.90624383739431)) ;
#84629 = CARTESIAN_POINT('Ctrl Pts',(1.29904734958516,0.750005336973062,5.94791050406099)) ;
#84630 = CARTESIAN_POINT('Ctrl Pts',(0.866031566390109,1.50001067394612,5.98957717072766)) ;
#84631 = CARTESIAN_POINT('Ctrl Pts',(0.,1.50001067394612,6.03124383739433)) ;
#84632 = CARTESIAN_POINT('Ctrl Pts',(-0.866031566390108,1.50001067394612,
6.07291050406099)) ;
#84633 = CARTESIAN_POINT('Ctrl Pts',(-1.29904734958516,0.750005336973063,
6.11457717072765)) ;
#84634 = CARTESIAN_POINT('Ctrl Pts',(-1.73206313278021,1.06058278574021E-16,
6.15624383739433)) ;
#84635 = CARTESIAN_POINT('Ctrl Pts',(-1.29904734958516,-0.750005336973063,
6.19791050406099)) ;
#84636 = CARTESIAN_POINT('Ctrl Pts',(-0.866031566390109,-1.50001067394612,
6.23957717072766)) ;
#84637 = CARTESIAN_POINT('Ctrl Pts',(-1.83698327053499E-16,-1.50001067394612,
6.28124383739432)) ;
#84638 = CARTESIAN_POINT('Ctrl Pts',(0.866031566390108,-1.50001067394612,
6.32291050406099)) ;
#84639 = CARTESIAN_POINT('Ctrl Pts',(1.29904734958516,-0.750005336973063,
6.36457717072766)) ;
#84640 = CARTESIAN_POINT('Ctrl Pts',(1.73206313278021,-3.18174835722064E-16,
6.40624383739432)) ;
#84641 = CARTESIAN_POINT('Ctrl Pts',(1.29904734958516,0.750005336973062,6.44791050406099)) ;
#84642 = CARTESIAN_POINT('Ctrl Pts',(0.866031566390109,1.50001067394612,6.48957717072766)) ;
#84643 = CARTESIAN_POINT('Ctrl Pts',(0.,1.50001067394612,6.53124383739432)) ;
#84644 = CARTESIAN_POINT('Ctrl Pts',(-0.866031566390108,1.50001067394612,
6.57291050406099)) ;
#84645 = CARTESIAN_POINT('Ctrl Pts',(-1.29904734958516,0.750005336973063,
6.61457717072766)) ;
#84646 = CARTESIAN_POINT('Ctrl Pts',(-1.73206313278021,1.06058278574021E-16,
6.65624383739432)) ;
#84647 = CARTESIAN_POINT('Ctrl Pts',(-1.29904734958516,-0.750005336973063,
6.69791050406099)) ;
#84648 = CARTESIAN_POINT('Ctrl Pts',(-0.866031566390109,-1.50001067394612,
6.73957717072765)) ;
#84649 = CARTESIAN_POINT('Ctrl Pts',(-1.83698327053499E-16,-1.50001067394612,
6.78124383739432)) ;
#84650 = CARTESIAN_POINT('Ctrl Pts',(0.866031566390108,-1.50001067394612,
6.82291050406099)) ;
#84651 = CARTESIAN_POINT('Ctrl Pts',(1.29904734958516,-0.750005336973063,
6.86457717072766)) ;
#84652 = CARTESIAN_POINT('Ctrl Pts',(1.73206313278021,-3.18174835722064E-16,
6.90624383739432)) ;
#84653 = CARTESIAN_POINT('Ctrl Pts',(1.29904734958516,0.750005336973062,6.94791050406099)) ;
#84654 = CARTESIAN_POINT('Ctrl Pts',(0.866031566390109,1.50001067394612,6.98957717072766)) ;
#84655 = CARTESIAN_POINT('Ctrl Pts',(0.,1.50001067394612,7.03124383739432)) ;
#84656 = CARTESIAN_POINT('Ctrl Pts',(-0.866031566390108,1.50001067394612,
7.07291050406099)) ;
#84657 = CARTESIAN_POINT('Ctrl Pts',(-1.29904734958516,0.750005336973063,
7.11457717072766)) ;
#84658 = CARTESIAN_POINT('Ctrl Pts',(-1.73206313278021,1.06058278574021E-16,
7.15624383739432)) ;
#84659 = CARTESIAN_POINT('Ctrl Pts',(-1.29904734958516,-0.750005336973063,
7.19791050406099)) ;
#84660 = CARTESIAN_POINT('Ctrl Pts',(-0.866031566390109,-1.50001067394612,
7.23957717072766)) ;
#84661 = CARTESIAN_POINT('Ctrl Pts',(-1.83698327053499E-16,-1.50001067394612,
7.28124383739432)) ;
#84662 = CARTESIAN_POINT('Ctrl Pts',(0.866031566390108,-1.50001067394612,
7.32291050406099)) ;
#84663 = CARTESIAN_POINT('Ctrl Pts',(1.29904734958516,-0.750005336973063,
7.36457717072765)) ;
#84664 = CARTESIAN_POINT('Ctrl Pts',(1.73206313278021,-3.18174835722064E-16,
7.40624383739432)) ;
#84665 = CARTESIAN_POINT('Ctrl Pts',(1.29904734958516,0.750005336973062,7.44791050406099)) ;
#84666 = CARTESIAN_POINT('Ctrl Pts',(0.866031566390109,1.50001067394612,7.48957717072766)) ;
#84667 = CARTESIAN_POINT('Ctrl Pts',(0.,1.50001067394612,7.53124383739432)) ;
#84668 = CARTESIAN_POINT('Ctrl Pts',(-0.866031566390108,1.50001067394612,
7.57291050406099)) ;
#84669 = CARTESIAN_POINT('Ctrl Pts',(-1.29904734958516,0.750005336973063,
7.61457717072766)) ;
#84670 = CARTESIAN_POINT('Ctrl Pts',(-1.73206313278021,1.06058278574021E-16,
7.65624383739432)) ;
#84671 = CARTESIAN_POINT('Ctrl Pts',(-1.29904734958516,-0.750005336973063,
7.69791050406099)) ;
#84672 = CARTESIAN_POINT('Ctrl Pts',(-0.866031566390109,-1.50001067394612,
7.73957717072766)) ;
#84673 = CARTESIAN_POINT('Ctrl Pts',(-1.83698327053499E-16,-1.50001067394612,
7.78124383739432)) ;
#84674 = CARTESIAN_POINT('Ctrl Pts',(0.866031566390108,-1.50001067394612,
7.82291050406099)) ;
#84675 = CARTESIAN_POINT('Ctrl Pts',(1.29904734958516,-0.750005336973063,
7.86457717072766)) ;
#84676 = CARTESIAN_POINT('Ctrl Pts',(1.73206313278021,-3.18174835722064E-16,
7.90624383739432)) ;
#84677 = CARTESIAN_POINT('Ctrl Pts',(1.29904734958516,0.750005336973062,7.94791050406099)) ;
#84678 = CARTESIAN_POINT('Ctrl Pts',(0.866031566390109,1.50001067394612,7.98957717072765)) ;
#84679 = CARTESIAN_POINT('Ctrl Pts',(0.,1.50001067394612,8.03124383739432)) ;
#84680 = CARTESIAN_POINT('Ctrl Pts',(-0.866031566390108,1.50001067394612,
8.07291050406099)) ;
#84681 = CARTESIAN_POINT('Ctrl Pts',(-1.29904734958516,0.750005336973063,
8.11457717072765)) ;
#84682 = CARTESIAN_POINT('Ctrl Pts',(-1.73206313278021,1.06058278574021E-16,
8.15624383739432)) ;
#84683 = CARTESIAN_POINT('Ctrl Pts',(-1.29904734958516,-0.750005336973063,
8.19791050406099)) ;
#84684 = CARTESIAN_POINT('Ctrl Pts',(-0.866031566390109,-1.50001067394612,
8.23957717072765)) ;
#84685 = CARTESIAN_POINT('Ctrl Pts',(-1.83698327053499E-16,-1.50001067394612,
8.28124383739432)) ;
#84686 = CARTESIAN_POINT('Ctrl Pts',(0.866031566390108,-1.50001067394612,
8.32291050406099)) ;
#84687 = CARTESIAN_POINT('Ctrl Pts',(1.29904734958516,-0.750005336973063,
8.36457717072766)) ;
#84688 = CARTESIAN_POINT('Ctrl Pts',(1.73206313278021,-3.18174835722064E-16,
8.40624383739432)) ;
#84689 = CARTESIAN_POINT('Ctrl Pts',(1.29904734958516,0.750005336973062,8.44791050406099)) ;
#84690 = CARTESIAN_POINT('Ctrl Pts',(0.866031566390109,1.50001067394612,8.48957717072766)) ;
#84691 = CARTESIAN_POINT('Ctrl Pts',(0.,1.50001067394612,8.53124383739432)) ;
#84692 = CARTESIAN_POINT('Ctrl Pts',(-0.866031566390108,1.50001067394612,
8.57291050406099)) ;
#84693 = CARTESIAN_POINT('Ctrl Pts',(-1.29904734958516,0.750005336973063,
8.61457717072765)) ;
#84694 = CARTESIAN_POINT('Ctrl Pts',(-1.73206313278021,1.06058278574021E-16,
8.65624383739432)) ;
#84695 = CARTESIAN_POINT('Ctrl Pts',(-1.29904734958516,-0.750005336973063,
8.69791050406099)) ;
#84696 = CARTESIAN_POINT('Ctrl Pts',(-0.866031566390109,-1.50001067394612,
8.73957717072765)) ;
#84697 = CARTESIAN_POINT('Ctrl Pts',(-1.83698327053499E-16,-1.50001067394612,
8.78124383739432)) ;
#84698 = CARTESIAN_POINT('Ctrl Pts',(0.866031566390108,-1.50001067394612,
8.82291050406099)) ;
#84699 = CARTESIAN_POINT('Ctrl Pts',(1.29904734958516,-0.750005336973063,
8.86457717072765)) ;
#84700 = CARTESIAN_POINT('Ctrl Pts',(1.73206313278021,-3.18174835722064E-16,
8.90624383739432)) ;
#84701 = CARTESIAN_POINT('Ctrl Pts',(1.29904734958516,0.750005336973062,8.94791050406099)) ;
#84702 = CARTESIAN_POINT('Ctrl Pts',(0.866031566390109,1.50001067394612,8.98957717072765)) ;
#84703 = CARTESIAN_POINT('Ctrl Pts',(0.,1.50001067394612,9.03124383739432)) ;
#84704 = CARTESIAN_POINT('Ctrl Pts',(0.00319785405614896,1.1752361228587,
0.218553781470594)) ;
#84705 = CARTESIAN_POINT('Ctrl Pts',(-0.677458612502694,1.17708821028189,
0.260285648324568)) ;
#84706 = CARTESIAN_POINT('Ctrl Pts',(-1.01778810567666,0.587620236790419,
0.302083333333337)) ;
#84707 = CARTESIAN_POINT('Ctrl Pts',(-1.35705080756888,8.30953963884779E-17,
0.343750000000004)) ;
#84708 = CARTESIAN_POINT('Ctrl Pts',(-1.01778810567666,-0.587620236790419,
0.38541666666667)) ;
#84709 = CARTESIAN_POINT('Ctrl Pts',(-0.67852540378444,-1.17524047358084,
0.427083333333337)) ;
#84710 = CARTESIAN_POINT('Ctrl Pts',(-1.43925448419919E-16,-1.17524047358084,
0.468750000000003)) ;
#84711 = CARTESIAN_POINT('Ctrl Pts',(0.678525403784439,-1.17524047358084,
0.51041666666667)) ;
#84712 = CARTESIAN_POINT('Ctrl Pts',(1.01778810567666,-0.587620236790419,
0.552083333333337)) ;
#84713 = CARTESIAN_POINT('Ctrl Pts',(1.35705080756888,-2.49286189165434E-16,
0.593750000000003)) ;
#84714 = CARTESIAN_POINT('Ctrl Pts',(1.01778810567666,0.587620236790418,0.63541666666667)) ;
#84715 = CARTESIAN_POINT('Ctrl Pts',(0.67852540378444,1.17524047358084,0.677083333333336)) ;
#84716 = CARTESIAN_POINT('Ctrl Pts',(0.,1.17524047358084,0.718750000000003)) ;
#84717 = CARTESIAN_POINT('Ctrl Pts',(-0.67852540378444,1.17524047358084,0.76041666666667)) ;
#84718 = CARTESIAN_POINT('Ctrl Pts',(-1.01778810567666,0.587620236790419,
0.802083333333336)) ;
#84719 = CARTESIAN_POINT('Ctrl Pts',(-1.35705080756888,8.30953963884779E-17,
0.843750000000003)) ;
#84720 = CARTESIAN_POINT('Ctrl Pts',(-1.01778810567666,-0.587620236790419,
0.885416666666669)) ;
#84721 = CARTESIAN_POINT('Ctrl Pts',(-0.67852540378444,-1.17524047358084,
0.927083333333336)) ;
#84722 = CARTESIAN_POINT('Ctrl Pts',(-1.43925448419919E-16,-1.17524047358084,
0.968750000000002)) ;
#84723 = CARTESIAN_POINT('Ctrl Pts',(0.678525403784439,-1.17524047358084,
1.01041666666667)) ;
#84724 = CARTESIAN_POINT('Ctrl Pts',(1.01778810567666,-0.587620236790419,
1.05208333333334)) ;
#84725 = CARTESIAN_POINT('Ctrl Pts',(1.35705080756888,-2.49286189165434E-16,
1.09375)) ;
#84726 = CARTESIAN_POINT('Ctrl Pts',(1.01778810567666,0.587620236790418,1.13541666666667)) ;
#84727 = CARTESIAN_POINT('Ctrl Pts',(0.67852540378444,1.17524047358084,1.17708333333334)) ;
#84728 = CARTESIAN_POINT('Ctrl Pts',(0.,1.17524047358084,1.21875)) ;
#84729 = CARTESIAN_POINT('Ctrl Pts',(-0.67852540378444,1.17524047358084,1.26041666666667)) ;
#84730 = CARTESIAN_POINT('Ctrl Pts',(-1.01778810567666,0.587620236790419,
1.30208333333334)) ;
#84731 = CARTESIAN_POINT('Ctrl Pts',(-1.35705080756888,8.30953963884779E-17,
1.34375)) ;
#84732 = CARTESIAN_POINT('Ctrl Pts',(-1.01778810567666,-0.587620236790419,
1.38541666666667)) ;
#84733 = CARTESIAN_POINT('Ctrl Pts',(-0.67852540378444,-1.17524047358084,
1.42708333333334)) ;
#84734 = CARTESIAN_POINT('Ctrl Pts',(-1.43925448419919E-16,-1.17524047358084,
1.46875)) ;
#84735 = CARTESIAN_POINT('Ctrl Pts',(0.678525403784439,-1.17524047358084,
1.51041666666667)) ;
#84736 = CARTESIAN_POINT('Ctrl Pts',(1.01778810567666,-0.587620236790419,
1.55208333333333)) ;
#84737 = CARTESIAN_POINT('Ctrl Pts',(1.35705080756888,-2.49286189165434E-16,
1.59375)) ;
#84738 = CARTESIAN_POINT('Ctrl Pts',(1.01778810567666,0.587620236790418,1.63541666666667)) ;
#84739 = CARTESIAN_POINT('Ctrl Pts',(0.67852540378444,1.17524047358084,1.67708333333333)) ;
#84740 = CARTESIAN_POINT('Ctrl Pts',(0.,1.17524047358084,1.71875)) ;
#84741 = CARTESIAN_POINT('Ctrl Pts',(-0.67852540378444,1.17524047358084,1.76041666666667)) ;
#84742 = CARTESIAN_POINT('Ctrl Pts',(-1.01778810567666,0.587620236790419,
1.80208333333333)) ;
#84743 = CARTESIAN_POINT('Ctrl Pts',(-1.35705080756888,8.30953963884779E-17,
1.84375)) ;
#84744 = CARTESIAN_POINT('Ctrl Pts',(-1.01778810567666,-0.587620236790419,
1.88541666666667)) ;
#84745 = CARTESIAN_POINT('Ctrl Pts',(-0.67852540378444,-1.17524047358084,
1.92708333333333)) ;
#84746 = CARTESIAN_POINT('Ctrl Pts',(-1.43925448419919E-16,-1.17524047358084,
1.96875)) ;
#84747 = CARTESIAN_POINT('Ctrl Pts',(0.678525403784439,-1.17524047358084,
2.01041666666667)) ;
#84748 = CARTESIAN_POINT('Ctrl Pts',(1.01778810567666,-0.587620236790419,
2.05208333333333)) ;
#84749 = CARTESIAN_POINT('Ctrl Pts',(1.35705080756888,-2.49286189165434E-16,
2.09375)) ;
#84750 = CARTESIAN_POINT('Ctrl Pts',(1.01778810567666,0.587620236790418,2.13541666666667)) ;
#84751 = CARTESIAN_POINT('Ctrl Pts',(0.67852540378444,1.17524047358084,2.17708333333333)) ;
#84752 = CARTESIAN_POINT('Ctrl Pts',(0.,1.17524047358084,2.21875)) ;
#84753 = CARTESIAN_POINT('Ctrl Pts',(-0.67852540378444,1.17524047358084,2.26041666666667)) ;
#84754 = CARTESIAN_POINT('Ctrl Pts',(-1.01778810567666,0.587620236790419,
2.30208333333333)) ;
#84755 = CARTESIAN_POINT('Ctrl Pts',(-1.35705080756888,8.30953963884779E-17,
2.34375)) ;
#84756 = CARTESIAN_POINT('Ctrl Pts',(-1.01778810567666,-0.587620236790419,
2.38541666666667)) ;
#84757 = CARTESIAN_POINT('Ctrl Pts',(-0.67852540378444,-1.17524047358084,
2.42708333333333)) ;
#84758 = CARTESIAN_POINT('Ctrl Pts',(-1.43925448419919E-16,-1.17524047358084,
2.46875)) ;
#84759 = CARTESIAN_POINT('Ctrl Pts',(0.678525403784439,-1.17524047358084,
2.51041666666667)) ;
#84760 = CARTESIAN_POINT('Ctrl Pts',(1.01778810567666,-0.587620236790419,
2.55208333333333)) ;
#84761 = CARTESIAN_POINT('Ctrl Pts',(1.35705080756888,-2.49286189165434E-16,
2.59375)) ;
#84762 = CARTESIAN_POINT('Ctrl Pts',(1.01778810567666,0.587620236790418,2.63541666666667)) ;
#84763 = CARTESIAN_POINT('Ctrl Pts',(0.67852540378444,1.17524047358084,2.67708333333333)) ;
#84764 = CARTESIAN_POINT('Ctrl Pts',(0.,1.17524047358084,2.71875)) ;
#84765 = CARTESIAN_POINT('Ctrl Pts',(-0.67852540378444,1.17524047358084,2.76041666666667)) ;
#84766 = CARTESIAN_POINT('Ctrl Pts',(-1.01778810567666,0.587620236790419,
2.80208333333333)) ;
#84767 = CARTESIAN_POINT('Ctrl Pts',(-1.35705080756888,8.30953963884779E-17,
2.84375)) ;
#84768 = CARTESIAN_POINT('Ctrl Pts',(-1.01778810567666,-0.587620236790419,
2.88541666666667)) ;
#84769 = CARTESIAN_POINT('Ctrl Pts',(-0.67852540378444,-1.17524047358084,
2.92708333333333)) ;
#84770 = CARTESIAN_POINT('Ctrl Pts',(-1.43925448419919E-16,-1.17524047358084,
2.96875)) ;
#84771 = CARTESIAN_POINT('Ctrl Pts',(0.678525403784439,-1.17524047358084,
3.01041666666666)) ;
#84772 = CARTESIAN_POINT('Ctrl Pts',(1.01778810567666,-0.587620236790419,
3.05208333333333)) ;
#84773 = CARTESIAN_POINT('Ctrl Pts',(1.35705080756888,-2.49286189165434E-16,
3.09375)) ;
#84774 = CARTESIAN_POINT('Ctrl Pts',(1.01778810567666,0.587620236790418,3.13541666666666)) ;
#84775 = CARTESIAN_POINT('Ctrl Pts',(0.67852540378444,1.17524047358084,3.17708333333333)) ;
#84776 = CARTESIAN_POINT('Ctrl Pts',(0.,1.17524047358084,3.21875)) ;
#84777 = CARTESIAN_POINT('Ctrl Pts',(-0.67852540378444,1.17524047358084,3.26041666666666)) ;
#84778 = CARTESIAN_POINT('Ctrl Pts',(-1.01778810567666,0.587620236790419,
3.30208333333333)) ;
#84779 = CARTESIAN_POINT('Ctrl Pts',(-1.35705080756888,8.30953963884779E-17,
3.34375)) ;
#84780 = CARTESIAN_POINT('Ctrl Pts',(-1.01778810567666,-0.587620236790419,
3.38541666666666)) ;
#84781 = CARTESIAN_POINT('Ctrl Pts',(-0.67852540378444,-1.17524047358084,
3.42708333333333)) ;
#84782 = CARTESIAN_POINT('Ctrl Pts',(-1.43925448419919E-16,-1.17524047358084,
3.46875)) ;
#84783 = CARTESIAN_POINT('Ctrl Pts',(0.678525403784439,-1.17524047358084,
3.51041666666666)) ;
#84784 = CARTESIAN_POINT('Ctrl Pts',(1.01778810567666,-0.587620236790419,
3.55208333333333)) ;
#84785 = CARTESIAN_POINT('Ctrl Pts',(1.35705080756888,-2.49286189165434E-16,
3.59375)) ;
#84786 = CARTESIAN_POINT('Ctrl Pts',(1.01778810567666,0.587620236790418,3.63541666666666)) ;
#84787 = CARTESIAN_POINT('Ctrl Pts',(0.67852540378444,1.17524047358084,3.67708333333333)) ;
#84788 = CARTESIAN_POINT('Ctrl Pts',(0.,1.17524047358084,3.71875)) ;
#84789 = CARTESIAN_POINT('Ctrl Pts',(-0.67852540378444,1.17524047358084,3.76041666666666)) ;
#84790 = CARTESIAN_POINT('Ctrl Pts',(-1.01778810567666,0.587620236790419,
3.80208333333333)) ;
#84791 = CARTESIAN_POINT('Ctrl Pts',(-1.35705080756888,8.30953963884779E-17,
3.84375)) ;
#84792 = CARTESIAN_POINT('Ctrl Pts',(-1.01778810567666,-0.587620236790419,
3.88541666666666)) ;
#84793 = CARTESIAN_POINT('Ctrl Pts',(-0.67852540378444,-1.17524047358084,
3.92708333333333)) ;
#84794 = CARTESIAN_POINT('Ctrl Pts',(-1.43925448419919E-16,-1.17524047358084,
3.96875)) ;
#84795 = CARTESIAN_POINT('Ctrl Pts',(0.678525403784439,-1.17524047358084,
4.01041666666666)) ;
#84796 = CARTESIAN_POINT('Ctrl Pts',(1.01778810567666,-0.587620236790419,
4.05208333333333)) ;
#84797 = CARTESIAN_POINT('Ctrl Pts',(1.35705080756888,-2.49286189165434E-16,
4.09375)) ;
#84798 = CARTESIAN_POINT('Ctrl Pts',(1.01778810567666,0.587620236790418,4.13541666666666)) ;
#84799 = CARTESIAN_POINT('Ctrl Pts',(0.67852540378444,1.17524047358084,4.17708333333333)) ;
#84800 = CARTESIAN_POINT('Ctrl Pts',(0.,1.17524047358084,4.21874999999999)) ;
#84801 = CARTESIAN_POINT('Ctrl Pts',(-0.67852540378444,1.17524047358084,4.26041666666666)) ;
#84802 = CARTESIAN_POINT('Ctrl Pts',(-1.01778810567666,0.587620236790419,
4.30208333333333)) ;
#84803 = CARTESIAN_POINT('Ctrl Pts',(-1.35705080756888,8.30953963884779E-17,
4.34374999999999)) ;
#84804 = CARTESIAN_POINT('Ctrl Pts',(-1.01778810567666,-0.587620236790419,
4.38541666666666)) ;
#84805 = CARTESIAN_POINT('Ctrl Pts',(-0.67852540378444,-1.17524047358084,
4.42708333333333)) ;
#84806 = CARTESIAN_POINT('Ctrl Pts',(-1.43925448419919E-16,-1.17524047358084,
4.46874999999999)) ;
#84807 = CARTESIAN_POINT('Ctrl Pts',(0.678525403784439,-1.17524047358084,
4.51041666666666)) ;
#84808 = CARTESIAN_POINT('Ctrl Pts',(1.01778810567666,-0.587620236790419,
4.55208333333333)) ;
#84809 = CARTESIAN_POINT('Ctrl Pts',(1.35705080756888,-2.49286189165434E-16,
4.59374999999999)) ;
#84810 = CARTESIAN_POINT('Ctrl Pts',(1.01778810567666,0.587620236790418,4.63541666666666)) ;
#84811 = CARTESIAN_POINT('Ctrl Pts',(0.67852540378444,1.17524047358084,4.67708333333333)) ;
#84812 = CARTESIAN_POINT('Ctrl Pts',(0.,1.17524047358084,4.71874999999999)) ;
#84813 = CARTESIAN_POINT('Ctrl Pts',(-0.67852540378444,1.17524047358084,4.76041666666666)) ;
#84814 = CARTESIAN_POINT('Ctrl Pts',(-1.01778810567666,0.587620236790419,
4.80208333333333)) ;
#84815 = CARTESIAN_POINT('Ctrl Pts',(-1.35705080756888,8.30953963884779E-17,
4.84374999999999)) ;
#84816 = CARTESIAN_POINT('Ctrl Pts',(-1.01778810567666,-0.587620236790419,
4.88541666666666)) ;
#84817 = CARTESIAN_POINT('Ctrl Pts',(-0.67852540378444,-1.17524047358084,
4.92708333333333)) ;
#84818 = CARTESIAN_POINT('Ctrl Pts',(-1.43925448419919E-16,-1.17524047358084,
4.96874999999999)) ;
#84819 = CARTESIAN_POINT('Ctrl Pts',(0.678525403784439,-1.17524047358084,
5.01041666666666)) ;
#84820 = CARTESIAN_POINT('Ctrl Pts',(1.01778810567666,-0.587620236790419,
5.05208333333333)) ;
#84821 = CARTESIAN_POINT('Ctrl Pts',(1.35705080756888,-2.49286189165434E-16,
5.09374999999999)) ;
#84822 = CARTESIAN_POINT('Ctrl Pts',(1.01778810567666,0.587620236790418,5.13541666666666)) ;
#84823 = CARTESIAN_POINT('Ctrl Pts',(0.67852540378444,1.17524047358084,5.17708333333333)) ;
#84824 = CARTESIAN_POINT('Ctrl Pts',(0.,1.17524047358084,5.21874999999999)) ;
#84825 = CARTESIAN_POINT('Ctrl Pts',(-0.67852540378444,1.17524047358084,5.26041666666666)) ;
#84826 = CARTESIAN_POINT('Ctrl Pts',(-1.01778810567666,0.587620236790419,
5.30208333333333)) ;
#84827 = CARTESIAN_POINT('Ctrl Pts',(-1.35705080756888,8.30953963884779E-17,
5.34374999999999)) ;
#84828 = CARTESIAN_POINT('Ctrl Pts',(-1.01778810567666,-0.587620236790419,
5.38541666666666)) ;
#84829 = CARTESIAN_POINT('Ctrl Pts',(-0.67852540378444,-1.17524047358084,
5.42708333333333)) ;
#84830 = CARTESIAN_POINT('Ctrl Pts',(-1.43925448419919E-16,-1.17524047358084,
5.46874999999999)) ;
#84831 = CARTESIAN_POINT('Ctrl Pts',(0.678525403784439,-1.17524047358084,
5.51041666666666)) ;
#84832 = CARTESIAN_POINT('Ctrl Pts',(1.01778810567666,-0.587620236790419,
5.55208333333333)) ;
#84833 = CARTESIAN_POINT('Ctrl Pts',(1.35705080756888,-2.49286189165434E-16,
5.59374999999999)) ;
#84834 = CARTESIAN_POINT('Ctrl Pts',(1.01778810567666,0.587620236790418,5.63541666666666)) ;
#84835 = CARTESIAN_POINT('Ctrl Pts',(0.67852540378444,1.17524047358084,5.67708333333333)) ;
#84836 = CARTESIAN_POINT('Ctrl Pts',(0.,1.17524047358084,5.71874999999999)) ;
#84837 = CARTESIAN_POINT('Ctrl Pts',(-0.67852540378444,1.17524047358084,5.76041666666666)) ;
#84838 = CARTESIAN_POINT('Ctrl Pts',(-1.01778810567666,0.587620236790419,
5.80208333333333)) ;
#84839 = CARTESIAN_POINT('Ctrl Pts',(-1.35705080756888,8.30953963884779E-17,
5.84374999999999)) ;
#84840 = CARTESIAN_POINT('Ctrl Pts',(-1.01778810567666,-0.587620236790419,
5.88541666666666)) ;
#84841 = CARTESIAN_POINT('Ctrl Pts',(-0.67852540378444,-1.17524047358084,
5.92708333333333)) ;
#84842 = CARTESIAN_POINT('Ctrl Pts',(-1.43925448419919E-16,-1.17524047358084,
5.96874999999999)) ;
#84843 = CARTESIAN_POINT('Ctrl Pts',(0.678525403784439,-1.17524047358084,
6.01041666666666)) ;
#84844 = CARTESIAN_POINT('Ctrl Pts',(1.01778810567666,-0.587620236790419,
6.05208333333333)) ;
#84845 = CARTESIAN_POINT('Ctrl Pts',(1.35705080756888,-2.49286189165434E-16,
6.09374999999999)) ;
#84846 = CARTESIAN_POINT('Ctrl Pts',(1.01778810567666,0.587620236790418,6.13541666666666)) ;
#84847 = CARTESIAN_POINT('Ctrl Pts',(0.67852540378444,1.17524047358084,6.17708333333332)) ;
#84848 = CARTESIAN_POINT('Ctrl Pts',(0.,1.17524047358084,6.21874999999999)) ;
#84849 = CARTESIAN_POINT('Ctrl Pts',(-0.67852540378444,1.17524047358084,6.26041666666666)) ;
#84850 = CARTESIAN_POINT('Ctrl Pts',(-1.01778810567666,0.587620236790419,
6.30208333333332)) ;
#84851 = CARTESIAN_POINT('Ctrl Pts',(-1.35705080756888,8.30953963884779E-17,
6.34374999999999)) ;
#84852 = CARTESIAN_POINT('Ctrl Pts',(-1.01778810567666,-0.587620236790419,
6.38541666666666)) ;
#84853 = CARTESIAN_POINT('Ctrl Pts',(-0.67852540378444,-1.17524047358084,
6.42708333333332)) ;
#84854 = CARTESIAN_POINT('Ctrl Pts',(-1.43925448419919E-16,-1.17524047358084,
6.46874999999999)) ;
#84855 = CARTESIAN_POINT('Ctrl Pts',(0.678525403784439,-1.17524047358084,
6.51041666666666)) ;
#84856 = CARTESIAN_POINT('Ctrl Pts',(1.01778810567666,-0.587620236790419,
6.55208333333332)) ;
#84857 = CARTESIAN_POINT('Ctrl Pts',(1.35705080756888,-2.49286189165434E-16,
6.59374999999999)) ;
#84858 = CARTESIAN_POINT('Ctrl Pts',(1.01778810567666,0.587620236790418,6.63541666666666)) ;
#84859 = CARTESIAN_POINT('Ctrl Pts',(0.67852540378444,1.17524047358084,6.67708333333332)) ;
#84860 = CARTESIAN_POINT('Ctrl Pts',(0.,1.17524047358084,6.71874999999999)) ;
#84861 = CARTESIAN_POINT('Ctrl Pts',(-0.67852540378444,1.17524047358084,6.76041666666666)) ;
#84862 = CARTESIAN_POINT('Ctrl Pts',(-1.01778810567666,0.587620236790419,
6.80208333333332)) ;
#84863 = CARTESIAN_POINT('Ctrl Pts',(-1.35705080756888,8.30953963884779E-17,
6.84374999999999)) ;
#84864 = CARTESIAN_POINT('Ctrl Pts',(-1.01778810567666,-0.587620236790419,
6.88541666666666)) ;
#84865 = CARTESIAN_POINT('Ctrl Pts',(-0.67852540378444,-1.17524047358084,
6.92708333333332)) ;
#84866 = CARTESIAN_POINT('Ctrl Pts',(-1.43925448419919E-16,-1.17524047358084,
6.96874999999999)) ;
#84867 = CARTESIAN_POINT('Ctrl Pts',(0.678525403784439,-1.17524047358084,
7.01041666666666)) ;
#84868 = CARTESIAN_POINT('Ctrl Pts',(1.01778810567666,-0.587620236790419,
7.05208333333332)) ;
#84869 = CARTESIAN_POINT('Ctrl Pts',(1.35705080756888,-2.49286189165434E-16,
7.09374999999999)) ;
#84870 = CARTESIAN_POINT('Ctrl Pts',(1.01778810567666,0.587620236790418,7.13541666666666)) ;
#84871 = CARTESIAN_POINT('Ctrl Pts',(0.67852540378444,1.17524047358084,7.17708333333332)) ;
#84872 = CARTESIAN_POINT('Ctrl Pts',(0.,1.17524047358084,7.21874999999999)) ;
#84873 = CARTESIAN_POINT('Ctrl Pts',(-0.67852540378444,1.17524047358084,7.26041666666666)) ;
#84874 = CARTESIAN_POINT('Ctrl Pts',(-1.01778810567666,0.587620236790419,
7.30208333333332)) ;
#84875 = CARTESIAN_POINT('Ctrl Pts',(-1.35705080756888,8.30953963884779E-17,
7.34374999999999)) ;
#84876 = CARTESIAN_POINT('Ctrl Pts',(-1.01778810567666,-0.587620236790419,
7.38541666666666)) ;
#84877 = CARTESIAN_POINT('Ctrl Pts',(-0.67852540378444,-1.17524047358084,
7.42708333333332)) ;
#84878 = CARTESIAN_POINT('Ctrl Pts',(-1.43925448419919E-16,-1.17524047358084,
7.46874999999999)) ;
#84879 = CARTESIAN_POINT('Ctrl Pts',(0.678525403784439,-1.17524047358084,
7.51041666666666)) ;
#84880 = CARTESIAN_POINT('Ctrl Pts',(1.01778810567666,-0.587620236790419,
7.55208333333332)) ;
#84881 = CARTESIAN_POINT('Ctrl Pts',(1.35705080756888,-2.49286189165434E-16,
7.59374999999999)) ;
#84882 = CARTESIAN_POINT('Ctrl Pts',(1.01778810567666,0.587620236790418,7.63541666666665)) ;
#84883 = CARTESIAN_POINT('Ctrl Pts',(0.67852540378444,1.17524047358084,7.67708333333332)) ;
#84884 = CARTESIAN_POINT('Ctrl Pts',(0.,1.17524047358084,7.71874999999999)) ;
#84885 = CARTESIAN_POINT('Ctrl Pts',(-0.67852540378444,1.17524047358084,7.76041666666666)) ;
#84886 = CARTESIAN_POINT('Ctrl Pts',(-1.01778810567666,0.587620236790419,
7.80208333333332)) ;
#84887 = CARTESIAN_POINT('Ctrl Pts',(-1.35705080756888,8.30953963884779E-17,
7.84374999999999)) ;
#84888 = CARTESIAN_POINT('Ctrl Pts',(-1.01778810567666,-0.587620236790419,
7.88541666666665)) ;
#84889 = CARTESIAN_POINT('Ctrl Pts',(-0.67852540378444,-1.17524047358084,
7.92708333333332)) ;
#84890 = CARTESIAN_POINT('Ctrl Pts',(-1.43925448419919E-16,-1.17524047358084,
7.96874999999999)) ;
#84891 = CARTESIAN_POINT('Ctrl Pts',(0.678525403784439,-1.17524047358084,
8.01041666666665)) ;
#84892 = CARTESIAN_POINT('Ctrl Pts',(1.01778810567666,-0.587620236790419,
8.05208333333332)) ;
#84893 = CARTESIAN_POINT('Ctrl Pts',(1.35705080756888,-2.49286189165434E-16,
8.09374999999999)) ;
#84894 = CARTESIAN_POINT('Ctrl Pts',(1.01778810567666,0.587620236790418,8.13541666666665)) ;
#84895 = CARTESIAN_POINT('Ctrl Pts',(0.67852540378444,1.17524047358084,8.17708333333332)) ;
#84896 = CARTESIAN_POINT('Ctrl Pts',(0.,1.17524047358084,8.21874999999999)) ;
#84897 = CARTESIAN_POINT('Ctrl Pts',(-0.67852540378444,1.17524047358084,8.26041666666665)) ;
#84898 = CARTESIAN_POINT('Ctrl Pts',(-1.01778810567666,0.587620236790419,
8.30208333333332)) ;
#84899 = CARTESIAN_POINT('Ctrl Pts',(-1.35705080756888,8.30953963884779E-17,
8.34374999999999)) ;
#84900 = CARTESIAN_POINT('Ctrl Pts',(-1.01778810567666,-0.587620236790419,
8.38541666666665)) ;
#84901 = CARTESIAN_POINT('Ctrl Pts',(-0.67852540378444,-1.17524047358084,
8.42708333333332)) ;
#84902 = CARTESIAN_POINT('Ctrl Pts',(-1.43925448419919E-16,-1.17524047358084,
8.46874999999999)) ;
#84903 = CARTESIAN_POINT('Ctrl Pts',(0.678525403784439,-1.17524047358084,
8.51041666666665)) ;
#84904 = CARTESIAN_POINT('Ctrl Pts',(1.01778810567666,-0.587620236790419,
8.55208333333332)) ;
#84905 = CARTESIAN_POINT('Ctrl Pts',(1.35705080756888,-2.49286189165434E-16,
8.59374999999999)) ;
#84906 = CARTESIAN_POINT('Ctrl Pts',(1.01778810567666,0.587620236790418,8.63541666666665)) ;
#84907 = CARTESIAN_POINT('Ctrl Pts',(0.67852540378444,1.17524047358084,8.67708333333332)) ;
#84908 = CARTESIAN_POINT('Ctrl Pts',(0.,1.17524047358084,8.71874999999999)) ;
#84909 = CARTESIAN_POINT('Ctrl Pts',(-0.67852540378444,1.17524047358084,8.76041666666665)) ;
#84910 = CARTESIAN_POINT('Ctrl Pts',(-1.01778810567666,0.587620236790419,
8.80208333333332)) ;
#84911 = CARTESIAN_POINT('Ctrl Pts',(-1.35705080756888,8.30953963884779E-17,
8.84374999999998)) ;
#84912 = CARTESIAN_POINT('Ctrl Pts',(-1.01778810567666,-0.587620236790419,
8.88541666666665)) ;
#84913 = CARTESIAN_POINT('Ctrl Pts',(-0.67852540378444,-1.17524047358084,
8.92708333333332)) ;
#84914 = CARTESIAN_POINT('Ctrl Pts',(-1.43925448419919E-16,-1.17524047358084,
8.96874999999999)) ;
#84915 = CARTESIAN_POINT('Ctrl Pts',(0.678525403784439,-1.17524047358084,
9.01041666666665)) ;
#84916 = CARTESIAN_POINT('Ctrl Pts',(1.01778810567666,-0.587620236790419,
9.05208333333332)) ;
#84917 = CARTESIAN_POINT('Ctrl Pts',(1.35705080756888,-2.49286189165434E-16,
9.09374999999999)) ;
#84918 = CARTESIAN_POINT('Ctrl Pts',(1.01778810567666,0.587620236790418,9.13541666666665)) ;
#84919 = CARTESIAN_POINT('Ctrl Pts',(0.67852540378444,1.17524047358084,9.17708333333332)) ;
#84920 = CARTESIAN_POINT('Ctrl Pts',(0.,1.17524047358084,9.21874999999998)) ;
#84921 = CARTESIAN_POINT('',(0.,1.5,0.03125)) ;
#84922 = CARTESIAN_POINT('Ctrl Pts',(0.,1.17524047358084,-0.218749999999996)) ;
#84923 = CARTESIAN_POINT('Ctrl Pts',(-0.67852540378444,1.17524047358084,-0.17708333333333)) ;
#84924 = CARTESIAN_POINT('Ctrl Pts',(-1.01778810567666,0.587620236790419,
-0.135416666666663)) ;
#84925 = CARTESIAN_POINT('Ctrl Pts',(-1.35705080756888,8.30953963884779E-17,
-0.0937499999999966)) ;
#84926 = CARTESIAN_POINT('Ctrl Pts',(-1.01778810567666,-0.587620236790419,
-0.05208333333333)) ;
#84927 = CARTESIAN_POINT('Ctrl Pts',(-0.67852540378444,-1.17524047358084,
-0.0104166666666634)) ;
#84928 = CARTESIAN_POINT('Ctrl Pts',(-1.43925448419919E-16,-1.17524047358084,
0.0312500000000032)) ;
#84929 = CARTESIAN_POINT('Ctrl Pts',(0.678525403784439,-1.17524047358084,
0.0729166666666698)) ;
#84930 = CARTESIAN_POINT('Ctrl Pts',(1.01778810567666,-0.587620236790419,
0.114583333333336)) ;
#84931 = CARTESIAN_POINT('Ctrl Pts',(1.35705080756888,-2.49286189165434E-16,
0.156250000000003)) ;
#84932 = CARTESIAN_POINT('Ctrl Pts',(1.01778810567666,0.587620236790418,0.19791666666667)) ;
#84933 = CARTESIAN_POINT('Ctrl Pts',(0.67852540378444,1.17524047358084,0.239583333333336)) ;
#84934 = CARTESIAN_POINT('Ctrl Pts',(0.,1.17524047358084,0.281250000000003)) ;
#84935 = CARTESIAN_POINT('Ctrl Pts',(-0.67852540378444,1.17524047358084,0.322916666666669)) ;
#84936 = CARTESIAN_POINT('Ctrl Pts',(-1.01778810567666,0.587620236790419,
0.364583333333336)) ;
#84937 = CARTESIAN_POINT('Ctrl Pts',(-1.35705080756888,8.30953963884779E-17,
0.406250000000002)) ;
#84938 = CARTESIAN_POINT('Ctrl Pts',(-1.01778810567666,-0.587620236790419,
0.447916666666669)) ;
#84939 = CARTESIAN_POINT('Ctrl Pts',(-0.67852540378444,-1.17524047358084,
0.489583333333336)) ;
#84940 = CARTESIAN_POINT('Ctrl Pts',(-1.43925448419919E-16,-1.17524047358084,
0.531250000000002)) ;
#84941 = CARTESIAN_POINT('Ctrl Pts',(0.678525403784439,-1.17524047358084,
0.572916666666669)) ;
#84942 = CARTESIAN_POINT('Ctrl Pts',(1.01778810567666,-0.587620236790419,
0.614583333333335)) ;
#84943 = CARTESIAN_POINT('Ctrl Pts',(1.35705080756888,-2.49286189165434E-16,
0.656250000000002)) ;
#84944 = CARTESIAN_POINT('Ctrl Pts',(1.01778810567666,0.587620236790418,0.697916666666669)) ;
#84945 = CARTESIAN_POINT('Ctrl Pts',(0.67852540378444,1.17524047358084,0.739583333333335)) ;
#84946 = CARTESIAN_POINT('Ctrl Pts',(0.,1.17524047358084,0.781250000000002)) ;
#84947 = CARTESIAN_POINT('Ctrl Pts',(-0.67852540378444,1.17524047358084,0.822916666666668)) ;
#84948 = CARTESIAN_POINT('Ctrl Pts',(-1.01778810567666,0.587620236790419,
0.864583333333335)) ;
#84949 = CARTESIAN_POINT('Ctrl Pts',(-1.35705080756888,8.30953963884779E-17,
0.906250000000001)) ;
#84950 = CARTESIAN_POINT('Ctrl Pts',(-1.01778810567666,-0.587620236790419,
0.947916666666668)) ;
#84951 = CARTESIAN_POINT('Ctrl Pts',(-0.67852540378444,-1.17524047358084,
0.989583333333335)) ;
#84952 = CARTESIAN_POINT('Ctrl Pts',(-1.43925448419919E-16,-1.17524047358084,
1.03125)) ;
#84953 = CARTESIAN_POINT('Ctrl Pts',(0.678525403784439,-1.17524047358084,
1.07291666666667)) ;
#84954 = CARTESIAN_POINT('Ctrl Pts',(1.01778810567666,-0.587620236790419,
1.11458333333333)) ;
#84955 = CARTESIAN_POINT('Ctrl Pts',(1.35705080756888,-2.49286189165434E-16,
1.15625)) ;
#84956 = CARTESIAN_POINT('Ctrl Pts',(1.01778810567666,0.587620236790418,1.19791666666667)) ;
#84957 = CARTESIAN_POINT('Ctrl Pts',(0.67852540378444,1.17524047358084,1.23958333333333)) ;
#84958 = CARTESIAN_POINT('Ctrl Pts',(0.,1.17524047358084,1.28125)) ;
#84959 = CARTESIAN_POINT('Ctrl Pts',(-0.67852540378444,1.17524047358084,1.32291666666667)) ;
#84960 = CARTESIAN_POINT('Ctrl Pts',(-1.01778810567666,0.587620236790419,
1.36458333333333)) ;
#84961 = CARTESIAN_POINT('Ctrl Pts',(-1.35705080756888,8.30953963884779E-17,
1.40625)) ;
#84962 = CARTESIAN_POINT('Ctrl Pts',(-1.01778810567666,-0.587620236790419,
1.44791666666667)) ;
#84963 = CARTESIAN_POINT('Ctrl Pts',(-0.67852540378444,-1.17524047358084,
1.48958333333333)) ;
#84964 = CARTESIAN_POINT('Ctrl Pts',(-1.43925448419919E-16,-1.17524047358084,
1.53125)) ;
#84965 = CARTESIAN_POINT('Ctrl Pts',(0.678525403784439,-1.17524047358084,
1.57291666666667)) ;
#84966 = CARTESIAN_POINT('Ctrl Pts',(1.01778810567666,-0.587620236790419,
1.61458333333333)) ;
#84967 = CARTESIAN_POINT('Ctrl Pts',(1.35705080756888,-2.49286189165434E-16,
1.65625)) ;
#84968 = CARTESIAN_POINT('Ctrl Pts',(1.01778810567666,0.587620236790418,1.69791666666667)) ;
#84969 = CARTESIAN_POINT('Ctrl Pts',(0.67852540378444,1.17524047358084,1.73958333333333)) ;
#84970 = CARTESIAN_POINT('Ctrl Pts',(0.,1.17524047358084,1.78125)) ;
#84971 = CARTESIAN_POINT('Ctrl Pts',(-0.67852540378444,1.17524047358084,1.82291666666667)) ;
#84972 = CARTESIAN_POINT('Ctrl Pts',(-1.01778810567666,0.587620236790419,
1.86458333333333)) ;
#84973 = CARTESIAN_POINT('Ctrl Pts',(-1.35705080756888,8.30953963884779E-17,
1.90625)) ;
#84974 = CARTESIAN_POINT('Ctrl Pts',(-1.01778810567666,-0.587620236790419,
1.94791666666667)) ;
#84975 = CARTESIAN_POINT('Ctrl Pts',(-0.67852540378444,-1.17524047358084,
1.98958333333333)) ;
#84976 = CARTESIAN_POINT('Ctrl Pts',(-1.43925448419919E-16,-1.17524047358084,
2.03125)) ;
#84977 = CARTESIAN_POINT('Ctrl Pts',(0.678525403784439,-1.17524047358084,
2.07291666666667)) ;
#84978 = CARTESIAN_POINT('Ctrl Pts',(1.01778810567666,-0.587620236790419,
2.11458333333333)) ;
#84979 = CARTESIAN_POINT('Ctrl Pts',(1.35705080756888,-2.49286189165434E-16,
2.15625)) ;
#84980 = CARTESIAN_POINT('Ctrl Pts',(1.01778810567666,0.587620236790418,2.19791666666667)) ;
#84981 = CARTESIAN_POINT('Ctrl Pts',(0.67852540378444,1.17524047358084,2.23958333333333)) ;
#84982 = CARTESIAN_POINT('Ctrl Pts',(0.,1.17524047358084,2.28125)) ;
#84983 = CARTESIAN_POINT('Ctrl Pts',(-0.67852540378444,1.17524047358084,2.32291666666667)) ;
#84984 = CARTESIAN_POINT('Ctrl Pts',(-1.01778810567666,0.587620236790419,
2.36458333333333)) ;
#84985 = CARTESIAN_POINT('Ctrl Pts',(-1.35705080756888,8.30953963884779E-17,
2.40625)) ;
#84986 = CARTESIAN_POINT('Ctrl Pts',(-1.01778810567666,-0.587620236790419,
2.44791666666666)) ;
#84987 = CARTESIAN_POINT('Ctrl Pts',(-0.67852540378444,-1.17524047358084,
2.48958333333333)) ;
#84988 = CARTESIAN_POINT('Ctrl Pts',(-1.43925448419919E-16,-1.17524047358084,
2.53125)) ;
#84989 = CARTESIAN_POINT('Ctrl Pts',(0.678525403784439,-1.17524047358084,
2.57291666666666)) ;
#84990 = CARTESIAN_POINT('Ctrl Pts',(1.01778810567666,-0.587620236790419,
2.61458333333333)) ;
#84991 = CARTESIAN_POINT('Ctrl Pts',(1.35705080756888,-2.49286189165434E-16,
2.65625)) ;
#84992 = CARTESIAN_POINT('Ctrl Pts',(1.01778810567666,0.587620236790418,2.69791666666666)) ;
#84993 = CARTESIAN_POINT('Ctrl Pts',(0.67852540378444,1.17524047358084,2.73958333333333)) ;
#84994 = CARTESIAN_POINT('Ctrl Pts',(0.,1.17524047358084,2.78125)) ;
#84995 = CARTESIAN_POINT('Ctrl Pts',(-0.67852540378444,1.17524047358084,2.82291666666666)) ;
#84996 = CARTESIAN_POINT('Ctrl Pts',(-1.01778810567666,0.587620236790419,
2.86458333333333)) ;
#84997 = CARTESIAN_POINT('Ctrl Pts',(-1.35705080756888,8.30953963884779E-17,
2.90625)) ;
#84998 = CARTESIAN_POINT('Ctrl Pts',(-1.01778810567666,-0.587620236790419,
2.94791666666666)) ;
#84999 = CARTESIAN_POINT('Ctrl Pts',(-0.67852540378444,-1.17524047358084,
2.98958333333333)) ;
#85000 = CARTESIAN_POINT('Ctrl Pts',(-1.43925448419919E-16,-1.17524047358084,
3.03125)) ;
#85001 = CARTESIAN_POINT('Ctrl Pts',(0.678525403784439,-1.17524047358084,
3.07291666666666)) ;
#85002 = CARTESIAN_POINT('Ctrl Pts',(1.01778810567666,-0.587620236790419,
3.11458333333333)) ;
#85003 = CARTESIAN_POINT('Ctrl Pts',(1.35705080756888,-2.49286189165434E-16,
3.15625)) ;
#85004 = CARTESIAN_POINT('Ctrl Pts',(1.01778810567666,0.587620236790418,3.19791666666666)) ;
#85005 = CARTESIAN_POINT('Ctrl Pts',(0.67852540378444,1.17524047358084,3.23958333333333)) ;
#85006 = CARTESIAN_POINT('Ctrl Pts',(0.,1.17524047358084,3.28125)) ;
#85007 = CARTESIAN_POINT('Ctrl Pts',(-0.67852540378444,1.17524047358084,3.32291666666666)) ;
#85008 = CARTESIAN_POINT('Ctrl Pts',(-1.01778810567666,0.587620236790419,
3.36458333333333)) ;
#85009 = CARTESIAN_POINT('Ctrl Pts',(-1.35705080756888,8.30953963884779E-17,
3.40625)) ;
#85010 = CARTESIAN_POINT('Ctrl Pts',(-1.01778810567666,-0.587620236790419,
3.44791666666666)) ;
#85011 = CARTESIAN_POINT('Ctrl Pts',(-0.67852540378444,-1.17524047358084,
3.48958333333333)) ;
#85012 = CARTESIAN_POINT('Ctrl Pts',(-1.43925448419919E-16,-1.17524047358084,
3.53125)) ;
#85013 = CARTESIAN_POINT('Ctrl Pts',(0.678525403784439,-1.17524047358084,
3.57291666666666)) ;
#85014 = CARTESIAN_POINT('Ctrl Pts',(1.01778810567666,-0.587620236790419,
3.61458333333333)) ;
#85015 = CARTESIAN_POINT('Ctrl Pts',(1.35705080756888,-2.49286189165434E-16,
3.65625)) ;
#85016 = CARTESIAN_POINT('Ctrl Pts',(1.01778810567666,0.587620236790418,3.69791666666666)) ;
#85017 = CARTESIAN_POINT('Ctrl Pts',(0.67852540378444,1.17524047358084,3.73958333333333)) ;
#85018 = CARTESIAN_POINT('Ctrl Pts',(0.,1.17524047358084,3.78125)) ;
#85019 = CARTESIAN_POINT('Ctrl Pts',(-0.67852540378444,1.17524047358084,3.82291666666666)) ;
#85020 = CARTESIAN_POINT('Ctrl Pts',(-1.01778810567666,0.587620236790419,
3.86458333333333)) ;
#85021 = CARTESIAN_POINT('Ctrl Pts',(-1.35705080756888,8.30953963884779E-17,
3.90625)) ;
#85022 = CARTESIAN_POINT('Ctrl Pts',(-1.01778810567666,-0.587620236790419,
3.94791666666666)) ;
#85023 = CARTESIAN_POINT('Ctrl Pts',(-0.67852540378444,-1.17524047358084,
3.98958333333333)) ;
#85024 = CARTESIAN_POINT('Ctrl Pts',(-1.43925448419919E-16,-1.17524047358084,
4.03124999999999)) ;
#85025 = CARTESIAN_POINT('Ctrl Pts',(0.678525403784439,-1.17524047358084,
4.07291666666666)) ;
#85026 = CARTESIAN_POINT('Ctrl Pts',(1.01778810567666,-0.587620236790419,
4.11458333333333)) ;
#85027 = CARTESIAN_POINT('Ctrl Pts',(1.35705080756888,-2.49286189165434E-16,
4.15624999999999)) ;
#85028 = CARTESIAN_POINT('Ctrl Pts',(1.01778810567666,0.587620236790418,4.19791666666666)) ;
#85029 = CARTESIAN_POINT('Ctrl Pts',(0.67852540378444,1.17524047358084,4.23958333333333)) ;
#85030 = CARTESIAN_POINT('Ctrl Pts',(0.,1.17524047358084,4.28124999999999)) ;
#85031 = CARTESIAN_POINT('Ctrl Pts',(-0.67852540378444,1.17524047358084,4.32291666666666)) ;
#85032 = CARTESIAN_POINT('Ctrl Pts',(-1.01778810567666,0.587620236790419,
4.36458333333333)) ;
#85033 = CARTESIAN_POINT('Ctrl Pts',(-1.35705080756888,8.30953963884779E-17,
4.40624999999999)) ;
#85034 = CARTESIAN_POINT('Ctrl Pts',(-1.01778810567666,-0.587620236790419,
4.44791666666666)) ;
#85035 = CARTESIAN_POINT('Ctrl Pts',(-0.67852540378444,-1.17524047358084,
4.48958333333333)) ;
#85036 = CARTESIAN_POINT('Ctrl Pts',(-1.43925448419919E-16,-1.17524047358084,
4.53124999999999)) ;
#85037 = CARTESIAN_POINT('Ctrl Pts',(0.678525403784439,-1.17524047358084,
4.57291666666666)) ;
#85038 = CARTESIAN_POINT('Ctrl Pts',(1.01778810567666,-0.587620236790419,
4.61458333333333)) ;
#85039 = CARTESIAN_POINT('Ctrl Pts',(1.35705080756888,-2.49286189165434E-16,
4.65624999999999)) ;
#85040 = CARTESIAN_POINT('Ctrl Pts',(1.01778810567666,0.587620236790418,4.69791666666666)) ;
#85041 = CARTESIAN_POINT('Ctrl Pts',(0.67852540378444,1.17524047358084,4.73958333333333)) ;
#85042 = CARTESIAN_POINT('Ctrl Pts',(0.,1.17524047358084,4.78124999999999)) ;
#85043 = CARTESIAN_POINT('Ctrl Pts',(-0.67852540378444,1.17524047358084,4.82291666666666)) ;
#85044 = CARTESIAN_POINT('Ctrl Pts',(-1.01778810567666,0.587620236790419,
4.86458333333333)) ;
#85045 = CARTESIAN_POINT('Ctrl Pts',(-1.35705080756888,8.30953963884779E-17,
4.90624999999999)) ;
#85046 = CARTESIAN_POINT('Ctrl Pts',(-1.01778810567666,-0.587620236790419,
4.94791666666666)) ;
#85047 = CARTESIAN_POINT('Ctrl Pts',(-0.67852540378444,-1.17524047358084,
4.98958333333333)) ;
#85048 = CARTESIAN_POINT('Ctrl Pts',(-1.43925448419919E-16,-1.17524047358084,
5.03124999999999)) ;
#85049 = CARTESIAN_POINT('Ctrl Pts',(0.678525403784439,-1.17524047358084,
5.07291666666666)) ;
#85050 = CARTESIAN_POINT('Ctrl Pts',(1.01778810567666,-0.587620236790419,
5.11458333333333)) ;
#85051 = CARTESIAN_POINT('Ctrl Pts',(1.35705080756888,-2.49286189165434E-16,
5.15624999999999)) ;
#85052 = CARTESIAN_POINT('Ctrl Pts',(1.01778810567666,0.587620236790418,5.19791666666666)) ;
#85053 = CARTESIAN_POINT('Ctrl Pts',(0.67852540378444,1.17524047358084,5.23958333333332)) ;
#85054 = CARTESIAN_POINT('Ctrl Pts',(0.,1.17524047358084,5.28124999999999)) ;
#85055 = CARTESIAN_POINT('Ctrl Pts',(-0.67852540378444,1.17524047358084,5.32291666666666)) ;
#85056 = CARTESIAN_POINT('Ctrl Pts',(-1.01778810567666,0.587620236790419,
5.36458333333333)) ;
#85057 = CARTESIAN_POINT('Ctrl Pts',(-1.35705080756888,8.30953963884779E-17,
5.40624999999999)) ;
#85058 = CARTESIAN_POINT('Ctrl Pts',(-1.01778810567666,-0.587620236790419,
5.44791666666666)) ;
#85059 = CARTESIAN_POINT('Ctrl Pts',(-0.67852540378444,-1.17524047358084,
5.48958333333333)) ;
#85060 = CARTESIAN_POINT('Ctrl Pts',(-1.43925448419919E-16,-1.17524047358084,
5.53124999999999)) ;
#85061 = CARTESIAN_POINT('Ctrl Pts',(0.678525403784439,-1.17524047358084,
5.57291666666666)) ;
#85062 = CARTESIAN_POINT('Ctrl Pts',(1.01778810567666,-0.587620236790419,
5.61458333333332)) ;
#85063 = CARTESIAN_POINT('Ctrl Pts',(1.35705080756888,-2.49286189165434E-16,
5.65624999999999)) ;
#85064 = CARTESIAN_POINT('Ctrl Pts',(1.01778810567666,0.587620236790418,5.69791666666666)) ;
#85065 = CARTESIAN_POINT('Ctrl Pts',(0.67852540378444,1.17524047358084,5.73958333333333)) ;
#85066 = CARTESIAN_POINT('Ctrl Pts',(0.,1.17524047358084,5.78124999999999)) ;
#85067 = CARTESIAN_POINT('Ctrl Pts',(-0.67852540378444,1.17524047358084,5.82291666666666)) ;
#85068 = CARTESIAN_POINT('Ctrl Pts',(-1.01778810567666,0.587620236790419,
5.86458333333332)) ;
#85069 = CARTESIAN_POINT('Ctrl Pts',(-1.35705080756888,8.30953963884779E-17,
5.90624999999999)) ;
#85070 = CARTESIAN_POINT('Ctrl Pts',(-1.01778810567666,-0.587620236790419,
5.94791666666666)) ;
#85071 = CARTESIAN_POINT('Ctrl Pts',(-0.67852540378444,-1.17524047358084,
5.98958333333333)) ;
#85072 = CARTESIAN_POINT('Ctrl Pts',(-1.43925448419919E-16,-1.17524047358084,
6.03124999999999)) ;
#85073 = CARTESIAN_POINT('Ctrl Pts',(0.678525403784439,-1.17524047358084,
6.07291666666666)) ;
#85074 = CARTESIAN_POINT('Ctrl Pts',(1.01778810567666,-0.587620236790419,
6.11458333333332)) ;
#85075 = CARTESIAN_POINT('Ctrl Pts',(1.35705080756888,-2.49286189165434E-16,
6.15624999999999)) ;
#85076 = CARTESIAN_POINT('Ctrl Pts',(1.01778810567666,0.587620236790418,6.19791666666666)) ;
#85077 = CARTESIAN_POINT('Ctrl Pts',(0.67852540378444,1.17524047358084,6.23958333333332)) ;
#85078 = CARTESIAN_POINT('Ctrl Pts',(0.,1.17524047358084,6.28124999999999)) ;
#85079 = CARTESIAN_POINT('Ctrl Pts',(-0.67852540378444,1.17524047358084,6.32291666666666)) ;
#85080 = CARTESIAN_POINT('Ctrl Pts',(-1.01778810567666,0.587620236790419,
6.36458333333332)) ;
#85081 = CARTESIAN_POINT('Ctrl Pts',(-1.35705080756888,8.30953963884779E-17,
6.40624999999999)) ;
#85082 = CARTESIAN_POINT('Ctrl Pts',(-1.01778810567666,-0.587620236790419,
6.44791666666666)) ;
#85083 = CARTESIAN_POINT('Ctrl Pts',(-0.67852540378444,-1.17524047358084,
6.48958333333332)) ;
#85084 = CARTESIAN_POINT('Ctrl Pts',(-1.43925448419919E-16,-1.17524047358084,
6.53124999999999)) ;
#85085 = CARTESIAN_POINT('Ctrl Pts',(0.678525403784439,-1.17524047358084,
6.57291666666666)) ;
#85086 = CARTESIAN_POINT('Ctrl Pts',(1.01778810567666,-0.587620236790419,
6.61458333333332)) ;
#85087 = CARTESIAN_POINT('Ctrl Pts',(1.35705080756888,-2.49286189165434E-16,
6.65624999999999)) ;
#85088 = CARTESIAN_POINT('Ctrl Pts',(1.01778810567666,0.587620236790418,6.69791666666666)) ;
#85089 = CARTESIAN_POINT('Ctrl Pts',(0.67852540378444,1.17524047358084,6.73958333333332)) ;
#85090 = CARTESIAN_POINT('Ctrl Pts',(0.,1.17524047358084,6.78124999999999)) ;
#85091 = CARTESIAN_POINT('Ctrl Pts',(-0.67852540378444,1.17524047358084,6.82291666666666)) ;
#85092 = CARTESIAN_POINT('Ctrl Pts',(-1.01778810567666,0.587620236790419,
6.86458333333332)) ;
#85093 = CARTESIAN_POINT('Ctrl Pts',(-1.35705080756888,8.30953963884779E-17,
6.90624999999999)) ;
#85094 = CARTESIAN_POINT('Ctrl Pts',(-1.01778810567666,-0.587620236790419,
6.94791666666665)) ;
#85095 = CARTESIAN_POINT('Ctrl Pts',(-0.67852540378444,-1.17524047358084,
6.98958333333332)) ;
#85096 = CARTESIAN_POINT('Ctrl Pts',(-1.43925448419919E-16,-1.17524047358084,
7.03124999999999)) ;
#85097 = CARTESIAN_POINT('Ctrl Pts',(0.678525403784439,-1.17524047358084,
7.07291666666666)) ;
#85098 = CARTESIAN_POINT('Ctrl Pts',(1.01778810567666,-0.587620236790419,
7.11458333333332)) ;
#85099 = CARTESIAN_POINT('Ctrl Pts',(1.35705080756888,-2.49286189165434E-16,
7.15624999999999)) ;
#85100 = CARTESIAN_POINT('Ctrl Pts',(1.01778810567666,0.587620236790418,7.19791666666666)) ;
#85101 = CARTESIAN_POINT('Ctrl Pts',(0.67852540378444,1.17524047358084,7.23958333333332)) ;
#85102 = CARTESIAN_POINT('Ctrl Pts',(0.,1.17524047358084,7.28124999999999)) ;
#85103 = CARTESIAN_POINT('Ctrl Pts',(-0.67852540378444,1.17524047358084,7.32291666666665)) ;
#85104 = CARTESIAN_POINT('Ctrl Pts',(-1.01778810567666,0.587620236790419,
7.36458333333332)) ;
#85105 = CARTESIAN_POINT('Ctrl Pts',(-1.35705080756888,8.30953963884779E-17,
7.40624999999999)) ;
#85106 = CARTESIAN_POINT('Ctrl Pts',(-1.01778810567666,-0.587620236790419,
7.44791666666665)) ;
#85107 = CARTESIAN_POINT('Ctrl Pts',(-0.67852540378444,-1.17524047358084,
7.48958333333332)) ;
#85108 = CARTESIAN_POINT('Ctrl Pts',(-1.43925448419919E-16,-1.17524047358084,
7.53124999999999)) ;
#85109 = CARTESIAN_POINT('Ctrl Pts',(0.678525403784439,-1.17524047358084,
7.57291666666665)) ;
#85110 = CARTESIAN_POINT('Ctrl Pts',(1.01778810567666,-0.587620236790419,
7.61458333333332)) ;
#85111 = CARTESIAN_POINT('Ctrl Pts',(1.35705080756888,-2.49286189165434E-16,
7.65624999999999)) ;
#85112 = CARTESIAN_POINT('Ctrl Pts',(1.01778810567666,0.587620236790418,7.69791666666665)) ;
#85113 = CARTESIAN_POINT('Ctrl Pts',(0.67852540378444,1.17524047358084,7.73958333333332)) ;
#85114 = CARTESIAN_POINT('Ctrl Pts',(0.,1.17524047358084,7.78124999999999)) ;
#85115 = CARTESIAN_POINT('Ctrl Pts',(-0.67852540378444,1.17524047358084,7.82291666666665)) ;
#85116 = CARTESIAN_POINT('Ctrl Pts',(-1.01778810567666,0.587620236790419,
7.86458333333332)) ;
#85117 = CARTESIAN_POINT('Ctrl Pts',(-1.35705080756888,8.30953963884779E-17,
7.90624999999999)) ;
#85118 = CARTESIAN_POINT('Ctrl Pts',(-1.01778810567666,-0.587620236790419,
7.94791666666665)) ;
#85119 = CARTESIAN_POINT('Ctrl Pts',(-0.67852540378444,-1.17524047358084,
7.98958333333332)) ;
#85120 = CARTESIAN_POINT('Ctrl Pts',(-1.43925448419919E-16,-1.17524047358084,
8.03124999999999)) ;
#85121 = CARTESIAN_POINT('Ctrl Pts',(0.678525403784439,-1.17524047358084,
8.07291666666665)) ;
#85122 = CARTESIAN_POINT('Ctrl Pts',(1.01778810567666,-0.587620236790419,
8.11458333333332)) ;
#85123 = CARTESIAN_POINT('Ctrl Pts',(1.35705080756888,-2.49286189165434E-16,
8.15624999999999)) ;
#85124 = CARTESIAN_POINT('Ctrl Pts',(1.01778810567666,0.587620236790418,8.19791666666665)) ;
#85125 = CARTESIAN_POINT('Ctrl Pts',(0.67852540378444,1.17524047358084,8.23958333333332)) ;
#85126 = CARTESIAN_POINT('Ctrl Pts',(0.,1.17524047358084,8.28124999999998)) ;
#85127 = CARTESIAN_POINT('Ctrl Pts',(-0.67852540378444,1.17524047358084,8.32291666666665)) ;
#85128 = CARTESIAN_POINT('Ctrl Pts',(-1.01778810567666,0.587620236790419,
8.36458333333332)) ;
#85129 = CARTESIAN_POINT('Ctrl Pts',(-1.35705080756888,8.30953963884779E-17,
8.40624999999999)) ;
#85130 = CARTESIAN_POINT('Ctrl Pts',(-1.01778810567666,-0.587620236790419,
8.44791666666665)) ;
#85131 = CARTESIAN_POINT('Ctrl Pts',(-0.67852540378444,-1.17524047358084,
8.48958333333332)) ;
#85132 = CARTESIAN_POINT('Ctrl Pts',(-1.43925448419919E-16,-1.17524047358084,
8.53124999999999)) ;
#85133 = CARTESIAN_POINT('Ctrl Pts',(0.678525403784439,-1.17524047358084,
8.57291666666665)) ;
#85134 = CARTESIAN_POINT('Ctrl Pts',(1.01778810567666,-0.587620236790419,
8.61458333333332)) ;
#85135 = CARTESIAN_POINT('Ctrl Pts',(1.35705080756888,-2.49286189165434E-16,
8.65624999999998)) ;
#85136 = CARTESIAN_POINT('Ctrl Pts',(1.01778810567666,0.587620236790418,8.69791666666665)) ;
#85137 = CARTESIAN_POINT('Ctrl Pts',(0.67852540378444,1.17524047358084,8.73958333333332)) ;
#85138 = CARTESIAN_POINT('Ctrl Pts',(0.,1.17524047358084,8.78124999999999)) ;
#85139 = CARTESIAN_POINT('Ctrl Pts',(0.,1.5,-0.03125)) ;
#85140 = CARTESIAN_POINT('Ctrl Pts',(-0.866025403784439,1.5,0.0104166666666666)) ;
#85141 = CARTESIAN_POINT('Ctrl Pts',(-1.29903810567666,0.750000000000001,
0.0520833333333332)) ;
#85142 = CARTESIAN_POINT('Ctrl Pts',(-1.73205080756888,1.06057523872491E-16,
0.0937499999999997)) ;
#85143 = CARTESIAN_POINT('Ctrl Pts',(-1.29903810567666,-0.75,0.135416666666666)) ;
#85144 = CARTESIAN_POINT('Ctrl Pts',(-0.866025403784439,-1.5,0.177083333333333)) ;
#85145 = CARTESIAN_POINT('Ctrl Pts',(-1.83697019872103E-16,-1.5,0.21875)) ;
#85146 = CARTESIAN_POINT('Ctrl Pts',(0.866025403784438,-1.5,0.260416666666666)) ;
#85147 = CARTESIAN_POINT('Ctrl Pts',(1.29903810567666,-0.750000000000001,
0.302083333333333)) ;
#85148 = CARTESIAN_POINT('Ctrl Pts',(1.73205080756888,-3.18172571617472E-16,
0.343749999999999)) ;
#85149 = CARTESIAN_POINT('Ctrl Pts',(1.29903810567666,0.749999999999999,0.385416666666666)) ;
#85150 = CARTESIAN_POINT('Ctrl Pts',(0.86602540378444,1.5,0.427083333333332)) ;
#85151 = CARTESIAN_POINT('Ctrl Pts',(0.,1.5,0.468749999999999)) ;
#85152 = CARTESIAN_POINT('Ctrl Pts',(-0.866025403784439,1.5,0.510416666666666)) ;
#85153 = CARTESIAN_POINT('Ctrl Pts',(-1.29903810567666,0.750000000000001,
0.552083333333332)) ;
#85154 = CARTESIAN_POINT('Ctrl Pts',(-1.73205080756888,1.06057523872491E-16,
0.593749999999999)) ;
#85155 = CARTESIAN_POINT('Ctrl Pts',(-1.29903810567666,-0.75,0.635416666666665)) ;
#85156 = CARTESIAN_POINT('Ctrl Pts',(-0.866025403784439,-1.5,0.677083333333332)) ;
#85157 = CARTESIAN_POINT('Ctrl Pts',(-1.83697019872103E-16,-1.5,0.718749999999998)) ;
#85158 = CARTESIAN_POINT('Ctrl Pts',(0.866025403784438,-1.5,0.760416666666665)) ;
#85159 = CARTESIAN_POINT('Ctrl Pts',(1.29903810567666,-0.750000000000001,
0.802083333333332)) ;
#85160 = CARTESIAN_POINT('Ctrl Pts',(1.73205080756888,-3.18172571617472E-16,
0.843749999999998)) ;
#85161 = CARTESIAN_POINT('Ctrl Pts',(1.29903810567666,0.749999999999999,0.885416666666665)) ;
#85162 = CARTESIAN_POINT('Ctrl Pts',(0.86602540378444,1.5,0.927083333333331)) ;
#85163 = CARTESIAN_POINT('Ctrl Pts',(0.,1.5,0.968749999999998)) ;
#85164 = CARTESIAN_POINT('Ctrl Pts',(-0.866025403784439,1.5,1.01041666666666)) ;
#85165 = CARTESIAN_POINT('Ctrl Pts',(-1.29903810567666,0.750000000000001,
1.05208333333333)) ;
#85166 = CARTESIAN_POINT('Ctrl Pts',(-1.73205080756888,1.06057523872491E-16,
1.09375)) ;
#85167 = CARTESIAN_POINT('Ctrl Pts',(-1.29903810567666,-0.75,1.13541666666666)) ;
#85168 = CARTESIAN_POINT('Ctrl Pts',(-0.866025403784439,-1.5,1.17708333333333)) ;
#85169 = CARTESIAN_POINT('Ctrl Pts',(-1.83697019872103E-16,-1.5,1.21875)) ;
#85170 = CARTESIAN_POINT('Ctrl Pts',(0.866025403784438,-1.5,1.26041666666666)) ;
#85171 = CARTESIAN_POINT('Ctrl Pts',(1.29903810567666,-0.750000000000001,
1.30208333333333)) ;
#85172 = CARTESIAN_POINT('Ctrl Pts',(1.73205080756888,-3.18172571617472E-16,
1.34375)) ;
#85173 = CARTESIAN_POINT('Ctrl Pts',(1.29903810567666,0.749999999999999,1.38541666666666)) ;
#85174 = CARTESIAN_POINT('Ctrl Pts',(0.86602540378444,1.5,1.42708333333333)) ;
#85175 = CARTESIAN_POINT('Ctrl Pts',(0.,1.5,1.46875)) ;
#85176 = CARTESIAN_POINT('Ctrl Pts',(-0.866025403784439,1.5,1.51041666666666)) ;
#85177 = CARTESIAN_POINT('Ctrl Pts',(-1.29903810567666,0.750000000000001,
1.55208333333333)) ;
#85178 = CARTESIAN_POINT('Ctrl Pts',(-1.73205080756888,1.06057523872491E-16,
1.59375)) ;
#85179 = CARTESIAN_POINT('Ctrl Pts',(-1.29903810567666,-0.75,1.63541666666666)) ;
#85180 = CARTESIAN_POINT('Ctrl Pts',(-0.866025403784439,-1.5,1.67708333333333)) ;
#85181 = CARTESIAN_POINT('Ctrl Pts',(-1.83697019872103E-16,-1.5,1.71875)) ;
#85182 = CARTESIAN_POINT('Ctrl Pts',(0.866025403784438,-1.5,1.76041666666666)) ;
#85183 = CARTESIAN_POINT('Ctrl Pts',(1.29903810567666,-0.750000000000001,
1.80208333333333)) ;
#85184 = CARTESIAN_POINT('Ctrl Pts',(1.73205080756888,-3.18172571617472E-16,
1.84375)) ;
#85185 = CARTESIAN_POINT('Ctrl Pts',(1.29903810567666,0.749999999999999,1.88541666666666)) ;
#85186 = CARTESIAN_POINT('Ctrl Pts',(0.86602540378444,1.5,1.92708333333333)) ;
#85187 = CARTESIAN_POINT('Ctrl Pts',(0.,1.5,1.96875)) ;
#85188 = CARTESIAN_POINT('Ctrl Pts',(-0.866025403784439,1.5,2.01041666666666)) ;
#85189 = CARTESIAN_POINT('Ctrl Pts',(-1.29903810567666,0.750000000000001,
2.05208333333333)) ;
#85190 = CARTESIAN_POINT('Ctrl Pts',(-1.73205080756888,1.06057523872491E-16,
2.09375)) ;
#85191 = CARTESIAN_POINT('Ctrl Pts',(-1.29903810567666,-0.75,2.13541666666666)) ;
#85192 = CARTESIAN_POINT('Ctrl Pts',(-0.866025403784439,-1.5,2.17708333333333)) ;
#85193 = CARTESIAN_POINT('Ctrl Pts',(-1.83697019872103E-16,-1.5,2.21875)) ;
#85194 = CARTESIAN_POINT('Ctrl Pts',(0.866025403784438,-1.5,2.26041666666666)) ;
#85195 = CARTESIAN_POINT('Ctrl Pts',(1.29903810567666,-0.750000000000001,
2.30208333333333)) ;
#85196 = CARTESIAN_POINT('Ctrl Pts',(1.73205080756888,-3.18172571617472E-16,
2.34374999999999)) ;
#85197 = CARTESIAN_POINT('Ctrl Pts',(1.29903810567666,0.749999999999999,2.38541666666666)) ;
#85198 = CARTESIAN_POINT('Ctrl Pts',(0.86602540378444,1.5,2.42708333333333)) ;
#85199 = CARTESIAN_POINT('Ctrl Pts',(0.,1.5,2.46874999999999)) ;
#85200 = CARTESIAN_POINT('Ctrl Pts',(-0.866025403784439,1.5,2.51041666666666)) ;
#85201 = CARTESIAN_POINT('Ctrl Pts',(-1.29903810567666,0.750000000000001,
2.55208333333333)) ;
#85202 = CARTESIAN_POINT('Ctrl Pts',(-1.73205080756888,1.06057523872491E-16,
2.59374999999999)) ;
#85203 = CARTESIAN_POINT('Ctrl Pts',(-1.29903810567666,-0.75,2.63541666666666)) ;
#85204 = CARTESIAN_POINT('Ctrl Pts',(-0.866025403784439,-1.5,2.67708333333333)) ;
#85205 = CARTESIAN_POINT('Ctrl Pts',(-1.83697019872103E-16,-1.5,2.71874999999999)) ;
#85206 = CARTESIAN_POINT('Ctrl Pts',(0.866025403784438,-1.5,2.76041666666666)) ;
#85207 = CARTESIAN_POINT('Ctrl Pts',(1.29903810567666,-0.750000000000001,
2.80208333333333)) ;
#85208 = CARTESIAN_POINT('Ctrl Pts',(1.73205080756888,-3.18172571617472E-16,
2.84374999999999)) ;
#85209 = CARTESIAN_POINT('Ctrl Pts',(1.29903810567666,0.749999999999999,2.88541666666666)) ;
#85210 = CARTESIAN_POINT('Ctrl Pts',(0.86602540378444,1.5,2.92708333333333)) ;
#85211 = CARTESIAN_POINT('Ctrl Pts',(0.,1.5,2.96874999999999)) ;
#85212 = CARTESIAN_POINT('Ctrl Pts',(-0.866025403784439,1.5,3.01041666666666)) ;
#85213 = CARTESIAN_POINT('Ctrl Pts',(-1.29903810567666,0.750000000000001,
3.05208333333333)) ;
#85214 = CARTESIAN_POINT('Ctrl Pts',(-1.73205080756888,1.06057523872491E-16,
3.09374999999999)) ;
#85215 = CARTESIAN_POINT('Ctrl Pts',(-1.29903810567666,-0.75,3.13541666666666)) ;
#85216 = CARTESIAN_POINT('Ctrl Pts',(-0.866025403784439,-1.5,3.17708333333333)) ;
#85217 = CARTESIAN_POINT('Ctrl Pts',(-1.83697019872103E-16,-1.5,3.21874999999999)) ;
#85218 = CARTESIAN_POINT('Ctrl Pts',(0.866025403784438,-1.5,3.26041666666666)) ;
#85219 = CARTESIAN_POINT('Ctrl Pts',(1.29903810567666,-0.750000000000001,
3.30208333333333)) ;
#85220 = CARTESIAN_POINT('Ctrl Pts',(1.73205080756888,-3.18172571617472E-16,
3.34374999999999)) ;
#85221 = CARTESIAN_POINT('Ctrl Pts',(1.29903810567666,0.749999999999999,3.38541666666666)) ;
#85222 = CARTESIAN_POINT('Ctrl Pts',(0.86602540378444,1.5,3.42708333333333)) ;
#85223 = CARTESIAN_POINT('Ctrl Pts',(0.,1.5,3.46874999999999)) ;
#85224 = CARTESIAN_POINT('Ctrl Pts',(-0.866025403784439,1.5,3.51041666666666)) ;
#85225 = CARTESIAN_POINT('Ctrl Pts',(-1.29903810567666,0.750000000000001,
3.55208333333333)) ;
#85226 = CARTESIAN_POINT('Ctrl Pts',(-1.73205080756888,1.06057523872491E-16,
3.59374999999999)) ;
#85227 = CARTESIAN_POINT('Ctrl Pts',(-1.29903810567666,-0.75,3.63541666666666)) ;
#85228 = CARTESIAN_POINT('Ctrl Pts',(-0.866025403784439,-1.5,3.67708333333333)) ;
#85229 = CARTESIAN_POINT('Ctrl Pts',(-1.83697019872103E-16,-1.5,3.71874999999999)) ;
#85230 = CARTESIAN_POINT('Ctrl Pts',(0.866025403784438,-1.5,3.76041666666666)) ;
#85231 = CARTESIAN_POINT('Ctrl Pts',(1.29903810567666,-0.750000000000001,
3.80208333333333)) ;
#85232 = CARTESIAN_POINT('Ctrl Pts',(1.73205080756888,-3.18172571617472E-16,
3.84374999999999)) ;
#85233 = CARTESIAN_POINT('Ctrl Pts',(1.29903810567666,0.749999999999999,3.88541666666666)) ;
#85234 = CARTESIAN_POINT('Ctrl Pts',(0.86602540378444,1.5,3.92708333333333)) ;
#85235 = CARTESIAN_POINT('Ctrl Pts',(0.,1.5,3.96874999999999)) ;
#85236 = CARTESIAN_POINT('Ctrl Pts',(-0.866025403784439,1.5,4.01041666666666)) ;
#85237 = CARTESIAN_POINT('Ctrl Pts',(-1.29903810567666,0.750000000000001,
4.05208333333332)) ;
#85238 = CARTESIAN_POINT('Ctrl Pts',(-1.73205080756888,1.06057523872491E-16,
4.09374999999999)) ;
#85239 = CARTESIAN_POINT('Ctrl Pts',(-1.29903810567666,-0.75,4.13541666666666)) ;
#85240 = CARTESIAN_POINT('Ctrl Pts',(-0.866025403784439,-1.5,4.17708333333333)) ;
#85241 = CARTESIAN_POINT('Ctrl Pts',(-1.83697019872103E-16,-1.5,4.21874999999999)) ;
#85242 = CARTESIAN_POINT('Ctrl Pts',(0.866025403784438,-1.5,4.26041666666666)) ;
#85243 = CARTESIAN_POINT('Ctrl Pts',(1.29903810567666,-0.750000000000001,
4.30208333333332)) ;
#85244 = CARTESIAN_POINT('Ctrl Pts',(1.73205080756888,-3.18172571617472E-16,
4.34374999999999)) ;
#85245 = CARTESIAN_POINT('Ctrl Pts',(1.29903810567666,0.749999999999999,4.38541666666666)) ;
#85246 = CARTESIAN_POINT('Ctrl Pts',(0.86602540378444,1.5,4.42708333333332)) ;
#85247 = CARTESIAN_POINT('Ctrl Pts',(0.,1.5,4.46874999999999)) ;
#85248 = CARTESIAN_POINT('Ctrl Pts',(-0.866025403784439,1.5,4.51041666666666)) ;
#85249 = CARTESIAN_POINT('Ctrl Pts',(-1.29903810567666,0.750000000000001,
4.55208333333332)) ;
#85250 = CARTESIAN_POINT('Ctrl Pts',(-1.73205080756888,1.06057523872491E-16,
4.59374999999999)) ;
#85251 = CARTESIAN_POINT('Ctrl Pts',(-1.29903810567666,-0.75,4.63541666666666)) ;
#85252 = CARTESIAN_POINT('Ctrl Pts',(-0.866025403784439,-1.5,4.67708333333332)) ;
#85253 = CARTESIAN_POINT('Ctrl Pts',(-1.83697019872103E-16,-1.5,4.71874999999999)) ;
#85254 = CARTESIAN_POINT('Ctrl Pts',(0.866025403784438,-1.5,4.76041666666666)) ;
#85255 = CARTESIAN_POINT('Ctrl Pts',(1.29903810567666,-0.750000000000001,
4.80208333333332)) ;
#85256 = CARTESIAN_POINT('Ctrl Pts',(1.73205080756888,-3.18172571617472E-16,
4.84374999999999)) ;
#85257 = CARTESIAN_POINT('Ctrl Pts',(1.29903810567666,0.749999999999999,4.88541666666666)) ;
#85258 = CARTESIAN_POINT('Ctrl Pts',(0.86602540378444,1.5,4.92708333333332)) ;
#85259 = CARTESIAN_POINT('Ctrl Pts',(0.,1.5,4.96874999999999)) ;
#85260 = CARTESIAN_POINT('Ctrl Pts',(-0.866025403784439,1.5,5.01041666666666)) ;
#85261 = CARTESIAN_POINT('Ctrl Pts',(-1.29903810567666,0.750000000000001,
5.05208333333332)) ;
#85262 = CARTESIAN_POINT('Ctrl Pts',(-1.73205080756888,1.06057523872491E-16,
5.09374999999999)) ;
#85263 = CARTESIAN_POINT('Ctrl Pts',(-1.29903810567666,-0.75,5.13541666666666)) ;
#85264 = CARTESIAN_POINT('Ctrl Pts',(-0.866025403784439,-1.5,5.17708333333332)) ;
#85265 = CARTESIAN_POINT('Ctrl Pts',(-1.83697019872103E-16,-1.5,5.21874999999999)) ;
#85266 = CARTESIAN_POINT('Ctrl Pts',(0.866025403784438,-1.5,5.26041666666666)) ;
#85267 = CARTESIAN_POINT('Ctrl Pts',(1.29903810567666,-0.750000000000001,
5.30208333333332)) ;
#85268 = CARTESIAN_POINT('Ctrl Pts',(1.73205080756888,-3.18172571617472E-16,
5.34374999999999)) ;
#85269 = CARTESIAN_POINT('Ctrl Pts',(1.29903810567666,0.749999999999999,5.38541666666665)) ;
#85270 = CARTESIAN_POINT('Ctrl Pts',(0.86602540378444,1.5,5.42708333333332)) ;
#85271 = CARTESIAN_POINT('Ctrl Pts',(0.,1.5,5.46874999999999)) ;
#85272 = CARTESIAN_POINT('Ctrl Pts',(-0.866025403784439,1.5,5.51041666666666)) ;
#85273 = CARTESIAN_POINT('Ctrl Pts',(-1.29903810567666,0.750000000000001,
5.55208333333332)) ;
#85274 = CARTESIAN_POINT('Ctrl Pts',(-1.73205080756888,1.06057523872491E-16,
5.59374999999999)) ;
#85275 = CARTESIAN_POINT('Ctrl Pts',(-1.29903810567666,-0.75,5.63541666666666)) ;
#85276 = CARTESIAN_POINT('Ctrl Pts',(-0.866025403784439,-1.5,5.67708333333332)) ;
#85277 = CARTESIAN_POINT('Ctrl Pts',(-1.83697019872103E-16,-1.5,5.71874999999999)) ;
#85278 = CARTESIAN_POINT('Ctrl Pts',(0.866025403784438,-1.5,5.76041666666665)) ;
#85279 = CARTESIAN_POINT('Ctrl Pts',(1.29903810567666,-0.750000000000001,
5.80208333333332)) ;
#85280 = CARTESIAN_POINT('Ctrl Pts',(1.73205080756888,-3.18172571617472E-16,
5.84374999999999)) ;
#85281 = CARTESIAN_POINT('Ctrl Pts',(1.29903810567666,0.749999999999999,5.88541666666666)) ;
#85282 = CARTESIAN_POINT('Ctrl Pts',(0.86602540378444,1.5,5.92708333333332)) ;
#85283 = CARTESIAN_POINT('Ctrl Pts',(0.,1.5,5.96874999999999)) ;
#85284 = CARTESIAN_POINT('Ctrl Pts',(-0.866025403784439,1.5,6.01041666666665)) ;
#85285 = CARTESIAN_POINT('Ctrl Pts',(-1.29903810567666,0.750000000000001,
6.05208333333332)) ;
#85286 = CARTESIAN_POINT('Ctrl Pts',(-1.73205080756888,1.06057523872491E-16,
6.09374999999999)) ;
#85287 = CARTESIAN_POINT('Ctrl Pts',(-1.29903810567666,-0.75,6.13541666666665)) ;
#85288 = CARTESIAN_POINT('Ctrl Pts',(-0.866025403784439,-1.5,6.17708333333332)) ;
#85289 = CARTESIAN_POINT('Ctrl Pts',(-1.83697019872103E-16,-1.5,6.21874999999999)) ;
#85290 = CARTESIAN_POINT('Ctrl Pts',(0.866025403784438,-1.5,6.26041666666665)) ;
#85291 = CARTESIAN_POINT('Ctrl Pts',(1.29903810567666,-0.750000000000001,
6.30208333333332)) ;
#85292 = CARTESIAN_POINT('Ctrl Pts',(1.73205080756888,-3.18172571617472E-16,
6.34374999999999)) ;
#85293 = CARTESIAN_POINT('Ctrl Pts',(1.29903810567666,0.749999999999999,6.38541666666665)) ;
#85294 = CARTESIAN_POINT('Ctrl Pts',(0.86602540378444,1.5,6.42708333333332)) ;
#85295 = CARTESIAN_POINT('Ctrl Pts',(0.,1.5,6.46874999999999)) ;
#85296 = CARTESIAN_POINT('Ctrl Pts',(-0.866025403784439,1.5,6.51041666666665)) ;
#85297 = CARTESIAN_POINT('Ctrl Pts',(-1.29903810567666,0.750000000000001,
6.55208333333332)) ;
#85298 = CARTESIAN_POINT('Ctrl Pts',(-1.73205080756888,1.06057523872491E-16,
6.59374999999999)) ;
#85299 = CARTESIAN_POINT('Ctrl Pts',(-1.29903810567666,-0.75,6.63541666666665)) ;
#85300 = CARTESIAN_POINT('Ctrl Pts',(-0.866025403784439,-1.5,6.67708333333332)) ;
#85301 = CARTESIAN_POINT('Ctrl Pts',(-1.83697019872103E-16,-1.5,6.71874999999999)) ;
#85302 = CARTESIAN_POINT('Ctrl Pts',(0.866025403784438,-1.5,6.76041666666665)) ;
#85303 = CARTESIAN_POINT('Ctrl Pts',(1.29903810567666,-0.750000000000001,
6.80208333333332)) ;
#85304 = CARTESIAN_POINT('Ctrl Pts',(1.73205080756888,-3.18172571617472E-16,
6.84374999999999)) ;
#85305 = CARTESIAN_POINT('Ctrl Pts',(1.29903810567666,0.749999999999999,6.88541666666665)) ;
#85306 = CARTESIAN_POINT('Ctrl Pts',(0.86602540378444,1.5,6.92708333333332)) ;
#85307 = CARTESIAN_POINT('Ctrl Pts',(0.,1.5,6.96874999999999)) ;
#85308 = CARTESIAN_POINT('Ctrl Pts',(-0.866025403784439,1.5,7.01041666666665)) ;
#85309 = CARTESIAN_POINT('Ctrl Pts',(-1.29903810567666,0.750000000000001,
7.05208333333332)) ;
#85310 = CARTESIAN_POINT('Ctrl Pts',(-1.73205080756888,1.06057523872491E-16,
7.09374999999999)) ;
#85311 = CARTESIAN_POINT('Ctrl Pts',(-1.29903810567666,-0.75,7.13541666666665)) ;
#85312 = CARTESIAN_POINT('Ctrl Pts',(-0.866025403784439,-1.5,7.17708333333332)) ;
#85313 = CARTESIAN_POINT('Ctrl Pts',(-1.83697019872103E-16,-1.5,7.21874999999998)) ;
#85314 = CARTESIAN_POINT('Ctrl Pts',(0.866025403784438,-1.5,7.26041666666665)) ;
#85315 = CARTESIAN_POINT('Ctrl Pts',(1.29903810567666,-0.750000000000001,
7.30208333333332)) ;
#85316 = CARTESIAN_POINT('Ctrl Pts',(1.73205080756888,-3.18172571617472E-16,
7.34374999999998)) ;
#85317 = CARTESIAN_POINT('Ctrl Pts',(1.29903810567666,0.749999999999999,7.38541666666665)) ;
#85318 = CARTESIAN_POINT('Ctrl Pts',(0.86602540378444,1.5,7.42708333333332)) ;
#85319 = CARTESIAN_POINT('Ctrl Pts',(0.,1.5,7.46874999999998)) ;
#85320 = CARTESIAN_POINT('Ctrl Pts',(-0.866025403784439,1.5,7.51041666666665)) ;
#85321 = CARTESIAN_POINT('Ctrl Pts',(-1.29903810567666,0.750000000000001,
7.55208333333332)) ;
#85322 = CARTESIAN_POINT('Ctrl Pts',(-1.73205080756888,1.06057523872491E-16,
7.59374999999998)) ;
#85323 = CARTESIAN_POINT('Ctrl Pts',(-1.29903810567666,-0.75,7.63541666666665)) ;
#85324 = CARTESIAN_POINT('Ctrl Pts',(-0.866025403784439,-1.5,7.67708333333332)) ;
#85325 = CARTESIAN_POINT('Ctrl Pts',(-1.83697019872103E-16,-1.5,7.71874999999998)) ;
#85326 = CARTESIAN_POINT('Ctrl Pts',(0.866025403784438,-1.5,7.76041666666665)) ;
#85327 = CARTESIAN_POINT('Ctrl Pts',(1.29903810567666,-0.750000000000001,
7.80208333333332)) ;
#85328 = CARTESIAN_POINT('Ctrl Pts',(1.73205080756888,-3.18172571617472E-16,
7.84374999999998)) ;
#85329 = CARTESIAN_POINT('Ctrl Pts',(1.29903810567666,0.749999999999999,7.88541666666665)) ;
#85330 = CARTESIAN_POINT('Ctrl Pts',(0.86602540378444,1.5,7.92708333333332)) ;
#85331 = CARTESIAN_POINT('Ctrl Pts',(0.,1.5,7.96874999999998)) ;
#85332 = CARTESIAN_POINT('Ctrl Pts',(-0.866025403784439,1.5,8.01041666666665)) ;
#85333 = CARTESIAN_POINT('Ctrl Pts',(-1.29903810567666,0.750000000000001,
8.05208333333332)) ;
#85334 = CARTESIAN_POINT('Ctrl Pts',(-1.73205080756888,1.06057523872491E-16,
8.09374999999998)) ;
#85335 = CARTESIAN_POINT('Ctrl Pts',(-1.29903810567666,-0.75,8.13541666666665)) ;
#85336 = CARTESIAN_POINT('Ctrl Pts',(-0.866025403784439,-1.5,8.17708333333332)) ;
#85337 = CARTESIAN_POINT('Ctrl Pts',(-1.83697019872103E-16,-1.5,8.21874999999998)) ;
#85338 = CARTESIAN_POINT('Ctrl Pts',(0.866025403784438,-1.5,8.26041666666665)) ;
#85339 = CARTESIAN_POINT('Ctrl Pts',(1.29903810567666,-0.750000000000001,
8.30208333333332)) ;
#85340 = CARTESIAN_POINT('Ctrl Pts',(1.73205080756888,-3.18172571617472E-16,
8.34374999999998)) ;
#85341 = CARTESIAN_POINT('Ctrl Pts',(1.29903810567666,0.749999999999999,8.38541666666665)) ;
#85342 = CARTESIAN_POINT('Ctrl Pts',(0.86602540378444,1.5,8.42708333333332)) ;
#85343 = CARTESIAN_POINT('Ctrl Pts',(0.,1.5,8.46874999999998)) ;
#85344 = CARTESIAN_POINT('Ctrl Pts',(-0.866025403784439,1.5,8.51041666666665)) ;
#85345 = CARTESIAN_POINT('Ctrl Pts',(-1.29903810567666,0.750000000000001,
8.55208333333331)) ;
#85346 = CARTESIAN_POINT('Ctrl Pts',(-1.73205080756888,1.06057523872491E-16,
8.59374999999998)) ;
#85347 = CARTESIAN_POINT('Ctrl Pts',(-1.29903810567666,-0.75,8.63541666666665)) ;
#85348 = CARTESIAN_POINT('Ctrl Pts',(-0.866025403784439,-1.5,8.67708333333331)) ;
#85349 = CARTESIAN_POINT('Ctrl Pts',(-1.83697019872103E-16,-1.5,8.71874999999998)) ;
#85350 = CARTESIAN_POINT('Ctrl Pts',(0.866025403784438,-1.5,8.76041666666665)) ;
#85351 = CARTESIAN_POINT('Ctrl Pts',(1.29903810567666,-0.750000000000001,
8.80208333333331)) ;
#85352 = CARTESIAN_POINT('Ctrl Pts',(1.73205080756888,-3.18172571617472E-16,
8.84374999999998)) ;
#85353 = CARTESIAN_POINT('Ctrl Pts',(1.29903810567666,0.749999999999999,8.88541666666665)) ;
#85354 = CARTESIAN_POINT('Ctrl Pts',(0.86602540378444,1.5,8.92708333333331)) ;
#85355 = CARTESIAN_POINT('Ctrl Pts',(0.,1.5,8.96874999999998)) ;
#85356 = CARTESIAN_POINT('Ctrl Pts',(-0.000186377689213934,1.49999998842112,
0.0312589667791176)) ;
#85357 = CARTESIAN_POINT('Ctrl Pts',(0.865963275659358,1.50010760906922,-0.0104106883850433)) ;
#85358 = CARTESIAN_POINT('Ctrl Pts',(1.29903810567666,0.750000000000001,-0.0520833333333332)) ;
#85359 = CARTESIAN_POINT('Ctrl Pts',(1.73205080756888,1.06057523872491E-16,
-0.0937499999999997)) ;
#85360 = CARTESIAN_POINT('Ctrl Pts',(1.29903810567666,-0.75,-0.135416666666666)) ;
#85361 = CARTESIAN_POINT('Ctrl Pts',(0.866025403784439,-1.5,-0.177083333333333)) ;
#85362 = CARTESIAN_POINT('Ctrl Pts',(1.83697019872103E-16,-1.5,-0.21875)) ;
#85363 = CARTESIAN_POINT('Ctrl Pts',(-0.866025403784438,-1.5,-0.260416666666666)) ;
#85364 = CARTESIAN_POINT('Ctrl Pts',(-1.29903810567666,-0.750000000000001,
-0.302083333333333)) ;
#85365 = CARTESIAN_POINT('Ctrl Pts',(-1.73205080756888,-3.18172571617472E-16,
-0.343749999999999)) ;
#85366 = CARTESIAN_POINT('Ctrl Pts',(-1.29903810567666,0.749999999999999,
-0.385416666666666)) ;
#85367 = CARTESIAN_POINT('Ctrl Pts',(-0.86602540378444,1.5,-0.427083333333332)) ;
#85368 = CARTESIAN_POINT('Ctrl Pts',(0.,1.5,-0.468749999999999)) ;
#85369 = CARTESIAN_POINT('Ctrl Pts',(-0.000146025735824457,1.17524046450886,
0.218758966779122)) ;
#85370 = CARTESIAN_POINT('Ctrl Pts',(0.678476726793011,1.17532478460315,0.177089311614961)) ;
#85371 = CARTESIAN_POINT('Ctrl Pts',(1.01778810567666,0.587620236790419,0.135416666666671)) ;
#85372 = CARTESIAN_POINT('Ctrl Pts',(1.35705080756888,8.30953963884779E-17,
0.0937500000000043)) ;
#85373 = CARTESIAN_POINT('Ctrl Pts',(1.01778810567666,-0.587620236790419,
0.0520833333333377)) ;
#85374 = CARTESIAN_POINT('Ctrl Pts',(0.67852540378444,-1.17524047358084,0.0104166666666711)) ;
#85375 = CARTESIAN_POINT('Ctrl Pts',(1.43925448419919E-16,-1.17524047358084,
-0.0312499999999955)) ;
#85376 = CARTESIAN_POINT('Ctrl Pts',(-0.678525403784439,-1.17524047358084,
-0.0729166666666621)) ;
#85377 = CARTESIAN_POINT('Ctrl Pts',(-1.01778810567666,-0.587620236790419,
-0.114583333333329)) ;
#85378 = CARTESIAN_POINT('Ctrl Pts',(-1.35705080756888,-2.49286189165434E-16,
-0.156249999999995)) ;
#85379 = CARTESIAN_POINT('Ctrl Pts',(-1.01778810567666,0.587620236790418,
-0.197916666666662)) ;
#85380 = CARTESIAN_POINT('Ctrl Pts',(-0.67852540378444,1.17524047358084,-0.239583333333328)) ;
#85381 = CARTESIAN_POINT('Ctrl Pts',(0.,1.17524047358084,-0.281249999999995)) ;
#85382 = CARTESIAN_POINT('Origin',(0.,0.,9.56735957759373E-18)) ;
#85383 = CARTESIAN_POINT('Origin',(0.,0.,10.5)) ;
#85384 = CARTESIAN_POINT('',(-0.214086590007416,0.905647899858295,8.375)) ;
#85385 = CARTESIAN_POINT('Ctrl Pts',(-0.214086590007055,0.905647899857224,
8.37499999999588)) ;
#85386 = CARTESIAN_POINT('Ctrl Pts',(-0.27901076445186,1.09462213692769,9.11708670961361)) ;
#85387 = CARTESIAN_POINT('Ctrl Pts',(-0.378092453297399,1.38212190130695,
10.249595595364)) ;
#85388 = CARTESIAN_POINT('',(0.214086590007411,0.905647899858296,8.375)) ;
#85389 = CARTESIAN_POINT('Origin',(0.,0.,8.375)) ;
#85390 = CARTESIAN_POINT('Ctrl Pts',(0.21408659000705,0.905647899857235,8.37499999999588)) ;
#85391 = CARTESIAN_POINT('Ctrl Pts',(0.279010764449613,1.09462213692116,9.11708670958797)) ;
#85392 = CARTESIAN_POINT('Ctrl Pts',(0.378092453294824,1.38212190129948,10.2495955953347)) ;
#85393 = CARTESIAN_POINT('Origin',(0.4,6.2338841963792E-17,10.5)) ;
#85394 = CARTESIAN_POINT('',(0.214086590007411,0.713019523490749,8.375)) ;
#85395 = CARTESIAN_POINT('',(0.214086590007411,3.33647752525978E-17,8.375)) ;
#85396 = CARTESIAN_POINT('',(0.398867118306387,0.749774655820362,10.4870511029892)) ;
#85397 = CARTESIAN_POINT('Origin',(0.606586399182262,0.251256313292347,10.5)) ;
#85398 = CARTESIAN_POINT('',(0.360220662867382,0.360220662867381,8.375)) ;
#85399 = CARTESIAN_POINT('',(0.434824804870729,0.180110331433686,8.375)) ;
#85400 = CARTESIAN_POINT('',(0.501858559970094,0.501858559970092,10.4902321148732)) ;
#85401 = CARTESIAN_POINT('Origin',(0.251256313292348,0.606586399182262,10.5)) ;
#85402 = CARTESIAN_POINT('',(0.71301952349075,0.214086590007409,8.375)) ;
#85403 = CARTESIAN_POINT('',(0.180110331433687,0.434824804870729,8.375)) ;
#85404 = CARTESIAN_POINT('',(0.750162198617137,0.400815427513497,10.5093203791284)) ;
#85405 = CARTESIAN_POINT('Origin',(0.,0.399999999999998,10.5)) ;
#85406 = CARTESIAN_POINT('',(0.,0.214086590007409,8.375)) ;
#85407 = CARTESIAN_POINT('Origin',(0.,0.,8.375)) ;
#85408 = CARTESIAN_POINT('',(0.713019523490766,-0.21408659000743,8.375)) ;
#85409 = CARTESIAN_POINT('',(-7.51067965057384E-16,-0.214086590007428,8.375)) ;
#85410 = CARTESIAN_POINT('',(-0.214086590007418,0.713019523490736,8.375)) ;
#85411 = CARTESIAN_POINT('',(-0.214086590007425,2.27939140812495E-15,8.375)) ;
#85412 = CARTESIAN_POINT('',(-0.360220662867393,0.360220662867369,8.375)) ;
#85413 = CARTESIAN_POINT('',(-0.434824804870735,0.180110331433695,8.375)) ;
#85414 = CARTESIAN_POINT('',(-0.713019523490764,0.214086590007402,8.375)) ;
#85415 = CARTESIAN_POINT('',(-0.180110331433678,0.434824804870723,8.375)) ;
#85416 = CARTESIAN_POINT('',(-0.905647899858292,0.214086590007404,8.375)) ;
#85417 = CARTESIAN_POINT('',(2.24602663287203E-15,0.214086590007395,8.375)) ;
#85418 = CARTESIAN_POINT('',(-0.905647899858305,-0.214086590007436,8.375)) ;
#85419 = CARTESIAN_POINT('Origin',(-4.11190782820327E-15,-4.14316783061991E-14,
8.375)) ;
#85420 = CARTESIAN_POINT('',(-0.713019523490751,-0.214086590007437,8.375)) ;
#85421 = CARTESIAN_POINT('',(-1.49495866781509E-15,-0.214086590007442,8.375)) ;
#85422 = CARTESIAN_POINT('',(-0.360220662867385,-0.360220662867411,8.375)) ;
#85423 = CARTESIAN_POINT('',(-0.180110331433702,-0.434824804870756,8.375)) ;
#85424 = CARTESIAN_POINT('',(-0.214086590007416,-0.713019523490781,8.375)) ;
#85425 = CARTESIAN_POINT('',(-0.434824804870743,-0.180110331433688,8.375)) ;
#85426 = CARTESIAN_POINT('',(-0.214086590007411,1.53550070536725E-15,8.375)) ;
#85427 = CARTESIAN_POINT('',(0.214086590007423,-0.713019523490768,8.375)) ;
#85428 = CARTESIAN_POINT('',(0.214086590007425,-7.10525927504996E-16,8.375)) ;
#85429 = CARTESIAN_POINT('',(0.360220662867396,-0.3602206628674,8.375)) ;
#85430 = CARTESIAN_POINT('',(0.434824804870748,-0.180110331433697,8.375)) ;
#85431 = CARTESIAN_POINT('',(0.180110331433693,-0.43482480487075,8.375)) ;
#85432 = CARTESIAN_POINT('Origin',(1.93815854595261E-14,-0.400000000000021,
10.5)) ;
#85433 = CARTESIAN_POINT('',(0.749774655820382,-0.398867118306411,10.4870511029892)) ;
#85434 = CARTESIAN_POINT('Origin',(0.251256313292365,-0.606586399182284,10.5)) ;
#85435 = CARTESIAN_POINT('',(0.501858559970111,-0.501858559970116,10.4902321148732)) ;
#85436 = CARTESIAN_POINT('Origin',(0.606586399182282,-0.251256313292371,10.5)) ;
#85437 = CARTESIAN_POINT('',(0.400815427513515,-0.75016219861716,10.5093203791284)) ;
#85438 = CARTESIAN_POINT('Origin',(0.400000000000019,-2.21124316886369E-14,
10.5)) ;
#85439 = CARTESIAN_POINT('Origin',(-0.4,-3.87008320770884E-14,10.5)) ;
#85440 = CARTESIAN_POINT('',(-0.398867118306393,-0.749774655820401,10.4870511029892)) ;
#85441 = CARTESIAN_POINT('Origin',(-0.606586399182264,-0.251256313292384,
10.5)) ;
#85442 = CARTESIAN_POINT('',(-0.501858559970097,-0.50185855997013,10.4902321148732)) ;
#85443 = CARTESIAN_POINT('Origin',(-0.251256313292353,-0.606586399182301,
10.5)) ;
#85444 = CARTESIAN_POINT('',(-0.75016219861714,-0.400815427513533,10.5093203791284)) ;
#85445 = CARTESIAN_POINT('Origin',(-2.79318507107464E-15,-0.400000000000039,
10.5)) ;
#85446 = CARTESIAN_POINT('Ctrl Pts',(-0.905647899857242,-0.214086590007075,
8.37499999999588)) ;
#85447 = CARTESIAN_POINT('Ctrl Pts',(-1.09462213691718,-0.279010764448275,
9.11708670957237)) ;
#85448 = CARTESIAN_POINT('Ctrl Pts',(-1.38212190129947,-0.378092453294853,
10.2495955953347)) ;
#85449 = CARTESIAN_POINT('Origin',(1.12142940769163E-15,-4.14316783061991E-14,
10.5)) ;
#85450 = CARTESIAN_POINT('Ctrl Pts',(-0.905647899857243,0.214086590007043,
8.37499999999588)) ;
#85451 = CARTESIAN_POINT('Ctrl Pts',(-1.09462213691218,0.279010764446527,
9.11708670955277)) ;
#85452 = CARTESIAN_POINT('Ctrl Pts',(-1.38212190129944,0.37809245329482,10.2495955953347)) ;
#85453 = CARTESIAN_POINT('Origin',(-1.65884003884516E-14,0.399999999999979,
10.5)) ;
#85454 = CARTESIAN_POINT('',(-0.749774655820378,0.398867118306375,10.4870511029892)) ;
#85455 = CARTESIAN_POINT('Origin',(-0.251256313292361,0.606586399182244,10.5)) ;
#85456 = CARTESIAN_POINT('',(-0.501858559970107,0.501858559970078,10.4902321148732)) ;
#85457 = CARTESIAN_POINT('Origin',(-0.60658639918228,0.251256313292334,10.5)) ;
#85458 = CARTESIAN_POINT('',(-0.400815427513509,0.75016219861712,10.5093203791284)) ;
#85459 = CARTESIAN_POINT('Origin',(-0.400000000000019,-1.65260615464876E-14,
10.5)) ;
#85460 = CARTESIAN_POINT('',(0.,0.,0.)) ;
#85461 = CARTESIAN_POINT('Origin',(1.4210854715202E-13,2.24999999999996,1.15)) ;
#85462 = CARTESIAN_POINT('',(1.4210854715202E-13,2.79999999999996,1.15)) ;
#85463 = CARTESIAN_POINT('',(1.4210854715202E-13,1.69999999999996,1.15)) ;
#85464 = CARTESIAN_POINT('',(1.4210854715202E-13,2.79999999999996,1.15)) ;
#85465 = CARTESIAN_POINT('',(1.4210854715202E-13,1.69999999999996,0.250000000000004)) ;
#85466 = CARTESIAN_POINT('',(1.4210854715202E-13,1.69999999999996,1.15)) ;
#85467 = CARTESIAN_POINT('',(1.4210854715202E-13,2.79999999999996,0.250000000000004)) ;
#85468 = CARTESIAN_POINT('',(1.4210854715202E-13,1.69999999999996,0.250000000000004)) ;
#85469 = CARTESIAN_POINT('',(1.4210854715202E-13,2.79999999999996,0.250000000000004)) ;
#85470 = CARTESIAN_POINT('Origin',(0.124026857534672,1.97110180828134,0.15959890864801)) ;
#85471 = CARTESIAN_POINT('',(0.106761092397404,1.69664435550248,0.159599907562201)) ;
#85472 = CARTESIAN_POINT('',(0.175835544643537,2.7944734497289,0.159598908636084)) ;
#85473 = CARTESIAN_POINT('',(0.106757295053336,1.69664459439572,0.159599945745868)) ;
#85474 = CARTESIAN_POINT('',(0.175868969413493,2.7944713463616,-0.740399164074464)) ;
#85475 = CARTESIAN_POINT('',(0.175835544859223,2.79447344971533,0.159598908636091)) ;
#85476 = CARTESIAN_POINT('',(0.106787672964718,1.69664268279975,-0.740398325032857)) ;
#85477 = CARTESIAN_POINT('',(0.17586791258293,2.79447141282259,-0.740399301632037)) ;
#85478 = CARTESIAN_POINT('',(0.106787673732876,1.69664268281332,-0.740399016126806)) ;
#85479 = CARTESIAN_POINT('Ctrl Pts',(1.4210854715202E-13,2.79999999999996,
1.15)) ;
#85480 = CARTESIAN_POINT('Ctrl Pts',(-1.15979797464453,2.79999999999996,1.0875)) ;
#85481 = CARTESIAN_POINT('Ctrl Pts',(-1.97989898732219,1.97989898732229,1.025)) ;
#85482 = CARTESIAN_POINT('Ctrl Pts',(-2.79999999999986,1.15979797464463,0.962500000000004)) ;
#85483 = CARTESIAN_POINT('Ctrl Pts',(-2.79999999999986,-3.53556862361244E-14,
0.900000000000004)) ;
#85484 = CARTESIAN_POINT('Ctrl Pts',(-2.79999999999986,-1.15979797464471,
0.837500000000003)) ;
#85485 = CARTESIAN_POINT('Ctrl Pts',(-1.97989898732219,-1.97989898732237,
0.775000000000004)) ;
#85486 = CARTESIAN_POINT('Ctrl Pts',(-1.15979797464453,-2.80000000000004,
0.712500000000004)) ;
#85487 = CARTESIAN_POINT('Ctrl Pts',(1.41765646048259E-13,-2.80000000000004,
0.650000000000004)) ;
#85488 = CARTESIAN_POINT('Ctrl Pts',(1.15979797464481,-2.80000000000004,0.587500000000004)) ;
#85489 = CARTESIAN_POINT('Ctrl Pts',(1.97989898732247,-1.97989898732237,0.525000000000004)) ;
#85490 = CARTESIAN_POINT('Ctrl Pts',(2.80000000000014,-1.15979797464471,0.462500000000004)) ;
#85491 = CARTESIAN_POINT('Ctrl Pts',(2.80000000000014,-3.60414884436469E-14,
0.400000000000004)) ;
#85492 = CARTESIAN_POINT('Ctrl Pts',(2.80000000000014,1.15979797464463,0.337500000000003)) ;
#85493 = CARTESIAN_POINT('Ctrl Pts',(1.97989898732247,1.97989898732229,0.275000000000004)) ;
#85494 = CARTESIAN_POINT('Ctrl Pts',(1.23176644636502,2.72803152827974,0.217984726165415)) ;
#85495 = CARTESIAN_POINT('Ctrl Pts',(0.175835544859223,2.79447344971533,0.15959890864801)) ;
#85496 = CARTESIAN_POINT('Ctrl Pts',(1.4210854715202E-13,1.69999999987093,
1.15)) ;
#85497 = CARTESIAN_POINT('Ctrl Pts',(-0.704163055980671,1.69999999987093,
1.0875)) ;
#85498 = CARTESIAN_POINT('Ctrl Pts',(-1.20208152792574,1.20208152792585,1.025)) ;
#85499 = CARTESIAN_POINT('Ctrl Pts',(-1.69999999987082,0.704163055980777,
0.962500000000004)) ;
#85500 = CARTESIAN_POINT('Ctrl Pts',(-1.69999999987082,-3.54230418100854E-14,
0.900000000000004)) ;
#85501 = CARTESIAN_POINT('Ctrl Pts',(-1.69999999987082,-0.704163055980848,
0.837500000000003)) ;
#85502 = CARTESIAN_POINT('Ctrl Pts',(-1.20208152792574,-1.20208152792592,
0.775000000000004)) ;
#85503 = CARTESIAN_POINT('Ctrl Pts',(-0.704163055980671,-1.699999999871,0.712500000000004)) ;
#85504 = CARTESIAN_POINT('Ctrl Pts',(1.41900357196181E-13,-1.699999999871,
0.650000000000004)) ;
#85505 = CARTESIAN_POINT('Ctrl Pts',(0.704163055980954,-1.699999999871,0.587500000000004)) ;
#85506 = CARTESIAN_POINT('Ctrl Pts',(1.20208152792603,-1.20208152792592,0.525000000000004)) ;
#85507 = CARTESIAN_POINT('Ctrl Pts',(1.6999999998711,-0.704163055980849,0.462500000000004)) ;
#85508 = CARTESIAN_POINT('Ctrl Pts',(1.6999999998711,-3.58394217217639E-14,
0.400000000000004)) ;
#85509 = CARTESIAN_POINT('Ctrl Pts',(1.6999999998711,0.704163055980777,0.337500000000003)) ;
#85510 = CARTESIAN_POINT('Ctrl Pts',(1.20208152792603,1.20208152792585,0.275000000000003)) ;
#85511 = CARTESIAN_POINT('Ctrl Pts',(0.747858199522055,1.65630485632982,0.217984726165415)) ;
#85512 = CARTESIAN_POINT('Ctrl Pts',(0.106757295085052,1.69664459434123,0.15959890864801)) ;
#85513 = CARTESIAN_POINT('Ctrl Pts',(1.4210854715202E-13,2.79999999999996,
1.15)) ;
#85514 = CARTESIAN_POINT('Ctrl Pts',(-0.0714659907330142,2.79999999999996,
1.14614879098044)) ;
#85515 = CARTESIAN_POINT('Ctrl Pts',(-0.143478336975935,2.797260141978,1.14220698202999)) ;
#85516 = CARTESIAN_POINT('Ctrl Pts',(-0.2157221640937,2.79167762249126,1.13818924661231)) ;
#85517 = CARTESIAN_POINT('Ctrl Pts',(-0.287457311955147,2.78613441033324,
1.13419980065195)) ;
#85518 = CARTESIAN_POINT('Ctrl Pts',(-0.359420096621436,2.77778812917758,
1.1301355191367)) ;
#85519 = CARTESIAN_POINT('Ctrl Pts',(-0.431282451398577,2.76658552138106,
1.12601289236609)) ;
#85520 = CARTESIAN_POINT('Ctrl Pts',(-0.503677894492994,2.75529981055572,
1.1218596831831)) ;
#85521 = CARTESIAN_POINT('Ctrl Pts',(-0.575970755478037,2.74111495138184,
1.1176472888834)) ;
#85522 = CARTESIAN_POINT('Ctrl Pts',(-0.647814825571844,2.72402935956442,
1.11339433084291)) ;
#85523 = CARTESIAN_POINT('Ctrl Pts',(-0.718447061165465,2.70723196007231,
1.1092131098473)) ;
#85524 = CARTESIAN_POINT('Ctrl Pts',(-0.788644831515218,2.68763094901302,
1.10499272100163)) ;
#85525 = CARTESIAN_POINT('Ctrl Pts',(-0.858078848064758,2.66527685062985,
1.10075203700996)) ;
#85526 = CARTESIAN_POINT('Ctrl Pts',(-0.927415582489676,2.64295407196997,
1.09651729452605)) ;
#85527 = CARTESIAN_POINT('Ctrl Pts',(-0.995990034381895,2.6178860276894,1.09226235220303)) ;
#85528 = CARTESIAN_POINT('Ctrl Pts',(-1.06348409700904,2.59017404345893,1.0880066141315)) ;
#85529 = CARTESIAN_POINT('Ctrl Pts',(-1.13098269717863,2.56246019618599,1.08375058995196)) ;
#85530 = CARTESIAN_POINT('Ctrl Pts',(-1.19740013263787,2.53210230701676,1.07949380953604)) ;
#85531 = CARTESIAN_POINT('Ctrl Pts',(-1.26243781057107,2.49925004240071,1.07525570443007)) ;
#85532 = CARTESIAN_POINT('Ctrl Pts',(-1.32956223361152,2.4653437072116,1.07088161899123)) ;
#85533 = CARTESIAN_POINT('Ctrl Pts',(-1.39521615895517,2.4287805517685,1.06652747273162)) ;
#85534 = CARTESIAN_POINT('Ctrl Pts',(-1.45910321389247,2.38977358994698,1.06221399156396)) ;
#85535 = CARTESIAN_POINT('Ctrl Pts',(-1.52143949914674,2.35171346804285,1.05800521417126)) ;
#85536 = CARTESIAN_POINT('Ctrl Pts',(-1.58209333574021,2.31132743945059,1.05383518418228)) ;
#85537 = CARTESIAN_POINT('Ctrl Pts',(-1.64082699787103,2.26885141934347,1.04972197829408)) ;
#85538 = CARTESIAN_POINT('Ctrl Pts',(-1.70175237824991,2.22479035473213,1.04545528311072)) ;
#85539 = CARTESIAN_POINT('Ctrl Pts',(-1.76061095855822,2.17848089233089,1.04124977763653)) ;
#85540 = CARTESIAN_POINT('Ctrl Pts',(-1.81718623839383,2.13021927861696,1.03712374144037)) ;
#85541 = CARTESIAN_POINT('Ctrl Pts',(-1.87376151822945,2.08195766490304,1.0329977052442)) ;
#85542 = CARTESIAN_POINT('Ctrl Pts',(-1.92805331228645,2.03174466235803,1.02895116533164)) ;
#85543 = CARTESIAN_POINT('Ctrl Pts',(-1.97989898732219,1.97989898732229,1.025)) ;
#85544 = CARTESIAN_POINT('Ctrl Pts',(-2.03043307399382,1.92936490065066,1.02114879098044)) ;
#85545 = CARTESIAN_POINT('Ctrl Pts',(-2.07941612016453,1.87650711010632,1.01720698202999)) ;
#85546 = CARTESIAN_POINT('Ctrl Pts',(-2.12655278283319,1.82147557266729,1.01318924661231)) ;
#85547 = CARTESIAN_POINT('Ctrl Pts',(-2.17335754942893,1.76683152025858,1.00919980065196)) ;
#85548 = CARTESIAN_POINT('Ctrl Pts',(-2.21834121045665,1.71004443522516,1.00513551913671)) ;
#85549 = CARTESIAN_POINT('Ctrl Pts',(-2.26123412889168,1.65130863691035,1.0010128923661)) ;
#85550 = CARTESIAN_POINT('Ctrl Pts',(-2.30444523497565,1.59213712551618,0.996859683183108)) ;
#85551 = CARTESIAN_POINT('Ctrl Pts',(-2.34553379709752,1.53098814317025,0.992647288883404)) ;
#85552 = CARTESIAN_POINT('Ctrl Pts',(-2.38425388841422,1.46810537618418,0.988394330842914)) ;
#85553 = CARTESIAN_POINT('Ctrl Pts',(-2.42232086608566,1.4062832883384,0.984213109847312)) ;
#85554 = CARTESIAN_POINT('Ctrl Pts',(-2.45809817768602,1.34278596106178,0.979992721001642)) ;
#85555 = CARTESIAN_POINT('Ctrl Pts',(-2.49138870707918,1.27788196256053,0.975752037009966)) ;
#85556 = CARTESIAN_POINT('Ctrl Pts',(-2.52463259401104,1.21306889929801,0.971517294526055)) ;
#85557 = CARTESIAN_POINT('Ctrl Pts',(-2.55539626985831,1.14685365524698,0.96726235220304)) ;
#85558 = CARTESIAN_POINT('Ctrl Pts',(-2.58352644726229,1.07953281390399,0.963006614131509)) ;
#85559 = CARTESIAN_POINT('Ctrl Pts',(-2.61165851582335,1.01220744666401,0.958750589951965)) ;
#85560 = CARTESIAN_POINT('Ctrl Pts',(-2.63715646553154,0.943776958367677,
0.95449380953605)) ;
#85561 = CARTESIAN_POINT('Ctrl Pts',(-2.65991498954339,0.874558316181138,
0.950255704430076)) ;
#85562 = CARTESIAN_POINT('Ctrl Pts',(-2.68340372472112,0.803118781928595,
0.94588161899124)) ;
#85563 = CARTESIAN_POINT('Ctrl Pts',(-2.70397400538774,0.730840390951192,
0.941527472731625)) ;
#85564 = CARTESIAN_POINT('Ctrl Pts',(-2.72156688794646,0.658083333957503,
0.937213991563964)) ;
#85565 = CARTESIAN_POINT('Ctrl Pts',(-2.73873272767254,0.587092353649035,
0.933005214171264)) ;
#85566 = CARTESIAN_POINT('Ctrl Pts',(-2.75306423214998,0.515646379806024,
0.928835184182286)) ;
#85567 = CARTESIAN_POINT('Ctrl Pts',(-2.76456012107105,0.444080327173848,
0.924721978294091)) ;
#85568 = CARTESIAN_POINT('Ctrl Pts',(-2.77648499311034,0.369843699988586,
0.920455283110725)) ;
#85569 = CARTESIAN_POINT('Ctrl Pts',(-2.78535855948034,0.295478663824547,
0.916249777636538)) ;
#85570 = CARTESIAN_POINT('Ctrl Pts',(-2.79123720917151,0.221347785477126,
0.912123741440374)) ;
#85571 = CARTESIAN_POINT('Ctrl Pts',(-2.79711585886268,0.147216907129704,
0.90799770524421)) ;
#85572 = CARTESIAN_POINT('Ctrl Pts',(-2.79999999999986,0.0733208567859007,
0.903951165331643)) ;
#85573 = CARTESIAN_POINT('Ctrl Pts',(-2.79999999999986,-3.530509218308E-14,
0.900000000000004)) ;
#85574 = CARTESIAN_POINT('Ctrl Pts',(-2.79999999999986,-0.0714659907331545,
0.896148790980443)) ;
#85575 = CARTESIAN_POINT('Ctrl Pts',(-2.79726014197791,-0.143478336976038,
0.89220698203)) ;
#85576 = CARTESIAN_POINT('Ctrl Pts',(-2.79167762249117,-0.215722164093765,
0.88818924661232)) ;
#85577 = CARTESIAN_POINT('Ctrl Pts',(-2.78613441033315,-0.287457311955207,
0.884199800651964)) ;
#85578 = CARTESIAN_POINT('Ctrl Pts',(-2.77778812917749,-0.359420096621492,
0.880135519136715)) ;
#85579 = CARTESIAN_POINT('Ctrl Pts',(-2.76658552138098,-0.431282451398629,
0.8760128923661)) ;
#85580 = CARTESIAN_POINT('Ctrl Pts',(-2.75529981055565,-0.503677894493051,
0.871859683183112)) ;
#85581 = CARTESIAN_POINT('Ctrl Pts',(-2.74111495138177,-0.575970755478099,
0.867647288883408)) ;
#85582 = CARTESIAN_POINT('Ctrl Pts',(-2.72402935956434,-0.647814825571912,
0.863394330842917)) ;
#85583 = CARTESIAN_POINT('Ctrl Pts',(-2.70723196007224,-0.718447061165532,
0.859213109847315)) ;
#85584 = CARTESIAN_POINT('Ctrl Pts',(-2.68763094901295,-0.788644831515286,
0.854992721001645)) ;
#85585 = CARTESIAN_POINT('Ctrl Pts',(-2.66527685062979,-0.858078848064827,
0.850752037009969)) ;
#85586 = CARTESIAN_POINT('Ctrl Pts',(-2.64295407196991,-0.927415582489755,
0.846517294526058)) ;
#85587 = CARTESIAN_POINT('Ctrl Pts',(-2.61788602768933,-0.995990034381983,
0.842262352203043)) ;
#85588 = CARTESIAN_POINT('Ctrl Pts',(-2.59017404345886,-1.06348409700914,
0.838006614131511)) ;
#85589 = CARTESIAN_POINT('Ctrl Pts',(-2.56246019618592,-1.13098269717874,
0.833750589951967)) ;
#85590 = CARTESIAN_POINT('Ctrl Pts',(-2.53210230701669,-1.19740013263799,
0.829493809536051)) ;
#85591 = CARTESIAN_POINT('Ctrl Pts',(-2.49925004240064,-1.2624378105712,0.825255704430077)) ;
#85592 = CARTESIAN_POINT('Ctrl Pts',(-2.46534370721153,-1.32956223361165,
0.820881618991241)) ;
#85593 = CARTESIAN_POINT('Ctrl Pts',(-2.42878055176843,-1.3952161589553,0.816527472731626)) ;
#85594 = CARTESIAN_POINT('Ctrl Pts',(-2.3897735899469,-1.45910321389261,0.812213991563964)) ;
#85595 = CARTESIAN_POINT('Ctrl Pts',(-2.35171346804278,-1.52143949914688,
0.808005214171265)) ;
#85596 = CARTESIAN_POINT('Ctrl Pts',(-2.31132743945051,-1.58209333574035,
0.803835184182287)) ;
#85597 = CARTESIAN_POINT('Ctrl Pts',(-2.2688514193434,-1.64082699787117,0.799721978294092)) ;
#85598 = CARTESIAN_POINT('Ctrl Pts',(-2.22479035473205,-1.70175237825006,
0.795455283110726)) ;
#85599 = CARTESIAN_POINT('Ctrl Pts',(-2.17848089233081,-1.76061095855837,
0.791249777636538)) ;
#85600 = CARTESIAN_POINT('Ctrl Pts',(-2.13021927861688,-1.81718623839399,
0.787123741440374)) ;
#85601 = CARTESIAN_POINT('Ctrl Pts',(-2.08195766490295,-1.87376151822962,
0.78299770524421)) ;
#85602 = CARTESIAN_POINT('Ctrl Pts',(-2.03174466235794,-1.92805331228663,
0.778951165331643)) ;
#85603 = CARTESIAN_POINT('Ctrl Pts',(-1.97989898732219,-1.97989898732237,
0.775000000000004)) ;
#85604 = CARTESIAN_POINT('Ctrl Pts',(-1.92936490065055,-2.03043307399401,
0.771148790980441)) ;
#85605 = CARTESIAN_POINT('Ctrl Pts',(-1.87650711010621,-2.07941612016473,
0.767206982029995)) ;
#85606 = CARTESIAN_POINT('Ctrl Pts',(-1.82147557266717,-2.12655278283339,
0.763189246612312)) ;
#85607 = CARTESIAN_POINT('Ctrl Pts',(-1.76683152025845,-2.17335754942914,
0.759199800651956)) ;
#85608 = CARTESIAN_POINT('Ctrl Pts',(-1.710044435225,-2.21834121045687,0.755135519136708)) ;
#85609 = CARTESIAN_POINT('Ctrl Pts',(-1.65130863691017,-2.26123412889191,
0.751012892366094)) ;
#85610 = CARTESIAN_POINT('Ctrl Pts',(-1.592137125516,-2.30444523497588,0.746859683183106)) ;
#85611 = CARTESIAN_POINT('Ctrl Pts',(-1.53098814317008,-2.34553379709775,
0.742647288883402)) ;
#85612 = CARTESIAN_POINT('Ctrl Pts',(-1.46810537618402,-2.38425388841444,
0.738394330842911)) ;
#85613 = CARTESIAN_POINT('Ctrl Pts',(-1.40628328833823,-2.42232086608588,
0.73421310984731)) ;
#85614 = CARTESIAN_POINT('Ctrl Pts',(-1.34278596106162,-2.45809817768623,
0.72999272100164)) ;
#85615 = CARTESIAN_POINT('Ctrl Pts',(-1.27788196256038,-2.49138870707938,
0.725752037009964)) ;
#85616 = CARTESIAN_POINT('Ctrl Pts',(-1.21306889929785,-2.52463259401125,
0.721517294526053)) ;
#85617 = CARTESIAN_POINT('Ctrl Pts',(-1.14685365524682,-2.55539626985851,
0.717262352203038)) ;
#85618 = CARTESIAN_POINT('Ctrl Pts',(-1.07953281390383,-2.5835264472625,0.713006614131506)) ;
#85619 = CARTESIAN_POINT('Ctrl Pts',(-1.01220744666384,-2.61165851582356,
0.708750589951962)) ;
#85620 = CARTESIAN_POINT('Ctrl Pts',(-0.943776958367505,-2.63715646553174,
0.704493809536046)) ;
#85621 = CARTESIAN_POINT('Ctrl Pts',(-0.874558316180958,-2.65991498954359,
0.700255704430072)) ;
#85622 = CARTESIAN_POINT('Ctrl Pts',(-0.803118781928421,-2.68340372472132,
0.695881618991236)) ;
#85623 = CARTESIAN_POINT('Ctrl Pts',(-0.730840390951022,-2.70397400538794,
0.691527472731622)) ;
#85624 = CARTESIAN_POINT('Ctrl Pts',(-0.65808333395734,-2.72156688794665,
0.68721399156396)) ;
#85625 = CARTESIAN_POINT('Ctrl Pts',(-0.587092353648857,-2.73873272767274,
0.68300521417126)) ;
#85626 = CARTESIAN_POINT('Ctrl Pts',(-0.515646379805832,-2.75306423215018,
0.678835184182282)) ;
#85627 = CARTESIAN_POINT('Ctrl Pts',(-0.444080327173642,-2.76456012107124,
0.674721978294085)) ;
#85628 = CARTESIAN_POINT('Ctrl Pts',(-0.369843699988397,-2.77648499311053,
0.67045528311072)) ;
#85629 = CARTESIAN_POINT('Ctrl Pts',(-0.295478663824374,-2.78535855948053,
0.666249777636534)) ;
#85630 = CARTESIAN_POINT('Ctrl Pts',(-0.22134778547697,-2.7912372091717,0.662123741440371)) ;
#85631 = CARTESIAN_POINT('Ctrl Pts',(-0.147216907129565,-2.79711585886286,
0.657997705244208)) ;
#85632 = CARTESIAN_POINT('Ctrl Pts',(-0.0733208567857782,-2.80000000000004,
0.653951165331642)) ;
#85633 = CARTESIAN_POINT('Ctrl Pts',(1.4166445794217E-13,-2.80000000000004,
0.650000000000004)) ;
#85634 = CARTESIAN_POINT('Ctrl Pts',(0.071465990733294,-2.80000000000004,
0.646148790980441)) ;
#85635 = CARTESIAN_POINT('Ctrl Pts',(0.143478336976213,-2.79726014197808,
0.642206982029997)) ;
#85636 = CARTESIAN_POINT('Ctrl Pts',(0.215722164093974,-2.79167762249134,
0.638189246612314)) ;
#85637 = CARTESIAN_POINT('Ctrl Pts',(0.287457311955519,-2.78613441033331,
0.634199800651952)) ;
#85638 = CARTESIAN_POINT('Ctrl Pts',(0.359420096621906,-2.77778812917764,
0.630135519136698)) ;
#85639 = CARTESIAN_POINT('Ctrl Pts',(0.431282451399145,-2.76658552138109,
0.626012892366077)) ;
#85640 = CARTESIAN_POINT('Ctrl Pts',(0.503677894493549,-2.75529981055575,
0.621859683183089)) ;
#85641 = CARTESIAN_POINT('Ctrl Pts',(0.575970755478578,-2.74111495138187,
0.617647288883386)) ;
#85642 = CARTESIAN_POINT('Ctrl Pts',(0.647814825572372,-2.72402935956444,
0.613394330842896)) ;
#85643 = CARTESIAN_POINT('Ctrl Pts',(0.718447061165981,-2.70723196007232,
0.609213109847295)) ;
#85644 = CARTESIAN_POINT('Ctrl Pts',(0.788644831515725,-2.68763094901303,
0.604992721001625)) ;
#85645 = CARTESIAN_POINT('Ctrl Pts',(0.858078848065254,-2.66527685062987,
0.60075203700995)) ;
#85646 = CARTESIAN_POINT('Ctrl Pts',(0.927415582490178,-2.64295407196998,
0.596517294526039)) ;
#85647 = CARTESIAN_POINT('Ctrl Pts',(0.995990034382399,-2.61788602768939,
0.592262352203023)) ;
#85648 = CARTESIAN_POINT('Ctrl Pts',(1.06348409700955,-2.59017404345891,0.588006614131492)) ;
#85649 = CARTESIAN_POINT('Ctrl Pts',(1.1309826971791,-2.56246019618599,0.583750589951951)) ;
#85650 = CARTESIAN_POINT('Ctrl Pts',(1.19740013263831,-2.53210230701677,0.579493809536038)) ;
#85651 = CARTESIAN_POINT('Ctrl Pts',(1.26243781057147,-2.49925004240073,0.575255704430066)) ;
#85652 = CARTESIAN_POINT('Ctrl Pts',(1.32956223361191,-2.46534370721162,0.570881618991231)) ;
#85653 = CARTESIAN_POINT('Ctrl Pts',(1.39521615895554,-2.42878055176853,0.566527472731617)) ;
#85654 = CARTESIAN_POINT('Ctrl Pts',(1.45910321389283,-2.38977358994701,0.562213991563956)) ;
#85655 = CARTESIAN_POINT('Ctrl Pts',(1.52143949914711,-2.35171346804288,0.558005214171256)) ;
#85656 = CARTESIAN_POINT('Ctrl Pts',(1.58209333574058,-2.31132743945061,0.553835184182279)) ;
#85657 = CARTESIAN_POINT('Ctrl Pts',(1.6408269978714,-2.26885141934349,0.549721978294083)) ;
#85658 = CARTESIAN_POINT('Ctrl Pts',(1.70175237825026,-2.22479035473215,0.545455283110718)) ;
#85659 = CARTESIAN_POINT('Ctrl Pts',(1.76061095855855,-2.17848089233092,0.541249777636533)) ;
#85660 = CARTESIAN_POINT('Ctrl Pts',(1.81718623839415,-2.13021927861701,0.53712374144037)) ;
#85661 = CARTESIAN_POINT('Ctrl Pts',(1.87376151822976,-2.08195766490309,0.532997705244207)) ;
#85662 = CARTESIAN_POINT('Ctrl Pts',(1.92805331228674,-2.0317446623581,0.528951165331642)) ;
#85663 = CARTESIAN_POINT('Ctrl Pts',(1.97989898732247,-1.97989898732237,0.525000000000004)) ;
#85664 = CARTESIAN_POINT('Ctrl Pts',(2.03043307399411,-1.92936490065073,0.521148790980441)) ;
#85665 = CARTESIAN_POINT('Ctrl Pts',(2.07941612016482,-1.87650711010639,0.517206982029996)) ;
#85666 = CARTESIAN_POINT('Ctrl Pts',(2.12655278283348,-1.82147557266736,0.513189246612313)) ;
#85667 = CARTESIAN_POINT('Ctrl Pts',(2.1733575494292,-1.76683152025867,0.509199800651959)) ;
#85668 = CARTESIAN_POINT('Ctrl Pts',(2.21834121045691,-1.71004443522525,0.505135519136713)) ;
#85669 = CARTESIAN_POINT('Ctrl Pts',(2.26123412889194,-1.65130863691045,0.501012892366101)) ;
#85670 = CARTESIAN_POINT('Ctrl Pts',(2.30444523497591,-1.59213712551628,0.496859683183113)) ;
#85671 = CARTESIAN_POINT('Ctrl Pts',(2.34553379709779,-1.53098814317035,0.492647288883409)) ;
#85672 = CARTESIAN_POINT('Ctrl Pts',(2.38425388841448,-1.46810537618429,0.488394330842918)) ;
#85673 = CARTESIAN_POINT('Ctrl Pts',(2.42232086608593,-1.4062832883385,0.484213109847316)) ;
#85674 = CARTESIAN_POINT('Ctrl Pts',(2.45809817768629,-1.34278596106188,0.479992721001646)) ;
#85675 = CARTESIAN_POINT('Ctrl Pts',(2.49138870707944,-1.27788196256063,0.475752037009969)) ;
#85676 = CARTESIAN_POINT('Ctrl Pts',(2.52463259401131,-1.21306889929811,0.471517294526058)) ;
#85677 = CARTESIAN_POINT('Ctrl Pts',(2.55539626985857,-1.14685365524709,0.467262352203043)) ;
#85678 = CARTESIAN_POINT('Ctrl Pts',(2.58352644726256,-1.0795328139041,0.463006614131512)) ;
#85679 = CARTESIAN_POINT('Ctrl Pts',(2.61165851582361,-1.01220744666414,0.458750589951969)) ;
#85680 = CARTESIAN_POINT('Ctrl Pts',(2.63715646553179,-0.943776958367838,
0.454493809536056)) ;
#85681 = CARTESIAN_POINT('Ctrl Pts',(2.65991498954363,-0.874558316181326,
0.450255704430083)) ;
#85682 = CARTESIAN_POINT('Ctrl Pts',(2.68340372472137,-0.803118781928774,
0.445881618991247)) ;
#85683 = CARTESIAN_POINT('Ctrl Pts',(2.70397400538799,-0.730840390951359,
0.441527472731631)) ;
#85684 = CARTESIAN_POINT('Ctrl Pts',(2.72156688794672,-0.658083333957661,
0.437213991563969)) ;
#85685 = CARTESIAN_POINT('Ctrl Pts',(2.73873272767281,-0.587092353649187,
0.433005214171268)) ;
#85686 = CARTESIAN_POINT('Ctrl Pts',(2.75306423215025,-0.51564637980617,0.428835184182291)) ;
#85687 = CARTESIAN_POINT('Ctrl Pts',(2.76456012107132,-0.444080327173988,
0.424721978294095)) ;
#85688 = CARTESIAN_POINT('Ctrl Pts',(2.77648499311062,-0.369843699988715,
0.420455283110728)) ;
#85689 = CARTESIAN_POINT('Ctrl Pts',(2.78535855948062,-0.295478663824664,
0.41624977763654)) ;
#85690 = CARTESIAN_POINT('Ctrl Pts',(2.79123720917179,-0.221347785477232,
0.412123741440376)) ;
#85691 = CARTESIAN_POINT('Ctrl Pts',(2.79711585886296,-0.147216907129799,
0.407997705244211)) ;
#85692 = CARTESIAN_POINT('Ctrl Pts',(2.80000000000014,-0.0733208567859839,
0.403951165331644)) ;
#85693 = CARTESIAN_POINT('Ctrl Pts',(2.80000000000014,-3.59712259978551E-14,
0.400000000000004)) ;
#85694 = CARTESIAN_POINT('Ctrl Pts',(2.80000000000014,0.0714659907331161,
0.396148790980441)) ;
#85695 = CARTESIAN_POINT('Ctrl Pts',(2.79726014197818,0.143478336976034,0.392206982029997)) ;
#85696 = CARTESIAN_POINT('Ctrl Pts',(2.79167762249144,0.215722164093794,0.388189246612314)) ;
#85697 = CARTESIAN_POINT('Ctrl Pts',(2.78613441033342,0.28745731195519,0.384199800651961)) ;
#85698 = CARTESIAN_POINT('Ctrl Pts',(2.77778812917777,0.359420096621429,0.380135519136715)) ;
#85699 = CARTESIAN_POINT('Ctrl Pts',(2.76658552138126,0.431282451398519,0.376012892366102)) ;
#85700 = CARTESIAN_POINT('Ctrl Pts',(2.75529981055593,0.503677894492942,0.371859683183114)) ;
#85701 = CARTESIAN_POINT('Ctrl Pts',(2.74111495138205,0.57597075547799,0.36764728888341)) ;
#85702 = CARTESIAN_POINT('Ctrl Pts',(2.72402935956463,0.647814825571804,0.363394330842919)) ;
#85703 = CARTESIAN_POINT('Ctrl Pts',(2.70723196007253,0.718447061165415,0.359213109847317)) ;
#85704 = CARTESIAN_POINT('Ctrl Pts',(2.68763094901325,0.78864483151516,0.354992721001648)) ;
#85705 = CARTESIAN_POINT('Ctrl Pts',(2.66527685063009,0.858078848064691,0.350752037009972)) ;
#85706 = CARTESIAN_POINT('Ctrl Pts',(2.64295407197021,0.927415582489618,0.346517294526062)) ;
#85707 = CARTESIAN_POINT('Ctrl Pts',(2.61788602768963,0.995990034381844,0.342262352203046)) ;
#85708 = CARTESIAN_POINT('Ctrl Pts',(2.59017404345916,1.063484097009,0.338006614131515)) ;
#85709 = CARTESIAN_POINT('Ctrl Pts',(2.56246019618623,1.1309826971786,0.333750589951971)) ;
#85710 = CARTESIAN_POINT('Ctrl Pts',(2.532102307017,1.19740013263786,0.329493809536055)) ;
#85711 = CARTESIAN_POINT('Ctrl Pts',(2.49925004240094,1.26243781057107,0.32525570443008)) ;
#85712 = CARTESIAN_POINT('Ctrl Pts',(2.46534370721183,1.32956223361153,0.320881618991244)) ;
#85713 = CARTESIAN_POINT('Ctrl Pts',(2.42878055176873,1.39521615895518,0.316527472731628)) ;
#85714 = CARTESIAN_POINT('Ctrl Pts',(2.3897735899472,1.45910321389249,0.312213991563967)) ;
#85715 = CARTESIAN_POINT('Ctrl Pts',(2.35171346804307,1.52143949914679,0.308005214171265)) ;
#85716 = CARTESIAN_POINT('Ctrl Pts',(2.31132743945079,1.58209333574028,0.303835184182287)) ;
#85717 = CARTESIAN_POINT('Ctrl Pts',(2.26885141934366,1.64082699787112,0.29972197829409)) ;
#85718 = CARTESIAN_POINT('Ctrl Pts',(2.22479035473232,1.70175237825,0.295455283110724)) ;
#85719 = CARTESIAN_POINT('Ctrl Pts',(2.17848089233108,1.76061095855831,0.291249777636537)) ;
#85720 = CARTESIAN_POINT('Ctrl Pts',(2.13021927861715,1.81718623839393,0.287123741440373)) ;
#85721 = CARTESIAN_POINT('Ctrl Pts',(2.08195766490322,1.87376151822955,0.282997705244209)) ;
#85722 = CARTESIAN_POINT('Ctrl Pts',(2.03174466235821,1.92805331228655,0.278951165331643)) ;
#85723 = CARTESIAN_POINT('Ctrl Pts',(1.97989898732247,1.97989898732229,0.275000000000004)) ;
#85724 = CARTESIAN_POINT('Ctrl Pts',(1.92934672113032,2.03045125351443,0.271147405516926)) ;
#85725 = CARTESIAN_POINT('Ctrl Pts',(1.87646907589625,2.07945136207899,0.267204145766144)) ;
#85726 = CARTESIAN_POINT('Ctrl Pts',(1.82141617942112,2.12660365403224,0.263184910469907)) ;
#85727 = CARTESIAN_POINT('Ctrl Pts',(1.76514929586526,2.17479571458848,0.259077045872825)) ;
#85728 = CARTESIAN_POINT('Ctrl Pts',(1.7066101530828,2.22105676270134,0.254889835146308)) ;
#85729 = CARTESIAN_POINT('Ctrl Pts',(1.64601164123507,2.26509286275836,0.250641311726231)) ;
#85730 = CARTESIAN_POINT('Ctrl Pts',(1.58754824217552,2.30757740589581,0.246542479716199)) ;
#85731 = CARTESIAN_POINT('Ctrl Pts',(1.5271686178725,2.34799057449375,0.24238662086617)) ;
#85732 = CARTESIAN_POINT('Ctrl Pts',(1.46510735126145,2.38609732602839,0.238191623029449)) ;
#85733 = CARTESIAN_POINT('Ctrl Pts',(1.40323139666294,2.42409029260176,0.234009151258246)) ;
#85734 = CARTESIAN_POINT('Ctrl Pts',(1.33968428229124,2.45979009971844,0.229787809461762)) ;
#85735 = CARTESIAN_POINT('Ctrl Pts',(1.27473511126994,2.49300028000314,0.225546484688788)) ;
#85736 = CARTESIAN_POINT('Ctrl Pts',(1.20988456109896,2.5261600329126,0.221311600075851)) ;
#85737 = CARTESIAN_POINT('Ctrl Pts',(1.14363676230229,2.55683732461154,0.217056831637654)) ;
#85738 = CARTESIAN_POINT('Ctrl Pts',(1.07628859269765,2.58487966165332,0.21280158160412)) ;
#85739 = CARTESIAN_POINT('Ctrl Pts',(1.00894375102516,2.61292061301535,0.208546541838861)) ;
#85740 = CARTESIAN_POINT('Ctrl Pts',(0.940499272947081,2.63832660736102,0.204291060106912)) ;
#85741 = CARTESIAN_POINT('Ctrl Pts',(0.871272148091887,2.66099320629711,0.200054549780001)) ;
#85742 = CARTESIAN_POINT('Ctrl Pts',(0.801822366682255,2.68373270825829,0.19580441348214)) ;
#85743 = CARTESIAN_POINT('Ctrl Pts',(0.731585564361363,2.7037150260078,0.19157340994441)) ;
#85744 = CARTESIAN_POINT('Ctrl Pts',(0.660892332187115,2.72088612868239,0.187380560333748)) ;
#85745 = CARTESIAN_POINT('Ctrl Pts',(0.590011263043028,2.73810285620388,0.183176570022037)) ;
#85746 = CARTESIAN_POINT('Ctrl Pts',(0.518672017063942,2.75249343444436,0.179010972847647)) ;
#85747 = CARTESIAN_POINT('Ctrl Pts',(0.447208193245961,2.76405586627579,0.17490179060408)) ;
#85748 = CARTESIAN_POINT('Ctrl Pts',(0.375298345274736,2.77569046222595,0.170766961894471)) ;
#85749 = CARTESIAN_POINT('Ctrl Pts',(0.303263024046943,2.78446165095677,0.166689286934451)) ;
#85750 = CARTESIAN_POINT('Ctrl Pts',(0.231432282248643,2.79041916183448,0.162685441802253)) ;
#85751 = CARTESIAN_POINT('Ctrl Pts',(0.212884643984362,2.7919574691657,0.161651596552725)) ;
#85752 = CARTESIAN_POINT('Ctrl Pts',(0.194350566384982,2.79330843635713,0.16062266376929)) ;
#85753 = CARTESIAN_POINT('Ctrl Pts',(0.175835544859223,2.79447344971533,0.15959890864801)) ;
#85754 = CARTESIAN_POINT('Ctrl Pts',(1.4210854715202E-13,1.69999999999996,
1.15)) ;
#85755 = CARTESIAN_POINT('Ctrl Pts',(-0.0491344664214032,1.69999999999996,
1.14563893032299)) ;
#85756 = CARTESIAN_POINT('Ctrl Pts',(-0.0986947229193856,1.69786604855678,
1.14116161433639)) ;
#85757 = CARTESIAN_POINT('Ctrl Pts',(-0.197622412403077,1.68919704412233,
1.13206229175992)) ;
#85758 = CARTESIAN_POINT('Ctrl Pts',(-0.246986299885041,1.68270496892852,
1.12744217992741)) ;
#85759 = CARTESIAN_POINT('Ctrl Pts',(-0.345200900950269,1.66532644813156,
1.11808594673948)) ;
#85760 = CARTESIAN_POINT('Ctrl Pts',(-0.394052183981859,1.65445972537225,
1.1133504999456)) ;
#85761 = CARTESIAN_POINT('Ctrl Pts',(-0.490749173516077,1.62839369436624,
1.10380957293898)) ;
#85762 = CARTESIAN_POINT('Ctrl Pts',(-0.538596442256585,1.61320599162947,
1.09900438073851)) ;
#85763 = CARTESIAN_POINT('Ctrl Pts',(-0.632803924485224,1.57863065558518,
1.08937157495477)) ;
#85764 = CARTESIAN_POINT('Ctrl Pts',(-0.679164591102349,1.55924670054701,
1.08454405638323)) ;
#85765 = CARTESIAN_POINT('Ctrl Pts',(-0.770056551850408,1.51642527652522,
1.07490236416373)) ;
#85766 = CARTESIAN_POINT('Ctrl Pts',(-0.814580080103976,1.49297402286675,
1.07008837300884)) ;
#85767 = CARTESIAN_POINT('Ctrl Pts',(-0.901240725533071,1.4423213594285,1.06053433003248)) ;
#85768 = CARTESIAN_POINT('Ctrl Pts',(-0.943370504022189,1.41511051821574,
1.05579458283318)) ;
#85769 = CARTESIAN_POINT('Ctrl Pts',(-1.02504405883689,1.35713483654882,1.04641395469392)) ;
#85770 = CARTESIAN_POINT('Ctrl Pts',(-1.06456093267498,1.32634106753781,1.04177439801107)) ;
#85771 = CARTESIAN_POINT('Ctrl Pts',(-1.13706958910421,1.26457389613212,1.03306783355715)) ;
#85772 = CARTESIAN_POINT('Ctrl Pts',(-1.17033107781674,1.23383197821735,1.02898539770902)) ;
#85773 = CARTESIAN_POINT('Ctrl Pts',(-1.23682484241365,1.16733821362043,1.02063893032299)) ;
#85774 = CARTESIAN_POINT('Ctrl Pts',(-1.27036030432452,1.13078488863717,1.01616161433639)) ;
#85775 = CARTESIAN_POINT('Ctrl Pts',(-1.33418283258382,1.0547025367344,1.00706229175992)) ;
#85776 = CARTESIAN_POINT('Ctrl Pts',(-1.36449778177453,1.01520640675666,1.00244217992741)) ;
#85777 = CARTESIAN_POINT('Ctrl Pts',(-1.42165752229676,0.933469726429385,
0.993085946739478)) ;
#85778 = CARTESIAN_POINT('Ctrl Pts',(-1.44851666244568,0.891242719575706,
0.9883504999456)) ;
#85779 = CARTESIAN_POINT('Ctrl Pts',(-1.49846029218269,0.804436155272762,
0.978809572938975)) ;
#85780 = CARTESIAN_POINT('Ctrl Pts',(-1.52155409277454,0.759863699489269,
0.974004380738511)) ;
#85781 = CARTESIAN_POINT('Ctrl Pts',(-1.56372038771819,0.668800495388183,
0.964371574954774)) ;
#85782 = CARTESIAN_POINT('Ctrl Pts',(-1.58279580340978,0.622312027589206,
0.959544056383236)) ;
#85783 = CARTESIAN_POINT('Ctrl Pts',(-1.61678680590419,0.527762386483063,
0.949902364163737)) ;
#85784 = CARTESIAN_POINT('Ctrl Pts',(-1.63168715416542,0.479696957243388,
0.94508837300885)) ;
#85785 = CARTESIAN_POINT('Ctrl Pts',(-1.65714864240798,0.382601785396132,
0.935534330032484)) ;
#85786 = CARTESIAN_POINT('Ctrl Pts',(-1.66769792412419,0.333570562993271,
0.930794582833185)) ;
#85787 = CARTESIAN_POINT('Ctrl Pts',(-1.68445485092669,0.2348236408896,0.921413954693928)) ;
#85788 = CARTESIAN_POINT('Ctrl Pts',(-1.69062301750293,0.185106508541409,
0.916774398011078)) ;
#85789 = CARTESIAN_POINT('Ctrl Pts',(-1.69821839440309,0.0901591601298727,
0.908067833557157)) ;
#85790 = CARTESIAN_POINT('Ctrl Pts',(-1.69999999999986,0.0449019172846421,
0.903985397709019)) ;
#85791 = CARTESIAN_POINT('Ctrl Pts',(-1.69999999999986,-0.0491344664215853,
0.895638930322986)) ;
#85792 = CARTESIAN_POINT('Ctrl Pts',(-1.69786604855668,-0.0986947229195726,
0.891161614336394)) ;
#85793 = CARTESIAN_POINT('Ctrl Pts',(-1.68919704412223,-0.19762241240327,
0.882062291759915)) ;
#85794 = CARTESIAN_POINT('Ctrl Pts',(-1.68270496892842,-0.246986299885236,
0.877442179927406)) ;
#85795 = CARTESIAN_POINT('Ctrl Pts',(-1.66532644813145,-0.34520090095047,
0.868085946739475)) ;
#85796 = CARTESIAN_POINT('Ctrl Pts',(-1.65445972537215,-0.394052183982064,
0.863350499945597)) ;
#85797 = CARTESIAN_POINT('Ctrl Pts',(-1.62839369436614,-0.490749173516282,
0.853809572938973)) ;
#85798 = CARTESIAN_POINT('Ctrl Pts',(-1.61320599162936,-0.538596442256787,
0.849004380738509)) ;
#85799 = CARTESIAN_POINT('Ctrl Pts',(-1.57863065558508,-0.632803924485399,
0.839371574954773)) ;
#85800 = CARTESIAN_POINT('Ctrl Pts',(-1.55924670054692,-0.679164591102501,
0.834544056383236)) ;
#85801 = CARTESIAN_POINT('Ctrl Pts',(-1.51642527652514,-0.770056551850542,
0.824902364163736)) ;
#85802 = CARTESIAN_POINT('Ctrl Pts',(-1.49297402286668,-0.814580080104112,
0.820088373008848)) ;
#85803 = CARTESIAN_POINT('Ctrl Pts',(-1.44232135942842,-0.901240725533217,
0.810534330032481)) ;
#85804 = CARTESIAN_POINT('Ctrl Pts',(-1.41511051821566,-0.94337050402234,
0.805794582833179)) ;
#85805 = CARTESIAN_POINT('Ctrl Pts',(-1.35713483654874,-1.02504405883705,
0.796413954693922)) ;
#85806 = CARTESIAN_POINT('Ctrl Pts',(-1.32634106753772,-1.06456093267515,
0.791774398011072)) ;
#85807 = CARTESIAN_POINT('Ctrl Pts',(-1.26457389613203,-1.13706958910438,
0.783067833557153)) ;
#85808 = CARTESIAN_POINT('Ctrl Pts',(-1.23383197821725,-1.17033107781691,
0.778985397709017)) ;
#85809 = CARTESIAN_POINT('Ctrl Pts',(-1.16733821362031,-1.23682484241385,
0.770638930322983)) ;
#85810 = CARTESIAN_POINT('Ctrl Pts',(-1.13078488863702,-1.27036030432474,
0.766161614336389)) ;
#85811 = CARTESIAN_POINT('Ctrl Pts',(-1.05470253673422,-1.33418283258406,
0.757062291759907)) ;
#85812 = CARTESIAN_POINT('Ctrl Pts',(-1.01520640675647,-1.36449778177477,
0.752442179927397)) ;
#85813 = CARTESIAN_POINT('Ctrl Pts',(-0.933469726429203,-1.42165752229699,
0.74308594673947)) ;
#85814 = CARTESIAN_POINT('Ctrl Pts',(-0.891242719575537,-1.4485166624459,
0.738350499945593)) ;
#85815 = CARTESIAN_POINT('Ctrl Pts',(-0.804436155272612,-1.49846029218289,
0.72880957293897)) ;
#85816 = CARTESIAN_POINT('Ctrl Pts',(-0.759863699489124,-1.52155409277474,
0.724004380738507)) ;
#85817 = CARTESIAN_POINT('Ctrl Pts',(-0.668800495388052,-1.56372038771838,
0.714371574954771)) ;
#85818 = CARTESIAN_POINT('Ctrl Pts',(-0.622312027589085,-1.58279580340996,
0.709544056383234)) ;
#85819 = CARTESIAN_POINT('Ctrl Pts',(-0.527762386482951,-1.61678680590438,
0.699902364163737)) ;
#85820 = CARTESIAN_POINT('Ctrl Pts',(-0.479696957243274,-1.6316871541656,
0.695088373008849)) ;
#85821 = CARTESIAN_POINT('Ctrl Pts',(-0.382601785395997,-1.65714864240817,
0.685534330032481)) ;
#85822 = CARTESIAN_POINT('Ctrl Pts',(-0.333570562993116,-1.66769792412438,
0.68079458283318)) ;
#85823 = CARTESIAN_POINT('Ctrl Pts',(-0.234823640889432,-1.68445485092688,
0.671413954693923)) ;
#85824 = CARTESIAN_POINT('Ctrl Pts',(-0.185106508541249,-1.69062301750311,
0.666774398011073)) ;
#85825 = CARTESIAN_POINT('Ctrl Pts',(-0.0901591601297333,-1.69821839440327,
0.658067833557153)) ;
#85826 = CARTESIAN_POINT('Ctrl Pts',(-0.0449019172845196,-1.70000000000004,
0.653985397709018)) ;
#85827 = CARTESIAN_POINT('Ctrl Pts',(0.0491344664216406,-1.70000000000004,
0.645638930322991)) ;
#85828 = CARTESIAN_POINT('Ctrl Pts',(0.098694722919575,-1.69786604855686,
0.641161614336403)) ;
#85829 = CARTESIAN_POINT('Ctrl Pts',(0.197622412403214,-1.68919704412242,
0.63206229175993)) ;
#85830 = CARTESIAN_POINT('Ctrl Pts',(0.246986299885175,-1.68270496892862,
0.627442179927422)) ;
#85831 = CARTESIAN_POINT('Ctrl Pts',(0.345200900950416,-1.66532644813167,
0.618085946739491)) ;
#85832 = CARTESIAN_POINT('Ctrl Pts',(0.394052183982023,-1.65445972537236,
0.613350499945611)) ;
#85833 = CARTESIAN_POINT('Ctrl Pts',(0.490749173516293,-1.62839369436635,
0.603809572938982)) ;
#85834 = CARTESIAN_POINT('Ctrl Pts',(0.538596442256835,-1.61320599162956,
0.599004380738515)) ;
#85835 = CARTESIAN_POINT('Ctrl Pts',(0.632803924485532,-1.57863065558525,
0.58937157495477)) ;
#85836 = CARTESIAN_POINT('Ctrl Pts',(0.67916459110268,-1.55924670054707,0.584544056383228)) ;
#85837 = CARTESIAN_POINT('Ctrl Pts',(0.770056551850753,-1.51642527652527,
0.574902364163725)) ;
#85838 = CARTESIAN_POINT('Ctrl Pts',(0.814580080104313,-1.4929740228668,0.570088373008839)) ;
#85839 = CARTESIAN_POINT('Ctrl Pts',(0.901240725533383,-1.44232135942856,
0.560534330032474)) ;
#85840 = CARTESIAN_POINT('Ctrl Pts',(0.943370504022482,-1.41511051821581,
0.555794582833176)) ;
#85841 = CARTESIAN_POINT('Ctrl Pts',(1.02504405883715,-1.35713483654892,0.546413954693923)) ;
#85842 = CARTESIAN_POINT('Ctrl Pts',(1.06456093267523,-1.32634106753792,0.541774398011074)) ;
#85843 = CARTESIAN_POINT('Ctrl Pts',(1.13706958910446,-1.26457389613223,0.533067833557155)) ;
#85844 = CARTESIAN_POINT('Ctrl Pts',(1.170331077817,-1.23383197821744,0.528985397709019)) ;
#85845 = CARTESIAN_POINT('Ctrl Pts',(1.23682484241396,-1.16733821362048,0.520638930322983)) ;
#85846 = CARTESIAN_POINT('Ctrl Pts',(1.27036030432486,-1.13078488863718,0.516161614336386)) ;
#85847 = CARTESIAN_POINT('Ctrl Pts',(1.33418283258419,-1.05470253673437,0.507062291759903)) ;
#85848 = CARTESIAN_POINT('Ctrl Pts',(1.36449778177489,-1.01520640675662,0.502442179927395)) ;
#85849 = CARTESIAN_POINT('Ctrl Pts',(1.42165752229712,-0.933469726429342,
0.493085946739464)) ;
#85850 = CARTESIAN_POINT('Ctrl Pts',(1.44851666244603,-0.891242719575662,
0.488350499945587)) ;
#85851 = CARTESIAN_POINT('Ctrl Pts',(1.49846029218302,-0.804436155272731,
0.478809572938964)) ;
#85852 = CARTESIAN_POINT('Ctrl Pts',(1.52155409277486,-0.75986369948925,0.474004380738501)) ;
#85853 = CARTESIAN_POINT('Ctrl Pts',(1.5637203877185,-0.66880049538819,0.464371574954767)) ;
#85854 = CARTESIAN_POINT('Ctrl Pts',(1.58279580341008,-0.622312027589227,
0.459544056383231)) ;
#85855 = CARTESIAN_POINT('Ctrl Pts',(1.61678680590449,-0.527762386483097,
0.449902364163734)) ;
#85856 = CARTESIAN_POINT('Ctrl Pts',(1.63168715416571,-0.479696957243424,
0.445088373008846)) ;
#85857 = CARTESIAN_POINT('Ctrl Pts',(1.65714864240828,-0.382601785396136,
0.435534330032477)) ;
#85858 = CARTESIAN_POINT('Ctrl Pts',(1.66769792412449,-0.333570562993245,
0.430794582833176)) ;
#85859 = CARTESIAN_POINT('Ctrl Pts',(1.68445485092699,-0.234823640889562,
0.421413954693918)) ;
#85860 = CARTESIAN_POINT('Ctrl Pts',(1.69062301750322,-0.185106508541393,
0.41677439801107)) ;
#85861 = CARTESIAN_POINT('Ctrl Pts',(1.69821839440337,-0.0901591601298977,
0.408067833557153)) ;
#85862 = CARTESIAN_POINT('Ctrl Pts',(1.70000000000014,-0.0449019172846905,
0.403985397709017)) ;
#85863 = CARTESIAN_POINT('Ctrl Pts',(1.70000000000014,0.0491344664214081,
0.395638930322996)) ;
#85864 = CARTESIAN_POINT('Ctrl Pts',(1.69786604855697,0.0986947229192886,
0.391161614336413)) ;
#85865 = CARTESIAN_POINT('Ctrl Pts',(1.68919704412254,0.197622412402883,0.382062291759944)) ;
#85866 = CARTESIAN_POINT('Ctrl Pts',(1.68270496892874,0.246986299884855,0.377442179927436)) ;
#85867 = CARTESIAN_POINT('Ctrl Pts',(1.6653264481318,0.345200900950092,0.368085946739505)) ;
#85868 = CARTESIAN_POINT('Ctrl Pts',(1.6544597253725,0.39405218398168,0.363350499945627)) ;
#85869 = CARTESIAN_POINT('Ctrl Pts',(1.62839369436652,0.490749173515883,0.353809572939006)) ;
#85870 = CARTESIAN_POINT('Ctrl Pts',(1.61320599162975,0.538596442256374,0.349004380738543)) ;
#85871 = CARTESIAN_POINT('Ctrl Pts',(1.5786306555855,0.632803924484977,0.339371574954809)) ;
#85872 = CARTESIAN_POINT('Ctrl Pts',(1.55924670054735,0.679164591102084,0.334544056383272)) ;
#85873 = CARTESIAN_POINT('Ctrl Pts',(1.5164252765256,0.770056551850128,0.324902364163773)) ;
#85874 = CARTESIAN_POINT('Ctrl Pts',(1.49297402286714,0.8145800801037,0.320088373008886)) ;
#85875 = CARTESIAN_POINT('Ctrl Pts',(1.44232135942892,0.901240725532785,0.310534330032521)) ;
#85876 = CARTESIAN_POINT('Ctrl Pts',(1.41511051821619,0.943370504021889,0.305794582833223)) ;
#85877 = CARTESIAN_POINT('Ctrl Pts',(1.35713483654931,1.02504405883658,0.296413954693968)) ;
#85878 = CARTESIAN_POINT('Ctrl Pts',(1.32634106753831,1.06456093267469,0.291774398011117)) ;
#85879 = CARTESIAN_POINT('Ctrl Pts',(1.26457389613253,1.13706958910406,0.283067833557182)) ;
#85880 = CARTESIAN_POINT('Ctrl Pts',(1.23383197821764,1.17033107781672,0.278985397709031)) ;
#85881 = CARTESIAN_POINT('Ctrl Pts',(1.16687638181328,1.23728667422108,0.270580960013422)) ;
#85882 = CARTESIAN_POINT('Ctrl Pts',(1.12981271916814,1.27125155805816,0.266042558666344)) ;
#85883 = CARTESIAN_POINT('Ctrl Pts',(1.05312491055298,1.33542920601837,0.256876436955199)) ;
#85884 = CARTESIAN_POINT('Ctrl Pts',(1.01357775753582,1.36570865657345,0.252253098649823)) ;
#85885 = CARTESIAN_POINT('Ctrl Pts',(0.931748953624498,1.42278628521131,0.242891701206208)) ;
#85886 = CARTESIAN_POINT('Ctrl Pts',(0.88948121648888,1.44959928904487,0.238154331961916)) ;
#85887 = CARTESIAN_POINT('Ctrl Pts',(0.802605102103923,1.49944189580254,0.228610939181518)) ;
#85888 = CARTESIAN_POINT('Ctrl Pts',(0.758004130384641,1.5224813065182,0.223805212363041)) ;
#85889 = CARTESIAN_POINT('Ctrl Pts',(0.664522073922145,1.56562908564902,0.213921625026436)) ;
#85890 = CARTESIAN_POINT('Ctrl Pts',(0.615539322328646,1.58552627802381,0.208842504663212)) ;
#85891 = CARTESIAN_POINT('Ctrl Pts',(0.518395366613399,1.61981274547806,0.198959682063373)) ;
#85892 = CARTESIAN_POINT('Ctrl Pts',(0.470304511490864,1.63441700888879,0.194154319763053)) ;
#85893 = CARTESIAN_POINT('Ctrl Pts',(0.373202345586565,1.65928853338962,0.184621349139331)) ;
#85894 = CARTESIAN_POINT('Ctrl Pts',(0.324189726756498,1.66954434240007,0.179894045756642)) ;
#85895 = CARTESIAN_POINT('Ctrl Pts',(0.225636251909037,1.68570400886284,0.170552555999424)) ;
#85896 = CARTESIAN_POINT('Ctrl Pts',(0.176094787103018,1.69157920510122,0.165939369337106)) ;
#85897 = CARTESIAN_POINT('Ctrl Pts',(0.120082623975991,1.69576670628109,0.16081390877527)) ;
#85898 = CARTESIAN_POINT('Ctrl Pts',(0.113425528473636,1.69622494453036,0.160206193633126)) ;
#85899 = CARTESIAN_POINT('Ctrl Pts',(0.106818383502283,1.69664075012557,0.159604472052141)) ;
#85900 = CARTESIAN_POINT('Ctrl Pts',(0.10676868707791,1.69664387765666,0.159599946131918)) ;
#85901 = CARTESIAN_POINT('Origin',(1.41383259008656E-13,-3.66373598126302E-14,
0.700000000000004)) ;
#85902 = CARTESIAN_POINT('Ctrl Pts',(1.4210854715202E-13,2.79999999999996,
0.250000000000004)) ;
#85903 = CARTESIAN_POINT('Ctrl Pts',(-0.0714659907350962,2.79999999999996,
0.246148790980329)) ;
#85904 = CARTESIAN_POINT('Ctrl Pts',(-0.143478336980131,2.79726014197784,
0.242206982029767)) ;
#85905 = CARTESIAN_POINT('Ctrl Pts',(-0.215722164100012,2.79167762249077,
0.238189246611963)) ;
#85906 = CARTESIAN_POINT('Ctrl Pts',(-0.287457311956658,2.78613441033296,
0.23419980065187)) ;
#85907 = CARTESIAN_POINT('Ctrl Pts',(-0.359420096618108,2.77778812917788,
0.230135519136895)) ;
#85908 = CARTESIAN_POINT('Ctrl Pts',(-0.431282451390436,2.76658552138233,
0.22601289236656)) ;
#85909 = CARTESIAN_POINT('Ctrl Pts',(-0.5036778944852,2.75529981055716,0.221859683183557)) ;
#85910 = CARTESIAN_POINT('Ctrl Pts',(-0.575970755470603,2.74111495138341,
0.217647288883837)) ;
#85911 = CARTESIAN_POINT('Ctrl Pts',(-0.647814825564774,2.7240293595661,0.213394330843329)) ;
#85912 = CARTESIAN_POINT('Ctrl Pts',(-0.718447061158909,2.70723196007406,
0.209213109847701)) ;
#85913 = CARTESIAN_POINT('Ctrl Pts',(-0.788644831509182,2.6876309490148,0.204992721002004)) ;
#85914 = CARTESIAN_POINT('Ctrl Pts',(-0.858078848059242,2.66527685063163,
0.200752037010299)) ;
#85915 = CARTESIAN_POINT('Ctrl Pts',(-0.927415582479881,2.64295407197328,
0.196517294526654)) ;
#85916 = CARTESIAN_POINT('Ctrl Pts',(-0.995990034367923,2.61788602769458,
0.192262352203906)) ;
#85917 = CARTESIAN_POINT('Ctrl Pts',(-1.06348409699106,2.59017404346631,0.18800661413264)) ;
#85918 = CARTESIAN_POINT('Ctrl Pts',(-1.13098269716956,2.56246019619026,0.183750589952547)) ;
#85919 = CARTESIAN_POINT('Ctrl Pts',(-1.19740013263746,2.53210230701722,0.17949380953608)) ;
#85920 = CARTESIAN_POINT('Ctrl Pts',(-1.26243781057895,2.49925004239673,0.175255704429561)) ;
#85921 = CARTESIAN_POINT('Ctrl Pts',(-1.32956223361862,2.46534370720774,0.17088161899077)) ;
#85922 = CARTESIAN_POINT('Ctrl Pts',(-1.39521615896152,2.42878055176483,0.166527472731199)) ;
#85923 = CARTESIAN_POINT('Ctrl Pts',(-1.45910321389809,2.38977358994354,0.162213991563582)) ;
#85924 = CARTESIAN_POINT('Ctrl Pts',(-1.5214394991492,2.35171346804115,0.158005214171092)) ;
#85925 = CARTESIAN_POINT('Ctrl Pts',(-1.58209333573967,2.31132743945085,0.15383518418232)) ;
#85926 = CARTESIAN_POINT('Ctrl Pts',(-1.64082699786767,2.2688514193459,0.149721978294324)) ;
#85927 = CARTESIAN_POINT('Ctrl Pts',(-1.70175237824719,2.22479035473423,0.145455283110917)) ;
#85928 = CARTESIAN_POINT('Ctrl Pts',(-1.76061095855609,2.17848089233263,0.14124977763669)) ;
#85929 = CARTESIAN_POINT('Ctrl Pts',(-1.81718623839227,2.1302192786183,0.137123741440487)) ;
#85930 = CARTESIAN_POINT('Ctrl Pts',(-1.87376151822845,2.08195766490396,0.132997705244284)) ;
#85931 = CARTESIAN_POINT('Ctrl Pts',(-1.92805331228597,2.03174466235851,0.128951165331679)) ;
#85932 = CARTESIAN_POINT('Ctrl Pts',(-1.97989898732219,1.97989898732229,0.125000000000004)) ;
#85933 = CARTESIAN_POINT('Ctrl Pts',(-2.03043307399602,1.92936490064846,0.121148790980274)) ;
#85934 = CARTESIAN_POINT('Ctrl Pts',(-2.0794161201688,1.87650711010172,0.117206982029653)) ;
#85935 = CARTESIAN_POINT('Ctrl Pts',(-2.12655278283934,1.82147557266011,0.113189246611789)) ;
#85936 = CARTESIAN_POINT('Ctrl Pts',(-2.17335754943038,1.76683152025651,0.109199800651814)) ;
#85937 = CARTESIAN_POINT('Ctrl Pts',(-2.21834121045375,1.71004443522861,0.105135519136963)) ;
#85938 = CARTESIAN_POINT('Ctrl Pts',(-2.26123412888485,1.6513086369197,0.101012892366755)) ;
#85939 = CARTESIAN_POINT('Ctrl Pts',(-2.30444523496933,1.59213712552534,0.0968596831837452)) ;
#85940 = CARTESIAN_POINT('Ctrl Pts',(-2.3455337970917,1.53098814317919,0.0926472888840185)) ;
#85941 = CARTESIAN_POINT('Ctrl Pts',(-2.38425388840886,1.46810537619287,0.0883943308435033)) ;
#85942 = CARTESIAN_POINT('Ctrl Pts',(-2.42232086608197,1.4062832883449,0.0842131098477466)) ;
#85943 = CARTESIAN_POINT('Ctrl Pts',(-2.45809817768381,1.34278596106596,0.0799927210019183)) ;
#85944 = CARTESIAN_POINT('Ctrl Pts',(-2.49138870707828,1.27788196256228,0.0757520370100814)) ;
#85945 = CARTESIAN_POINT('Ctrl Pts',(-2.52463259401001,1.21306889930012,0.0715172945261934)) ;
#85946 = CARTESIAN_POINT('Ctrl Pts',(-2.55539626985716,1.14685365524949,0.0672623522032017)) ;
#85947 = CARTESIAN_POINT('Ctrl Pts',(-2.58352644726108,1.07953281390689,0.0630066141316928)) ;
#85948 = CARTESIAN_POINT('Ctrl Pts',(-2.61165851582251,1.01220744666622,0.0587505899521033)) ;
#85949 = CARTESIAN_POINT('Ctrl Pts',(-2.63715646553102,0.943776958369179,
0.0544938095361427)) ;
#85950 = CARTESIAN_POINT('Ctrl Pts',(-2.65991498954313,0.87455831618191,0.0502557044301233)) ;
#85951 = CARTESIAN_POINT('Ctrl Pts',(-2.68340372472091,0.80311878192931,0.0458816189912835)) ;
#85952 = CARTESIAN_POINT('Ctrl Pts',(-2.70397400538756,0.730840390951851,
0.0415274727316643)) ;
#85953 = CARTESIAN_POINT('Ctrl Pts',(-2.72156688794631,0.658083333958098,
0.0372139915639986)) ;
#85954 = CARTESIAN_POINT('Ctrl Pts',(-2.73873272767104,0.587092353655318,
0.0330052141716357)) ;
#85955 = CARTESIAN_POINT('Ctrl Pts',(-2.75306423214757,0.515646379818062,
0.0288351841829885)) ;
#85956 = CARTESIAN_POINT('Ctrl Pts',(-2.76456012106818,0.444080327191637,
0.0247219782951128)) ;
#85957 = CARTESIAN_POINT('Ctrl Pts',(-2.77648499310844,0.369843700003427,
0.0204552831115665)) ;
#85958 = CARTESIAN_POINT('Ctrl Pts',(-2.78535855947916,0.295478663836406,
0.0162497776372025)) ;
#85959 = CARTESIAN_POINT('Ctrl Pts',(-2.79123720917081,0.221347785486007,
0.0121237414408675)) ;
#85960 = CARTESIAN_POINT('Ctrl Pts',(-2.79711585886245,0.147216907135608,
0.00799770524453251)) ;
#85961 = CARTESIAN_POINT('Ctrl Pts',(-2.79999999999986,0.0733208567888282,
0.0039511653318002)) ;
#85962 = CARTESIAN_POINT('Ctrl Pts',(-2.79999999999986,-3.530509218308E-14,
3.5527136788005E-15)) ;
#85963 = CARTESIAN_POINT('Ctrl Pts',(-2.79999999999986,-0.071465990727953,
-0.00385120901927697)) ;
#85964 = CARTESIAN_POINT('Ctrl Pts',(-2.7972601419783,-0.143478336965554,
-0.00779301796942602)) ;
#85965 = CARTESIAN_POINT('Ctrl Pts',(-2.79167762249238,-0.215722164077992,
-0.0118107533868033)) ;
#85966 = CARTESIAN_POINT('Ctrl Pts',(-2.78613441033479,-0.287457311939202,
-0.0158001993471373)) ;
#85967 = CARTESIAN_POINT('Ctrl Pts',(-2.77778812917958,-0.359420096605276,
-0.0198644808623646)) ;
#85968 = CARTESIAN_POINT('Ctrl Pts',(-2.76658552138353,-0.431282451382235,
-0.0239871076329595)) ;
#85969 = CARTESIAN_POINT('Ctrl Pts',(-2.75529981055853,-0.503677894477359,
-0.0281403168159786)) ;
#85970 = CARTESIAN_POINT('Ctrl Pts',(-2.74111495138493,-0.575970755463133,
-0.0323527111157155)) ;
#85971 = CARTESIAN_POINT('Ctrl Pts',(-2.72402935956772,-0.647814825557682,
-0.0366056691562411)) ;
#85972 = CARTESIAN_POINT('Ctrl Pts',(-2.7072319600783,-0.718447061141654,
-0.040786890151263)) ;
#85973 = CARTESIAN_POINT('Ctrl Pts',(-2.68763094902248,-0.78864483148189,
-0.0450072789963427)) ;
#85974 = CARTESIAN_POINT('Ctrl Pts',(-2.66527685064352,-0.858078848022196,
-0.0492479629874277)) ;
#85975 = CARTESIAN_POINT('Ctrl Pts',(-2.64295407198129,-0.927415582458213,
-0.0534827054719884)) ;
#85976 = CARTESIAN_POINT('Ctrl Pts',(-2.61788602769748,-0.995990034361363,
-0.0577376477956646)) ;
#85977 = CARTESIAN_POINT('Ctrl Pts',(-2.59017404346296,-1.06348409699912,
-0.0619933858678578)) ;
#85978 = CARTESIAN_POINT('Ctrl Pts',(-2.56246019619536,-1.13098269715648,
-0.0662494100466235)) ;
#85979 = CARTESIAN_POINT('Ctrl Pts',(-2.53210230703243,-1.1974001326039,-0.0705061904617605)) ;
#85980 = CARTESIAN_POINT('Ctrl Pts',(-2.49925004242354,-1.26243781052585,
-0.0747442955669683)) ;
#85981 = CARTESIAN_POINT('Ctrl Pts',(-2.46534370723371,-1.32956223357075,
-0.0791183810060595)) ;
#85982 = CARTESIAN_POINT('Ctrl Pts',(-2.42878055178955,-1.39521615891874,
-0.0834725272659328)) ;
#85983 = CARTESIAN_POINT('Ctrl Pts',(-2.38977358996665,-1.45910321386024,
-0.0877860084338508)) ;
#85984 = CARTESIAN_POINT('Ctrl Pts',(-2.35171346806522,-1.52143949911202,
-0.0919947858263564)) ;
#85985 = CARTESIAN_POINT('Ctrl Pts',(-2.31132743947584,-1.5820933357032,-0.0961648158151461)) ;
#85986 = CARTESIAN_POINT('Ctrl Pts',(-2.26885141937174,-1.64082699783198,
-0.100278021703165)) ;
#85987 = CARTESIAN_POINT('Ctrl Pts',(-2.22479035475663,-1.70175237821829,
-0.104544716887014)) ;
#85988 = CARTESIAN_POINT('Ctrl Pts',(-2.17848089235109,-1.76061095853362,
-0.108750222361676)) ;
#85989 = CARTESIAN_POINT('Ctrl Pts',(-2.1302192786324,-1.81718623837581,-0.1128762585583)) ;
#85990 = CARTESIAN_POINT('Ctrl Pts',(-2.08195766491371,-1.87376151821799,
-0.117002294754924)) ;
#85991 = CARTESIAN_POINT('Ctrl Pts',(-2.0317446623635,-1.92805331228106,-0.121048834667934)) ;
#85992 = CARTESIAN_POINT('Ctrl Pts',(-1.97989898732219,-1.97989898732237,
-0.124999999999997)) ;
#85993 = CARTESIAN_POINT('Ctrl Pts',(-1.92936490065135,-2.03043307399321,
-0.1288512090195)) ;
#85994 = CARTESIAN_POINT('Ctrl Pts',(-1.87650711010787,-2.07941612016318,
-0.132793017969882)) ;
#85995 = CARTESIAN_POINT('Ctrl Pts',(-1.82147557266977,-2.12655278283116,
-0.1368107533875)) ;
#85996 = CARTESIAN_POINT('Ctrl Pts',(-1.76683152026772,-2.1733575494213,-0.14080019934737)) ;
#85997 = CARTESIAN_POINT('Ctrl Pts',(-1.71004443524148,-2.21834121044387,
-0.144864480862115)) ;
#85998 = CARTESIAN_POINT('Ctrl Pts',(-1.6513086369343,-2.26123412887429,-0.148987107632213)) ;
#85999 = CARTESIAN_POINT('Ctrl Pts',(-1.59213712553966,-2.30444523495957,
-0.153140316815256)) ;
#86000 = CARTESIAN_POINT('Ctrl Pts',(-1.53098814319316,-2.34553379708271,
-0.157352711115019)) ;
#86001 = CARTESIAN_POINT('Ctrl Pts',(-1.46810537620645,-2.38425388840062,
-0.161605669155572)) ;
#86002 = CARTESIAN_POINT('Ctrl Pts',(-1.40628328836495,-2.42232086607022,
-0.165786890150902)) ;
#86003 = CARTESIAN_POINT('Ctrl Pts',(-1.3427859610928,-2.45809817766906,-0.170007278996297)) ;
#86004 = CARTESIAN_POINT('Ctrl Pts',(-1.27788196259615,-2.49138870706103,
-0.1742479629877)) ;
#86005 = CARTESIAN_POINT('Ctrl Pts',(-1.21306889933907,-2.52463259399128,
-0.178482705471281)) ;
#86006 = CARTESIAN_POINT('Ctrl Pts',(-1.14685365529364,-2.55539626983734,
-0.182737647793968)) ;
#86007 = CARTESIAN_POINT('Ctrl Pts',(-1.07953281395635,-2.58352644724055,
-0.186993385865175)) ;
#86008 = CARTESIAN_POINT('Ctrl Pts',(-1.01220744670876,-2.61165851580639,
-0.191249410045235)) ;
#86009 = CARTESIAN_POINT('Ctrl Pts',(-0.943776958404474,-2.63715646551875,
-0.195506190461672)) ;
#86010 = CARTESIAN_POINT('Ctrl Pts',(-0.874558316209742,-2.65991498953412,
-0.199744295568167)) ;
#86011 = CARTESIAN_POINT('Ctrl Pts',(-0.803118781955034,-2.68340372471343,
-0.204118381007154)) ;
#86012 = CARTESIAN_POINT('Ctrl Pts',(-0.730840390975363,-2.70397400538142,
-0.208472527266922)) ;
#86013 = CARTESIAN_POINT('Ctrl Pts',(-0.658083333979333,-2.72156688794133,
-0.212786008434736)) ;
#86014 = CARTESIAN_POINT('Ctrl Pts',(-0.587092353674923,-2.73873272766704,
-0.216994785827209)) ;
#86015 = CARTESIAN_POINT('Ctrl Pts',(-0.515646379835979,-2.75306423214443,
-0.221164815815966)) ;
#86016 = CARTESIAN_POINT('Ctrl Pts',(-0.444080327207839,-2.76456012106575,
-0.22527802170395)) ;
#86017 = CARTESIAN_POINT('Ctrl Pts',(-0.369843700016937,-2.77648499310689,
-0.229544716887661)) ;
#86018 = CARTESIAN_POINT('Ctrl Pts',(-0.295478663847176,-2.78535855947826,
-0.233750222362187)) ;
#86019 = CARTESIAN_POINT('Ctrl Pts',(-0.221347785494045,-2.79123720917034,
-0.237876258558679)) ;
#86020 = CARTESIAN_POINT('Ctrl Pts',(-0.147216907140913,-2.79711585886242,
-0.242002294755171)) ;
#86021 = CARTESIAN_POINT('Ctrl Pts',(-0.0733208567914072,-2.80000000000004,
-0.246048834668055)) ;
#86022 = CARTESIAN_POINT('Ctrl Pts',(1.41775480244632E-13,-2.80000000000004,
-0.249999999999996)) ;
#86023 = CARTESIAN_POINT('Ctrl Pts',(0.0714659907356313,-2.80000000000004,
-0.253851209019685)) ;
#86024 = CARTESIAN_POINT('Ctrl Pts',(0.143478336980926,-2.7972601419779,-0.257793017970261)) ;
#86025 = CARTESIAN_POINT('Ctrl Pts',(0.215722164101068,-2.79167762249079,
-0.26181075338808)) ;
#86026 = CARTESIAN_POINT('Ctrl Pts',(0.287457311966629,-2.78613441033227,
-0.26580019934867)) ;
#86027 = CARTESIAN_POINT('Ctrl Pts',(0.359420096637054,-2.77778812917578,
-0.26986448086416)) ;
#86028 = CARTESIAN_POINT('Ctrl Pts',(0.43128245141828,-2.7665855213781,-0.273987107635021)) ;
#86029 = CARTESIAN_POINT('Ctrl Pts',(0.503677894511869,-2.75529981055238,
-0.278140316817974)) ;
#86030 = CARTESIAN_POINT('Ctrl Pts',(0.575970755496058,-2.74111495137817,
-0.282352711117639)) ;
#86031 = CARTESIAN_POINT('Ctrl Pts',(0.647814825588991,-2.72402935956048,
-0.286605669158088)) ;
#86032 = CARTESIAN_POINT('Ctrl Pts',(0.718447061190441,-2.70723196006605,
-0.290786890154163)) ;
#86033 = CARTESIAN_POINT('Ctrl Pts',(0.788644831547911,-2.6876309490038,-0.295007279000315)) ;
#86034 = CARTESIAN_POINT('Ctrl Pts',(0.858078848104923,-2.66527685061709,
-0.299247962992474)) ;
#86035 = CARTESIAN_POINT('Ctrl Pts',(0.927415582529159,-2.64295407195629,
-0.303482705476368)) ;
#86036 = CARTESIAN_POINT('Ctrl Pts',(0.995990034420632,-2.61788602767484,
-0.307737647799362)) ;
#86037 = CARTESIAN_POINT('Ctrl Pts',(1.063484097047,-2.59017404344353,-0.31199338587087)) ;
#86038 = CARTESIAN_POINT('Ctrl Pts',(1.13098269720771,-2.56246019617309,-0.316249410049879)) ;
#86039 = CARTESIAN_POINT('Ctrl Pts',(1.19740013265829,-2.53210230700705,-0.320506190465256)) ;
#86040 = CARTESIAN_POINT('Ctrl Pts',(1.26243781058317,-2.49925004239482,-0.324744295570696)) ;
#86041 = CARTESIAN_POINT('Ctrl Pts',(1.32956223362246,-2.4653437072059,-0.329118381009465)) ;
#86042 = CARTESIAN_POINT('Ctrl Pts',(1.39521615896498,-2.42878055176307,-0.333472527269013)) ;
#86043 = CARTESIAN_POINT('Ctrl Pts',(1.45910321390119,-2.3897735899419,-0.337786008436608)) ;
#86044 = CARTESIAN_POINT('Ctrl Pts',(1.52143949914924,-2.35171346804128,-0.341994785828894)) ;
#86045 = CARTESIAN_POINT('Ctrl Pts',(1.58209333573682,-2.31132743945296,-0.346164815817466)) ;
#86046 = CARTESIAN_POINT('Ctrl Pts',(1.64082699786211,-2.26885141935021,-0.350278021705267)) ;
#86047 = CARTESIAN_POINT('Ctrl Pts',(1.70175237824273,-2.22479035473798,-0.354544716888746)) ;
#86048 = CARTESIAN_POINT('Ctrl Pts',(1.76061095855268,-2.17848089233573,-0.358750222363044)) ;
#86049 = CARTESIAN_POINT('Ctrl Pts',(1.81718623838984,-2.13021927862069,-0.362876258559316)) ;
#86050 = CARTESIAN_POINT('Ctrl Pts',(1.87376151822699,-2.08195766490564,-0.367002294755587)) ;
#86051 = CARTESIAN_POINT('Ctrl Pts',(1.92805331228543,-2.03174466235941,-0.371048834668258)) ;
#86052 = CARTESIAN_POINT('Ctrl Pts',(1.97989898732247,-1.97989898732237,-0.374999999999996)) ;
#86053 = CARTESIAN_POINT('Ctrl Pts',(2.03043307398575,-1.9293649006591,-0.378851209018922)) ;
#86054 = CARTESIAN_POINT('Ctrl Pts',(2.07941612014859,-1.8765071101239,-0.382793017968699)) ;
#86055 = CARTESIAN_POINT('Ctrl Pts',(2.12655278281006,-1.82147557269471,-0.386810753385691)) ;
#86056 = CARTESIAN_POINT('Ctrl Pts',(2.17335754939861,-1.7668315202958,-0.390800199345357)) ;
#86057 = CARTESIAN_POINT('Ctrl Pts',(2.21834121041981,-1.71004443527286,-0.394864480859893)) ;
#86058 = CARTESIAN_POINT('Ctrl Pts',(2.26123412884909,-1.65130863696912,-0.398987107629781)) ;
#86059 = CARTESIAN_POINT('Ctrl Pts',(2.30444523493625,-1.59213712557381,-0.403140316812903)) ;
#86060 = CARTESIAN_POINT('Ctrl Pts',(2.34553379706123,-1.5309881432265,-0.40735271111275)) ;
#86061 = CARTESIAN_POINT('Ctrl Pts',(2.38425388838089,-1.46810537623884,-0.411605669153394)) ;
#86062 = CARTESIAN_POINT('Ctrl Pts',(2.4223208660529,-1.4062832883953,-0.415786890148887)) ;
#86063 = CARTESIAN_POINT('Ctrl Pts',(2.45809817765399,-1.34278596112091,-0.420007278994453)) ;
#86064 = CARTESIAN_POINT('Ctrl Pts',(2.49138870704804,-1.27788196262186,-0.424247962986031)) ;
#86065 = CARTESIAN_POINT('Ctrl Pts',(2.52463259397961,-1.21306889936383,-0.428482705469693)) ;
#86066 = CARTESIAN_POINT('Ctrl Pts',(2.55539626982691,-1.14685365531737,-0.432737647792464)) ;
#86067 = CARTESIAN_POINT('Ctrl Pts',(2.58352644723128,-1.07953281397895,-0.436993385863757)) ;
#86068 = CARTESIAN_POINT('Ctrl Pts',(2.61165851579408,-1.01220744674031,-0.441249410043268)) ;
#86069 = CARTESIAN_POINT('Ctrl Pts',(2.63715646550409,-0.943776958445191,
-0.445506190459158)) ;
#86070 = CARTESIAN_POINT('Ctrl Pts',(2.65991498951784,-0.874558316259777,
-0.449744295565114)) ;
#86071 = CARTESIAN_POINT('Ctrl Pts',(2.68340372469986,-0.803118782001304,
-0.454118381004365)) ;
#86072 = CARTESIAN_POINT('Ctrl Pts',(2.70397400537026,-0.73084039101769,-0.4584725272644)) ;
#86073 = CARTESIAN_POINT('Ctrl Pts',(2.72156688793222,-0.658083334017594,
-0.462786008432479)) ;
#86074 = CARTESIAN_POINT('Ctrl Pts',(2.73873272766113,-0.58709235370434,-0.4669947858255)) ;
#86075 = CARTESIAN_POINT('Ctrl Pts',(2.75306423214098,-0.51564637985638,-0.471164815814798)) ;
#86076 = CARTESIAN_POINT('Ctrl Pts',(2.76456012106405,-0.444080327219168,
-0.47527802170331)) ;
#86077 = CARTESIAN_POINT('Ctrl Pts',(2.7764849931058,-0.369843700026418,-0.479544716887134)) ;
#86078 = CARTESIAN_POINT('Ctrl Pts',(2.78535855947762,-0.295478663854794,
-0.483750222361771)) ;
#86079 = CARTESIAN_POINT('Ctrl Pts',(2.79123720917,-0.221347785499792,-0.48787625855837)) ;
#86080 = CARTESIAN_POINT('Ctrl Pts',(2.79711585886238,-0.14721690714479,-0.492002294754969)) ;
#86081 = CARTESIAN_POINT('Ctrl Pts',(2.80000000000014,-0.0733208567934236,
-0.496048834667957)) ;
#86082 = CARTESIAN_POINT('Ctrl Pts',(2.80000000000014,-3.98570065840431E-14,
-0.499999999999997)) ;
#86083 = CARTESIAN_POINT('Ctrl Pts',(2.80000000000014,0.0714659907286896,
-0.503851209019321)) ;
#86084 = CARTESIAN_POINT('Ctrl Pts',(2.79726014197852,0.143478336967113,-0.507793017969516)) ;
#86085 = CARTESIAN_POINT('Ctrl Pts',(2.79167762249248,0.215722164080371,-0.51181075338694)) ;
#86086 = CARTESIAN_POINT('Ctrl Pts',(2.78613441033398,0.287457311952493,-0.515800199347882)) ;
#86087 = CARTESIAN_POINT('Ctrl Pts',(2.77778812917701,0.35942009662955,-0.519864480863741)) ;
#86088 = CARTESIAN_POINT('Ctrl Pts',(2.76658552137832,0.431282451417391,-0.523987107634981)) ;
#86089 = CARTESIAN_POINT('Ctrl Pts',(2.75529981055261,0.503677894511009,-0.528140316817935)) ;
#86090 = CARTESIAN_POINT('Ctrl Pts',(2.74111495137841,0.575970755495219,-0.532352711117601)) ;
#86091 = CARTESIAN_POINT('Ctrl Pts',(2.72402935956074,0.64781482558818,-0.536605669158051)) ;
#86092 = CARTESIAN_POINT('Ctrl Pts',(2.7072319600679,0.718447061182986,-0.540786890153733)) ;
#86093 = CARTESIAN_POINT('Ctrl Pts',(2.68763094900779,0.788644831533882,-0.545007278999483)) ;
#86094 = CARTESIAN_POINT('Ctrl Pts',(2.66527685062371,0.858078848084507,-0.549247962991238)) ;
#86095 = CARTESIAN_POINT('Ctrl Pts',(2.64295407196269,0.927415582511202,-0.55348270547527)) ;
#86096 = CARTESIAN_POINT('Ctrl Pts',(2.61788602768083,0.995990034405129,-0.557737647798405)) ;
#86097 = CARTESIAN_POINT('Ctrl Pts',(2.59017404344894,1.06348409703389,-0.561993385870055)) ;
#86098 = CARTESIAN_POINT('Ctrl Pts',(2.56246019617494,1.13098269720426,-0.566249410049665)) ;
#86099 = CARTESIAN_POINT('Ctrl Pts',(2.53210230700456,1.19740013266423,-0.570506190465644)) ;
#86100 = CARTESIAN_POINT('Ctrl Pts',(2.49925004238731,1.26243781059807,-0.574744295571679)) ;
#86101 = CARTESIAN_POINT('Ctrl Pts',(2.46534370719862,1.32956223363589,-0.579118381010364)) ;
#86102 = CARTESIAN_POINT('Ctrl Pts',(2.42878055175614,1.39521615897695,-0.583472527269825)) ;
#86103 = CARTESIAN_POINT('Ctrl Pts',(2.38977358993544,1.45910321391176,-0.587786008437335)) ;
#86104 = CARTESIAN_POINT('Ctrl Pts',(2.35171346803545,1.52143949915813,-0.591994785829516)) ;
#86105 = CARTESIAN_POINT('Ctrl Pts',(2.31132743944791,1.58209333574409,-0.596164815817983)) ;
#86106 = CARTESIAN_POINT('Ctrl Pts',(2.26885141934603,1.64082699786784,-0.600278021705682)) ;
#86107 = CARTESIAN_POINT('Ctrl Pts',(2.22479035473437,1.70175237824734,-0.604544716889087)) ;
#86108 = CARTESIAN_POINT('Ctrl Pts',(2.17848089233277,1.76061095855623,-0.608750222363314)) ;
#86109 = CARTESIAN_POINT('Ctrl Pts',(2.13021927861845,1.8171862383924,-0.612876258559516)) ;
#86110 = CARTESIAN_POINT('Ctrl Pts',(2.08195766490413,1.87376151822856,-0.617002294755718)) ;
#86111 = CARTESIAN_POINT('Ctrl Pts',(2.03174466235868,1.92805331228608,-0.621048834668323)) ;
#86112 = CARTESIAN_POINT('Ctrl Pts',(1.97989898732247,1.97989898732229,-0.624999999999997)) ;
#86113 = CARTESIAN_POINT('Ctrl Pts',(1.92934280789448,2.03045516675028,-0.628852892711265)) ;
#86114 = CARTESIAN_POINT('Ctrl Pts',(1.87646083611033,2.0794589999143,-0.632796468752567)) ;
#86115 = CARTESIAN_POINT('Ctrl Pts',(1.82140324313394,2.12661473377325,-0.636816033965384)) ;
#86116 = CARTESIAN_POINT('Ctrl Pts',(1.76686270451503,2.17332762085388,-0.640797850820597)) ;
#86117 = CARTESIAN_POINT('Ctrl Pts',(1.71018744420271,2.21822633676819,-0.644854210151207)) ;
#86118 = CARTESIAN_POINT('Ctrl Pts',(1.65157064835192,2.26104276684513,-0.64896871670484)) ;
#86119 = CARTESIAN_POINT('Ctrl Pts',(1.59322015670206,2.30366467596553,-0.653064530486818)) ;
#86120 = CARTESIAN_POINT('Ctrl Pts',(1.53294606340057,2.34422259843339,-0.657217933521998)) ;
#86121 = CARTESIAN_POINT('Ctrl Pts',(1.47098180002052,2.38248033444321,-0.661411074170311)) ;
#86122 = CARTESIAN_POINT('Ctrl Pts',(1.40920818579906,2.42062036058638,-0.665591313531771)) ;
#86123 = CARTESIAN_POINT('Ctrl Pts',(1.34575523781256,2.45647383441825,-0.669811010885196)) ;
#86124 = CARTESIAN_POINT('Ctrl Pts',(1.28089107539402,2.48984297757431,-0.674051302933831)) ;
#86125 = CARTESIAN_POINT('Ctrl Pts',(1.21613126706714,2.52315843613023,-0.678284773159621)) ;
#86126 = CARTESIAN_POINT('Ctrl Pts',(1.14996533229138,2.55399715855579,-0.682538733416948)) ;
#86127 = CARTESIAN_POINT('Ctrl Pts',(1.08268935536029,2.58220521256341,-0.686793792120889)) ;
#86128 = CARTESIAN_POINT('Ctrl Pts',(1.01452793048841,2.61078452484886,-0.691104853474501)) ;
#86129 = CARTESIAN_POINT('Ctrl Pts',(0.945227658599892,2.63666307800147,-0.695417001006243)) ;
#86130 = CARTESIAN_POINT('Ctrl Pts',(0.875117841601264,2.65973095694117,-0.699710035604307)) ;
#86131 = CARTESIAN_POINT('Ctrl Pts',(0.805725192645433,2.68256286970239,-0.703959155849829)) ;
#86132 = CARTESIAN_POINT('Ctrl Pts',(0.735540180656531,2.70264128788266,-0.708189513573025)) ;
#86133 = CARTESIAN_POINT('Ctrl Pts',(0.66489291968411,2.71991128630217,-0.712382093349892)) ;
#86134 = CARTESIAN_POINT('Ctrl Pts',(0.593150457159884,2.73744901101153,-0.716639668143048)) ;
#86135 = CARTESIAN_POINT('Ctrl Pts',(0.520932013366811,2.75209047495254,-0.720858244268042)) ;
#86136 = CARTESIAN_POINT('Ctrl Pts',(0.448583832441685,2.76383294453045,-0.725019102062247)) ;
#86137 = CARTESIAN_POINT('Ctrl Pts',(0.376235651516553,2.77557541410835,-0.729179959856452)) ;
#86138 = CARTESIAN_POINT('Ctrl Pts',(0.303758415027341,2.78441910171876,-0.733283067332032)) ;
#86139 = CARTESIAN_POINT('Ctrl Pts',(0.231488339806442,2.7904145119558,-0.737311433537144)) ;
#86140 = CARTESIAN_POINT('Ctrl Pts',(0.212934509996843,2.79195370810077,-0.738345632280566)) ;
#86141 = CARTESIAN_POINT('Ctrl Pts',(0.194394253672223,2.79330543747825,-0.739374915040527)) ;
#86142 = CARTESIAN_POINT('Ctrl Pts',(0.175873072149721,2.79447108814753,-0.740399016341689)) ;
#86143 = CARTESIAN_POINT('Ctrl Pts',(1.4210854715202E-13,1.69999999999996,
0.250000000000004)) ;
#86144 = CARTESIAN_POINT('Ctrl Pts',(-0.70416305603412,1.69999999999996,0.187500000000004)) ;
#86145 = CARTESIAN_POINT('Ctrl Pts',(-1.20208152801699,1.20208152801709,0.125000000000004)) ;
#86146 = CARTESIAN_POINT('Ctrl Pts',(-1.69999999999986,0.704163056034226,
0.0625000000000035)) ;
#86147 = CARTESIAN_POINT('Ctrl Pts',(-1.69999999999986,-3.54230418100775E-14,
3.53883589099269E-15)) ;
#86148 = CARTESIAN_POINT('Ctrl Pts',(-1.69999999999986,-0.704163056034298,
-0.0624999999999964)) ;
#86149 = CARTESIAN_POINT('Ctrl Pts',(-1.20208152801699,-1.20208152801717,
-0.124999999999997)) ;
#86150 = CARTESIAN_POINT('Ctrl Pts',(-0.70416305603412,-1.70000000000004,
-0.187499999999997)) ;
#86151 = CARTESIAN_POINT('Ctrl Pts',(1.41900357196165E-13,-1.70000000000004,
-0.249999999999996)) ;
#86152 = CARTESIAN_POINT('Ctrl Pts',(0.704163056034403,-1.70000000000004,
-0.312499999999996)) ;
#86153 = CARTESIAN_POINT('Ctrl Pts',(1.20208152801727,-1.20208152801717,-0.374999999999996)) ;
#86154 = CARTESIAN_POINT('Ctrl Pts',(1.70000000000014,-0.704163056034298,
-0.437499999999997)) ;
#86155 = CARTESIAN_POINT('Ctrl Pts',(1.70000000000014,-3.58394217217876E-14,
-0.499999999999997)) ;
#86156 = CARTESIAN_POINT('Ctrl Pts',(1.70000000000014,0.704163056034226,-0.562499999999996)) ;
#86157 = CARTESIAN_POINT('Ctrl Pts',(1.20208152801727,1.20208152801709,-0.624999999999997)) ;
#86158 = CARTESIAN_POINT('Ctrl Pts',(0.747866155279392,1.65629690075497,-0.682014275214703)) ;
#86159 = CARTESIAN_POINT('Ctrl Pts',(0.106776946927047,1.6966433578112,-0.740399301632037)) ;
#86160 = CARTESIAN_POINT('Ctrl Pts',(1.4210854715202E-13,2.79999999999996,
0.250000000000004)) ;
#86161 = CARTESIAN_POINT('Ctrl Pts',(-1.15979797464453,2.79999999999996,0.187500000000004)) ;
#86162 = CARTESIAN_POINT('Ctrl Pts',(-1.97989898732219,1.97989898732229,0.125000000000004)) ;
#86163 = CARTESIAN_POINT('Ctrl Pts',(-2.79999999999986,1.15979797464463,0.0625000000000035)) ;
#86164 = CARTESIAN_POINT('Ctrl Pts',(-2.79999999999986,-3.53556862361244E-14,
3.53883589099269E-15)) ;
#86165 = CARTESIAN_POINT('Ctrl Pts',(-2.79999999999986,-1.15979797464471,
-0.0624999999999964)) ;
#86166 = CARTESIAN_POINT('Ctrl Pts',(-1.97989898732219,-1.97989898732237,
-0.124999999999997)) ;
#86167 = CARTESIAN_POINT('Ctrl Pts',(-1.15979797464453,-2.80000000000004,
-0.187499999999997)) ;
#86168 = CARTESIAN_POINT('Ctrl Pts',(1.41765646048259E-13,-2.80000000000004,
-0.249999999999996)) ;
#86169 = CARTESIAN_POINT('Ctrl Pts',(1.15979797464481,-2.80000000000004,-0.312499999999996)) ;
#86170 = CARTESIAN_POINT('Ctrl Pts',(1.97989898732247,-1.97989898732237,-0.374999999999996)) ;
#86171 = CARTESIAN_POINT('Ctrl Pts',(2.80000000000014,-1.15979797464471,-0.437499999999997)) ;
#86172 = CARTESIAN_POINT('Ctrl Pts',(2.80000000000014,-3.60414884436469E-14,
-0.499999999999997)) ;
#86173 = CARTESIAN_POINT('Ctrl Pts',(2.80000000000014,1.15979797464463,-0.562499999999996)) ;
#86174 = CARTESIAN_POINT('Ctrl Pts',(1.97989898732247,1.97989898732229,-0.624999999999997)) ;
#86175 = CARTESIAN_POINT('Ctrl Pts',(1.23177954987185,2.72801842477293,-0.682014275214703)) ;
#86176 = CARTESIAN_POINT('Ctrl Pts',(0.175867912585632,2.79447141286552,-0.740399301632037)) ;
#86177 = CARTESIAN_POINT('Ctrl Pts',(1.4210854715202E-13,1.69999999999996,
0.250000000000004)) ;
#86178 = CARTESIAN_POINT('Ctrl Pts',(-0.70416305603412,1.69999999999996,0.187500000000004)) ;
#86179 = CARTESIAN_POINT('Ctrl Pts',(-1.20208152801699,1.20208152801709,0.125000000000004)) ;
#86180 = CARTESIAN_POINT('Ctrl Pts',(-1.69999999999986,0.704163056034226,
0.0625000000000035)) ;
#86181 = CARTESIAN_POINT('Ctrl Pts',(-1.69999999999986,-3.54230418100775E-14,
3.53883589099269E-15)) ;
#86182 = CARTESIAN_POINT('Ctrl Pts',(-1.69999999999986,-0.704163056034298,
-0.0624999999999964)) ;
#86183 = CARTESIAN_POINT('Ctrl Pts',(-1.20208152801699,-1.20208152801717,
-0.124999999999997)) ;
#86184 = CARTESIAN_POINT('Ctrl Pts',(-0.70416305603412,-1.70000000000004,
-0.187499999999997)) ;
#86185 = CARTESIAN_POINT('Ctrl Pts',(1.41900357196165E-13,-1.70000000000004,
-0.249999999999996)) ;
#86186 = CARTESIAN_POINT('Ctrl Pts',(0.704163056034403,-1.70000000000004,
-0.312499999999996)) ;
#86187 = CARTESIAN_POINT('Ctrl Pts',(1.20208152801727,-1.20208152801717,-0.374999999999996)) ;
#86188 = CARTESIAN_POINT('Ctrl Pts',(1.70000000000014,-0.704163056034299,
-0.437499999999997)) ;
#86189 = CARTESIAN_POINT('Ctrl Pts',(1.70000000000014,-3.58394217217876E-14,
-0.499999999999997)) ;
#86190 = CARTESIAN_POINT('Ctrl Pts',(1.70000000000014,0.704163056034226,-0.562499999999996)) ;
#86191 = CARTESIAN_POINT('Ctrl Pts',(1.20208152801727,1.20208152801709,-0.624999999999997)) ;
#86192 = CARTESIAN_POINT('Ctrl Pts',(0.747870497506527,1.65629255852784,-0.682013730167249)) ;
#86193 = CARTESIAN_POINT('Ctrl Pts',(0.106787672942461,1.69664268274361,-0.740398324795293)) ;
#86194 = CARTESIAN_POINT('Ctrl Pts',(1.4210854715202E-13,1.69999999999996,
1.15)) ;
#86195 = CARTESIAN_POINT('Ctrl Pts',(-0.70416305603412,1.69999999999996,1.0875)) ;
#86196 = CARTESIAN_POINT('Ctrl Pts',(-1.20208152801699,1.20208152801709,1.025)) ;
#86197 = CARTESIAN_POINT('Ctrl Pts',(-1.69999999999986,0.704163056034226,
0.962500000000004)) ;
#86198 = CARTESIAN_POINT('Ctrl Pts',(-1.69999999999986,-3.54230418100775E-14,
0.900000000000004)) ;
#86199 = CARTESIAN_POINT('Ctrl Pts',(-1.69999999999986,-0.704163056034298,
0.837500000000003)) ;
#86200 = CARTESIAN_POINT('Ctrl Pts',(-1.20208152801699,-1.20208152801717,
0.775000000000003)) ;
#86201 = CARTESIAN_POINT('Ctrl Pts',(-0.70416305603412,-1.70000000000004,
0.712500000000004)) ;
#86202 = CARTESIAN_POINT('Ctrl Pts',(1.41900357196165E-13,-1.70000000000004,
0.650000000000004)) ;
#86203 = CARTESIAN_POINT('Ctrl Pts',(0.704163056034403,-1.70000000000004,
0.587500000000003)) ;
#86204 = CARTESIAN_POINT('Ctrl Pts',(1.20208152801727,-1.20208152801717,0.525000000000004)) ;
#86205 = CARTESIAN_POINT('Ctrl Pts',(1.70000000000014,-0.704163056034299,
0.462500000000004)) ;
#86206 = CARTESIAN_POINT('Ctrl Pts',(1.70000000000014,-3.58394217217876E-14,
0.400000000000004)) ;
#86207 = CARTESIAN_POINT('Ctrl Pts',(1.70000000000014,0.704163056034226,0.337500000000003)) ;
#86208 = CARTESIAN_POINT('Ctrl Pts',(1.20208152801727,1.20208152801709,0.275000000000003)) ;
#86209 = CARTESIAN_POINT('Ctrl Pts',(0.74786742326303,1.65629563277133,0.217985883945845)) ;
#86210 = CARTESIAN_POINT('Ctrl Pts',(0.106780079053036,1.69664316069034,0.159600983615826)) ;
#86211 = CARTESIAN_POINT('Ctrl Pts',(0.0547743647132352,1.6999161967754,0.154864735933285)) ;
#86212 = CARTESIAN_POINT('Ctrl Pts',(0.00276865037343428,1.70318923286046,
0.150128488250745)) ;
#86213 = CARTESIAN_POINT('Ctrl Pts',(1.4210854715202E-13,1.69999999999996,
0.250000000000004)) ;
#86214 = CARTESIAN_POINT('Ctrl Pts',(-0.70416305603412,1.69999999999996,0.187500000000004)) ;
#86215 = CARTESIAN_POINT('Ctrl Pts',(-1.20208152801699,1.20208152801709,0.125000000000004)) ;
#86216 = CARTESIAN_POINT('Ctrl Pts',(-1.69999999999986,0.704163056034226,
0.0625000000000035)) ;
#86217 = CARTESIAN_POINT('Ctrl Pts',(-1.69999999999986,-3.54230418100775E-14,
3.53883589099269E-15)) ;
#86218 = CARTESIAN_POINT('Ctrl Pts',(-1.69999999999986,-0.704163056034298,
-0.0624999999999964)) ;
#86219 = CARTESIAN_POINT('Ctrl Pts',(-1.20208152801699,-1.20208152801717,
-0.124999999999997)) ;
#86220 = CARTESIAN_POINT('Ctrl Pts',(-0.70416305603412,-1.70000000000004,
-0.187499999999997)) ;
#86221 = CARTESIAN_POINT('Ctrl Pts',(1.41900357196165E-13,-1.70000000000004,
-0.249999999999996)) ;
#86222 = CARTESIAN_POINT('Ctrl Pts',(0.704163056034403,-1.70000000000004,
-0.312499999999996)) ;
#86223 = CARTESIAN_POINT('Ctrl Pts',(1.20208152801727,-1.20208152801717,-0.374999999999996)) ;
#86224 = CARTESIAN_POINT('Ctrl Pts',(1.70000000000014,-0.704163056034299,
-0.437499999999997)) ;
#86225 = CARTESIAN_POINT('Ctrl Pts',(1.70000000000014,-3.58394217217876E-14,
-0.499999999999997)) ;
#86226 = CARTESIAN_POINT('Ctrl Pts',(1.70000000000014,0.704163056034226,-0.562499999999996)) ;
#86227 = CARTESIAN_POINT('Ctrl Pts',(1.20208152801727,1.20208152801709,-0.624999999999997)) ;
#86228 = CARTESIAN_POINT('Ctrl Pts',(0.74786742326303,1.65629563277133,-0.682014116054154)) ;
#86229 = CARTESIAN_POINT('Ctrl Pts',(0.106780079053036,1.69664316069034,-0.740399016384173)) ;
#86230 = CARTESIAN_POINT('Ctrl Pts',(0.0547743647132352,1.6999161967754,-0.745135264066715)) ;
#86231 = CARTESIAN_POINT('Ctrl Pts',(0.00276865037343428,1.70318923286046,
-0.749871511749254)) ;
#86232 = CARTESIAN_POINT('',(0.,0.,0.)) ;
#86233 = CARTESIAN_POINT('Origin',(0.,0.,0.2375)) ;
#86234 = CARTESIAN_POINT('',(-2.9375,3.59739997249535E-16,0.299999999999999)) ;
#86235 = CARTESIAN_POINT('Origin',(0.,0.,0.299999999999999)) ;
#86236 = CARTESIAN_POINT('',(-3.,-3.67394039744206E-16,0.2375)) ;
#86237 = CARTESIAN_POINT('Origin',(-2.9375,-3.59739997249535E-16,0.2375)) ;
#86238 = CARTESIAN_POINT('',(3.,-3.67394039744206E-16,0.2375)) ;
#86239 = CARTESIAN_POINT('Origin',(0.,0.,0.2375)) ;
#86240 = CARTESIAN_POINT('Origin',(0.,0.,0.2375)) ;
#86241 = CARTESIAN_POINT('Origin',(0.,0.,0.299999999999999)) ;
#86242 = CARTESIAN_POINT('',(-3.,3.67394039744206E-16,-0.237500000000001)) ;
#86243 = CARTESIAN_POINT('',(3.,-3.67394039744206E-16,-0.237500000000001)) ;
#86244 = CARTESIAN_POINT('Origin',(0.,0.,-0.237500000000001)) ;
#86245 = CARTESIAN_POINT('Origin',(0.,0.,-0.237500000000001)) ;
#86246 = CARTESIAN_POINT('',(3.,-3.67394039744206E-16,0.299999999999999)) ;
#86247 = CARTESIAN_POINT('Origin',(0.,0.,0.299999999999999)) ;
#86248 = CARTESIAN_POINT('',(1.6,-1.95943487863577E-16,0.299999999999999)) ;
#86249 = CARTESIAN_POINT('Origin',(0.,0.,0.299999999999999)) ;
#86250 = CARTESIAN_POINT('Origin',(0.,0.,-0.237500000000001)) ;
#86251 = CARTESIAN_POINT('',(-2.9375,-3.59739997249535E-16,-0.300000000000001)) ;
#86252 = CARTESIAN_POINT('Origin',(-2.9375,-3.59739997249535E-16,-0.237500000000001)) ;
#86253 = CARTESIAN_POINT('Origin',(0.,0.,-0.300000000000001)) ;
#86254 = CARTESIAN_POINT('Origin',(0.,0.,-0.300000000000001)) ;
#86255 = CARTESIAN_POINT('',(1.6,-1.95943487863577E-16,-0.300000000000001)) ;
#86256 = CARTESIAN_POINT('Origin',(0.,0.,-0.300000000000001)) ;
#86257 = CARTESIAN_POINT('Origin',(0.,0.,0.299999999999999)) ;
#86258 = CARTESIAN_POINT('',(1.6,-1.95943487863577E-16,0.299999999999999)) ;
#86259 = CARTESIAN_POINT('',(-80.3777276305476,121.192596095838,-307.39779808526)) ;
#86260 = CARTESIAN_POINT('',(-80.3778327055775,128.492596095082,-307.39779808526)) ;
#86261 = CARTESIAN_POINT('',(-80.3468802972841,127.892596540544,-307.39779808526)) ;
#86262 = CARTESIAN_POINT('',(-80.3777276305498,121.192596095839,-307.397798085256)) ;
#86263 = CARTESIAN_POINT('',(-80.3778327055782,128.492596095083,-307.397798085257)) ;
#86264 = CARTESIAN_POINT('',(-80.3468802972853,127.892596540545,-307.397798085256)) ;
#86265 = CARTESIAN_POINT('',(-80.3777276305479,121.192596095839,-307.397798085263)) ;
#86266 = CARTESIAN_POINT('',(-80.3778327055784,128.492596095083,-307.397798085262)) ;
#86267 = CARTESIAN_POINT('',(-80.3468802972845,127.892596540545,-307.397798085262)) ;
#86268 = CARTESIAN_POINT('',(-80.377727630548,121.192596095839,-307.397798085262)) ;
#86269 = CARTESIAN_POINT('',(-80.3778327055784,128.492596095083,-307.397798085262)) ;
#86270 = CARTESIAN_POINT('',(-80.3468802972846,127.892596540545,-307.397798085261)) ;
#86271 = CARTESIAN_POINT('',(337.680564494733,-43.6559761620887,-732.37256189943)) ;
#86272 = CARTESIAN_POINT('',(-7.105427357601E-14,-1.49999999999999,4.44089209850063E-15)) ;
#86273 = CARTESIAN_POINT('',(232.1370762928,-212.771889361246,183.235801346415)) ;
#86274 = CARTESIAN_POINT('',(232.137076292802,-212.771889361247,88.2358013464112)) ;
#86275 = CARTESIAN_POINT('',(409.637076292801,-212.771889361238,183.235801346417)) ;
#86276 = CARTESIAN_POINT('',(409.6370762928,-212.771889361236,88.2358013464131)) ;
#86277 = CARTESIAN_POINT('',(0.,0.,0.)) ;
#86278 = CARTESIAN_POINT('',(336.680564494862,732.37256189937,42.1559761620865)) ;
#86279 = UNCERTAINTY_MEASURE_WITH_UNIT(LENGTH_MEASURE(0.01),#86331,
'DISTANCE_ACCURACY_VALUE',
'Maximum model space distance between geometric entities at asserted c
onnectivities') ;
#86280 = UNCERTAINTY_MEASURE_WITH_UNIT(LENGTH_MEASURE(0.01),#86331,
'DISTANCE_ACCURACY_VALUE',
'Maximum model space distance between geometric entities at asserted c
onnectivities') ;
#86281 = UNCERTAINTY_MEASURE_WITH_UNIT(LENGTH_MEASURE(0.01),#86331,
'DISTANCE_ACCURACY_VALUE',
'Maximum model space distance between geometric entities at asserted c
onnectivities') ;
#86282 = UNCERTAINTY_MEASURE_WITH_UNIT(LENGTH_MEASURE(0.01),#86331,
'DISTANCE_ACCURACY_VALUE',
'Maximum model space distance between geometric entities at asserted c
onnectivities') ;
#86283 = UNCERTAINTY_MEASURE_WITH_UNIT(LENGTH_MEASURE(0.01),#86331,
'DISTANCE_ACCURACY_VALUE',
'Maximum model space distance between geometric entities at asserted c
onnectivities') ;
#86284 = UNCERTAINTY_MEASURE_WITH_UNIT(LENGTH_MEASURE(0.01),#86331,
'DISTANCE_ACCURACY_VALUE',
'Maximum model space distance between geometric entities at asserted c
onnectivities') ;
#86285 = UNCERTAINTY_MEASURE_WITH_UNIT(LENGTH_MEASURE(0.01),#86331,
'DISTANCE_ACCURACY_VALUE',
'Maximum model space distance between geometric entities at asserted c
onnectivities') ;
#86286 = UNCERTAINTY_MEASURE_WITH_UNIT(LENGTH_MEASURE(0.01),#86331,
'DISTANCE_ACCURACY_VALUE',
'Maximum model space distance between geometric entities at asserted c
onnectivities') ;
#86287 = UNCERTAINTY_MEASURE_WITH_UNIT(LENGTH_MEASURE(0.01),#86331,
'DISTANCE_ACCURACY_VALUE',
'Maximum model space distance between geometric entities at asserted c
onnectivities') ;
#86288 = UNCERTAINTY_MEASURE_WITH_UNIT(LENGTH_MEASURE(0.01),#86331,
'DISTANCE_ACCURACY_VALUE',
'Maximum model space distance between geometric entities at asserted c
onnectivities') ;
#86289 = UNCERTAINTY_MEASURE_WITH_UNIT(LENGTH_MEASURE(0.01),#86331,
'DISTANCE_ACCURACY_VALUE',
'Maximum model space distance between geometric entities at asserted c
onnectivities') ;
#86290 = UNCERTAINTY_MEASURE_WITH_UNIT(LENGTH_MEASURE(0.01),#86331,
'DISTANCE_ACCURACY_VALUE',
'Maximum model space distance between geometric entities at asserted c
onnectivities') ;
#86291 = UNCERTAINTY_MEASURE_WITH_UNIT(LENGTH_MEASURE(0.01),#86331,
'DISTANCE_ACCURACY_VALUE',
'Maximum model space distance between geometric entities at asserted c
onnectivities') ;
#86292 = UNCERTAINTY_MEASURE_WITH_UNIT(LENGTH_MEASURE(0.01),#86331,
'DISTANCE_ACCURACY_VALUE',
'Maximum model space distance between geometric entities at asserted c
onnectivities') ;
#86293 = UNCERTAINTY_MEASURE_WITH_UNIT(LENGTH_MEASURE(0.01),#86331,
'DISTANCE_ACCURACY_VALUE',
'Maximum model space distance between geometric entities at asserted c
onnectivities') ;
#86294 = UNCERTAINTY_MEASURE_WITH_UNIT(LENGTH_MEASURE(0.01),#86331,
'DISTANCE_ACCURACY_VALUE',
'Maximum model space distance between geometric entities at asserted c
onnectivities') ;
#86295 = UNCERTAINTY_MEASURE_WITH_UNIT(LENGTH_MEASURE(0.01),#86331,
'DISTANCE_ACCURACY_VALUE',
'Maximum model space distance between geometric entities at asserted c
onnectivities') ;
#86296 = UNCERTAINTY_MEASURE_WITH_UNIT(LENGTH_MEASURE(0.01),#86331,
'DISTANCE_ACCURACY_VALUE',
'Maximum model space distance between geometric entities at asserted c
onnectivities') ;
#86297 = UNCERTAINTY_MEASURE_WITH_UNIT(LENGTH_MEASURE(0.01),#86331,
'DISTANCE_ACCURACY_VALUE',
'Maximum model space distance between geometric entities at asserted c
onnectivities') ;
#86298 = UNCERTAINTY_MEASURE_WITH_UNIT(LENGTH_MEASURE(0.01),#86331,
'DISTANCE_ACCURACY_VALUE',
'Maximum model space distance between geometric entities at asserted c
onnectivities') ;
#86299 = UNCERTAINTY_MEASURE_WITH_UNIT(LENGTH_MEASURE(0.01),#86331,
'DISTANCE_ACCURACY_VALUE',
'Maximum model space distance between geometric entities at asserted c
onnectivities') ;
#86300 = UNCERTAINTY_MEASURE_WITH_UNIT(LENGTH_MEASURE(0.01),#86331,
'DISTANCE_ACCURACY_VALUE',
'Maximum model space distance between geometric entities at asserted c
onnectivities') ;
#86301 = UNCERTAINTY_MEASURE_WITH_UNIT(LENGTH_MEASURE(0.01),#86331,
'DISTANCE_ACCURACY_VALUE',
'Maximum model space distance between geometric entities at asserted c
onnectivities') ;
#86302 = UNCERTAINTY_MEASURE_WITH_UNIT(LENGTH_MEASURE(0.01),#86331,
'DISTANCE_ACCURACY_VALUE',
'Maximum model space distance between geometric entities at asserted c
onnectivities') ;
#86303 = UNCERTAINTY_MEASURE_WITH_UNIT(LENGTH_MEASURE(0.01),#86331,
'DISTANCE_ACCURACY_VALUE',
'Maximum model space distance between geometric entities at asserted c
onnectivities') ;
#86304 = UNCERTAINTY_MEASURE_WITH_UNIT(LENGTH_MEASURE(0.01),#86331,
'DISTANCE_ACCURACY_VALUE',
'Maximum model space distance between geometric entities at asserted c
onnectivities') ;
#86305 = (
GEOMETRIC_REPRESENTATION_CONTEXT(3)
GLOBAL_UNCERTAINTY_ASSIGNED_CONTEXT((#86279))
GLOBAL_UNIT_ASSIGNED_CONTEXT((#86331,#86333,#86334))
REPRESENTATION_CONTEXT('','3D')
) ;
#86306 = (
GEOMETRIC_REPRESENTATION_CONTEXT(3)
GLOBAL_UNCERTAINTY_ASSIGNED_CONTEXT((#86280))
GLOBAL_UNIT_ASSIGNED_CONTEXT((#86331,#86333,#86334))
REPRESENTATION_CONTEXT('','3D')
) ;
#86307 = (
GEOMETRIC_REPRESENTATION_CONTEXT(3)
GLOBAL_UNCERTAINTY_ASSIGNED_CONTEXT((#86281))
GLOBAL_UNIT_ASSIGNED_CONTEXT((#86331,#86333,#86334))
REPRESENTATION_CONTEXT('','3D')
) ;
#86308 = (
GEOMETRIC_REPRESENTATION_CONTEXT(3)
GLOBAL_UNCERTAINTY_ASSIGNED_CONTEXT((#86282))
GLOBAL_UNIT_ASSIGNED_CONTEXT((#86331,#86333,#86334))
REPRESENTATION_CONTEXT('','3D')
) ;
#86309 = (
GEOMETRIC_REPRESENTATION_CONTEXT(3)
GLOBAL_UNCERTAINTY_ASSIGNED_CONTEXT((#86283))
GLOBAL_UNIT_ASSIGNED_CONTEXT((#86331,#86333,#86334))
REPRESENTATION_CONTEXT('','3D')
) ;
#86310 = (
GEOMETRIC_REPRESENTATION_CONTEXT(3)
GLOBAL_UNCERTAINTY_ASSIGNED_CONTEXT((#86284))
GLOBAL_UNIT_ASSIGNED_CONTEXT((#86331,#86333,#86334))
REPRESENTATION_CONTEXT('','3D')
) ;
#86311 = (
GEOMETRIC_REPRESENTATION_CONTEXT(3)
GLOBAL_UNCERTAINTY_ASSIGNED_CONTEXT((#86285))
GLOBAL_UNIT_ASSIGNED_CONTEXT((#86331,#86333,#86334))
REPRESENTATION_CONTEXT('','3D')
) ;
#86312 = (
GEOMETRIC_REPRESENTATION_CONTEXT(3)
GLOBAL_UNCERTAINTY_ASSIGNED_CONTEXT((#86286))
GLOBAL_UNIT_ASSIGNED_CONTEXT((#86331,#86333,#86334))
REPRESENTATION_CONTEXT('','3D')
) ;
#86313 = (
GEOMETRIC_REPRESENTATION_CONTEXT(3)
GLOBAL_UNCERTAINTY_ASSIGNED_CONTEXT((#86287))
GLOBAL_UNIT_ASSIGNED_CONTEXT((#86331,#86333,#86334))
REPRESENTATION_CONTEXT('','3D')
) ;
#86314 = (
GEOMETRIC_REPRESENTATION_CONTEXT(3)
GLOBAL_UNCERTAINTY_ASSIGNED_CONTEXT((#86288))
GLOBAL_UNIT_ASSIGNED_CONTEXT((#86331,#86333,#86334))
REPRESENTATION_CONTEXT('','3D')
) ;
#86315 = (
GEOMETRIC_REPRESENTATION_CONTEXT(3)
GLOBAL_UNCERTAINTY_ASSIGNED_CONTEXT((#86289))
GLOBAL_UNIT_ASSIGNED_CONTEXT((#86331,#86333,#86334))
REPRESENTATION_CONTEXT('','3D')
) ;
#86316 = (
GEOMETRIC_REPRESENTATION_CONTEXT(3)
GLOBAL_UNCERTAINTY_ASSIGNED_CONTEXT((#86290))
GLOBAL_UNIT_ASSIGNED_CONTEXT((#86331,#86333,#86334))
REPRESENTATION_CONTEXT('','3D')
) ;
#86317 = (
GEOMETRIC_REPRESENTATION_CONTEXT(3)
GLOBAL_UNCERTAINTY_ASSIGNED_CONTEXT((#86291))
GLOBAL_UNIT_ASSIGNED_CONTEXT((#86331,#86333,#86334))
REPRESENTATION_CONTEXT('','3D')
) ;
#86318 = (
GEOMETRIC_REPRESENTATION_CONTEXT(3)
GLOBAL_UNCERTAINTY_ASSIGNED_CONTEXT((#86292))
GLOBAL_UNIT_ASSIGNED_CONTEXT((#86331,#86333,#86334))
REPRESENTATION_CONTEXT('','3D')
) ;
#86319 = (
GEOMETRIC_REPRESENTATION_CONTEXT(3)
GLOBAL_UNCERTAINTY_ASSIGNED_CONTEXT((#86293))
GLOBAL_UNIT_ASSIGNED_CONTEXT((#86331,#86333,#86334))
REPRESENTATION_CONTEXT('','3D')
) ;
#86320 = (
GEOMETRIC_REPRESENTATION_CONTEXT(3)
GLOBAL_UNCERTAINTY_ASSIGNED_CONTEXT((#86294))
GLOBAL_UNIT_ASSIGNED_CONTEXT((#86331,#86333,#86334))
REPRESENTATION_CONTEXT('','3D')
) ;
#86321 = (
GEOMETRIC_REPRESENTATION_CONTEXT(3)
GLOBAL_UNCERTAINTY_ASSIGNED_CONTEXT((#86295))
GLOBAL_UNIT_ASSIGNED_CONTEXT((#86331,#86333,#86334))
REPRESENTATION_CONTEXT('','3D')
) ;
#86322 = (
GEOMETRIC_REPRESENTATION_CONTEXT(3)
GLOBAL_UNCERTAINTY_ASSIGNED_CONTEXT((#86296))
GLOBAL_UNIT_ASSIGNED_CONTEXT((#86331,#86333,#86334))
REPRESENTATION_CONTEXT('','3D')
) ;
#86323 = (
GEOMETRIC_REPRESENTATION_CONTEXT(3)
GLOBAL_UNCERTAINTY_ASSIGNED_CONTEXT((#86297))
GLOBAL_UNIT_ASSIGNED_CONTEXT((#86331,#86333,#86334))
REPRESENTATION_CONTEXT('','3D')
) ;
#86324 = (
GEOMETRIC_REPRESENTATION_CONTEXT(3)
GLOBAL_UNCERTAINTY_ASSIGNED_CONTEXT((#86298))
GLOBAL_UNIT_ASSIGNED_CONTEXT((#86331,#86333,#86334))
REPRESENTATION_CONTEXT('','3D')
) ;
#86325 = (
GEOMETRIC_REPRESENTATION_CONTEXT(3)
GLOBAL_UNCERTAINTY_ASSIGNED_CONTEXT((#86299))
GLOBAL_UNIT_ASSIGNED_CONTEXT((#86331,#86333,#86334))
REPRESENTATION_CONTEXT('','3D')
) ;
#86326 = (
GEOMETRIC_REPRESENTATION_CONTEXT(3)
GLOBAL_UNCERTAINTY_ASSIGNED_CONTEXT((#86300))
GLOBAL_UNIT_ASSIGNED_CONTEXT((#86331,#86333,#86334))
REPRESENTATION_CONTEXT('','3D')
) ;
#86327 = (
GEOMETRIC_REPRESENTATION_CONTEXT(3)
GLOBAL_UNCERTAINTY_ASSIGNED_CONTEXT((#86301))
GLOBAL_UNIT_ASSIGNED_CONTEXT((#86331,#86333,#86334))
REPRESENTATION_CONTEXT('','3D')
) ;
#86328 = (
GEOMETRIC_REPRESENTATION_CONTEXT(3)
GLOBAL_UNCERTAINTY_ASSIGNED_CONTEXT((#86302))
GLOBAL_UNIT_ASSIGNED_CONTEXT((#86331,#86333,#86334))
REPRESENTATION_CONTEXT('','3D')
) ;
#86329 = (
GEOMETRIC_REPRESENTATION_CONTEXT(3)
GLOBAL_UNCERTAINTY_ASSIGNED_CONTEXT((#86303))
GLOBAL_UNIT_ASSIGNED_CONTEXT((#86331,#86333,#86334))
REPRESENTATION_CONTEXT('','3D')
) ;
#86330 = (
GEOMETRIC_REPRESENTATION_CONTEXT(3)
GLOBAL_UNCERTAINTY_ASSIGNED_CONTEXT((#86304))
GLOBAL_UNIT_ASSIGNED_CONTEXT((#86331,#86333,#86334))
REPRESENTATION_CONTEXT('','3D')
) ;
#86331 = (
LENGTH_UNIT()
NAMED_UNIT(*)
SI_UNIT(.MILLI.,.METRE.)
) ;
#86332 = (
LENGTH_UNIT()
NAMED_UNIT(*)
SI_UNIT($,.METRE.)
) ;
#86333 = (
NAMED_UNIT(*)
PLANE_ANGLE_UNIT()
SI_UNIT($,.RADIAN.)
) ;
#86334 = (
NAMED_UNIT(*)
SI_UNIT($,.STERADIAN.)
SOLID_ANGLE_UNIT()
) ;
#86335 = SHAPE_DEFINITION_REPRESENTATION(#86360,#86451) ;
#86336 = SHAPE_DEFINITION_REPRESENTATION(#86361,#86452) ;
#86337 = SHAPE_DEFINITION_REPRESENTATION(#86362,#86453) ;
#86338 = SHAPE_DEFINITION_REPRESENTATION(#86363,#86454) ;
#86339 = SHAPE_DEFINITION_REPRESENTATION(#86364,#86455) ;
#86340 = SHAPE_DEFINITION_REPRESENTATION(#86365,#86456) ;
#86341 = SHAPE_DEFINITION_REPRESENTATION(#86371,#86457) ;
#86342 = SHAPE_DEFINITION_REPRESENTATION(#86372,#86458) ;
#86343 = SHAPE_DEFINITION_REPRESENTATION(#86383,#86459) ;
#86344 = SHAPE_DEFINITION_REPRESENTATION(#86384,#86460) ;
#86345 = SHAPE_DEFINITION_REPRESENTATION(#86385,#86461) ;
#86346 = SHAPE_DEFINITION_REPRESENTATION(#86386,#86462) ;
#86347 = SHAPE_DEFINITION_REPRESENTATION(#86387,#86463) ;
#86348 = SHAPE_DEFINITION_REPRESENTATION(#86397,#86464) ;
#86349 = SHAPE_DEFINITION_REPRESENTATION(#86398,#86465) ;
#86350 = SHAPE_DEFINITION_REPRESENTATION(#86408,#86466) ;
#86351 = SHAPE_DEFINITION_REPRESENTATION(#86409,#86467) ;
#86352 = SHAPE_DEFINITION_REPRESENTATION(#86423,#86468) ;
#86353 = SHAPE_DEFINITION_REPRESENTATION(#86424,#86469) ;
#86354 = SHAPE_DEFINITION_REPRESENTATION(#86425,#86470) ;
#86355 = SHAPE_DEFINITION_REPRESENTATION(#86426,#86471) ;
#86356 = SHAPE_DEFINITION_REPRESENTATION(#86427,#86472) ;
#86357 = SHAPE_DEFINITION_REPRESENTATION(#86428,#86473) ;
#86358 = SHAPE_DEFINITION_REPRESENTATION(#86429,#86474) ;
#86359 = SHAPE_DEFINITION_REPRESENTATION(#86430,#86475) ;
#86360 = PRODUCT_DEFINITION_SHAPE('',$,#86477) ;
#86361 = PRODUCT_DEFINITION_SHAPE('',$,#86478) ;
#86362 = PRODUCT_DEFINITION_SHAPE('',$,#86479) ;
#86363 = PRODUCT_DEFINITION_SHAPE('',$,#86480) ;
#86364 = PRODUCT_DEFINITION_SHAPE('',$,#86481) ;
#86365 = PRODUCT_DEFINITION_SHAPE('',$,#86482) ;
#86366 = PRODUCT_DEFINITION_SHAPE($,$,#670) ;
#86367 = PRODUCT_DEFINITION_SHAPE($,$,#671) ;
#86368 = PRODUCT_DEFINITION_SHAPE($,$,#672) ;
#86369 = PRODUCT_DEFINITION_SHAPE($,$,#673) ;
#86370 = PRODUCT_DEFINITION_SHAPE($,$,#674) ;
#86371 = PRODUCT_DEFINITION_SHAPE('',$,#86483) ;
#86372 = PRODUCT_DEFINITION_SHAPE('',$,#86484) ;
#86373 = PRODUCT_DEFINITION_SHAPE($,$,#675) ;
#86374 = PRODUCT_DEFINITION_SHAPE($,$,#676) ;
#86375 = PRODUCT_DEFINITION_SHAPE($,$,#677) ;
#86376 = PRODUCT_DEFINITION_SHAPE($,$,#678) ;
#86377 = PRODUCT_DEFINITION_SHAPE($,$,#679) ;
#86378 = PRODUCT_DEFINITION_SHAPE($,$,#680) ;
#86379 = PRODUCT_DEFINITION_SHAPE($,$,#681) ;
#86380 = PRODUCT_DEFINITION_SHAPE($,$,#682) ;
#86381 = PRODUCT_DEFINITION_SHAPE($,$,#683) ;
#86382 = PRODUCT_DEFINITION_SHAPE($,$,#684) ;
#86383 = PRODUCT_DEFINITION_SHAPE('',$,#86485) ;
#86384 = PRODUCT_DEFINITION_SHAPE('',$,#86486) ;
#86385 = PRODUCT_DEFINITION_SHAPE('',$,#86487) ;
#86386 = PRODUCT_DEFINITION_SHAPE('',$,#86488) ;
#86387 = PRODUCT_DEFINITION_SHAPE('',$,#86489) ;
#86388 = PRODUCT_DEFINITION_SHAPE($,$,#685) ;
#86389 = PRODUCT_DEFINITION_SHAPE($,$,#686) ;
#86390 = PRODUCT_DEFINITION_SHAPE($,$,#687) ;
#86391 = PRODUCT_DEFINITION_SHAPE($,$,#688) ;
#86392 = PRODUCT_DEFINITION_SHAPE($,$,#689) ;
#86393 = PRODUCT_DEFINITION_SHAPE($,$,#690) ;
#86394 = PRODUCT_DEFINITION_SHAPE($,$,#691) ;
#86395 = PRODUCT_DEFINITION_SHAPE($,$,#692) ;
#86396 = PRODUCT_DEFINITION_SHAPE($,$,#693) ;
#86397 = PRODUCT_DEFINITION_SHAPE('',$,#86490) ;
#86398 = PRODUCT_DEFINITION_SHAPE('',$,#86491) ;
#86399 = PRODUCT_DEFINITION_SHAPE($,$,#694) ;
#86400 = PRODUCT_DEFINITION_SHAPE($,$,#695) ;
#86401 = PRODUCT_DEFINITION_SHAPE($,$,#696) ;
#86402 = PRODUCT_DEFINITION_SHAPE($,$,#697) ;
#86403 = PRODUCT_DEFINITION_SHAPE($,$,#698) ;
#86404 = PRODUCT_DEFINITION_SHAPE($,$,#699) ;
#86405 = PRODUCT_DEFINITION_SHAPE($,$,#700) ;
#86406 = PRODUCT_DEFINITION_SHAPE($,$,#701) ;
#86407 = PRODUCT_DEFINITION_SHAPE($,$,#702) ;
#86408 = PRODUCT_DEFINITION_SHAPE('',$,#86492) ;
#86409 = PRODUCT_DEFINITION_SHAPE('',$,#86493) ;
#86410 = PRODUCT_DEFINITION_SHAPE($,$,#703) ;
#86411 = PRODUCT_DEFINITION_SHAPE($,$,#704) ;
#86412 = PRODUCT_DEFINITION_SHAPE($,$,#705) ;
#86413 = PRODUCT_DEFINITION_SHAPE($,$,#706) ;
#86414 = PRODUCT_DEFINITION_SHAPE($,$,#707) ;
#86415 = PRODUCT_DEFINITION_SHAPE($,$,#708) ;
#86416 = PRODUCT_DEFINITION_SHAPE($,$,#709) ;
#86417 = PRODUCT_DEFINITION_SHAPE($,$,#710) ;
#86418 = PRODUCT_DEFINITION_SHAPE($,$,#711) ;
#86419 = PRODUCT_DEFINITION_SHAPE($,$,#712) ;
#86420 = PRODUCT_DEFINITION_SHAPE($,$,#713) ;
#86421 = PRODUCT_DEFINITION_SHAPE($,$,#714) ;
#86422 = PRODUCT_DEFINITION_SHAPE($,$,#715) ;
#86423 = PRODUCT_DEFINITION_SHAPE('',$,#86494) ;
#86424 = PRODUCT_DEFINITION_SHAPE('',$,#86495) ;
#86425 = PRODUCT_DEFINITION_SHAPE('',$,#86496) ;
#86426 = PRODUCT_DEFINITION_SHAPE('',$,#86497) ;
#86427 = PRODUCT_DEFINITION_SHAPE('',$,#86498) ;
#86428 = PRODUCT_DEFINITION_SHAPE('',$,#86499) ;
#86429 = PRODUCT_DEFINITION_SHAPE('',$,#86500) ;
#86430 = PRODUCT_DEFINITION_SHAPE('',$,#86501) ;
#86431 = PRODUCT_DEFINITION_SHAPE($,$,#716) ;
#86432 = PRODUCT_DEFINITION_SHAPE($,$,#717) ;
#86433 = PRODUCT_DEFINITION_SHAPE($,$,#718) ;
#86434 = PRODUCT_DEFINITION_SHAPE($,$,#719) ;
#86435 = PRODUCT_DEFINITION_SHAPE($,$,#720) ;
#86436 = PRODUCT_DEFINITION_SHAPE($,$,#721) ;
#86437 = PRODUCT_DEFINITION_SHAPE($,$,#722) ;
#86438 = PRODUCT_DEFINITION_SHAPE($,$,#723) ;
#86439 = PRODUCT_DEFINITION_SHAPE($,$,#724) ;
#86440 = PRODUCT_DEFINITION_SHAPE($,$,#725) ;
#86441 = PRODUCT_DEFINITION_SHAPE($,$,#726) ;
#86442 = PRODUCT_DEFINITION_SHAPE($,$,#727) ;
#86443 = PRODUCT_DEFINITION_SHAPE($,$,#728) ;
#86444 = PRODUCT_DEFINITION_SHAPE($,$,#729) ;
#86445 = PRODUCT_DEFINITION_SHAPE($,$,#730) ;
#86446 = PRODUCT_DEFINITION_SHAPE($,$,#731) ;
#86447 = PRODUCT_DEFINITION_SHAPE($,$,#732) ;
#86448 = PRODUCT_DEFINITION_SHAPE($,$,#733) ;
#86449 = PRODUCT_DEFINITION_SHAPE($,$,#734) ;
#86450 = PRODUCT_DEFINITION_SHAPE($,$,#735) ;
#86451 = SHAPE_REPRESENTATION('',(#32771,#36521,#36522),#86305) ;
#86452 = SHAPE_REPRESENTATION('',(#32772,#33714,#33715),#86306) ;
#86453 = SHAPE_REPRESENTATION('',(#32773),#86307) ;
#86454 = SHAPE_REPRESENTATION('',(#33060,#33712,#33713),#86308) ;
#86455 = SHAPE_REPRESENTATION('',(#33061,#33118,#33119,#33120,#33121,#33122),
#86309) ;
#86456 = SHAPE_REPRESENTATION('',(#33062),#86310) ;
#86457 = SHAPE_REPRESENTATION('',(#33123,#33195,#33196,#33197,#33198,#33199,
#33200),#86311) ;
#86458 = SHAPE_REPRESENTATION('',(#33124),#86312) ;
#86459 = SHAPE_REPRESENTATION('',(#33716,#36515,#36516,#36517,#36518,#36519,
#36520),#86313) ;
#86460 = SHAPE_REPRESENTATION('',(#33717,#36339,#36340,#36341,#36342),#86314) ;
#86461 = SHAPE_REPRESENTATION('',(#33718),#86315) ;
#86462 = SHAPE_REPRESENTATION('',(#35474,#35902,#35903,#35904,#35905,#35906,
#35907,#35908,#35909,#35910),#86316) ;
#86463 = SHAPE_REPRESENTATION('',(#35475),#86317) ;
#86464 = SHAPE_REPRESENTATION('',(#35911,#36134,#36135,#36136,#36137,#36138,
#36139,#36140,#36141,#36142),#86318) ;
#86465 = SHAPE_REPRESENTATION('',(#35912),#86319) ;
#86466 = SHAPE_REPRESENTATION('',(#36143,#36330,#36331,#36332,#36333,#36334,
#36335,#36336,#36337,#36338),#86320) ;
#86467 = SHAPE_REPRESENTATION('',(#36144),#86321) ;
#86468 = SHAPE_REPRESENTATION('',(#36343),#86322) ;
#86469 = SHAPE_REPRESENTATION('',(#36377,#36503,#36504,#36505),#86323) ;
#86470 = SHAPE_REPRESENTATION('',(#36378,#36506,#36507,#36508),#86324) ;
#86471 = SHAPE_REPRESENTATION('',(#36379,#36509,#36510,#36511),#86325) ;
#86472 = SHAPE_REPRESENTATION('',(#36380,#36512,#36513,#36514),#86326) ;
#86473 = SHAPE_REPRESENTATION('',(#36381),#86327) ;
#86474 = SHAPE_REPRESENTATION('',(#36482),#86328) ;
#86475 = SHAPE_REPRESENTATION('',(#36486),#86329) ;
#86476 = PRODUCT_DEFINITION_CONTEXT('part definition',#86553,'design') ;
#86477 = PRODUCT_DEFINITION('MAS-640',
'MAS-640',#86502,#86476) ;
#86478 = PRODUCT_DEFINITION('Case','Case',#86503,#86476) ;
#86479 = PRODUCT_DEFINITION('Lid','Lid',#86504,#86476) ;
#86480 = PRODUCT_DEFINITION('Box','Box',#86505,#86476) ;
#86481 = PRODUCT_DEFINITION('Box_Nuts','Box_Nuts',#86506,#86476) ;
#86482 = PRODUCT_DEFINITION('Hex_Nut','Hex_Nut',#86507,#86476) ;
#86483 = PRODUCT_DEFINITION('Box_Screws','Box_Screws',#86508,#86476) ;
#86484 = PRODUCT_DEFINITION('Flat_Head_Screw','Flat_Head_Screw',#86509,#86476) ;
#86485 = PRODUCT_DEFINITION('Internals','Internals',#86510,#86476) ;
#86486 = PRODUCT_DEFINITION('Terminal_Rail','Terminal_Rail',#86511,#86476) ;
#86487 = PRODUCT_DEFINITION('Insulator','Insulator',#86512,#86476) ;
#86488 = PRODUCT_DEFINITION('Screws','Screws',#86513,#86476) ;
#86489 = PRODUCT_DEFINITION('Pan_Head_Screw','Pan_Head_Screw',#86514,#86476) ;
#86490 = PRODUCT_DEFINITION('Plates','Plates',#86515,#86476) ;
#86491 = PRODUCT_DEFINITION('Squash_Plate','Squash_Plate',#86516,#86476) ;
#86492 = PRODUCT_DEFINITION('Washers','Washers',#86517,#86476) ;
#86493 = PRODUCT_DEFINITION('Flat_Washer_Large','Flat_Washer_Large',#86518,
#86476) ;
#86494 = PRODUCT_DEFINITION('Breadboard','Breadboard',#86519,#86476) ;
#86495 = PRODUCT_DEFINITION('Screw_Washer_Assembly_1',
'Screw_Washer_Assembly_1',#86520,#86476) ;
#86496 = PRODUCT_DEFINITION('Screw_Washer_Assembly_2',
'Screw_Washer_Assembly_2',#86521,#86476) ;
#86497 = PRODUCT_DEFINITION('Screw_Washer_Assembly_3',
'Screw_Washer_Assembly_3',#86522,#86476) ;
#86498 = PRODUCT_DEFINITION('Screw_Washer_Assembly_4',
'Screw_Washer_Assembly_4',#86523,#86476) ;
#86499 = PRODUCT_DEFINITION('Pan_Head_Phillips_Screw',
'Pan_Head_Phillips_Screw',#86524,#86476) ;
#86500 = PRODUCT_DEFINITION('Lock_Washer','Lock_Washer',#86525,#86476) ;
#86501 = PRODUCT_DEFINITION('Flat_Washer_Small','Flat_Washer_Small',#86526,
#86476) ;
#86502 = PRODUCT_DEFINITION_FORMATION('',$,#86555) ;
#86503 = PRODUCT_DEFINITION_FORMATION('',$,#86556) ;
#86504 = PRODUCT_DEFINITION_FORMATION('',$,#86557) ;
#86505 = PRODUCT_DEFINITION_FORMATION('',$,#86558) ;
#86506 = PRODUCT_DEFINITION_FORMATION('',$,#86559) ;
#86507 = PRODUCT_DEFINITION_FORMATION('',$,#86560) ;
#86508 = PRODUCT_DEFINITION_FORMATION('',$,#86561) ;
#86509 = PRODUCT_DEFINITION_FORMATION('',$,#86562) ;
#86510 = PRODUCT_DEFINITION_FORMATION('',$,#86563) ;
#86511 = PRODUCT_DEFINITION_FORMATION('',$,#86564) ;
#86512 = PRODUCT_DEFINITION_FORMATION('',$,#86565) ;
#86513 = PRODUCT_DEFINITION_FORMATION('',$,#86566) ;
#86514 = PRODUCT_DEFINITION_FORMATION('',$,#86567) ;
#86515 = PRODUCT_DEFINITION_FORMATION('',$,#86568) ;
#86516 = PRODUCT_DEFINITION_FORMATION('',$,#86569) ;
#86517 = PRODUCT_DEFINITION_FORMATION('',$,#86570) ;
#86518 = PRODUCT_DEFINITION_FORMATION('',$,#86571) ;
#86519 = PRODUCT_DEFINITION_FORMATION('',$,#86572) ;
#86520 = PRODUCT_DEFINITION_FORMATION('',$,#86573) ;
#86521 = PRODUCT_DEFINITION_FORMATION('',$,#86574) ;
#86522 = PRODUCT_DEFINITION_FORMATION('',$,#86575) ;
#86523 = PRODUCT_DEFINITION_FORMATION('',$,#86576) ;
#86524 = PRODUCT_DEFINITION_FORMATION('',$,#86577) ;
#86525 = PRODUCT_DEFINITION_FORMATION('',$,#86578) ;
#86526 = PRODUCT_DEFINITION_FORMATION('',$,#86579) ;
#86527 = PRODUCT_RELATED_PRODUCT_CATEGORY('MAS-640',
'MAS-640',(#86555)) ;
#86528 = PRODUCT_RELATED_PRODUCT_CATEGORY('Case','Case',(#86556)) ;
#86529 = PRODUCT_RELATED_PRODUCT_CATEGORY('Lid','Lid',(#86557)) ;
#86530 = PRODUCT_RELATED_PRODUCT_CATEGORY('Box','Box',(#86558)) ;
#86531 = PRODUCT_RELATED_PRODUCT_CATEGORY('Box_Nuts','Box_Nuts',(#86559)) ;
#86532 = PRODUCT_RELATED_PRODUCT_CATEGORY('Hex_Nut','Hex_Nut',(#86560)) ;
#86533 = PRODUCT_RELATED_PRODUCT_CATEGORY('Box_Screws','Box_Screws',(#86561)) ;
#86534 = PRODUCT_RELATED_PRODUCT_CATEGORY('Flat_Head_Screw',
'Flat_Head_Screw',(#86562)) ;
#86535 = PRODUCT_RELATED_PRODUCT_CATEGORY('Internals','Internals',(#86563)) ;
#86536 = PRODUCT_RELATED_PRODUCT_CATEGORY('Terminal_Rail','Terminal_Rail',
(#86564)) ;
#86537 = PRODUCT_RELATED_PRODUCT_CATEGORY('Insulator','Insulator',(#86565)) ;
#86538 = PRODUCT_RELATED_PRODUCT_CATEGORY('Screws','Screws',(#86566)) ;
#86539 = PRODUCT_RELATED_PRODUCT_CATEGORY('Pan_Head_Screw',
'Pan_Head_Screw',(#86567)) ;
#86540 = PRODUCT_RELATED_PRODUCT_CATEGORY('Plates','Plates',(#86568)) ;
#86541 = PRODUCT_RELATED_PRODUCT_CATEGORY('Squash_Plate','Squash_Plate',(#86569)) ;
#86542 = PRODUCT_RELATED_PRODUCT_CATEGORY('Washers','Washers',(#86570)) ;
#86543 = PRODUCT_RELATED_PRODUCT_CATEGORY('Flat_Washer_Large',
'Flat_Washer_Large',(#86571)) ;
#86544 = PRODUCT_RELATED_PRODUCT_CATEGORY('Breadboard','Breadboard',(#86572)) ;
#86545 = PRODUCT_RELATED_PRODUCT_CATEGORY('Screw_Washer_Assembly_1',
'Screw_Washer_Assembly_1',(#86573)) ;
#86546 = PRODUCT_RELATED_PRODUCT_CATEGORY('Screw_Washer_Assembly_2',
'Screw_Washer_Assembly_2',(#86574)) ;
#86547 = PRODUCT_RELATED_PRODUCT_CATEGORY('Screw_Washer_Assembly_3',
'Screw_Washer_Assembly_3',(#86575)) ;
#86548 = PRODUCT_RELATED_PRODUCT_CATEGORY('Screw_Washer_Assembly_4',
'Screw_Washer_Assembly_4',(#86576)) ;
#86549 = PRODUCT_RELATED_PRODUCT_CATEGORY('Pan_Head_Phillips_Screw',
'Pan_Head_Phillips_Screw',(#86577)) ;
#86550 = PRODUCT_RELATED_PRODUCT_CATEGORY('Lock_Washer','Lock_Washer',(#86578)) ;
#86551 = PRODUCT_RELATED_PRODUCT_CATEGORY('Flat_Washer_Small',
'Flat_Washer_Small',(#86579)) ;
#86552 = APPLICATION_PROTOCOL_DEFINITION('international standard',
'automotive_design',2009,#86553) ;
#86553 = APPLICATION_CONTEXT(
'Core Data for Automotive Mechanical Design Process') ;
#86554 = PRODUCT_CONTEXT('part definition',#86553,'mechanical') ;
#86555 = PRODUCT('MAS-640','MAS-640',$,(#86554)) ;
#86556 = PRODUCT('Case','Case',$,(#86554)) ;
#86557 = PRODUCT('Lid','Lid',$,(#86554)) ;
#86558 = PRODUCT('Box','Box',$,(#86554)) ;
#86559 = PRODUCT('Box_Nuts','Box_Nuts',$,(#86554)) ;
#86560 = PRODUCT('Hex_Nut','Hex_Nut',$,(#86554)) ;
#86561 = PRODUCT('Box_Screws','Box_Screws',$,(#86554)) ;
#86562 = PRODUCT('Flat_Head_Screw','Flat_Head_Screw',$,(#86554)) ;
#86563 = PRODUCT('Internals','Internals',$,(#86554)) ;
#86564 = PRODUCT('Terminal_Rail','Terminal_Rail',$,(#86554)) ;
#86565 = PRODUCT('Insulator','Insulator',$,(#86554)) ;
#86566 = PRODUCT('Screws','Screws',$,(#86554)) ;
#86567 = PRODUCT('Pan_Head_Screw','Pan_Head_Screw',$,(#86554)) ;
#86568 = PRODUCT('Plates','Plates',$,(#86554)) ;
#86569 = PRODUCT('Squash_Plate','Squash_Plate',$,(#86554)) ;
#86570 = PRODUCT('Washers','Washers',$,(#86554)) ;
#86571 = PRODUCT('Flat_Washer_Large','Flat_Washer_Large',$,(#86554)) ;
#86572 = PRODUCT('Breadboard','Breadboard',$,(#86554)) ;
#86573 = PRODUCT('Screw_Washer_Assembly_1','Screw_Washer_Assembly_1',$,(#86554)) ;
#86574 = PRODUCT('Screw_Washer_Assembly_2','Screw_Washer_Assembly_2',$,(#86554)) ;
#86575 = PRODUCT('Screw_Washer_Assembly_3','Screw_Washer_Assembly_3',$,(#86554)) ;
#86576 = PRODUCT('Screw_Washer_Assembly_4','Screw_Washer_Assembly_4',$,(#86554)) ;
#86577 = PRODUCT('Pan_Head_Phillips_Screw','Pan_Head_Phillips_Screw',$,(#86554)) ;
#86578 = PRODUCT('Lock_Washer','Lock_Washer',$,(#86554)) ;
#86579 = PRODUCT('Flat_Washer_Small','Flat_Washer_Small',$,(#86554)) ;
#86580 = PRESENTATION_STYLE_ASSIGNMENT((#86585)) ;
#86581 = PRESENTATION_STYLE_ASSIGNMENT((#86586)) ;
#86582 = PRESENTATION_STYLE_ASSIGNMENT((#86587)) ;
#86583 = PRESENTATION_STYLE_ASSIGNMENT((#86588)) ;
#86584 = PRESENTATION_STYLE_ASSIGNMENT((#86589)) ;
#86585 = SURFACE_STYLE_USAGE(.BOTH.,#86590) ;
#86586 = SURFACE_STYLE_USAGE(.BOTH.,#86591) ;
#86587 = SURFACE_STYLE_USAGE(.BOTH.,#86592) ;
#86588 = SURFACE_STYLE_USAGE(.BOTH.,#86593) ;
#86589 = SURFACE_STYLE_USAGE(.BOTH.,#86594) ;
#86590 = SURFACE_SIDE_STYLE('',(#86595)) ;
#86591 = SURFACE_SIDE_STYLE('',(#86596)) ;
#86592 = SURFACE_SIDE_STYLE('',(#86597)) ;
#86593 = SURFACE_SIDE_STYLE('',(#86598)) ;
#86594 = SURFACE_SIDE_STYLE('',(#86599)) ;
#86595 = SURFACE_STYLE_FILL_AREA(#86600) ;
#86596 = SURFACE_STYLE_FILL_AREA(#86601) ;
#86597 = SURFACE_STYLE_FILL_AREA(#86602) ;
#86598 = SURFACE_STYLE_FILL_AREA(#86603) ;
#86599 = SURFACE_STYLE_FILL_AREA(#86604) ;
#86600 = FILL_AREA_STYLE('Steel - Satin',(#86605)) ;
#86601 = FILL_AREA_STYLE('Opaque(228,229,230)',(#86606)) ;
#86602 = FILL_AREA_STYLE('Opaque(203,203,203)',(#86607)) ;
#86603 = FILL_AREA_STYLE('Opaque(42,42,42)',(#86608)) ;
#86604 = FILL_AREA_STYLE('Opaque(64,64,64)',(#86609)) ;
#86605 = FILL_AREA_STYLE_COLOUR('Steel - Satin',#86610) ;
#86606 = FILL_AREA_STYLE_COLOUR('Opaque(228,229,230)',#86611) ;
#86607 = FILL_AREA_STYLE_COLOUR('Opaque(203,203,203)',#86612) ;
#86608 = FILL_AREA_STYLE_COLOUR('Opaque(42,42,42)',#86613) ;
#86609 = FILL_AREA_STYLE_COLOUR('Opaque(64,64,64)',#86614) ;
#86610 = COLOUR_RGB('Steel - Satin', 0.09019608, 0.27058824, 0.51372549) ;
#86611 = COLOUR_RGB('Opaque(228,229,230)', 0.09019608, 0.27058824, 0.51372549) ;
#86612 = COLOUR_RGB('Opaque(203,203,203)', 0.66274510, 0.83137255, 0.94901961) ;
#86613 = COLOUR_RGB('Opaque(42,42,42)', 0.72549020, 0.75294118, 0.79215686) ;
#86614 = COLOUR_RGB('Opaque(64,64,64)', 0.31764706, 0.68627451, 0.89019608) ;
ENDSEC;
END-ISO-10303-21;
